#162262 = CARTESIAN_POINT ( 'NONE',  ( 4.270664716992385479, -1.744513905240049567, -0.6754176267826096369 ) ) ;
#162263 = CARTESIAN_POINT ( 'NONE',  ( -0.02319159430947541692, 2.051704324979522820, -2.228571760951563618 ) ) ;
#162264 = CARTESIAN_POINT ( 'NONE',  ( 5.885121196783658526, 9.023669275293071834, 1.199719254218452047 ) ) ;
#162265 = CARTESIAN_POINT ( 'NONE',  ( -1.499999999999997558, 7.388542872122518368, -4.154462424328208670 ) ) ;
#162266 = CARTESIAN_POINT ( 'NONE',  ( -5.998939594393441155, 7.096481464931535754, 1.069142741232721461 ) ) ;
#162267 = CARTESIAN_POINT ( 'NONE',  ( -5.829642864196175722, 7.824335979694092558, 1.443375672974064550 ) ) ;
#162268 = CARTESIAN_POINT ( 'NONE',  ( 2.998324526916512411, 6.649795714711241423, 0.000000000000000000 ) ) ;
#162269 = CARTESIAN_POINT ( 'NONE',  ( 0.8132587859420150611, -1.660809389245621492, -1.058212622827129357 ) ) ;
#162270 = CARTESIAN_POINT ( 'NONE',  ( 2.495720449669075247, -1.994069261235394741, 0.2986488809556055446 ) ) ;
#162271 = CARTESIAN_POINT ( 'NONE',  ( -7.374745490829552885, 10.69128794168811680, -1.199719254218446718 ) ) ;
#162272 = CARTESIAN_POINT ( 'NONE',  ( 6.378184920586140727, 6.405913593630768510, 0.000000000000000000 ) ) ;
#162273 = CARTESIAN_POINT ( 'NONE',  ( -11.86145016429273014, 10.19999999999999929, -1.100000000000000311 ) ) ;
#162274 = CARTESIAN_POINT ( 'NONE',  ( 2.466951935624495551, 0.1062163371072753354, -2.188993582743845590 ) ) ;
#162275 = PRESENTATION_STYLE_ASSIGNMENT (( #196892 ) ) ;
#162276 = CARTESIAN_POINT ( 'NONE',  ( -8.299562589859897699, 12.83457345481192036, -0.7998128361456281477 ) ) ;
#162277 = CARTESIAN_POINT ( 'NONE',  ( -0.9486429539267164923, 3.042910930033675854, 1.028101543437260013 ) ) ;
#162278 = CARTESIAN_POINT ( 'NONE',  ( 3.469446951953614189E-15, 6.400000000000023448, 1.214306433183764966E-14 ) ) ;
#162279 = CARTESIAN_POINT ( 'NONE',  ( -10.41986968326957808, 5.020773655391575829, -5.279272669861445166 ) ) ;
#162280 = CARTESIAN_POINT ( 'NONE',  ( 6.923409998072794558, 11.22906209772695618, 1.040834085586084257E-14 ) ) ;
#162281 = CARTESIAN_POINT ( 'NONE',  ( 8.103009739377979415, -6.893137084989842123, -7.439168848974011539 ) ) ;
#162282 = CARTESIAN_POINT ( 'NONE',  ( 6.427974226654860956, 7.632296364919712417, -1.082531754730548412 ) ) ;
#162283 = EDGE_LOOP ( 'NONE', ( #121466, #96917, #73998, #134568, #153751 ) ) ;
#162285 = CARTESIAN_POINT ( 'NONE',  ( 2.086589530005359183, -1.236640506920426263, 1.588416314350507674 ) ) ;
#162284 = CARTESIAN_POINT ( 'NONE',  ( 5.284640796330934087, 1.621094592300664328, -0.8731043043393662550 ) ) ;
#162286 = CARTESIAN_POINT ( 'NONE',  ( 3.726148964702048705, -2.024938297411133625, -1.087335920097615594 ) ) ;
#162288 = CARTESIAN_POINT ( 'NONE',  ( 2.254548712976621516, -0.4907705908011159579, -1.795021142807408543 ) ) ;
#162287 = CARTESIAN_POINT ( 'NONE',  ( -0.02919842301645457147, -0.002306431287177941429, -2.073770398395402115 ) ) ;
#162289 = CARTESIAN_POINT ( 'NONE',  ( 3.285556943749998737, -2.005208332855377140, -1.896917185911906500 ) ) ;
#162290 = CARTESIAN_POINT ( 'NONE',  ( -9.386220697865741869, 15.51845925627288203, -7.476614105868906179 ) ) ;
#162291 = CARTESIAN_POINT ( 'NONE',  ( 5.888906298306328502, -1.818048641159516476, -0.5935555146628914702 ) ) ;
#162292 = CARTESIAN_POINT ( 'NONE',  ( -7.147119532698295252, 11.49005655479003174, 0.000000000000000000 ) ) ;
#162293 = CARTESIAN_POINT ( 'NONE',  ( -4.502716413514296079, 8.267269892493059658, -0.7216878364870338292 ) ) ;
#162295 = CARTESIAN_POINT ( 'NONE',  ( 3.678450976403758066, -1.802590750232490491, -0.4997190347926713794 ) ) ;
#162294 = CARTESIAN_POINT ( 'NONE',  ( 5.390208805286830440, -0.5092157624977285968, -2.027641083400610000 ) ) ;
#162296 = CARTESIAN_POINT ( 'NONE',  ( 5.639828713604826405, 9.523624565940227882, -0.7216878364870267237 ) ) ;
#162297 = EDGE_CURVE ( 'NONE', #83982, #8134, #97143, .T. ) ;
#162298 = CARTESIAN_POINT ( 'NONE',  ( 5.372543328820884589, -0.05112055865702340440, -1.840719716649619198 ) ) ;
#162299 = STYLED_ITEM ( 'NONE', ( #37465 ), #22947 ) ;
#162300 = FACE_OUTER_BOUND ( 'NONE', #99631, .T. ) ;
#162301 = CARTESIAN_POINT ( 'NONE',  ( 0.08202876420372311184, -7.861065518611666469, -10.99977341864973468 ) ) ;
#162302 = CARTESIAN_POINT ( 'NONE',  ( 5.355954780876127863, 1.722648150766812103, -0.09025627888907016005 ) ) ;
#162303 = CARTESIAN_POINT ( 'NONE',  ( -6.847031270101295419, 7.946956888995021728, -1.199719254218446718 ) ) ;
#162304 = CARTESIAN_POINT ( 'NONE',  ( 0.7208516900601771304, 1.708106959156988847, 0.2981761063507569198 ) ) ;
#162305 = FILL_AREA_STYLE ('',( #48559 ) ) ;
#162306 = CARTESIAN_POINT ( 'NONE',  ( 0.000000000000000000, 7.999999999999992895, 0.000000000000000000 ) ) ;
#162307 = CARTESIAN_POINT ( 'NONE',  ( 4.645498245716852992, 1.942073188235559522, -0.9706016350095565404 ) ) ;
#162308 = CARTESIAN_POINT ( 'NONE',  ( 3.351995281737112364, 1.825872481133209879, -0.0009662468829912954560 ) ) ;
#162309 = CARTESIAN_POINT ( 'NONE',  ( 1.041763817972749750, 1.313373124611896703, 1.457441342770829262 ) ) ;
#162310 = CARTESIAN_POINT ( 'NONE',  ( 0.5623061109219238407, -1.172325791230070857, 1.762859051686527012 ) ) ;
#162312 = CARTESIAN_POINT ( 'NONE',  ( -1.201851678989727383E-14, 4.509375000341417916, -1.575800808251660134 ) ) ;
#162311 = CARTESIAN_POINT ( 'NONE',  ( 0.1294186239076781653, -2.093018298938463140, 0.9351526010841960668 ) ) ;
#162313 = CARTESIAN_POINT ( 'NONE',  ( 2.065088895208962327, 8.523968132013681753, 2.459875961809493639 ) ) ;
#162314 = CARTESIAN_POINT ( 'NONE',  ( 9.738834413317897898, 10.25639499182604730, 0.000000000000000000 ) ) ;
#162315 = CARTESIAN_POINT ( 'NONE',  ( 3.088655771522513582, -1.261447869382603004, 1.704333039148818507 ) ) ;
#162316 = CARTESIAN_POINT ( 'NONE',  ( -4.934804725694236893, 4.859619722839116918, -0.7216878364870207285 ) ) ;
#162317 = COLOUR_RGB ( '', 0.08235294, 0.09019608, 0.10196078) ;
#162318 = CARTESIAN_POINT ( 'NONE',  ( 2.373851744317274193, 1.000000000000000888, -11.76285798163019969 ) ) ;
#162319 = CARTESIAN_POINT ( 'NONE',  ( -4.406036734316898240, 6.163462161501577441, -1.443375672974051449 ) ) ;
#162320 = CARTESIAN_POINT ( 'NONE',  ( 0.3915760470782835845, -1.894197279051227811, 0.8358220917567968922 ) ) ;
#162322 = CARTESIAN_POINT ( 'NONE',  ( 0.7500000000000006661, 13.61458333401613352, 1.299038105676657340 ) ) ;
#162321 = CARTESIAN_POINT ( 'NONE',  ( 6.983263157960365675, -0.006178392973848687020, 2.053544886540019210 ) ) ;
#162324 = VERTEX_POINT ( 'NONE', #75173 ) ;
#162323 = CARTESIAN_POINT ( 'NONE',  ( 2.174768466102798836, 0.9529365794415098900, 2.006655600372597714 ) ) ;
#162325 = CARTESIAN_POINT ( 'NONE',  ( 0.3000039258060793745, 1.578900123410318823, -1.670874907869798864 ) ) ;
#162327 = CARTESIAN_POINT ( 'NONE',  ( 5.858276910504900847, -2.062741130177087268, -0.005609060510954055022 ) ) ;
#162326 = CARTESIAN_POINT ( 'NONE',  ( 4.033714395265605823, 4.664753868353354704, -1.199719254218446718 ) ) ;
#162329 = CARTESIAN_POINT ( 'NONE',  ( 1.001543065824772753E-15, -2.012499999999999289, 4.012584370867899430 ) ) ;
#162328 = CARTESIAN_POINT ( 'NONE',  ( 6.690022453700429139, 6.769724048930809701, 0.7998128361456331437 ) ) ;
#162330 = CARTESIAN_POINT ( 'NONE',  ( 6.398522151006641678, 6.429640362454684954, 0.000000000000000000 ) ) ;
#162331 = CARTESIAN_POINT ( 'NONE',  ( 0.2331563151865486683, 2.034376611827843906, -2.362208330281903024 ) ) ;
#162332 = CARTESIAN_POINT ( 'NONE',  ( 5.847170753249844033, 0.5281823367668266878, -1.763884204139199330 ) ) ;
#162333 = EDGE_CURVE ( 'NONE', #211245, #178928, #24094, .T. ) ;
#162335 = ORIENTED_EDGE ( 'NONE', *, *, #32928, .F. ) ;
#162334 = CARTESIAN_POINT ( 'NONE',  ( 4.008406971134620633, 7.828225232965717595, 0.7998128361456321445 ) ) ;
#162336 = CARTESIAN_POINT ( 'NONE',  ( -0.2104748580754426390, 2.865278511227668634, -2.591885361450113834 ) ) ;
#162337 = CARTESIAN_POINT ( 'NONE',  ( 1.922448523189672853, 1.607815062812420370, 0.6247884732281087095 ) ) ;
#162338 = CARTESIAN_POINT ( 'NONE',  ( 1.639861632979456418, 2.010800986640928656, -0.1531718788195315928 ) ) ;
#162339 = CARTESIAN_POINT ( 'NONE',  ( 1.846706770127172881, 0.3881029198684777803, -2.265567138619323018 ) ) ;
#162340 = CARTESIAN_POINT ( 'NONE',  ( -1.201851678989727383E-14, 3.759375000341422801, -1.575800808251660134 ) ) ;
#162341 = CARTESIAN_POINT ( 'NONE',  ( 2.073834635255236147, 2.165437736866062224, -0.6553434645707820749 ) ) ;
#162342 = CARTESIAN_POINT ( 'NONE',  ( 4.442079272866404693, 0.9008978453017953969, -1.903793715863113523 ) ) ;
#162343 = CARTESIAN_POINT ( 'NONE',  ( -3.135678666510573365, 6.880318554229450712, 0.000000000000000000 ) ) ;
#162344 = CARTESIAN_POINT ( 'NONE',  ( 3.057584390254026729, 1.761565543986362670, -0.1695560061622681525 ) ) ;
#162345 = CARTESIAN_POINT ( 'NONE',  ( 6.173040012923759257, 6.096301524699504704, -0.7998128361456281477 ) ) ;
#162347 = CARTESIAN_POINT ( 'NONE',  ( 4.845436733290686249, 0.7204735554154987343, -2.176297985750157427 ) ) ;
#162346 = CARTESIAN_POINT ( 'NONE',  ( 6.183927461164522299, 6.387205924212962849, 0.000000000000000000 ) ) ;
#162348 = CARTESIAN_POINT ( 'NONE',  ( -3.249150368769345043, 6.942425863539538611, 0.7998128361456341429 ) ) ;
#162349 =( GEOMETRIC_REPRESENTATION_CONTEXT ( 3 ) GLOBAL_UNCERTAINTY_ASSIGNED_CONTEXT ( ( #49407 ) ) GLOBAL_UNIT_ASSIGNED_CONTEXT ( ( #31107, #49471, #63588 ) ) REPRESENTATION_CONTEXT ( 'NONE', 'WORKASPACE' ) );
#162350 = UNCERTAINTY_MEASURE_WITH_UNIT (LENGTH_MEASURE( 1.000000000000000082E-05 ), #46512, 'distance_accuracy_value', 'NONE');
#162351 = CARTESIAN_POINT ( 'NONE',  ( 6.331294547457450683, 7.449227062530913379, -1.082531754730543083 ) ) ;
#162352 = CARTESIAN_POINT ( 'NONE',  ( 1.499999999999987121, 2.045833333333356929, -0.8660254037844262731 ) ) ;
#162353 = CARTESIAN_POINT ( 'NONE',  ( 4.488337453930180132, -0.4787454259813396229, -2.138356021698713416 ) ) ;
#162354 = CARTESIAN_POINT ( 'NONE',  ( -4.355193658487827690, 6.104145239700998538, -1.599625672291256295 ) ) ;
#162355 = CARTESIAN_POINT ( 'NONE',  ( 0.2184521437216075668, 7.205153265248421590, -1.990034439536078725 ) ) ;
#162356 = EDGE_CURVE ( 'NONE', #81693, #95637, #194271, .T. ) ;
#162357 = CARTESIAN_POINT ( 'NONE',  ( 4.929342268689171469, 7.989555622611471897, -1.003472558803005565 ) ) ;
#162358 = CARTESIAN_POINT ( 'NONE',  ( -1.364683531249997417, 3.259375000341423245, 1.214306433183764966E-14 ) ) ;
#162359 = CARTESIAN_POINT ( 'NONE',  ( 3.527879399192564325, -1.148099800794393444, -1.546878348965428973 ) ) ;
#162360 = CARTESIAN_POINT ( 'NONE',  ( 1.364683531249997417, 9.234375000341396245, 2.602085213965210642E-15 ) ) ;
#162361 = CARTESIAN_POINT ( 'NONE',  ( -3.294268138440636928, 6.787137228248626641, 1.040834085586084257E-14 ) ) ;
#162362 = CARTESIAN_POINT ( 'NONE',  ( 6.135037582782754129, 1.979230198018981701, 0.7618025574447004900 ) ) ;
#162363 = CARTESIAN_POINT ( 'NONE',  ( -5.966997003790228682, 8.054858819212300958, -1.443375672974066548 ) ) ;
#162364 = VERTEX_POINT ( 'NONE', #80503 ) ;
#162365 = CARTESIAN_POINT ( 'NONE',  ( -4.611181642423629157, 7.433443445252599702, 1.082531754730549967 ) ) ;
#162366 = CARTESIAN_POINT ( 'NONE',  ( 3.506755287428983792, 7.242964935309132990, 1.040834085586084257E-14 ) ) ;
#162367 = CARTESIAN_POINT ( 'NONE',  ( 6.356982874815331641, 0.3076174260261410054, -1.815216213958574132 ) ) ;
#162368 = STYLED_ITEM ( 'NONE', ( #43218 ), #37246 ) ;
#162369 = CARTESIAN_POINT ( 'NONE',  ( 11.41381675112453564, 13.53005666089991443, 3.704697986577181190 ) ) ;
#162370 = CARTESIAN_POINT ( 'NONE',  ( 0.6823417656249899377, 3.488541667008085323, -1.181850606188754593 ) ) ;
#162371 = CARTESIAN_POINT ( 'NONE',  ( 2.366429680491717313, 0.08383053003592833008, -1.738530308508005273 ) ) ;
#162372 = CARTESIAN_POINT ( 'NONE',  ( -15.75000000000000000, 13.40000000000000036, 1.099999999999996758 ) ) ;
#162373 = CARTESIAN_POINT ( 'NONE',  ( 0.000000000000000000, 6.161115872820241535, 1.249999999999999778 ) ) ;
#162374 = CARTESIAN_POINT ( 'NONE',  ( -1.402160292154681736E-14, 0.2593750003414224681, -1.575800808251665908 ) ) ;
#162375 = CARTESIAN_POINT ( 'NONE',  ( -4.286372615631644400, 7.381325999705229179, -1.030941853605553016 ) ) ;
#162376 = VECTOR ( 'NONE', #147834, 1000.000000000000000 ) ;
#162377 = CARTESIAN_POINT ( 'NONE',  ( 6.719591497160966931, -2.098179372288328182, 0.5198544864785522579 ) ) ;
#162378 = CARTESIAN_POINT ( 'NONE',  ( -10.62011439820619429, 11.28455497419572318, -0.7998128361456221525 ) ) ;
#162379 = CARTESIAN_POINT ( 'NONE',  ( -5.029711800545518585, 8.811821500704338561, 0.7216878364870458196 ) ) ;
#162380 = CARTESIAN_POINT ( 'NONE',  ( 6.051685545382852638, 0.6321331830463626789, -2.067208725892249799 ) ) ;
#162382 = ORIENTED_EDGE ( 'NONE', *, *, #140437, .T. ) ;
#162381 = DIRECTION ( 'NONE',  ( -1.276756478318932585E-15, 1.000000000000000000, -1.665334536937738262E-16 ) ) ;
#162383 = CARTESIAN_POINT ( 'NONE',  ( 0.6823417656249917140, 4.842708333674755394, 1.181850606188765695 ) ) ;
#162384 = CARTESIAN_POINT ( 'NONE',  ( 6.081318999601531772, 1.822420489394786625, -0.7521447986948930353 ) ) ;
#162385 = CARTESIAN_POINT ( 'NONE',  ( 4.868316058674494684, -0.4618845756635507893, 1.671066720262862182 ) ) ;
#162386 = ADVANCED_FACE ( 'NONE', ( #31768 ), #15479, .T. ) ;
#162388 = CARTESIAN_POINT ( 'NONE',  ( 1.488088480104592826, -2.181432686776756391, -0.2102995727721947705 ) ) ;
#162387 = CARTESIAN_POINT ( 'NONE',  ( -0.6801582343750074422, 0.5989583336747372755, -1.178068619123841643 ) ) ;
#162389 = CARTESIAN_POINT ( 'NONE',  ( 3.505163243484223479, 1.820685690116738531, -1.417681053453226703 ) ) ;
#162390 = CARTESIAN_POINT ( 'NONE',  ( 5.606733736089553055, 1.563247385715782700, -1.342922781998987736 ) ) ;
#162391 = CARTESIAN_POINT ( 'NONE',  ( 1.376788300709189450, 1.794419955772775355, -0.7429034522522351969 ) ) ;
#162392 = CARTESIAN_POINT ( 'NONE',  ( -5.355107487273497391, 9.191449801886996340, 0.7216878364870458196 ) ) ;
#162394 = EDGE_CURVE ( 'NONE', #123589, #23747, #58250, .T. ) ;
#162393 = CARTESIAN_POINT ( 'NONE',  ( -3.481411583659053566, 7.283673624236017830, 0.000000000000000000 ) ) ;
#162395 =( NAMED_UNIT ( * ) SI_UNIT ( $, .STERADIAN. ) SOLID_ANGLE_UNIT ( ) );
#162396 = CARTESIAN_POINT ( 'NONE',  ( 4.078469121099765005, 1.002472831208834680, 1.868716877859360137 ) ) ;
#162397 = CARTESIAN_POINT ( 'NONE',  ( 2.865861461037176205, -0.1511401116795624278, -2.010826411938296143 ) ) ;
#162398 = CARTESIAN_POINT ( 'NONE',  ( -5.707619481228822345, 7.681975366232176583, -1.443375672974051449 ) ) ;
#162399 = CARTESIAN_POINT ( 'NONE',  ( 4.383934217864794647, 1.438874268414831015, 1.673263306058408340 ) ) ;
#162400 = CARTESIAN_POINT ( 'NONE',  ( -3.285556943750000070, -0.1968749995220411830, 0.000000000000000000 ) ) ;
#162401 = CARTESIAN_POINT ( 'NONE',  ( -1.325546123766559337, -3.124052913013680488, -3.130165297716357209 ) ) ;
#162402 = CARTESIAN_POINT ( 'NONE',  ( 0.001355176523862845501, 14.56276549857873093, 11.93721147252166048 ) ) ;
#162403 = CARTESIAN_POINT ( 'NONE',  ( -6.994027139803241866, 9.253060644560830994, -1.599625672291271394 ) ) ;
#162405 = LINE ( 'NONE', #29197, #196337 ) ;
#162404 = CARTESIAN_POINT ( 'NONE',  ( -4.631600894319110040, 8.440630447364583233, 0.4419995416731822280 ) ) ;
#162406 = CARTESIAN_POINT ( 'NONE',  ( 0.3282377607281116716, 2.073664549684627545, 1.224999999999953015 ) ) ;
#162407 = VERTEX_POINT ( 'NONE', #152968 ) ;
#162408 = CARTESIAN_POINT ( 'NONE',  ( 3.995036845513312951, 1.742007986889832161, -1.100897373992800299 ) ) ;
#162409 = CARTESIAN_POINT ( 'NONE',  ( -9.569358774130435563, 3.553060279300347180, -7.167287524826059020 ) ) ;
#162410 = CARTESIAN_POINT ( 'NONE',  ( 0.3773006915670404915, -8.233136995002887204, 9.492905263954449779 ) ) ;
#162411 = CARTESIAN_POINT ( 'NONE',  ( -4.069418662396130593, 7.899405539437467816, -0.7998128361456281477 ) ) ;
#162412 = CARTESIAN_POINT ( 'NONE',  ( -4.522526758610270647, 7.433975764090723359, -1.199719254218453823 ) ) ;
#162413 = CARTESIAN_POINT ( 'NONE',  ( 3.457679895445249674, -1.530724978927421986, -1.317682070945853656 ) ) ;
#162414 = CARTESIAN_POINT ( 'NONE',  ( 1.499999999999987121, 0.2541666666666844154, 0.8660254037844524744 ) ) ;
#162416 = CARTESIAN_POINT ( 'NONE',  ( 10.24960094225127172, 11.06021530882240356, -0.7216878364870257245 ) ) ;
#162415 = CARTESIAN_POINT ( 'NONE',  ( -5.978219388983010418, 5.939287140093762574, -0.7998128361456362523 ) ) ;
#162417 = CARTESIAN_POINT ( 'NONE',  ( 7.644099680006512187, 7.812537802962739697, 1.040834085586084257E-14 ) ) ;
#162418 = CARTESIAN_POINT ( 'NONE',  ( 3.432544477427549534, 2.010279954523132240, 0.4531449079418439774 ) ) ;
#162419 = CARTESIAN_POINT ( 'NONE',  ( 2.461564753630896440, -1.930417925741171103, -0.5826551686555283549 ) ) ;
#162420 = DIRECTION ( 'NONE',  ( -0.000000000000000000, -1.000000000000000000, -0.000000000000000000 ) ) ;
#162421 = CARTESIAN_POINT ( 'NONE',  ( 5.843727902690005749, 6.776436293681846301, -1.199719254218445830 ) ) ;
#162422 = FACE_OUTER_BOUND ( 'NONE', #84599, .T. ) ;
#162423 = CARTESIAN_POINT ( 'NONE',  ( 0.9547317490294878750, 0.3612830171869831353, -1.805165878648997690 ) ) ;
#162424 = CARTESIAN_POINT ( 'NONE',  ( 6.322910218073367616, 2.057572540570989261, 0.7984293639632376038 ) ) ;
#162425 = CARTESIAN_POINT ( 'NONE',  ( 5.899733120602060232, 6.912052057904395141, -1.199719254218452047 ) ) ;
#162426 = CARTESIAN_POINT ( 'NONE',  ( 2.618638089201937635, 1.414096770131420877, -1.634928933042498755 ) ) ;
#162427 = CARTESIAN_POINT ( 'NONE',  ( -5.097502569058225852, 5.049433873430440478, -0.7216878364870207285 ) ) ;
#162428 = CARTESIAN_POINT ( 'NONE',  ( 4.100857973768299303, 1.937344669444723166, 0.8546590867991187279 ) ) ;
#162429 = CARTESIAN_POINT ( 'NONE',  ( 2.812212034788389214, -1.912053501320301718, 1.275153900055803646 ) ) ;
#162430 = CARTESIAN_POINT ( 'NONE',  ( 0.01777464290183803503, 3.404255796403599987, -2.081138097628782990 ) ) ;
#162431 = CARTESIAN_POINT ( 'NONE',  ( 1.129532124359374334, -1.183843481993757774, -1.448407549327054955 ) ) ;
#162432 = CARTESIAN_POINT ( 'NONE',  ( 4.996930482532231821, 1.639556309048403770, -1.094490209086243171 ) ) ;
#162433 = CARTESIAN_POINT ( 'NONE',  ( 4.698454014923811428, 1.387101836239763131, -1.463925544105355803 ) ) ;
#162435 = CARTESIAN_POINT ( 'NONE',  ( 9.856414487010587422, 11.56186699200962487, 1.082531754730548412 ) ) ;
#162434 = CARTESIAN_POINT ( 'NONE',  ( -1.364683531250012516, 2.738541667008090208, -0.7879004041258289570 ) ) ;
#162437 = CARTESIAN_POINT ( 'NONE',  ( 5.936178820057578243, 1.039279821879979693, -1.831694563109196316 ) ) ;
#162436 = CARTESIAN_POINT ( 'NONE',  ( -6.226218857173722476, 8.287007971501239467, 1.599625672291283607 ) ) ;
#162438 = CARTESIAN_POINT ( 'NONE',  ( 6.619590326553026038, 0.3579758704960536719, -2.039031579972025554 ) ) ;
#162439 = CARTESIAN_POINT ( 'NONE',  ( 5.575427483717746213, 7.527751369135936343, 1.599625672291267398 ) ) ;
#162440 = CARTESIAN_POINT ( 'NONE',  ( -5.280010757518168063, 8.247430752824802980, -1.199719254218446718 ) ) ;
#162441 = DIRECTION ( 'NONE',  ( 0.2684563758389304500, 5.821219718043054220E-15, 0.9632918427306581544 ) ) ;
#162442 = CARTESIAN_POINT ( 'NONE',  ( 4.680523324745738734, -1.912062325676016306, -0.4798145647967356764 ) ) ;
#162443 = CARTESIAN_POINT ( 'NONE',  ( 5.941667304196568189, -1.900381328601069342, 0.6844855596733252501 ) ) ;
#162444 = CARTESIAN_POINT ( 'NONE',  ( -0.7500000000000215383, 0.4729166673494850093, 1.299038105676659116 ) ) ;
#162445 = CARTESIAN_POINT ( 'NONE',  ( 4.565214137342485934, -2.059927483508086965, -1.040394749072820701 ) ) ;
#162446 = CARTESIAN_POINT ( 'NONE',  ( 2.149356475496758456, 1.796580072245733462, -1.012980232677022974 ) ) ;
#162447 = CARTESIAN_POINT ( 'NONE',  ( 7.510853912290742507, 8.825379654836435606, -1.082531754730537976 ) ) ;
#162448 = CARTESIAN_POINT ( 'NONE',  ( 5.123001941117305336, 7.070197912760590064, 1.599625672291268286 ) ) ;
#162449 = CARTESIAN_POINT ( 'NONE',  ( 5.246079093845007257, 5.085123462432798114, 0.7998128361456352531 ) ) ;
#162450 = CARTESIAN_POINT ( 'NONE',  ( -1.201851678989727383E-14, 2.134375000341423689, 1.575800808251672791 ) ) ;
#162451 = CARTESIAN_POINT ( 'NONE',  ( 3.040771591214902259, 6.769593633051179005, -0.7998128361456362523 ) ) ;
#162452 = CARTESIAN_POINT ( 'NONE',  ( 5.463572716182812705, 9.317992568947877530, 0.7216878364870438212 ) ) ;
#162453 = CARTESIAN_POINT ( 'NONE',  ( 4.510331875626576448, 2.170777084992558059, -0.04906379945510477847 ) ) ;
#162454 = DIRECTION ( 'NONE',  ( 0.6507913734559641616, -0.7592566023653004592, 0.000000000000000000 ) ) ;
#162456 = CARTESIAN_POINT ( 'NONE',  ( 2.753256032281672372, 1.832158412346639453, -0.1828795585285883096 ) ) ;
#162455 = CARTESIAN_POINT ( 'NONE',  ( -2.806174608348664723, 6.217694776474651519, 1.040834085586084257E-14 ) ) ;
#162458 = CARTESIAN_POINT ( 'NONE',  ( 6.620655732516647518, 0.01042156863438310939, 1.726407961933309920 ) ) ;
#162457 = CARTESIAN_POINT ( 'NONE',  ( 0.6823417656249899377, 4.676041667008086655, -1.181850606188754593 ) ) ;
#162459 = CARTESIAN_POINT ( 'NONE',  ( 5.108995794240286159, -0.3219066699026683631, 2.167653318578148358 ) ) ;
#162460 = CARTESIAN_POINT ( 'NONE',  ( 8.753616243065934555, 13.39305056715447861, 8.208245953058789013 ) ) ;
#162461 = CARTESIAN_POINT ( 'NONE',  ( 5.506774338047922157, 1.717276559928378132, -1.473185486808053835 ) ) ;
#162462 = CARTESIAN_POINT ( 'NONE',  ( -4.712932107567791462, 7.040231785572885315, -1.411385885297003373 ) ) ;
#162463 = CARTESIAN_POINT ( 'NONE',  ( 4.595652554671352696, 8.489339133230261680, -0.03962354257190832396 ) ) ;
#162464 = VECTOR ( 'NONE', #47393, 1000.000000000000114 ) ;
#162465 = CARTESIAN_POINT ( 'NONE',  ( -5.221298554594238084, 8.145246509451649075, 1.082531754730549967 ) ) ;
#162466 = CARTESIAN_POINT ( 'NONE',  ( -9.828980619278564011E-14, 7.054063922337708625, 3.955400951015630273 ) ) ;
#162467 =( BOUNDED_CURVE ( )  B_SPLINE_CURVE ( 2, ( #48423, #67803, #114536, #32152, #98230 ),
 .UNSPECIFIED., .F., .T. ) 
 B_SPLINE_CURVE_WITH_KNOTS ( ( 3, 2, 3 ),
 ( 0.01067668659529987657, 0.01250000000000000069, 0.01407841936770215865 ),
 .UNSPECIFIED. ) 
 CURVE ( )  GEOMETRIC_REPRESENTATION_ITEM ( )  RATIONAL_B_SPLINE_CURVE ( ( 0.9340561916853915569, 0.9413733574794114212, 1.000000000000000000, 0.9492476566127876492, 0.9369473844697255860 ) ) 
 REPRESENTATION_ITEM ( '' )  );
#162468 = CARTESIAN_POINT ( 'NONE',  ( 0.9886869571070689977, 1.563518247070281086, -0.8293041508813036033 ) ) ;
#162469 = CARTESIAN_POINT ( 'NONE',  ( 4.529943747908701468, -1.973814829549960237, 0.3949202218342766080 ) ) ;
#162470 = B_SPLINE_CURVE_WITH_KNOTS ( 'NONE', 3,
 ( #33275, #149162, #66805, #35401, #184847, #132947 ),
 .UNSPECIFIED., .F., .F.,
 ( 4, 2, 4 ),
 ( 0.000000000000000000, 0.002037565947615825948, 0.004075131895231652764 ),
 .UNSPECIFIED. ) ;
#162471 = CARTESIAN_POINT ( 'NONE',  ( 5.459129407796876166, 9.520734742405036144, 1.040834085586084257E-14 ) ) ;
#162472 = CARTESIAN_POINT ( 'NONE',  ( 3.575310672209235374, 0.05349853608750848588, -2.105455972502618955 ) ) ;
#162473 = CARTESIAN_POINT ( 'NONE',  ( 2.548326723280808892, -1.319200400300493570, 1.389225609306585119 ) ) ;
#162474 = CARTESIAN_POINT ( 'NONE',  ( 3.846762897975340767, 5.510976019103107859, -1.599625672291256295 ) ) ;
#162475 = CARTESIAN_POINT ( 'NONE',  ( 3.226963424687212090, -1.818787540941589009, -0.7562359814760648558 ) ) ;
#162476 = CARTESIAN_POINT ( 'NONE',  ( 5.818619510638624703, -0.7308962487734929070, -1.883076464014792117 ) ) ;
#162477 = CARTESIAN_POINT ( 'NONE',  ( 1.709613803025863188, -1.856884215550944850, 0.2259493607114013147 ) ) ;
#162478 = CARTESIAN_POINT ( 'NONE',  ( 1.697631272820496307, -1.418720726069604865, -1.355276769646639901 ) ) ;
#162481 = ORIENTED_EDGE ( 'NONE', *, *, #180453, .F. ) ;
#162480 = CARTESIAN_POINT ( 'NONE',  ( 1.336036003918249948, -1.064896177285217016, -1.588262137521757822 ) ) ;
#162479 = CARTESIAN_POINT ( 'NONE',  ( 3.826516835200497457, 1.638561065401537897, 0.5390252620694930830 ) ) ;
#162483 = CARTESIAN_POINT ( 'NONE',  ( 6.046573322014824114, 7.117052299514516456, -1.082531754730543083 ) ) ;
#162482 = CARTESIAN_POINT ( 'NONE',  ( 0.8564375766340023288, 2.204168734417511821, -0.1118928034387969561 ) ) ;
#162484 = CARTESIAN_POINT ( 'NONE',  ( 1.364683531249988757, 1.446875000341421469, 0.000000000000000000 ) ) ;
#162486 = AXIS2_PLACEMENT_3D ( 'NONE', #103890, #120205, #73504 ) ;
#162485 = CARTESIAN_POINT ( 'NONE',  ( 7.242026607993941489, 11.60078147596829901, 0.7998128361456462443 ) ) ;
#162487 = DIRECTION ( 'NONE',  ( 0.000000000000000000, 0.7999999999999973799, 0.6000000000000034195 ) ) ;
#162488 = FACE_OUTER_BOUND ( 'NONE', #97260, .T. ) ;
#162489 = FACE_OUTER_BOUND ( 'NONE', #94510, .T. ) ;
#162490 = ORIENTED_EDGE ( 'NONE', *, *, #118098, .T. ) ;
#162491 = CYLINDRICAL_SURFACE ( 'NONE', #82216, 0.08000000000000004330 ) ;
#162492 = CARTESIAN_POINT ( 'NONE',  ( 1.434126425884488354, 1.231690216755284562, 1.664001042209894088 ) ) ;
#162493 = CARTESIAN_POINT ( 'NONE',  ( -1.500000000000013101, 1.420833333333354043, 0.8660254037844403729 ) ) ;
#162494 = CARTESIAN_POINT ( 'NONE',  ( 6.425674737872927089, 9.584038729905381970, -1.199719254218440723 ) ) ;
#162495 = CARTESIAN_POINT ( 'NONE',  ( -7.557780564614042795, 10.90482886110335414, -1.199719254218446718 ) ) ;
#162496 = CARTESIAN_POINT ( 'NONE',  ( 3.705121118284530279, 7.544668081299086282, -1.734723475976807094E-15 ) ) ;
#162497 = CARTESIAN_POINT ( 'NONE',  ( 5.672555391165950311, 0.8593836824349295744, 1.938725756316476589 ) ) ;
#162498 = CARTESIAN_POINT ( 'NONE',  ( 3.410758162289653672, 6.136912401716668519, -1.199719254218453823 ) ) ;
#162499 = CARTESIAN_POINT ( 'NONE',  ( -1.364683531249997417, 2.759375000341422801, 1.214306433183764966E-14 ) ) ;
#162500 = ORIENTED_EDGE ( 'NONE', *, *, #170541, .F. ) ;
#162501 = CARTESIAN_POINT ( 'NONE',  ( 0.7499999999999920064, 4.483333333333352932, 1.299038105676669330 ) ) ;
#162503 = CARTESIAN_POINT ( 'NONE',  ( 3.225950485047770933, 5.851027101609320269, 1.199719254218450271 ) ) ;
#162502 = CARTESIAN_POINT ( 'NONE',  ( 6.514115657861259123, 1.956686900881845714, -0.1430618042221123987 ) ) ;
#162504 = CARTESIAN_POINT ( 'NONE',  ( 4.218124927476913477, -1.674631575811252215, -1.122325875776951420 ) ) ;
#162505 = CARTESIAN_POINT ( 'NONE',  ( 3.696418550083080401, 1.350829783741511969, -1.358666786172907592 ) ) ;
#162506 = DIRECTION ( 'NONE',  ( 0.000000000000000000, 1.000000000000000000, 0.000000000000000000 ) ) ;
#162507 = CARTESIAN_POINT ( 'NONE',  ( 1.699035084177059174, 1.824418957995146195, 1.213967346723361596 ) ) ;
#162508 = CARTESIAN_POINT ( 'NONE',  ( -1.500000000000013101, 0.9520833340161557468, 0.8660254037844403729 ) ) ;
#162509 = CARTESIAN_POINT ( 'NONE',  ( 4.781498422495529255, 0.1932255103699429266, -2.003883580701450562 ) ) ;
#162510 = CARTESIAN_POINT ( 'NONE',  ( -5.371001409308059138, 9.417918744168066070, -0.7998128361456231517 ) ) ;
#162512 = CARTESIAN_POINT ( 'NONE',  ( 6.064083512088704886, -1.132370213454384045, 1.788784107109566701 ) ) ;
#162511 = CARTESIAN_POINT ( 'NONE',  ( -2.968872451712654126, 6.407508927065978632, 1.040834085586084257E-14 ) ) ;
#162514 = CARTESIAN_POINT ( 'NONE',  ( -7.553827861469316396, 8.841829255582865699, -1.199719254218452047 ) ) ;
#162513 = CARTESIAN_POINT ( 'NONE',  ( 2.771125873548622831, 1.984386128312282116, -0.6585125772022564217 ) ) ;
#162516 = ORIENTED_EDGE ( 'NONE', *, *, #75988, .F. ) ;
#162515 = CARTESIAN_POINT ( 'NONE',  ( 0.4633286609967076086, 1.707074611214503435, -0.2455724507211871910 ) ) ;
#162517 = CARTESIAN_POINT ( 'NONE',  ( 7.298366762858032430, 7.409182732956175244, 1.040834085586084257E-14 ) ) ;
#162518 = EDGE_CURVE ( 'NONE', #8341, #112905, #166819, .T. ) ;
#162519 = DIRECTION ( 'NONE',  ( 0.000000000000000000, 0.000000000000000000, 1.000000000000000000 ) ) ;
#162520 = CARTESIAN_POINT ( 'NONE',  ( 0.000000000000000000, -0.2000000000000057288, 6.200000000000000178 ) ) ;
#162522 = CARTESIAN_POINT ( 'NONE',  ( 9.042925270190632858, 10.61279623905300085, 1.082531754730549967 ) ) ;
#162521 = CARTESIAN_POINT ( 'NONE',  ( 6.632963465583686435, 8.761543347979550589, -1.599625672291262513 ) ) ;
#162523 = VERTEX_POINT ( 'NONE', #86386 ) ;
#162524 = DIRECTION ( 'NONE',  ( -0.05872483221476459958, -0.000000000000000000, -0.9982742078614211811 ) ) ;
#162526 = CARTESIAN_POINT ( 'NONE',  ( 1.295247000857565167, 1.673883212702592660, -0.6929762496888560719 ) ) ;
#162525 = CARTESIAN_POINT ( 'NONE',  ( 5.397027666691686321, 8.454226823519094935, 1.199719254218451159 ) ) ;
#162527 = CARTESIAN_POINT ( 'NONE',  ( -7.043624497499477499, 8.176315654292865887, 1.199719254218450271 ) ) ;
#162528 = CARTESIAN_POINT ( 'NONE',  ( 3.623053363349855172, 5.249981562040033189, 1.599625672291267398 ) ) ;
#162529 = ORIENTED_EDGE ( 'NONE', *, *, #147605, .F. ) ;
#162530 = CARTESIAN_POINT ( 'NONE',  ( 6.387826650694035990, 7.481494509678370264, -1.199719254218452047 ) ) ;
#162531 = CARTESIAN_POINT ( 'NONE',  ( 2.156637704053586901, 0.3978940469637832766, 1.767043172555267772 ) ) ;
#162532 = CARTESIAN_POINT ( 'NONE',  ( 6.639320575229251453, 0.008029245381881154262, 1.796863947021019481 ) ) ;
#162533 = SURFACE_SIDE_STYLE ('',( #100705 ) ) ;
#162534 = CARTESIAN_POINT ( 'NONE',  ( 4.027228449831594226, 7.557535101434955216, 0.3677212997342318990 ) ) ;
#162535 = ORIENTED_EDGE ( 'NONE', *, *, #90176, .F. ) ;
#162536 = EDGE_CURVE ( 'NONE', #96352, #14053, #193894, .T. ) ;
#162537 = COLOUR_RGB ( '', 0.40784314, 0.44705882, 0.49803922) ;
#162538 = CARTESIAN_POINT ( 'NONE',  ( 2.506119797010537997, 1.860588423725167306, 0.04906839929019050223 ) ) ;
#162539 = EDGE_CURVE ( 'NONE', #322, #50087, #138557, .T. ) ;
#162540 = CARTESIAN_POINT ( 'NONE',  ( 0.1049102937123137097, -0.09321989032292328503, 1.913444960606479395 ) ) ;
#162541 = CARTESIAN_POINT ( 'NONE',  ( 0.1471128783409255958, -1.407412912164500263, -1.162481699956314785 ) ) ;
#162542 = CARTESIAN_POINT ( 'NONE',  ( 1.493107181547908668, 4.435412813646488317, 0.1630395111544306885 ) ) ;
#162543 = CARTESIAN_POINT ( 'NONE',  ( 4.635702676548680401, 8.322458603728597026, -0.3981331281527732968 ) ) ;
#162544 = DIRECTION ( 'NONE',  ( 0.000000000000000000, 0.000000000000000000, 1.000000000000000000 ) ) ;
#162545 = CARTESIAN_POINT ( 'NONE',  ( -4.175548123328963079, 4.934189567714277302, 1.082531754730560403 ) ) ;
#162546 = CARTESIAN_POINT ( 'NONE',  ( 8.459924665247367415, 8.972259652317825740, -0.7216878364870267237 ) ) ;
#162547 = CARTESIAN_POINT ( 'NONE',  ( 4.258625426654465862, -0.6138343748593175775, -1.871441549783653180 ) ) ;
#162548 = CARTESIAN_POINT ( 'NONE',  ( -3.567766978690493307, 7.314145241780881435, 1.040834085586084257E-14 ) ) ;
#162549 = DIRECTION ( 'NONE',  ( -0.05872483221476467591, 7.952201780260630618E-17, -0.9982742078614211811 ) ) ;
#162550 = CARTESIAN_POINT ( 'NONE',  ( 6.580031370938625557, -2.148343778048496411, -0.4316624935760752790 ) ) ;
#162551 = CARTESIAN_POINT ( 'NONE',  ( 4.552304845665864796, 6.880248622055519903, 1.357528830636938189 ) ) ;
#162552 = CARTESIAN_POINT ( 'NONE',  ( 5.508790920392054424, 1.458765576344657866, -1.258282468310659707 ) ) ;
#162553 = CARTESIAN_POINT ( 'NONE',  ( -5.682838942422375084, 9.781729199468104596, 0.000000000000000000 ) ) ;
#162554 = CARTESIAN_POINT ( 'NONE',  ( -1.225000000000036282, 2.291666667349470554, -0.7072540797573277915 ) ) ;
#162555 = CARTESIAN_POINT ( 'NONE',  ( 2.649284799151204073, -1.834272514977531632, 1.226802785254533346 ) ) ;
#162556 = CARTESIAN_POINT ( 'NONE',  ( -6.243047111023654949, 6.927230885129543658, 0.8200755559147846485 ) ) ;
#162557 = CARTESIAN_POINT ( 'NONE',  ( 0.07037084582631887575, 0.7337836260858082715, 1.766209603411242668 ) ) ;
#162558 = ORIENTED_EDGE ( 'NONE', *, *, #202320, .T. ) ;
#162559 = ORIENTED_EDGE ( 'NONE', *, *, #157961, .F. ) ;
#162560 = CARTESIAN_POINT ( 'NONE',  ( 0.1331715793776600265, 0.003733371859311259821, -1.953671397793784070 ) ) ;
#162561 = CARTESIAN_POINT ( 'NONE',  ( 1.804143404396211681, 1.437808690349717589, -1.305647666910898730 ) ) ;
#162562 = CARTESIAN_POINT ( 'NONE',  ( 0.7376574009502723239, -1.897405874265755354, -0.6818954202830117550 ) ) ;
#162564 = CARTESIAN_POINT ( 'NONE',  ( 4.944130858096120740, -0.8794851946119870423, 1.640036094180880477 ) ) ;
#162563 = CARTESIAN_POINT ( 'NONE',  ( -5.981082042284069367, 7.006959133200059142, 1.199719254218452935 ) ) ;
#162565 = CARTESIAN_POINT ( 'NONE',  ( 6.225128807330042591, 7.291680359087043151, -1.199719254218452047 ) ) ;
#162566 = CARTESIAN_POINT ( 'NONE',  ( 6.509000000000037645, 7.629137130509070275, 2.600000000000001421 ) ) ;
#162567 = CARTESIAN_POINT ( 'NONE',  ( -5.603597561149804562, 5.431951997629870910, 0.7998128361456341429 ) ) ;
#162568 = CARTESIAN_POINT ( 'NONE',  ( -5.915100157312088491, 10.12297696016459092, -0.7998128361456362523 ) ) ;
#162569 = CARTESIAN_POINT ( 'NONE',  ( 1.312353134292881141, 1.468346937154514364, -1.627112938194043235 ) ) ;
#162570 = CARTESIAN_POINT ( 'NONE',  ( 3.063779527008311021, 5.557864633942907417, 1.082531754730546636 ) ) ;
#162571 = CARTESIAN_POINT ( 'NONE',  ( 0.3817069231124535778, 3.999999999999974243, -1.007084182327222965 ) ) ;
#162572 = SURFACE_SIDE_STYLE ('',( #212352 ) ) ;
#162573 = CARTESIAN_POINT ( 'NONE',  ( 2.033574986395149775, -1.191784744093337123, -1.383114941912518159 ) ) ;
#162574 = CARTESIAN_POINT ( 'NONE',  ( -3.110706179331648169, 5.716575411607132118, 1.199719254218462483 ) ) ;
#162575 = PRESENTATION_LAYER_ASSIGNMENT (  '', '', ( #69140 ) ) ;
#162576 = CARTESIAN_POINT ( 'NONE',  ( -0.4603033281871871663, 3.129930857433576907, -1.947265364836649137 ) ) ;
#162577 = CARTESIAN_POINT ( 'NONE',  ( 6.509000000000011887, 3.696273625755361447, 2.514342382328867753 ) ) ;
#162578 = CARTESIAN_POINT ( 'NONE',  ( 7.716561984472250835, 12.15440608185967086, 1.040834085586084257E-14 ) ) ;
#162579 = CARTESIAN_POINT ( 'NONE',  ( 6.305291373979138747, 1.520805759102667132, 1.009792402853857407 ) ) ;
#162580 = CARTESIAN_POINT ( 'NONE',  ( 4.645332984504850771, 1.754159843842403976, -0.8783796436172899291 ) ) ;
#162581 = CARTESIAN_POINT ( 'NONE',  ( -7.167456763118792651, 11.51378332361394818, 0.000000000000000000 ) ) ;
#162582 = CARTESIAN_POINT ( 'NONE',  ( 5.636439174979242850, 7.598931675607687453, -1.599625672291262513 ) ) ;
#162583 = CARTESIAN_POINT ( 'NONE',  ( 4.528971853086540378, -2.003544689622422936, 0.8885388601788182239 ) ) ;
#162584 = CARTESIAN_POINT ( 'NONE',  ( 5.671388329218120639, 5.511041227042920099, 1.040834085586084257E-14 ) ) ;
#162585 = CARTESIAN_POINT ( 'NONE',  ( 3.766520095694513959, -0.8345382577515870759, -1.894767260282135712 ) ) ;
#162587 = CARTESIAN_POINT ( 'NONE',  ( -0.6823417656250212460, 1.363541667008083547, 1.181850606188755259 ) ) ;
#162586 =( NAMED_UNIT ( * ) PLANE_ANGLE_UNIT ( ) SI_UNIT ( $, .RADIAN. ) );
#162588 = EDGE_LOOP ( 'NONE', ( #99669, #201664, #30105, #42464 ) ) ;
#162589 = CARTESIAN_POINT ( 'NONE',  ( 3.797728626882245884, 1.624942816722572125, -1.626123495085467496 ) ) ;
#162590 = CARTESIAN_POINT ( 'NONE',  ( 7.619319141200063150, 9.912291636198670375, 1.443375672974076540 ) ) ;
#162592 = CARTESIAN_POINT ( 'NONE',  ( 3.285556943750000070, -0.2843749995220419269, 0.000000000000000000 ) ) ;
#162591 = CARTESIAN_POINT ( 'NONE',  ( 6.048345925472183637, 8.149765894507963182, 1.443375672974065660 ) ) ;
#162593 = CARTESIAN_POINT ( 'NONE',  ( 6.620655732516631531, 2.063554893983750027, 2.233578047529918287 ) ) ;
#162594 = CARTESIAN_POINT ( 'NONE',  ( -10.50059885609814536, 5.377696206510357513, -5.808392519734771220 ) ) ;
#162595 = CARTESIAN_POINT ( 'NONE',  ( 3.749888610702892144, 0.6998405808875374223, 1.811630882863373149 ) ) ;
#162596 = ORIENTED_EDGE ( 'NONE', *, *, #107493, .F. ) ;
#162597 = CARTESIAN_POINT ( 'NONE',  ( 0.04277205541326366267, -9.414847940711716490, 9.500256024741366545 ) ) ;
#162598 = EDGE_CURVE ( 'NONE', #100096, #96449, #120023, .T. ) ;
#162599 = CARTESIAN_POINT ( 'NONE',  ( 5.484596585704371918, -1.208295678440996390, 1.482354609825987435 ) ) ;
#162600 = CARTESIAN_POINT ( 'NONE',  ( 5.016472913109910614, 1.187476848380929928, -1.251119849200056366 ) ) ;
#162601 = CARTESIAN_POINT ( 'NONE',  ( 5.102750050473856547, 1.865045247124358818, 0.7672954931761332142 ) ) ;
#162602 = CARTESIAN_POINT ( 'NONE',  ( 4.992985585870878928, -2.287786813913486039, 0.2239274308311194894 ) ) ;
#162603 = CARTESIAN_POINT ( 'NONE',  ( 11.43204722947019825, 12.44407245973824239, 3.649275849833181429 ) ) ;
#162604 = CARTESIAN_POINT ( 'NONE',  ( 0.7157882511714327434, -0.3199875008889854766, 2.183444778895065941 ) ) ;
#162606 = CARTESIAN_POINT ( 'NONE',  ( -5.316205630334276400, 5.374863788244313767, -0.7216878364870338292 ) ) ;
#162605 = CARTESIAN_POINT ( 'NONE',  ( 0.000000000000000000, 11.37999999999999901, 0.000000000000000000 ) ) ;
#162607 = CARTESIAN_POINT ( 'NONE',  ( 6.169200886764430791, 0.1279487620423936933, -1.765195888111121159 ) ) ;
#162608 = CARTESIAN_POINT ( 'NONE',  ( 4.553361389630797618, -1.314998166741452090, 1.528740011303417745 ) ) ;
#162610 = CARTESIAN_POINT ( 'NONE',  ( 2.256202855815407915, 0.9821592622454662358, 2.071323110799852873 ) ) ;
#162609 = CARTESIAN_POINT ( 'NONE',  ( 3.562760505341037831, 7.378580699531681830, -1.734723475976807094E-15 ) ) ;
#162611 = CARTESIAN_POINT ( 'NONE',  ( 1.464397578914914400, 0.1305661322733233098, -1.735479185401978208 ) ) ;
#162612 = CARTESIAN_POINT ( 'NONE',  ( 11.89942855770814312, 13.79999999999999893, 0.6999999999999992895 ) ) ;
#162613 = CARTESIAN_POINT ( 'NONE',  ( 1.141452232654313059, -0.03515412242651934360, -1.733669386235114906 ) ) ;
#162614 = CARTESIAN_POINT ( 'NONE',  ( -2.353626204688216217E-14, 0.7343750003414536431, 1.570758158831780271 ) ) ;
#162615 = LINE ( 'NONE', #66125, #108265 ) ;
#162616 = EDGE_CURVE ( 'NONE', #7772, #72818, #56024, .T. ) ;
#162617 = CARTESIAN_POINT ( 'NONE',  ( 1.574930973106080545, 1.458645925580204006, -1.608354241196547685 ) ) ;
#162618 = CARTESIAN_POINT ( 'NONE',  ( 2.764861550476094276, -0.1531697945360478985, -2.010801143277194392 ) ) ;
#162619 = CARTESIAN_POINT ( 'NONE',  ( -1.500000000000001332, 0.9312500006828163812, 0.000000000000000000 ) ) ;
#162620 = CARTESIAN_POINT ( 'NONE',  ( 6.041620323887018529, -1.397190737843529540, -1.326607404314980254 ) ) ;
#162621 = CARTESIAN_POINT ( 'NONE',  ( 0.6823417656249969321, 13.27604166700806232, -1.181850606188757036 ) ) ;
#162622 = CARTESIAN_POINT ( 'NONE',  ( 2.232967058637932656, 1.447036570497368446, -1.685575845266892747 ) ) ;
#162623 = VERTEX_POINT ( 'NONE', #4033 ) ;
#162624 = CARTESIAN_POINT ( 'NONE',  ( 6.773376336902542150, -7.645781813054120413, 6.661184053806703531 ) ) ;
#162625 = CARTESIAN_POINT ( 'NONE',  ( 0.7499999999999885647, -0.5166666666666444030, 1.299038105676657340 ) ) ;
#162626 = CARTESIAN_POINT ( 'NONE',  ( 7.944187942603509356, 11.35563746875774882, 1.199719254218460707 ) ) ;
#162627 =( LENGTH_UNIT ( ) NAMED_UNIT ( * ) SI_UNIT ( .MILLI., .METRE. ) );
#162628 = CARTESIAN_POINT ( 'NONE',  ( -1.402160292154681736E-14, -1.178124999658576311, 1.575800808251672791 ) ) ;
#162629 = CARTESIAN_POINT ( 'NONE',  ( 5.688919983501732780, 1.323409507385058914, 1.130498143038612513 ) ) ;
#162630 = CARTESIAN_POINT ( 'NONE',  ( 3.314850587115983238, -1.487306837207631016, 1.279512770686676904 ) ) ;
#162632 = CARTESIAN_POINT ( 'NONE',  ( -7.429504990608782222, 8.730472579540773381, 1.082531754730549967 ) ) ;
#162631 = CARTESIAN_POINT ( 'NONE',  ( 2.198393463710220264, 5.716542807637226886, 0.7998128361456462443 ) ) ;
#162633 = VECTOR ( 'NONE', #188982, 1000.000000000000000 ) ;
#162634 = DIRECTION ( 'NONE',  ( 0.7592566023652995710, 0.6507913734559650498, -0.000000000000000000 ) ) ;
#162635 = CARTESIAN_POINT ( 'NONE',  ( 4.341306091576823789, -1.971171287362062818, 1.110239852968941232 ) ) ;
#162636 = CARTESIAN_POINT ( 'NONE',  ( 0.9946673667629982729, 2.031838985545178389, 0.3545390999590279368 ) ) ;
#162637 = CARTESIAN_POINT ( 'NONE',  ( -5.506582945444718824, 9.576097202994168001, 0.7998128361456481317 ) ) ;
#162638 = CARTESIAN_POINT ( 'NONE',  ( 2.096875702627752691, -0.6037365238656807742, -2.180425337281781673 ) ) ;
#162639 = EDGE_LOOP ( 'NONE', ( #91133, #79110, #24243, #154493 ) ) ;
#162640 = CARTESIAN_POINT ( 'NONE',  ( -1.500000000000013101, 1.660416667349487119, -0.8660254037844313801 ) ) ;
#162641 = CARTESIAN_POINT ( 'NONE',  ( 3.479631686803522417, 1.184185218286455621, 1.448006030947253331 ) ) ;
#162642 = CARTESIAN_POINT ( 'NONE',  ( 2.918323747256291956, -1.167012588333454781, -1.282868673017246941 ) ) ;
#162643 = EDGE_CURVE ( 'NONE', #82462, #109831, #153527, .T. ) ;
#162644 = CARTESIAN_POINT ( 'NONE',  ( 5.987848539424092564, -2.180829346447300310, -0.2163489798085171945 ) ) ;
#162645 = CARTESIAN_POINT ( 'NONE',  ( 6.616287922300326585, -1.079552588663035051, -2.039509185488725951 ) ) ;
#162646 = CARTESIAN_POINT ( 'NONE',  ( 3.784175263432405956, -1.067420458145739826, 1.879713924940962677 ) ) ;
#162647 = CARTESIAN_POINT ( 'NONE',  ( 4.628815217244971691, -1.774851831708891714, 0.7884768782448601243 ) ) ;
#162648 = CARTESIAN_POINT ( 'NONE',  ( -9.130526383799315582, 12.73969898348616070, 1.199719254218462483 ) ) ;
#162649 = CARTESIAN_POINT ( 'NONE',  ( 6.766881895623299670, -1.710433013466134744, -0.7576501205904457859 ) ) ;
#162650 =( NAMED_UNIT ( * ) SI_UNIT ( $, .STERADIAN. ) SOLID_ANGLE_UNIT ( ) );
#162651 = EDGE_CURVE ( 'NONE', #143111, #187426, #45003, .T. ) ;
#162652 = CARTESIAN_POINT ( 'NONE',  ( 4.324073113486339714, 7.195437805949965515, 1.011975886212188813 ) ) ;
#162653 = LINE ( 'NONE', #80319, #31197 ) ;
#162654 = CARTESIAN_POINT ( 'NONE',  ( 2.687227643083427534E-13, -3.232243495192088201, 3.285556943749999625 ) ) ;
#162655 = CARTESIAN_POINT ( 'NONE',  ( -1.360316468750034646, 2.619791667008062319, -0.7853790794159261068 ) ) ;
#162656 = CARTESIAN_POINT ( 'NONE',  ( 5.678361341766085424, 1.528739221709461082, 1.314999087022615587 ) ) ;
#162657 = CARTESIAN_POINT ( 'NONE',  ( -4.256897044566581911, 4.068727428190179296, 1.214306433183764966E-14 ) ) ;
#162658 =( BOUNDED_SURFACE ( )  B_SPLINE_SURFACE ( 1, 2, ( 
 ( #63226, #180186, #76274, #109917, #210535, #44872, #28601, #126176, #45936, #47000, #94690, #11263, #142382, #129389, #92560, #192140, #175928, #128328, #12325, #78405, #112055, #27521, #29673, #95757, #10199, #161810, #114187, #13400, #145594, #211590, #179122, #80545, #195368, #113116, #96825, #64299, #162874, #14454, #146642, #196432, #48076, #99993, #166059, #17646, #116301, #184427, #201730, #199604, #83730, #51247, #149822, #19792, #181233, #197482, #84804, #1392, #67453, #81606, #132536, #151952, #182291, #115243, #134658, #119506, #164991, #36044, #16582, #3522, #32861, #133599, #117372, #98937, #183369, #34974, #82664, #53371, #163945, #33918, #101045, #49125, #102124, #15520, #85875, #150893, #167135, #147690, #18720, #2454, #68530, #200661, #148748, #52310, #168193, #118440, #318, #69596, #66388, #135704, #31808, #213708, #50180, #198534, #65331, #97884, #131478, #71731, #55510, #157294, #5651, #105353, #20844, #139993, #171390, #56586, #37117, #203866, #90164, #173560, #106450, #121665, #88012, #107529, #8884, #138916, #22981, #170314, #7807, #156230, #89100, #21902, #187632, #153010, #154083, #73900, #103196, #137845, #72814, #57650, #25132, #169258, #6735, #104269, #91234, #86943, #123809, #41421, #39259, #74963, #155154, #204935, #122746, #188708, #189770, #141073, #40344, #172474, #24061, #206014, #207081, #120591, #136770, #58712, #185492, #4586, #70660, #202799, #54448, #186568, #38196, #13147, #212400, #43552, #129136, #109673, #30488, #125932, #192961, #110729, #59773, #12084, #144282, #175675, #146386, #42486, #127003, #78151, #76027, #195112, #108595, #178876, #29420, #128075, #26199, #44614, #210275, #60841, #28343, #142130, #61915, #46749, #194031, #191890, #94438, #27264, #160477, #45682, #174623, #143211, #93371, #92317, #211342, #124861, #11007, #209201, #96572, #159407, #176729, #158358, #79224, #111798, #177804, #190827, #95511, #161559, #112861, #145341, #62967, #77084, #162619, #14195, #80288, #9951, #208144, #100790, #34719, #116042, #114981, #148496, #31553, #48865, #183111, #130187, #97628, #17389, #18466, #16324, #197225, #47822, #166874, #151698, #113933, #81354, #182030, #180981, #164733, #32602, #179929, #65082, #66128, #64042, #98677, #85610, #83472, #163685, #82407, #33659, #15267, #35789, #131237, #149553, #64, #117109, #118181, #132272, #99733, #134404, #198280, #49921, #50988, #147434, #84544, #213458, #165805, #150634, #67200, #1138, #133337, #200408, #101865, #199341, #2195, #68272, #52054, #184169, #167933, #19533, #196180, #7543, #73628, #186299, #3267, #155957, #153822, #205750, #5393, #71471, #36850, #6473, #4328, #139727, #70397, #57381, #123545, #136515, #121401, #22720, #172211, #41155, #107264, #21639, #189510, #56319, #173284, #204670, #24866, #90970, #203601, #86679, #37935, #87746, #54183, #187373, #119243, #69334, #122479, #105088, #23800 ),
 ( #135445, #137584, #188440, #201467, #138648, #55254, #120323, #53110, #185227, #171126, #39004, #202534, #40074, #106186, #88834, #104009, #154892, #102934, #170054, #89905, #168994, #20593, #72550, #152746, #109409, #75766, #140805, #127814, #30218, #9689, #46473, #206817, #8619, #190564, #178608, #95238, #157032, #126732, #94175, #11815, #110468, #141874, #174357, #25935, #12873, #207883, #62697, #10747, #76818, #142938, #26998, #161287, #112596, #176469, #208938, #28079, #60573, #145071, #92043, #108337, #210005, #192692, #44346, #58451, #43288, #128858, #93104, #158100, #45415, #74701, #59506, #78949, #125663, #194840, #191625, #160214, #77891, #175414, #144012, #61647, #159146, #124606, #42220, #193769, #111531, #177538, #211074, #29149, #150377, #876, #99485, #212137, #98414, #115785, #32349, #214243, #47556, #181773, #166616, #165543, #163424, #65874, #147180, #132022, #17136, #80020, #114726, #97366, #63773, #182853, #117930, #196972, #180724, #68009, #130981, #16065, #146123, #50726, #82149, #33407, #162358, #164478, #66942, #84292, #83212, #148241, #213206, #18208, #134149, #49662, #198032, #81092, #133082, #199080, #149295, #64835, #116851, #129931, #48611, #34471, #13937, #195920, #100543, #1947, #200158, #15001, #113667, #51812, #183924, #96302, #179671, #31291, #20349, #136265, #152499, #151444, #36600, #37684, #123303, #86434, #57135, #55006, #202285, #137336, #122230, #23546, #101613, #71219, #168745, #155709, #167680, #188190, #103761, #35536, #4082, #19280, #121156, #53937, #203353, #39825, #89656, #85362, #187123, #70153, #7291, #3017, #105933, #171958, #120073, #73369, #169812, #21400, #87510, #186049, #139474, #205503, #38754, #153574, #104835, #5144, #69085, #184975, #201222, #88583, #170880, #22472, #135206, #154641, #52863, #6222, #118997, #138400, #102688, #72292, #204419, #56074, #97924, #190319, #43049, #175173, #124362, #76578, #208700, #25690, #213746, #107011, #191383, #142690, #140561, #196473, #173035, #31847, #93932, #192451, #90725, #109162, #60327, #125417, #92862, #206574, #126488, #48115, #44105, #41978, #158909, #91798, #10505, #110226, #24617, #207641, #108088, #156788, #61405, #65369, #75520, #59259, #163982, #9449, #26761, #8374, #143770, #176234, #27836, #40905, #159973, #11577, #180225, #77648, #209764, #157855, #114227, #15557, #130485, #81644, #174117, #147731, #189266, #74457, #141633, #58202, #98976, #116338, #36081, #197519, #165029, #84843, #85914, #83769, #50219, #115280, #102164, #117411, #182329, #68568, #33957, #100033, #17683, #166095, #32898, #132569, #353, #149862, #1430, #67495, #101082, #16622, #37157, #118478, #18758, #151988, #133639, #183407, #181272, #103234, #66426, #19830, #82704, #199640, #86978, #131516, #51286, #168232, #20879, #35011, #167171, #184463, #150932, #3562, #148783, #49163, #2494, #169294, #134695, #198570, #200699, #52351, #69635 ) ),
 .UNSPECIFIED., .F., .F., .T. ) 
 B_SPLINE_SURFACE_WITH_KNOTS ( ( 2, 2 ),
 ( 3, 2, 2, 2, 2, 2, 2, 2, 2, 2, 2, 2, 2, 2, 2, 2, 2, 2, 2, 2, 2, 2, 2, 2, 2, 2, 2, 2, 2, 2, 2, 2, 2, 2, 2, 2, 2, 2, 2, 2, 2, 2, 2, 2, 2, 2, 2, 2, 2, 2, 2, 2, 2, 2, 2, 2, 2, 2, 2, 2, 2, 2, 2, 2, 2, 2, 2, 2, 2, 2, 2, 2, 2, 2, 2, 2, 2, 2, 2, 2, 2, 2, 2, 2, 2, 2, 2, 2, 2, 2, 2, 2, 2, 2, 2, 2, 2, 2, 2, 2, 2, 2, 2, 2, 2, 2, 2, 2, 2, 2, 2, 2, 2, 2, 2, 2, 2, 2, 2, 2, 2, 2, 2, 2, 2, 2, 2, 2, 2, 2, 2, 2, 2, 2, 2, 2, 2, 2, 2, 2, 2, 2, 2, 2, 2, 2, 2, 2, 2, 2, 2, 2, 2, 2, 2, 2, 2, 2, 2, 2, 2, 2, 2, 2, 2, 2, 2, 2, 3 ),
 ( 0.000000000000000000, 1.000000000000000000 ),
 ( 0.000000000000000000, 0.005952380952380952051, 0.01190476190476190410, 0.01785714285714285615, 0.02380952380952380820, 0.02976190476190476025, 0.03571428571428571230, 0.04166666666666666435, 0.04761904761904761640, 0.05357142857142856845, 0.05952380952380952051, 0.06547619047619047949, 0.07142857142857142461, 0.07738095238095238360, 0.08333333333333332871, 0.08928571428571428770, 0.09523809523809523281, 0.1011904761904761918, 0.1071428571428571369, 0.1130952380952380959, 0.1190476190476190410, 0.1250000000000000000, 0.1309523809523809590, 0.1369047619047619180, 0.1428571428571428492, 0.1488095238095238082, 0.1547619047619047672, 0.1607142857142857262, 0.1666666666666666574, 0.1726190476190476164, 0.1785714285714285754, 0.1845238095238095344, 0.1904761904761904656, 0.1964285714285714246, 0.2023809523809523836, 0.2083333333333333426, 0.2142857142857142738, 0.2202380952380952328, 0.2261904761904761918, 0.2321428571428571508, 0.2380952380952380820, 0.2440476190476190410, 0.2500000000000000000, 0.2559523809523809312, 0.2619047619047619180, 0.2678571428571428492, 0.2738095238095238360, 0.2797619047619047672, 0.2857142857142856984, 0.2916666666666666852, 0.2976190476190476164, 0.3035714285714285476, 0.3095238095238095344, 0.3154761904761904656, 0.3214285714285714524, 0.3273809523809523836, 0.3333333333333333148, 0.3392857142857143016, 0.3452380952380952328, 0.3511904761904761640, 0.3571428571428571508, 0.3630952380952380820, 0.3690476190476190688, 0.3750000000000000000, 0.3809523809523809312, 0.3869047619047619180, 0.3928571428571428492, 0.3988095238095238360, 0.4047619047619047672, 0.4107142857142856984, 0.4166666666666666852, 0.4226190476190476164, 0.4285714285714285476, 0.4345238095238095344, 0.4404761904761904656, 0.4464285714285714524, 0.4523809523809523836, 0.4583333333333333148, 0.4642857142857143016, 0.4702380952380952328, 0.4761904761904761640, 0.4821428571428571508, 0.4880952380952380820, 0.4940476190476190688, 0.5000000000000000000, 0.5059523809523809312, 0.5119047619047618625, 0.5178571428571429047, 0.5238095238095238360, 0.5297619047619047672, 0.5357142857142856984, 0.5416666666666666297, 0.5476190476190476719, 0.5535714285714286031, 0.5595238095238095344, 0.5654761904761904656, 0.5714285714285713969, 0.5773809523809523281, 0.5833333333333333703, 0.5892857142857143016, 0.5952380952380952328, 0.6011904761904761640, 0.6071428571428570953, 0.6130952380952381375, 0.6190476190476190688, 0.6250000000000000000, 0.6309523809523809312, 0.6369047619047618625, 0.6428571428571429047, 0.6488095238095238360, 0.6547619047619047672, 0.6607142857142856984, 0.6666666666666666297, 0.6726190476190476719, 0.6785714285714286031, 0.6845238095238095344, 0.6904761904761904656, 0.6964285714285713969, 0.7023809523809523281, 0.7083333333333333703, 0.7142857142857143016, 0.7202380952380952328, 0.7261904761904761640, 0.7321428571428570953, 0.7380952380952381375, 0.7440476190476190688, 0.7500000000000000000, 0.7559523809523809312, 0.7619047619047618625, 0.7678571428571429047, 0.7738095238095238360, 0.7797619047619047672, 0.7857142857142856984, 0.7916666666666666297, 0.7976190476190476719, 0.8035714285714286031, 0.8095238095238095344, 0.8154761904761904656, 0.8214285714285713969, 0.8273809523809523281, 0.8333333333333333703, 0.8392857142857143016, 0.8452380952380952328, 0.8511904761904761640, 0.8571428571428570953, 0.8630952380952381375, 0.8690476190476190688, 0.8750000000000000000, 0.8809523809523809312, 0.8869047619047618625, 0.8928571428571429047, 0.8988095238095238360, 0.9047619047619047672, 0.9107142857142856984, 0.9166666666666666297, 0.9226190476190476719, 0.9285714285714286031, 0.9345238095238095344, 0.9404761904761904656, 0.9464285714285713969, 0.9523809523809523281, 0.9583333333333333703, 0.9642857142857143016, 0.9702380952380952328, 0.9761904761904761640, 0.9821428571428570953, 0.9880952380952381375, 0.9940476190476190688, 1.000000000000000000 ),
 .UNSPECIFIED. ) 
 GEOMETRIC_REPRESENTATION_ITEM ( )  RATIONAL_B_SPLINE_SURFACE ( (
 ( 1.000000000000000000, 0.8660254037844387076, 1.000000000000000000, 0.8660254037844387076, 1.000000000000000000, 0.8660254037844387076, 1.000000000000000000, 0.8660254037844387076, 1.000000000000000000, 0.8660254037844387076, 1.000000000000000000, 0.8660254037844387076, 1.000000000000000000, 0.8660254037844387076, 1.000000000000000000, 0.8660254037844387076, 1.000000000000000000, 0.8660254037844387076, 1.000000000000000000, 0.8660254037844387076, 1.000000000000000000, 0.8660254037844387076, 1.000000000000000000, 0.8660254037844387076, 1.000000000000000000, 0.8660254037844387076, 1.000000000000000000, 0.8660254037844387076, 1.000000000000000000, 0.8660254037844387076, 1.000000000000000000, 0.8660254037844387076, 1.000000000000000000, 0.8660254037844387076, 1.000000000000000000, 0.8660254037844387076, 1.000000000000000000, 0.8660254037844387076, 1.000000000000000000, 0.8660254037844387076, 1.000000000000000000, 0.8660254037844387076, 1.000000000000000000, 0.8660254037844387076, 1.000000000000000000, 0.8660254037844387076, 1.000000000000000000, 0.8660254037844387076, 1.000000000000000000, 0.8660254037844387076, 1.000000000000000000, 0.8660254037844387076, 1.000000000000000000, 0.8660254037844387076, 1.000000000000000000, 0.8660254037844387076, 1.000000000000000000, 0.8660254037844387076, 1.000000000000000000, 0.8660254037844387076, 1.000000000000000000, 0.8660254037844387076, 1.000000000000000000, 0.8660254037844387076, 1.000000000000000000, 0.8660254037844387076, 1.000000000000000000, 0.8660254037844387076, 1.000000000000000000, 0.8660254037844387076, 1.000000000000000000, 0.8660254037844387076, 1.000000000000000000, 0.8660254037844387076, 1.000000000000000000, 0.8660254037844387076, 1.000000000000000000, 0.8660254037844387076, 1.000000000000000000, 0.8660254037844387076, 1.000000000000000000, 0.8660254037844387076, 1.000000000000000000, 0.8660254037844387076, 1.000000000000000000, 0.8660254037844387076, 1.000000000000000000, 0.8660254037844387076, 1.000000000000000000, 0.8660254037844387076, 1.000000000000000000, 0.8660254037844387076, 1.000000000000000000, 0.8660254037844387076, 1.000000000000000000, 0.8660254037844387076, 1.000000000000000000, 0.8660254037844387076, 1.000000000000000000, 0.8660254037844387076, 1.000000000000000000, 0.8660254037844387076, 1.000000000000000000, 0.8660254037844387076, 1.000000000000000000, 0.8660254037844387076, 1.000000000000000000, 0.8660254037844387076, 1.000000000000000000, 0.8660254037844387076, 1.000000000000000000, 0.8660254037844387076, 1.000000000000000000, 0.8660254037844387076, 1.000000000000000000, 0.8660254037844387076, 1.000000000000000000, 0.8660254037844387076, 1.000000000000000000, 0.8660254037844387076, 1.000000000000000000, 0.8660254037844387076, 1.000000000000000000, 0.8660254037844387076, 1.000000000000000000, 0.8660254037844387076, 1.000000000000000000, 0.8660254037844387076, 1.000000000000000000, 0.8660254037844387076, 1.000000000000000000, 0.8660254037844387076, 1.000000000000000000, 0.8660254037844387076, 1.000000000000000000, 0.8660254037844387076, 1.000000000000000000, 0.8660254037844387076, 1.000000000000000000, 0.8660254037844387076, 1.000000000000000000, 0.8660254037844387076, 1.000000000000000000, 0.8660254037844387076, 1.000000000000000000, 0.8660254037844387076, 1.000000000000000000, 0.8660254037844387076, 1.000000000000000000, 0.8660254037844387076, 1.000000000000000000, 0.8660254037844387076, 1.000000000000000000, 0.8660254037844387076, 1.000000000000000000, 0.8660254037844387076, 1.000000000000000000, 0.8660254037844387076, 1.000000000000000000, 0.8660254037844387076, 1.000000000000000000, 0.8660254037844387076, 1.000000000000000000, 0.8660254037844387076, 1.000000000000000000, 0.8660254037844387076, 1.000000000000000000, 0.8660254037844387076, 1.000000000000000000, 0.8660254037844387076, 1.000000000000000000, 0.8660254037844387076, 1.000000000000000000, 0.8660254037844387076, 1.000000000000000000, 0.8660254037844387076, 1.000000000000000000, 0.8660254037844387076, 1.000000000000000000, 0.8660254037844387076, 1.000000000000000000, 0.8660254037844387076, 1.000000000000000000, 0.8660254037844387076, 1.000000000000000000, 0.8660254037844387076, 1.000000000000000000, 0.8660254037844387076, 1.000000000000000000, 0.8660254037844387076, 1.000000000000000000, 0.8660254037844387076, 1.000000000000000000, 0.8660254037844387076, 1.000000000000000000, 0.8660254037844387076, 1.000000000000000000, 0.8660254037844387076, 1.000000000000000000, 0.8660254037844387076, 1.000000000000000000, 0.8660254037844387076, 1.000000000000000000, 0.8660254037844387076, 1.000000000000000000, 0.8660254037844387076, 1.000000000000000000, 0.8660254037844387076, 1.000000000000000000, 0.8660254037844387076, 1.000000000000000000, 0.8660254037844387076, 1.000000000000000000, 0.8660254037844387076, 1.000000000000000000, 0.8660254037844387076, 1.000000000000000000, 0.8660254037844387076, 1.000000000000000000, 0.8660254037844387076, 1.000000000000000000, 0.8660254037844387076, 1.000000000000000000, 0.8660254037844387076, 1.000000000000000000, 0.8660254037844387076, 1.000000000000000000, 0.8660254037844387076, 1.000000000000000000, 0.8660254037844387076, 1.000000000000000000, 0.8660254037844387076, 1.000000000000000000, 0.8660254037844387076, 1.000000000000000000, 0.8660254037844387076, 1.000000000000000000, 0.8660254037844387076, 1.000000000000000000, 0.8660254037844387076, 1.000000000000000000, 0.8660254037844387076, 1.000000000000000000, 0.8660254037844387076, 1.000000000000000000, 0.8660254037844387076, 1.000000000000000000, 0.8660254037844387076, 1.000000000000000000, 0.8660254037844387076, 1.000000000000000000, 0.8660254037844387076, 1.000000000000000000, 0.8660254037844387076, 1.000000000000000000, 0.8660254037844387076, 1.000000000000000000, 0.8660254037844387076, 1.000000000000000000, 0.8660254037844387076, 1.000000000000000000, 0.8660254037844387076, 1.000000000000000000, 0.8660254037844387076, 1.000000000000000000, 0.8660254037844387076, 1.000000000000000000, 0.8660254037844387076, 1.000000000000000000, 0.8660254037844387076, 1.000000000000000000, 0.8660254037844387076, 1.000000000000000000, 0.8660254037844387076, 1.000000000000000000, 0.8660254037844387076, 1.000000000000000000, 0.8660254037844387076, 1.000000000000000000, 0.8660254037844387076, 1.000000000000000000, 0.8660254037844387076, 1.000000000000000000, 0.8660254037844387076, 1.000000000000000000, 0.8660254037844387076, 1.000000000000000000, 0.8660254037844387076, 1.000000000000000000, 0.8660254037844387076, 1.000000000000000000, 0.8660254037844387076, 1.000000000000000000, 0.8660254037844387076, 1.000000000000000000, 0.8660254037844387076, 1.000000000000000000, 0.8660254037844387076, 1.000000000000000000, 0.8660254037844387076, 1.000000000000000000, 0.8660254037844387076, 1.000000000000000000, 0.8660254037844387076, 1.000000000000000000, 0.8660254037844387076, 1.000000000000000000, 0.8660254037844387076, 1.000000000000000000, 0.8660254037844387076, 1.000000000000000000, 0.8660254037844387076, 1.000000000000000000, 0.8660254037844387076, 1.000000000000000000, 0.8660254037844387076, 1.000000000000000000, 0.8660254037844387076, 1.000000000000000000, 0.8660254037844387076, 1.000000000000000000, 0.8660254037844387076, 1.000000000000000000, 0.8660254037844387076, 1.000000000000000000, 0.8660254037844387076, 1.000000000000000000, 0.8660254037844387076, 1.000000000000000000, 0.8660254037844387076, 1.000000000000000000, 0.8660254037844387076, 1.000000000000000000, 0.8660254037844387076, 1.000000000000000000, 0.8660254037844387076, 1.000000000000000000),
 ( 1.000000000000000000, 0.8660254037844387076, 1.000000000000000000, 0.8660254037844387076, 1.000000000000000000, 0.8660254037844387076, 1.000000000000000000, 0.8660254037844387076, 1.000000000000000000, 0.8660254037844387076, 1.000000000000000000, 0.8660254037844387076, 1.000000000000000000, 0.8660254037844387076, 1.000000000000000000, 0.8660254037844387076, 1.000000000000000000, 0.8660254037844387076, 1.000000000000000000, 0.8660254037844387076, 1.000000000000000000, 0.8660254037844387076, 1.000000000000000000, 0.8660254037844387076, 1.000000000000000000, 0.8660254037844387076, 1.000000000000000000, 0.8660254037844387076, 1.000000000000000000, 0.8660254037844387076, 1.000000000000000000, 0.8660254037844387076, 1.000000000000000000, 0.8660254037844387076, 1.000000000000000000, 0.8660254037844387076, 1.000000000000000000, 0.8660254037844387076, 1.000000000000000000, 0.8660254037844387076, 1.000000000000000000, 0.8660254037844387076, 1.000000000000000000, 0.8660254037844387076, 1.000000000000000000, 0.8660254037844387076, 1.000000000000000000, 0.8660254037844387076, 1.000000000000000000, 0.8660254037844387076, 1.000000000000000000, 0.8660254037844387076, 1.000000000000000000, 0.8660254037844387076, 1.000000000000000000, 0.8660254037844387076, 1.000000000000000000, 0.8660254037844387076, 1.000000000000000000, 0.8660254037844387076, 1.000000000000000000, 0.8660254037844387076, 1.000000000000000000, 0.8660254037844387076, 1.000000000000000000, 0.8660254037844387076, 1.000000000000000000, 0.8660254037844387076, 1.000000000000000000, 0.8660254037844387076, 1.000000000000000000, 0.8660254037844387076, 1.000000000000000000, 0.8660254037844387076, 1.000000000000000000, 0.8660254037844387076, 1.000000000000000000, 0.8660254037844387076, 1.000000000000000000, 0.8660254037844387076, 1.000000000000000000, 0.8660254037844387076, 1.000000000000000000, 0.8660254037844387076, 1.000000000000000000, 0.8660254037844387076, 1.000000000000000000, 0.8660254037844387076, 1.000000000000000000, 0.8660254037844387076, 1.000000000000000000, 0.8660254037844387076, 1.000000000000000000, 0.8660254037844387076, 1.000000000000000000, 0.8660254037844387076, 1.000000000000000000, 0.8660254037844387076, 1.000000000000000000, 0.8660254037844387076, 1.000000000000000000, 0.8660254037844387076, 1.000000000000000000, 0.8660254037844387076, 1.000000000000000000, 0.8660254037844387076, 1.000000000000000000, 0.8660254037844387076, 1.000000000000000000, 0.8660254037844387076, 1.000000000000000000, 0.8660254037844387076, 1.000000000000000000, 0.8660254037844387076, 1.000000000000000000, 0.8660254037844387076, 1.000000000000000000, 0.8660254037844387076, 1.000000000000000000, 0.8660254037844387076, 1.000000000000000000, 0.8660254037844387076, 1.000000000000000000, 0.8660254037844387076, 1.000000000000000000, 0.8660254037844387076, 1.000000000000000000, 0.8660254037844387076, 1.000000000000000000, 0.8660254037844387076, 1.000000000000000000, 0.8660254037844387076, 1.000000000000000000, 0.8660254037844387076, 1.000000000000000000, 0.8660254037844387076, 1.000000000000000000, 0.8660254037844387076, 1.000000000000000000, 0.8660254037844387076, 1.000000000000000000, 0.8660254037844387076, 1.000000000000000000, 0.8660254037844387076, 1.000000000000000000, 0.8660254037844387076, 1.000000000000000000, 0.8660254037844387076, 1.000000000000000000, 0.8660254037844387076, 1.000000000000000000, 0.8660254037844387076, 1.000000000000000000, 0.8660254037844387076, 1.000000000000000000, 0.8660254037844387076, 1.000000000000000000, 0.8660254037844387076, 1.000000000000000000, 0.8660254037844387076, 1.000000000000000000, 0.8660254037844387076, 1.000000000000000000, 0.8660254037844387076, 1.000000000000000000, 0.8660254037844387076, 1.000000000000000000, 0.8660254037844387076, 1.000000000000000000, 0.8660254037844387076, 1.000000000000000000, 0.8660254037844387076, 1.000000000000000000, 0.8660254037844387076, 1.000000000000000000, 0.8660254037844387076, 1.000000000000000000, 0.8660254037844387076, 1.000000000000000000, 0.8660254037844387076, 1.000000000000000000, 0.8660254037844387076, 1.000000000000000000, 0.8660254037844387076, 1.000000000000000000, 0.8660254037844387076, 1.000000000000000000, 0.8660254037844387076, 1.000000000000000000, 0.8660254037844387076, 1.000000000000000000, 0.8660254037844387076, 1.000000000000000000, 0.8660254037844387076, 1.000000000000000000, 0.8660254037844387076, 1.000000000000000000, 0.8660254037844387076, 1.000000000000000000, 0.8660254037844387076, 1.000000000000000000, 0.8660254037844387076, 1.000000000000000000, 0.8660254037844387076, 1.000000000000000000, 0.8660254037844387076, 1.000000000000000000, 0.8660254037844387076, 1.000000000000000000, 0.8660254037844387076, 1.000000000000000000, 0.8660254037844387076, 1.000000000000000000, 0.8660254037844387076, 1.000000000000000000, 0.8660254037844387076, 1.000000000000000000, 0.8660254037844387076, 1.000000000000000000, 0.8660254037844387076, 1.000000000000000000, 0.8660254037844387076, 1.000000000000000000, 0.8660254037844387076, 1.000000000000000000, 0.8660254037844387076, 1.000000000000000000, 0.8660254037844387076, 1.000000000000000000, 0.8660254037844387076, 1.000000000000000000, 0.8660254037844387076, 1.000000000000000000, 0.8660254037844387076, 1.000000000000000000, 0.8660254037844387076, 1.000000000000000000, 0.8660254037844387076, 1.000000000000000000, 0.8660254037844387076, 1.000000000000000000, 0.8660254037844387076, 1.000000000000000000, 0.8660254037844387076, 1.000000000000000000, 0.8660254037844387076, 1.000000000000000000, 0.8660254037844387076, 1.000000000000000000, 0.8660254037844387076, 1.000000000000000000, 0.8660254037844387076, 1.000000000000000000, 0.8660254037844387076, 1.000000000000000000, 0.8660254037844387076, 1.000000000000000000, 0.8660254037844387076, 1.000000000000000000, 0.8660254037844387076, 1.000000000000000000, 0.8660254037844387076, 1.000000000000000000, 0.8660254037844387076, 1.000000000000000000, 0.8660254037844387076, 1.000000000000000000, 0.8660254037844387076, 1.000000000000000000, 0.8660254037844387076, 1.000000000000000000, 0.8660254037844387076, 1.000000000000000000, 0.8660254037844387076, 1.000000000000000000, 0.8660254037844387076, 1.000000000000000000, 0.8660254037844387076, 1.000000000000000000, 0.8660254037844387076, 1.000000000000000000, 0.8660254037844387076, 1.000000000000000000, 0.8660254037844387076, 1.000000000000000000, 0.8660254037844387076, 1.000000000000000000, 0.8660254037844387076, 1.000000000000000000, 0.8660254037844387076, 1.000000000000000000, 0.8660254037844387076, 1.000000000000000000, 0.8660254037844387076, 1.000000000000000000, 0.8660254037844387076, 1.000000000000000000, 0.8660254037844387076, 1.000000000000000000, 0.8660254037844387076, 1.000000000000000000, 0.8660254037844387076, 1.000000000000000000, 0.8660254037844387076, 1.000000000000000000, 0.8660254037844387076, 1.000000000000000000, 0.8660254037844387076, 1.000000000000000000, 0.8660254037844387076, 1.000000000000000000, 0.8660254037844387076, 1.000000000000000000, 0.8660254037844387076, 1.000000000000000000, 0.8660254037844387076, 1.000000000000000000, 0.8660254037844387076, 1.000000000000000000, 0.8660254037844387076, 1.000000000000000000, 0.8660254037844387076, 1.000000000000000000, 0.8660254037844387076, 1.000000000000000000, 0.8660254037844387076, 1.000000000000000000, 0.8660254037844387076, 1.000000000000000000, 0.8660254037844387076, 1.000000000000000000, 0.8660254037844387076, 1.000000000000000000, 0.8660254037844387076, 1.000000000000000000, 0.8660254037844387076, 1.000000000000000000) ) ) 
 REPRESENTATION_ITEM ( '' )  SURFACE ( )  );
#162659 = CARTESIAN_POINT ( 'NONE',  ( 6.909851844459134362, 11.21324425184434936, -0.7998128361456291469 ) ) ;
#162660 = APPLICATION_CONTEXT ( 'automotive_design' ) ;
#162661 = DIRECTION ( 'NONE',  ( 0.000000000000000000, 0.000000000000000000, 1.000000000000000000 ) ) ;
#162663 = CARTESIAN_POINT ( 'NONE',  ( -6.781144757626061725, -7.161464053357567749, 6.776370306708065172 ) ) ;
#162662 = CARTESIAN_POINT ( 'NONE',  ( 2.965264444195826243, 0.2674972279559268973, -1.805858685475017378 ) ) ;
#162664 = CARTESIAN_POINT ( 'NONE',  ( -9.000007961041697868, 1.000000000000000888, -7.937244906211844864 ) ) ;
#162665 = EDGE_LOOP ( 'NONE', ( #173602, #205459, #34352, #117167 ) ) ;
#162666 = CARTESIAN_POINT ( 'NONE',  ( -3.648552735408985725, 7.270745601370182776, -0.7216878364870458196 ) ) ;
#162667 = CARTESIAN_POINT ( 'NONE',  ( -1.642778471874998480, -3.988541666188710089, 2.845375778867863303 ) ) ;
#162668 = CARTESIAN_POINT ( 'NONE',  ( -7.811469059767924605, 12.26513100303794168, -0.7998128361456281477 ) ) ;
#162669 = CARTESIAN_POINT ( 'NONE',  ( 6.498695841808301843, -1.981098178724240322, -0.3918999010058578092 ) ) ;
#162670 = CARTESIAN_POINT ( 'NONE',  ( 1.383610671357866639, 0.1525377206293351273, -2.115047022047947589 ) ) ;
#162671 = ORIENTED_EDGE ( 'NONE', *, *, #64463, .T. ) ;
#162672 = CARTESIAN_POINT ( 'NONE',  ( -5.261446130555064826, 8.296048364692991228, 1.199719254218452935 ) ) ;
#162673 = CARTESIAN_POINT ( 'NONE',  ( 2.201794467188260995, 0.7177229581568910222, -1.717183780122087056 ) ) ;
#162674 = CARTESIAN_POINT ( 'NONE',  ( 4.650610384687404952, 5.384465856012134566, 1.199719254218462483 ) ) ;
#162675 = CARTESIAN_POINT ( 'NONE',  ( 6.684453628662900826, -2.020573120193806638, -0.4047117086388977714 ) ) ;
#162676 = CARTESIAN_POINT ( 'NONE',  ( 6.205703963786828758, 1.882472927010571118, 0.7231429968634556227 ) ) ;
#162677 = ORIENTED_EDGE ( 'NONE', *, *, #118655, .F. ) ;
#162678 = ORIENTED_EDGE ( 'NONE', *, *, #117402, .F. ) ;
#162679 = CARTESIAN_POINT ( 'NONE',  ( 0.07419657009811017612, 6.490528840037850244, -3.104513093580470340 ) ) ;
#162680 = CARTESIAN_POINT ( 'NONE',  ( 8.154303043976348420, 8.478051404252736845, 0.7998128361456281477 ) ) ;
#162682 = CARTESIAN_POINT ( 'NONE',  ( 0.07680821025394034274, 2.052785608010514018, -2.228496998325917744 ) ) ;
#162681 = CARTESIAN_POINT ( 'NONE',  ( -4.145761110728687804, 8.058748072483927771, -0.7998128361456481317 ) ) ;
#162683 = CARTESIAN_POINT ( 'NONE',  ( 6.410638904775656677, 6.895589754593423493, 0.7569561588358000304 ) ) ;
#162684 = CARTESIAN_POINT ( 'NONE',  ( 6.257185446134499784, -2.006139278912861368, -0.2004013049526700285 ) ) ;
#162685 = CARTESIAN_POINT ( 'NONE',  ( 4.558453444723221892, -1.645810703501834560, -0.8254300276653583346 ) ) ;
#162686 = DIRECTION ( 'NONE',  ( -0.7592566023652990159, -0.6507913734559659380, 0.000000000000000000 ) ) ;
#162687 = CARTESIAN_POINT ( 'NONE',  ( 3.844573663522454332, 2.296428955072826295, 0.2277027427845106922 ) ) ;
#162688 = CARTESIAN_POINT ( 'NONE',  ( 5.234329823327693809, 8.264412672927770487, 1.199719254218451159 ) ) ;
#162689 = CARTESIAN_POINT ( 'NONE',  ( 5.431013727915853906, 0.1530101862373678123, 2.156222312673663488 ) ) ;
#162690 = CARTESIAN_POINT ( 'NONE',  ( 8.471147050440139381, 8.777426401801974976, -0.7998128361456281477 ) ) ;
#162691 = CARTESIAN_POINT ( 'NONE',  ( 1.347104335016526599, 0.5619601930287048130, -1.858996895088180556 ) ) ;
#162692 = CARTESIAN_POINT ( 'NONE',  ( -3.249150368769345043, 6.942425863539538611, 0.7998128361456341429 ) ) ;
#162693 = ORIENTED_EDGE ( 'NONE', *, *, #199649, .T. ) ;
#162694 = ADVANCED_FACE ( 'NONE', ( #117883 ), #14056, .T. ) ;
#162695 = COLOUR_RGB ( '', 0.08235294, 0.09019608, 0.10196078) ;
#162696 = CARTESIAN_POINT ( 'NONE',  ( 5.114793989753786185, 0.7273159113986256141, -2.180329384352611033 ) ) ;
#162697 = DIRECTION ( 'NONE',  ( 0.000000000000000000, -1.000000000000000000, 0.000000000000000000 ) ) ;
#162698 = CARTESIAN_POINT ( 'NONE',  ( -4.630991987519598396, 7.560518531151607213, 1.199719254218452935 ) ) ;
#162699 = CARTESIAN_POINT ( 'NONE',  ( 4.768341783539651324, -1.221614081569386334, 1.416756073533788518 ) ) ;
#162702 = CARTESIAN_POINT ( 'NONE',  ( -6.608673532018475960, 6.674816973635147477, -0.7998128361456362523 ) ) ;
#162701 = CARTESIAN_POINT ( 'NONE',  ( -1.402160292154681736E-14, -0.2562499993171780122, 1.732050807568877637 ) ) ;
#162700 = CARTESIAN_POINT ( 'NONE',  ( 1.300873410958070409, -0.2835801433653042380, -1.891145142470892715 ) ) ;
#162703 = CARTESIAN_POINT ( 'NONE',  ( 2.895379187063460424, 1.892502543702856865, -1.135010264495312837 ) ) ;
#162704 = CARTESIAN_POINT ( 'NONE',  ( 6.883263157960373135, 2.058310207169287143, 2.252834201749584153 ) ) ;
#162705 = CARTESIAN_POINT ( 'NONE',  ( -11.33772463945036968, 10.90000000000000036, -3.600000000000002309 ) ) ;
#162706 = CARTESIAN_POINT ( 'NONE',  ( 6.170369307550815030, 8.292126506933040986, 1.443375672974064550 ) ) ;
#162707 = CARTESIAN_POINT ( 'NONE',  ( -2.462777459176719308, 6.024990802348131780, -0.7998128361456281477 ) ) ;
#162708 = CARTESIAN_POINT ( 'NONE',  ( -4.923019175093582334, 8.757623114335565617, 0.7216878364870267237 ) ) ;
#162709 = CARTESIAN_POINT ( 'NONE',  ( 1.335163258876404857, -1.783904897583366012, 0.8392522581757311251 ) ) ;
#162710 = CARTESIAN_POINT ( 'NONE',  ( 0.7457024085506950284, -1.977219658456253359, 1.189539768987533330 ) ) ;
#162711 = CARTESIAN_POINT ( 'NONE',  ( 2.734756269166933151, -1.876540383875524576, -0.5722209215143353456 ) ) ;
#162712 = CARTESIAN_POINT ( 'NONE',  ( 5.120015017920454881, 2.040880116263335431, -0.2974388374509198685 ) ) ;
#162713 = CARTESIAN_POINT ( 'NONE',  ( 5.016153647376212277, 5.914896012436124728, 1.082531754730558626 ) ) ;
#162714 = CARTESIAN_POINT ( 'NONE',  ( 6.527324610336440180, 6.579909898339485252, 0.7998128361456331437 ) ) ;
#162715 = VERTEX_POINT ( 'NONE', #54956 ) ;
#162716 = CARTESIAN_POINT ( 'NONE',  ( -1.201851678989727383E-14, 5.509375000341415252, -1.575800808251660134 ) ) ;
#162717 = CARTESIAN_POINT ( 'NONE',  ( 0.000000000000000000, -1.600000000000000755, 0.000000000000000000 ) ) ;
#162718 = CARTESIAN_POINT ( 'NONE',  ( 2.968872451268290913, 5.447139712246216625, -1.082531754730543971 ) ) ;
#162719 = CARTESIAN_POINT ( 'NONE',  ( 1.446384731406271218, -0.9785283779201507937, 1.938150590114567473 ) ) ;
#162721 = DIRECTION ( 'NONE',  ( 0.000000000000000000, 1.000000000000000000, 0.000000000000000000 ) ) ;
#162720 = CARTESIAN_POINT ( 'NONE',  ( -1.938011383317839176E-15, -9.900000000000005684, -10.91970695577503214 ) ) ;
#162722 = CARTESIAN_POINT ( 'NONE',  ( 11.44779964734654598, 10.99810470129597917, -3.599999963171534478 ) ) ;
#162724 = CARTESIAN_POINT ( 'NONE',  ( 0.3999999999999758193, 3.000000000029069636, -2.023857702507768419 ) ) ;
#162723 = B_SPLINE_CURVE_WITH_KNOTS ( 'NONE', 3,
 ( #22784, #6540, #137650, #121470 ),
 .UNSPECIFIED., .F., .F.,
 ( 4, 4 ),
 ( 0.000000000000000000, 6.033646489354581229E-05 ),
 .UNSPECIFIED. ) ;
#162725 = CARTESIAN_POINT ( 'NONE',  ( 2.213927045526514537, -0.8776910013945339317, -1.651823421649289081 ) ) ;
#162726 = CARTESIAN_POINT ( 'NONE',  ( 6.292270065666691892, -2.150519007954437622, -0.2187886337903441336 ) ) ;
#162727 = CARTESIAN_POINT ( 'NONE',  ( -6.133411998150831046, 5.998805638374869353, -0.1291943307598683033 ) ) ;
#162729 = CARTESIAN_POINT ( 'NONE',  ( 6.727182134110193168, 4.701113012587437190, 2.373661997258198486 ) ) ;
#162728 = FACE_OUTER_BOUND ( 'NONE', #80142, .T. ) ;
#162730 = CARTESIAN_POINT ( 'NONE',  ( -1.364683531250014514, -0.2614583329919080157, -0.7879004041258359514 ) ) ;
#162731 = CARTESIAN_POINT ( 'NONE',  ( 2.174333686202088334, 0.8191313854410250395, 1.728107290330855639 ) ) ;
#162732 = CARTESIAN_POINT ( 'NONE',  ( 3.713518252986651724, -1.743675808792734205, 0.3021571867034832382 ) ) ;
#162733 = CARTESIAN_POINT ( 'NONE',  ( 2.121601645288184290, -0.4173985973947492711, 1.866012167355892704 ) ) ;
#162734 = CARTESIAN_POINT ( 'NONE',  ( -6.389970470742427189, 6.349387058821269747, -0.7998128361456291469 ) ) ;
#162736 = CARTESIAN_POINT ( 'NONE',  ( 5.607027416250175200, -0.04201266709560196738, 1.915314589656505362 ) ) ;
#162735 = CARTESIAN_POINT ( 'NONE',  ( 7.564733433744389224, -6.863455982311506887, 7.986233326679982092 ) ) ;
#162737 = CARTESIAN_POINT ( 'NONE',  ( 6.707475516188797116, -1.580950341439198992, -1.174378316608926331 ) ) ;
#162738 = CARTESIAN_POINT ( 'NONE',  ( 1.499999999999989120, 4.504166666666688634, 0.8660254037844524744 ) ) ;
#162739 = CARTESIAN_POINT ( 'NONE',  ( 2.601940685209406467, 1.502730264585940168, 1.496503045097858919 ) ) ;
#162740 = DIRECTION ( 'NONE',  ( -0.6507913734559640506, -0.7592566023653003482, 0.000000000000000000 ) ) ;
#162741 = CARTESIAN_POINT ( 'NONE',  ( 4.803500792215161574, -0.4985019455652460740, 1.802925825644098534 ) ) ;
#162743 = EDGE_LOOP ( 'NONE', ( #10406, #22985, #194981, #59779, #3935, #14794, #190994, #169427, #176521 ) ) ;
#162742 = CARTESIAN_POINT ( 'NONE',  ( 0.7854531640391904102, 1.224056292049885419, 1.354719642434290439 ) ) ;
#162745 = DIRECTION ( 'NONE',  ( 0.000000000000000000, 0.000000000000000000, -1.000000000000000000 ) ) ;
#162744 = CARTESIAN_POINT ( 'NONE',  ( 4.160898416275903067, -1.636102012888400292, 1.481223685352812680 ) ) ;
#162746 = CARTESIAN_POINT ( 'NONE',  ( -1.364683531250014514, -0.7614583329919104582, -0.7879004041258359514 ) ) ;
#162747 = CARTESIAN_POINT ( 'NONE',  ( 2.172402883950707686, -0.9704110660942105726, -1.820128386451558500 ) ) ;
#162748 = CARTESIAN_POINT ( 'NONE',  ( 4.801558957534076022, 8.753569217098425170, 0.7998128361456462443 ) ) ;
#162749 = B_SPLINE_CURVE_WITH_KNOTS ( 'NONE', 3,
 ( #197770, #178358, #66672, #198824, #78695, #46229 ),
 .UNSPECIFIED., .F., .F.,
 ( 4, 2, 4 ),
 ( 0.000000000000000000, 0.002109688543090480761, 0.004219377086180961522 ),
 .UNSPECIFIED. ) ;
#162750 = CARTESIAN_POINT ( 'NONE',  ( -7.720478407978036195, 11.09464301169468037, -1.199719254218446718 ) ) ;
#162751 = CARTESIAN_POINT ( 'NONE',  ( 11.97929049433705373, 13.88000000000000078, 0.7046979865771783036 ) ) ;
#162752 = CARTESIAN_POINT ( 'NONE',  ( 9.673906298550626559, 11.24497775551929557, 1.199719254218452047 ) ) ;
#162753 = CARTESIAN_POINT ( 'NONE',  ( 11.89942855770814312, 11.29999999999999893, -0.7000000000000009548 ) ) ;
#162754 = CARTESIAN_POINT ( 'NONE',  ( 1.000000000000001554, 5.868705557303652398, -4.125226524755055024 ) ) ;
#162755 = CARTESIAN_POINT ( 'NONE',  ( 7.452141709366786770, 8.723195411463290583, 1.199719254218452047 ) ) ;
#162756 = VERTEX_POINT ( 'NONE', #118950 ) ;
#162757 = CARTESIAN_POINT ( 'NONE',  ( 4.545415791725802457, 1.850806902094417783, -0.9279678557222792445 ) ) ;
#162758 = CARTESIAN_POINT ( 'NONE',  ( -1.500000000000011324, 5.420833333333356485, 0.8660254037844403729 ) ) ;
#162759 = CARTESIAN_POINT ( 'NONE',  ( 2.899875653925917174, -0.6810940995312758650, 2.051530325002319799 ) ) ;
#162760 = CARTESIAN_POINT ( 'NONE',  ( -5.764421489320544545, 7.269302474779911982, -1.197982331091128616 ) ) ;
#162761 = CARTESIAN_POINT ( 'NONE',  ( 1.805337931753002501, 1.756199045189226204, -0.9973023101699033388 ) ) ;
#162762 = VERTEX_POINT ( 'NONE', #85314 ) ;
#162764 = CARTESIAN_POINT ( 'NONE',  ( 6.155038550924133212, 10.12470270947942730, 0.7216878364870438212 ) ) ;
#162763 = CARTESIAN_POINT ( 'NONE',  ( 0.07479286986305369589, 0.2526433113205875935, -1.890777245541554574 ) ) ;
#162765 = CARTESIAN_POINT ( 'NONE',  ( -3.648552735408985725, 7.270745601370182776, -0.7216878364870458196 ) ) ;
#162766 = CARTESIAN_POINT ( 'NONE',  ( -0.1531117392989979065, -1.803405091603600185, -0.9023890051431044945 ) ) ;
#162767 = CARTESIAN_POINT ( 'NONE',  ( 5.144143540903125533, 0.6357783856077160456, 2.097287126430439130 ) ) ;
#162768 = CARTESIAN_POINT ( 'NONE',  ( -0.7500000000000215383, 5.222916667349482012, 1.299038105676671107 ) ) ;
#162769 = CARTESIAN_POINT ( 'NONE',  ( 4.148624843374196125, 1.876505540506741010, 0.3678670841067503416 ) ) ;
#162770 = CARTESIAN_POINT ( 'NONE',  ( -5.115504031057831469, 4.862509545855891346, 0.7998128361456341429 ) ) ;
#162771 = CARTESIAN_POINT ( 'NONE',  ( 6.792271770322100721, 7.026664608238323950, -0.7216878364870257245 ) ) ;
#162773 = CARTESIAN_POINT ( 'NONE',  ( 2.442982655898734645, -1.755780842375562312, -0.9913809985205720432 ) ) ;
#162772 = CARTESIAN_POINT ( 'NONE',  ( -9.788623718942277563, 10.52240854829523187, 1.040834085586084257E-14 ) ) ;
#162774 = CARTESIAN_POINT ( 'NONE',  ( 0.6823417656249969321, 12.83854166700806942, -1.181850606188757036 ) ) ;
#162775 = CARTESIAN_POINT ( 'NONE',  ( -3.494969737272722643, 7.299491470118629088, -0.7998128361456481317 ) ) ;
#162776 = CARTESIAN_POINT ( 'NONE',  ( 5.104412161113025093, -0.5839786719442441321, -1.623048794067801781 ) ) ;
#162777 = CARTESIAN_POINT ( 'NONE',  ( 0.1405533004714799583, 1.991423289015941345, -2.694406653617386294 ) ) ;
#162778 = CARTESIAN_POINT ( 'NONE',  ( 9.164948653157988900, 11.71552606681625619, -1.443375672974057666 ) ) ;
#162779 = CARTESIAN_POINT ( 'NONE',  ( -6.716119544743476943, -7.217450603038121137, -6.719405205105408285 ) ) ;
#162780 = CARTESIAN_POINT ( 'NONE',  ( 4.487912541323413329, 5.194651705420806564, 1.199719254218462483 ) ) ;
#162781 = DIRECTION ( 'NONE',  ( 1.000000000000000000, 1.725633230170963762E-31, 8.638326563840814399E-31 ) ) ;
#162782 = VERTEX_POINT ( 'NONE', #121108 ) ;
#162783 = CARTESIAN_POINT ( 'NONE',  ( 0.2861044793709514589, -1.271156181823060560, -1.634742764404631066 ) ) ;
#162784 = ORIENTED_EDGE ( 'NONE', *, *, #62145, .F. ) ;
#162785 = CARTESIAN_POINT ( 'NONE',  ( 4.986864056229866726, -1.707513420791425540, -0.6052512474536574372 ) ) ;
#162786 = CARTESIAN_POINT ( 'NONE',  ( 3.881377115262159894, 7.750300077773022878, 0.7998128361456271485 ) ) ;
#162787 = DIRECTION ( 'NONE',  ( 0.000000000000000000, 0.000000000000000000, 1.000000000000000000 ) ) ;
#162788 = CARTESIAN_POINT ( 'NONE',  ( 5.725234622465176670, 1.600757532941178063, 0.8479277756611166561 ) ) ;
#162789 = CARTESIAN_POINT ( 'NONE',  ( 4.950135482320912494, 6.868520377498098739, -1.443375672974068769 ) ) ;
#162790 = CARTESIAN_POINT ( 'NONE',  ( 7.777446446097294519, -5.502990254781792601, -7.779015489124648575 ) ) ;
#162791 = CARTESIAN_POINT ( 'NONE',  ( 2.800927341068761844, 1.851789894747071008, 1.171597702228709181 ) ) ;
#162792 = ORIENTED_EDGE ( 'NONE', *, *, #89086, .T. ) ;
#162793 = EDGE_CURVE ( 'NONE', #28009, #173308, #8919, .T. ) ;
#162795 = CARTESIAN_POINT ( 'NONE',  ( 9.562578416340237197, 10.05076299535211781, 0.7998128361456462443 ) ) ;
#162794 = CARTESIAN_POINT ( 'NONE',  ( 6.865680895677650497, -0.4029405758906497437, 1.823372528724865438 ) ) ;
#162796 = CARTESIAN_POINT ( 'NONE',  ( 4.622610566699385082, 0.3315282304991398754, 1.886534565956134335 ) ) ;
#162797 = CARTESIAN_POINT ( 'NONE',  ( 0.000000000000000000, 8.920000000000001705, 0.000000000000000000 ) ) ;
#162798 = SURFACE_SIDE_STYLE ('',( #46922 ) ) ;
#162799 = CARTESIAN_POINT ( 'NONE',  ( -1.364683531250014514, -0.4697916663252449943, 0.7879004041258379498 ) ) ;
#162800 = CARTESIAN_POINT ( 'NONE',  ( 5.341549334104194635, 6.294524313618772737, 1.082531754730558626 ) ) ;
#162801 = CARTESIAN_POINT ( 'NONE',  ( -9.341204650135658483, 10.00041963468749984, 1.040834085586084257E-14 ) ) ;
#162802 = CARTESIAN_POINT ( 'NONE',  ( 1.938557520917514987, 2.138169252768943984, 0.3173444169591658204 ) ) ;
#162803 = CARTESIAN_POINT ( 'NONE',  ( -6.608673532018475960, 6.674816973635147477, -0.7998128361456362523 ) ) ;
#162804 = CARTESIAN_POINT ( 'NONE',  ( 4.960304097753311936, 6.880383762169266504, 1.599625672291268286 ) ) ;
#162805 = CARTESIAN_POINT ( 'NONE',  ( 2.467563089314188662, 1.790814366166630034, -0.3536809140580049471 ) ) ;
#162806 = CARTESIAN_POINT ( 'NONE',  ( -3.090368948911150770, 5.692848642783215674, 1.199719254218462483 ) ) ;
#162807 = CARTESIAN_POINT ( 'NONE',  ( 4.752862199841776381, -1.465721779273346570, 1.088108411805274622 ) ) ;
#162808 = EDGE_CURVE ( 'NONE', #129260, #76748, #176973, .T. ) ;
#162809 = CARTESIAN_POINT ( 'NONE',  ( 13.13868652300558715, 6.588164048981460574, -1.077943021382721245 ) ) ;
#162810 = CARTESIAN_POINT ( 'NONE',  ( 2.531394148431935776, -0.1834752923718513118, 1.903540536635806912 ) ) ;
#162811 = VERTEX_POINT ( 'NONE', #24569 ) ;
#162812 = CARTESIAN_POINT ( 'NONE',  ( 3.367590298639517421, -0.3867537717311599343, 1.931019599036578160 ) ) ;
#162813 = EDGE_LOOP ( 'NONE', ( #181970, #202290, #138289, #13244 ) ) ;
#162814 = CARTESIAN_POINT ( 'NONE',  ( 4.985854738014197984, -1.927824157794202353, -0.2341192097771953584 ) ) ;
#162815 = EDGE_LOOP ( 'NONE', ( #32769, #20881, #187568, #160826 ) ) ;
#162816 = CARTESIAN_POINT ( 'NONE',  ( -5.237192476628793614, 9.332084666034067055, 0.7998128361456291469 ) ) ;
#162818 = CARTESIAN_POINT ( 'NONE',  ( 4.799148092389167175, -0.2621723519393297508, -2.104289960152181393 ) ) ;
#162817 = CARTESIAN_POINT ( 'NONE',  ( 6.343235766347262938, 8.493804042195527870, -1.599625672291281386 ) ) ;
#162819 = MANIFOLD_SOLID_BREP ( 'Sweep1[10]', #191758 ) ;
#162820 = CARTESIAN_POINT ( 'NONE',  ( 10.97030176249251099, 9.799999999999982947, 1.695215491223429183 ) ) ;
#162821 = CARTESIAN_POINT ( 'NONE',  ( 2.613799471529183460, -0.5979904443059110841, 1.816458080996792068 ) ) ;
#162822 = CARTESIAN_POINT ( 'NONE',  ( 5.456969279648811622, 6.453098228331718644, -1.278498092073777626 ) ) ;
#162823 = CARTESIAN_POINT ( 'NONE',  ( 6.983263157960366563, 2.446371134953594151, 2.328889586965996905 ) ) ;
#162824 = ORIENTED_EDGE ( 'NONE', *, *, #12707, .F. ) ;
#162825 = CARTESIAN_POINT ( 'NONE',  ( 3.203469434578891661, 6.959407783642502565, -0.7998128361456362523 ) ) ;
#162826 = CARTESIAN_POINT ( 'NONE',  ( 4.793612393603923216, 1.877549684267119101, -0.7266104139797191497 ) ) ;
#162827 = CARTESIAN_POINT ( 'NONE',  ( 0.08118383494905327680, -9.908729948657658326, 9.499653137018322369 ) ) ;
#162828 = CARTESIAN_POINT ( 'NONE',  ( 4.705575438601840688, -0.4840451379145363497, 1.760283039881085809 ) ) ;
#162829 = CARTESIAN_POINT ( 'NONE',  ( 1.082579992370054311, 1.234693400583252609, -1.661741702728709802 ) ) ;
#162830 = CARTESIAN_POINT ( 'NONE',  ( -8.026063749610056419, 10.38682701267698150, -1.443375672974059665 ) ) ;
#162831 = CARTESIAN_POINT ( 'NONE',  ( -6.169688749744446810, 7.059909438329341036, 1.079748085779270950 ) ) ;
#162832 = CARTESIAN_POINT ( 'NONE',  ( 3.475000000000000533, -2.902083332377417779, -2.006292185433951047 ) ) ;
#162833 = CARTESIAN_POINT ( 'NONE',  ( 5.524238439434661530, 1.113281918156138639, -1.503147240406087271 ) ) ;
#162834 = CARTESIAN_POINT ( 'NONE',  ( 5.099838337034727331, 9.101561826515851550, -0.7998128361456281477 ) ) ;
#162835 = CARTESIAN_POINT ( 'NONE',  ( -3.574546055497324293, 7.322054164722185732, 0.7998128361456341429 ) ) ;
#162836 = AXIS2_PLACEMENT_3D ( 'NONE', #39248, #120580, #188696 ) ;
#162837 = CARTESIAN_POINT ( 'NONE',  ( 1.364683531249996529, 10.77604166700806765, 0.7879004041258405033 ) ) ;
#162838 = CARTESIAN_POINT ( 'NONE',  ( -4.791917227426195858, 7.677988301050826969, -1.199719254218452047 ) ) ;
#162840 = CARTESIAN_POINT ( 'NONE',  ( -4.462041952228957165, 5.338708711422782471, -1.082531754730549967 ) ) ;
#162839 = CARTESIAN_POINT ( 'NONE',  ( -11.97929049433705373, 11.37999999999999901, -0.7046979865771821894 ) ) ;
#162841 = CARTESIAN_POINT ( 'NONE',  ( -4.608882153641705059, 7.464447381635583412, -1.199719254218452047 ) ) ;
#162842 = CARTESIAN_POINT ( 'NONE',  ( 1.780221101387355009, -1.146701191353172611, -1.723467693327894068 ) ) ;
#162843 = CARTESIAN_POINT ( 'NONE',  ( 2.161849840330143824, 1.305120488479810659, 1.667033946717882742 ) ) ;
#162844 = CARTESIAN_POINT ( 'NONE',  ( 7.130698725783555680, 10.40656671580112658, 1.199719254218460707 ) ) ;
#162845 = CARTESIAN_POINT ( 'NONE',  ( 0.000000000000000000, 2.800000000000024691, 1.214306433183764966E-14 ) ) ;
#162846 = CARTESIAN_POINT ( 'NONE',  ( 1.041781249306489965, 1.318715992218882693, 1.462978117936466926 ) ) ;
#162847 = CARTESIAN_POINT ( 'NONE',  ( 5.168313817042160530, 6.667327647676385638, 1.400930397336812572 ) ) ;
#162848 = CARTESIAN_POINT ( 'NONE',  ( 3.985733972737593778, 6.633478153960411738, -1.082531754730548412 ) ) ;
#162850 = CARTESIAN_POINT ( 'NONE',  ( 0.000000000000000000, 2.800000000000024691, 1.214306433183764966E-14 ) ) ;
#162849 = CARTESIAN_POINT ( 'NONE',  ( -3.475000000000000533, -3.849999999999999201, 0.000000000000000000 ) ) ;
#162851 = CARTESIAN_POINT ( 'NONE',  ( 3.099882009726143917, -2.289598904869084350, 0.1129434519280565069 ) ) ;
#162852 = CARTESIAN_POINT ( 'NONE',  ( 1.207329354700342305, -0.4456725867950651621, 1.770335049871730071 ) ) ;
#162853 = CARTESIAN_POINT ( 'NONE',  ( 1.951281838316549777, -1.706683157587106425, 0.8630329916254894096 ) ) ;
#162854 = ORIENTED_EDGE ( 'NONE', *, *, #155093, .F. ) ;
#162855 = CARTESIAN_POINT ( 'NONE',  ( 6.087247782411444597, 10.04561347954795281, -0.7216878364870267237 ) ) ;
#162856 = EDGE_CURVE ( 'NONE', #41100, #130351, #86755, .T. ) ;
#162857 = CARTESIAN_POINT ( 'NONE',  ( 1.424089148264463089, -1.997494042244374768, 0.2507359931839692191 ) ) ;
#162858 = CARTESIAN_POINT ( 'NONE',  ( 1.428482823135175606, -1.248714028858177283, 1.512975372890807524 ) ) ;
#162859 = CARTESIAN_POINT ( 'NONE',  ( -10.32183501870554387, 10.93656236477829502, 0.7998128361456462443 ) ) ;
#162860 = CARTESIAN_POINT ( 'NONE',  ( -5.703176172842872482, 9.805455968292021041, 0.000000000000000000 ) ) ;
#162861 = CARTESIAN_POINT ( 'NONE',  ( -7.725699985795428049, -5.832912386296868590, -7.725699985795385416 ) ) ;
#162863 = CARTESIAN_POINT ( 'NONE',  ( 3.379546851323252721, 1.122120933264129539, 1.368648242959294992 ) ) ;
#162862 = CARTESIAN_POINT ( 'NONE',  ( 4.242189115703227209, 0.5575990197337198362, 2.014825664747122769 ) ) ;
#162864 = CARTESIAN_POINT ( 'NONE',  ( -1.225000000000046052, 0.04166666734950023182, -0.7072540797573217963 ) ) ;
#162865 = CARTESIAN_POINT ( 'NONE',  ( 6.509759575370489770, -1.074588918421373940, -2.024802758542126213 ) ) ;
#162866 = CARTESIAN_POINT ( 'NONE',  ( 4.435344831996881787, 0.7407458870649418214, -1.574957418989342939 ) ) ;
#162867 = CARTESIAN_POINT ( 'NONE',  ( 7.879259827836241570, 12.34422023245099176, 1.040834085586084257E-14 ) ) ;
#162868 = CARTESIAN_POINT ( 'NONE',  ( 7.221001870987139526, -6.414086731524418994, -6.604641253243922705 ) ) ;
#162869 = CARTESIAN_POINT ( 'NONE',  ( 4.850818353276647343, -0.8162368348260983231, 1.529697846671844941 ) ) ;
#162870 = CARTESIAN_POINT ( 'NONE',  ( 5.090355501040885855, 1.120491699331874536, -1.859593947532897973 ) ) ;
#162871 = CARTESIAN_POINT ( 'NONE',  ( 2.822068529938852155, 6.444163718237301275, -0.7998128361456291469 ) ) ;
#162872 = CARTESIAN_POINT ( 'NONE',  ( 5.348842313791752900, -1.825074749614737701, -0.8578464102408298597 ) ) ;
#162873 = CARTESIAN_POINT ( 'NONE',  ( 6.500000003069670740, 7.552736074387352678E-08, -2.052068128417939175 ) ) ;
#162874 = CARTESIAN_POINT ( 'NONE',  ( -1.499999999999997780, 4.931250000682820378, 1.214306433183764966E-14 ) ) ;
#162875 = CARTESIAN_POINT ( 'NONE',  ( 3.293886989636186868, -0.7820812614263569218, 1.760672275598859748 ) ) ;
#162876 = CARTESIAN_POINT ( 'NONE',  ( -1.402160292154681736E-14, 9.593750000682801371, 1.732050807568881190 ) ) ;
#162877 = CARTESIAN_POINT ( 'NONE',  ( 0.2061412868327249515, 1.650399489264813502, 1.486927644236696766 ) ) ;
#162878 = VERTEX_POINT ( 'NONE', #63214 ) ;
#162880 = TOROIDAL_SURFACE ( 'NONE', #69453, 6.330000000000000959, 0.08000000000000000167 ) ;
#162879 = CARTESIAN_POINT ( 'NONE',  ( 6.983263157960365675, 7.629137130509066722, 2.646189081643287810 ) ) ;
#162881 = CARTESIAN_POINT ( 'NONE',  ( -1.201851678989727383E-14, 3.587500000000020339, -1.732050807568863648 ) ) ;
#162882 = CARTESIAN_POINT ( 'NONE',  ( 4.774442650306744085, 8.721933525333202653, -0.7998128361456281477 ) ) ;
#162883 = CARTESIAN_POINT ( 'NONE',  ( 1.489269531296941507, -2.110695925841240772, -0.6924467157797905559 ) ) ;
#162884 = CARTESIAN_POINT ( 'NONE',  ( 7.782016984564060103, 9.141736572488651902, 1.082531754730558626 ) ) ;
#162885 = CARTESIAN_POINT ( 'NONE',  ( 0.4396008313321266292, 7.377972292137268795, 2.042906170116781439 ) ) ;
#162886 = CARTESIAN_POINT ( 'NONE',  ( 6.861835142292135536, 9.098836647464588978, 1.443375672974065660 ) ) ;
#162887 = CARTESIAN_POINT ( 'NONE',  ( -3.851925040058337579, 6.547644075826416277, -1.082531754730546636 ) ) ;
#162889 = CARTESIAN_POINT ( 'NONE',  ( 5.810998785189021909, -1.628375694745004321, 1.266036720739783128 ) ) ;
#162888 = LINE ( 'NONE', #86683, #199269 ) ;
#162890 = CARTESIAN_POINT ( 'NONE',  ( -3.253066792275140173, 5.882662793374543675, 1.199719254218462483 ) ) ;
#162891 = CARTESIAN_POINT ( 'NONE',  ( 1.499999999999989120, 5.577083334016153415, -0.8660254037844323793 ) ) ;
#162892 = CARTESIAN_POINT ( 'NONE',  ( 1.364683531249986537, 0.1552083336747499542, -0.7879004041258309554 ) ) ;
#162893 = CARTESIAN_POINT ( 'NONE',  ( 6.573518820989787237, 1.789947451694915204, -0.5432430119688207437 ) ) ;
#162894 = CARTESIAN_POINT ( 'NONE',  ( 5.414640894582111841, -1.106827951885097638, -1.334981224695269475 ) ) ;
#162895 = CARTESIAN_POINT ( 'NONE',  ( 4.300191697305631777, 1.341742100086223743, -1.108517911846224502 ) ) ;
#162896 = CARTESIAN_POINT ( 'NONE',  ( 4.844340958784499662, 4.546152628203684820, 0.7998128361456341429 ) ) ;
#162897 = ADVANCED_FACE ( 'NONE', ( #113106 ), #134830, .T. ) ;
#162898 = CARTESIAN_POINT ( 'NONE',  ( 3.386539700769741312, -0.4487184517108309123, -2.247870937536749381 ) ) ;
#162899 = CARTESIAN_POINT ( 'NONE',  ( 1.364683531249992088, 5.696875000341418804, 1.214306433183764966E-14 ) ) ;
#162900 = CARTESIAN_POINT ( 'NONE',  ( 1.394213304513430174, 1.506067903837378097, -1.058747118707924262 ) ) ;
#162901 = CARTESIAN_POINT ( 'NONE',  ( -0.3645075752536136582, 3.999999999999973799, 0.9782388703846811584 ) ) ;
#162902 = CARTESIAN_POINT ( 'NONE',  ( -11.30177626766236365, 6.974151656887320527, -4.150880038395990290 ) ) ;
#162903 = CARTESIAN_POINT ( 'NONE',  ( 1.834698128333624112, 0.1755570873784827179, 1.817110820650599923 ) ) ;
#162904 = CARTESIAN_POINT ( 'NONE',  ( 2.725232599228684993, 2.001511357256777313, 0.2440295182731533341 ) ) ;
#162905 = CARTESIAN_POINT ( 'NONE',  ( 1.201424296212102893, -0.5295503721958020327, 2.126384922054704862 ) ) ;
#162906 = CARTESIAN_POINT ( 'NONE',  ( 9.673880494682652653, 13.47554395514287684, -8.174421919205036247 ) ) ;
#162907 = CARTESIAN_POINT ( 'NONE',  ( 4.454198790814194453, 2.105553956100237656, -0.04914431425445846269 ) ) ;
#162908 = CARTESIAN_POINT ( 'NONE',  ( -6.418895661066105873, 9.576129806964074120, -1.199719254218440723 ) ) ;
#162909 = CARTESIAN_POINT ( 'NONE',  ( 9.143844951682952527, 13.34121998047297808, 9.071981315083665010 ) ) ;
#162910 = CARTESIAN_POINT ( 'NONE',  ( 1.434126425884488354, 1.231690216755284562, 1.664001042209894088 ) ) ;
#162911 = CARTESIAN_POINT ( 'NONE',  ( 5.691725559638619814, 5.534767995866836543, 1.040834085586084257E-14 ) ) ;
#162912 = CARTESIAN_POINT ( 'NONE',  ( 1.360316468749997565, 2.744791667008062763, 0.7853790794158921340 ) ) ;
#162913 = CARTESIAN_POINT ( 'NONE',  ( 4.072980787186268437, -1.570383936966279981, 1.425070900414181052 ) ) ;
#162914 = ITEM_DEFINED_TRANSFORMATION ( 'NONE', 'NONE', #207992,  #200407 ) ;
#162916 = ADVANCED_FACE ( 'NONE', ( #143443 ), #110965, .T. ) ;
#162915 = CARTESIAN_POINT ( 'NONE',  ( -0.02299388927988389730, 0.001624902753813092359, -1.910968047046639251 ) ) ;
#162917 = ORIENTED_EDGE ( 'NONE', *, *, #119057, .F. ) ;
#162918 = CARTESIAN_POINT ( 'NONE',  ( -4.522526758610270647, 7.433975764090723359, -1.199719254218453823 ) ) ;
#162919 = CARTESIAN_POINT ( 'NONE',  ( 9.748476143425788720, 11.33197590787365172, -1.199719254218440723 ) ) ;
#162920 = CARTESIAN_POINT ( 'NONE',  ( 5.465345319640213972, 8.429967735338637524, -1.082531754730548412 ) ) ;
#162921 = CARTESIAN_POINT ( 'NONE',  ( 3.475000000000000533, -3.310416665710749218, 2.006292185433948827 ) ) ;
#162922 = CARTESIAN_POINT ( 'NONE',  ( -3.716906668440817185, 7.488141546489591072, 0.7998128361456341429 ) ) ;
#162923 = CARTESIAN_POINT ( 'NONE',  ( 3.199477664157297063, 1.824241505505564964, -0.8673461216518009165 ) ) ;
#162924 = CARTESIAN_POINT ( 'NONE',  ( 0.7277292075377658209, -1.999665741513008799, 0.6608504825312794262 ) ) ;
#162925 = CARTESIAN_POINT ( 'NONE',  ( -6.466312919074983512, 6.508729591867735031, -0.7998128361456362523 ) ) ;
#162926 = CARTESIAN_POINT ( 'NONE',  ( 9.511208455186636712, 11.05516360492796935, 1.199719254218453823 ) ) ;
#162927 = CARTESIAN_POINT ( 'NONE',  ( 4.979284885303652430, -0.09383206328643842187, 1.858730327737258436 ) ) ;
#162928 = CARTESIAN_POINT ( 'NONE',  ( 7.401861798056875053, 10.72292363345333399, -1.199719254218441611 ) ) ;
#162929 = FACE_OUTER_BOUND ( 'NONE', #175842, .T. ) ;
#162930 = CARTESIAN_POINT ( 'NONE',  ( -4.878955176071358757, 6.785476686873604280, -1.599625672291271394 ) ) ;
#162931 = CARTESIAN_POINT ( 'NONE',  ( -9.246297574839990929, 11.81043314211192019, 1.443375672974076540 ) ) ;
#162933 = CARTESIAN_POINT ( 'NONE',  ( 1.855835942623608181, -0.6640040153468586004, 1.846199708051485811 ) ) ;
#162932 = CARTESIAN_POINT ( 'NONE',  ( -6.856673000209188906, 9.022537805042615489, 1.599625672291283607 ) ) ;
#162934 = CARTESIAN_POINT ( 'NONE',  ( 0.5675189469334164238, 0.2105291993744831114, -2.151437729447757796 ) ) ;
#162936 = CARTESIAN_POINT ( 'NONE',  ( -5.391143034427437364, 6.494952464278877180, 1.342996321926675396 ) ) ;
#162935 = CARTESIAN_POINT ( 'NONE',  ( -5.367048706163331850, 7.354919138647580290, -1.599625672291271394 ) ) ;
#162937 = CARTESIAN_POINT ( 'NONE',  ( -1.402160292154681736E-14, 0.9468750003414176941, -1.575800808251659024 ) ) ;
#162938 = CARTESIAN_POINT ( 'NONE',  ( 3.180671111220879865, -0.8518272437034493105, -1.510038686645834183 ) ) ;
#162939 = CARTESIAN_POINT ( 'NONE',  ( 2.325747778006927557, 1.687818050649522617, 0.4237310505307323449 ) ) ;
#162941 = CARTESIAN_POINT ( 'NONE',  ( 7.944714827928056167, 8.371181508778631652, 0.7216878364870458196 ) ) ;
#162940 = CARTESIAN_POINT ( 'NONE',  ( 6.164718480307596060, -1.636601974411681981, 1.627217620858178337 ) ) ;
#162942 = CARTESIAN_POINT ( 'NONE',  ( -10.96041802301306944, 4.843384909922287207, -4.379099270644332798 ) ) ;
#162943 = CARTESIAN_POINT ( 'NONE',  ( 2.548181945144313953, 2.060261615984103400, 0.05380422017278729124 ) ) ;
#162944 = CARTESIAN_POINT ( 'NONE',  ( 6.342516933094585418, 6.294024598232139667, 1.040834085586084257E-14 ) ) ;
#162945 = CARTESIAN_POINT ( 'NONE',  ( 1.704453651327157537, -1.458331393932917885, -1.392334588655015803 ) ) ;
#162946 = CARTESIAN_POINT ( 'NONE',  ( 6.925078400183531713, -0.004750840071900476122, 2.044148492825672569 ) ) ;
#162947 = CARTESIAN_POINT ( 'NONE',  ( -3.797165540279144214, 6.587721009371067638, 1.199719254218452935 ) ) ;
#162949 = EDGE_CURVE ( 'NONE', #57555, #87955, #52128, .T. ) ;
#162948 = CIRCLE ( 'NONE', #62568, 0.08000000000000020983 ) ;
#162950 = CARTESIAN_POINT ( 'NONE',  ( 0.9890677962714401472, 1.739647146885098694, -0.9275093368027197416 ) ) ;
#162952 = CARTESIAN_POINT ( 'NONE',  ( -6.509323148336870091, 7.727203440215372865, 1.082531754730549078 ) ) ;
#162951 = CARTESIAN_POINT ( 'NONE',  ( 4.377155534175989793, -1.710687068321177007, -0.8549628122409487219 ) ) ;
#162953 = CARTESIAN_POINT ( 'NONE',  ( -6.414416072596845986, 8.576847732820027659, -1.443375672974066548 ) ) ;
#162954 = CARTESIAN_POINT ( 'NONE',  ( 7.095713291905693332, 9.371694488680407886, 1.599625672291268286 ) ) ;
#162955 = CARTESIAN_POINT ( 'NONE',  ( -6.526270840131767059, 8.707344961610770540, -1.599625672291271394 ) ) ;
#162956 = CARTESIAN_POINT ( 'NONE',  ( 1.119792439799172978, -0.4886160933238526405, 1.959555815251372568 ) ) ;
#162957 = DIRECTION ( 'NONE',  ( 0.000000000000000000, 1.000000000000000000, 0.000000000000000000 ) ) ;
#162958 = CARTESIAN_POINT ( 'NONE',  ( 4.208297055918253093, -2.301676378859803584, 0.1658454734064350733 ) ) ;
#162959 = CARTESIAN_POINT ( 'NONE',  ( 5.863715402168388380, -0.4781514528688200483, 1.902565108626976809 ) ) ;
#162960 = CARTESIAN_POINT ( 'NONE',  ( 2.149198318390078910, 1.709348667602617722, -0.9624241554767107854 ) ) ;
#162961 = CARTESIAN_POINT ( 'NONE',  ( -4.956281507356261606, 4.676749934870729319, -0.1948928627674308134 ) ) ;
#162962 = CARTESIAN_POINT ( 'NONE',  ( -0.01695367945527340853, -2.016028864686558730, -0.04667425414178057869 ) ) ;
#162963 = ORIENTED_EDGE ( 'NONE', *, *, #105361, .T. ) ;
#162964 = CARTESIAN_POINT ( 'NONE',  ( 1.059931528796464129, 1.266109226500349960, 1.696929307225014449 ) ) ;
#162966 = CARTESIAN_POINT ( 'NONE',  ( -7.694415870955439551, 8.935572256658169010, 1.199719254218462483 ) ) ;
#162965 = CARTESIAN_POINT ( 'NONE',  ( -5.935772324684618795, 5.819489221753827657, 0.000000000000000000 ) ) ;
#162967 = CARTESIAN_POINT ( 'NONE',  ( 1.130510352786683326, -1.665311210022573540, 0.7854980884962546872 ) ) ;
#162968 = ORIENTED_EDGE ( 'NONE', *, *, #46280, .T. ) ;
#162969 = CARTESIAN_POINT ( 'NONE',  ( 4.416952212917071741, -1.612892420192946652, 1.453532087098859504 ) ) ;
#162970 = CARTESIAN_POINT ( 'NONE',  ( 11.80845508765946050, 7.960079180001382149, 2.175004853915265546 ) ) ;
#162971 = CARTESIAN_POINT ( 'NONE',  ( 1.916421503514931679, -2.120014230100770725, 0.05699577502370903326 ) ) ;
#162972 = CARTESIAN_POINT ( 'NONE',  ( -1.201851678989727383E-14, 2.493750000682819046, 1.732050807568877637 ) ) ;
#162973 = CARTESIAN_POINT ( 'NONE',  ( 7.242026607993941489, 11.60078147596829901, 0.7998128361456462443 ) ) ;
#162974 = CARTESIAN_POINT ( 'NONE',  ( -0.3282377607281317111, 0.4486645496846296544, -1.225000000000047828 ) ) ;
#162975 = CARTESIAN_POINT ( 'NONE',  ( 2.882161881593125585, -1.062215874558822826, 1.765801728998709352 ) ) ;
#162976 = VECTOR ( 'NONE', #116468, 1000.000000000000000 ) ;
#162978 = CARTESIAN_POINT ( 'NONE',  ( 0.3976880421775743635, -0.6195963491163231085, -1.733980255833282191 ) ) ;
#162977 = CARTESIAN_POINT ( 'NONE',  ( -8.585337585951595685, 11.03931315507545108, -1.599625672291263179 ) ) ;
#162979 = CARTESIAN_POINT ( 'NONE',  ( 1.364683531249990311, 3.884375000341417028, 1.214306433183764966E-14 ) ) ;
#162980 = CARTESIAN_POINT ( 'NONE',  ( 1.342212891865499298E-15, -1.000000000000000888, 10.92000000000000171 ) ) ;
#162981 = CARTESIAN_POINT ( 'NONE',  ( 1.466385641617009128, 4.235413722433956529, -0.3259940066991331431 ) ) ;
#162982 = CARTESIAN_POINT ( 'NONE',  ( 1.318052817733056825, -2.207296558944459974, 0.4957021660386366491 ) ) ;
#162983 = CARTESIAN_POINT ( 'NONE',  ( -10.15469386695561482, 10.94949038764413096, 1.040834085586084257E-14 ) ) ;
#162984 = CARTESIAN_POINT ( 'NONE',  ( 2.917991513842286277, -1.809334129394428947, 0.09316547460730231767 ) ) ;
#162985 = CARTESIAN_POINT ( 'NONE',  ( 1.727608309356289729, 0.7294743340424666433, -1.771600730223451547 ) ) ;
#162986 = CARTESIAN_POINT ( 'NONE',  ( 3.666520218671379450, -0.8364210039109070127, -1.894060025281426807 ) ) ;
#162987 = CARTESIAN_POINT ( 'NONE',  ( -1.402160292154681736E-14, 1.009375000341417916, -1.575800808251659024 ) ) ;
#162988 = AXIS2_PLACEMENT_3D ( 'NONE', #34201, #99228, #129678 ) ;
#162989 = CARTESIAN_POINT ( 'NONE',  ( 1.270321628189803542, -1.252206795699914332, 1.522702518494284396 ) ) ;
#162990 = CARTESIAN_POINT ( 'NONE',  ( 0.3406813593837527687, 0.3259726575214479394, 1.898462188649749249 ) ) ;
#162991 = CARTESIAN_POINT ( 'NONE',  ( 3.238977024203249400, -1.650389259550872456, 0.8806316622528218563 ) ) ;
#162993 = CARTESIAN_POINT ( 'NONE',  ( 4.597876849858236525, 8.486543085689454813, -0.1053875944492469602 ) ) ;
#162992 = CARTESIAN_POINT ( 'NONE',  ( 1.137850649969934347, -2.084210194689451789, 0.9910022104400189047 ) ) ;
#162994 = CARTESIAN_POINT ( 'NONE',  ( 2.259996020855909116, -1.860750554326926487, 0.04185779618384557338 ) ) ;
#162995 = CARTESIAN_POINT ( 'NONE',  ( -1.364683531250012516, 3.030208333674755394, 0.7879004041258379498 ) ) ;
#162996 = CARTESIAN_POINT ( 'NONE',  ( 5.740703853076708718, -2.011634581743710903, -0.4553567745326501104 ) ) ;
#162997 = CARTESIAN_POINT ( 'NONE',  ( -4.252453736180621391, 8.112946458852704268, -0.7998128361456281477 ) ) ;
#162998 = CARTESIAN_POINT ( 'NONE',  ( -1.300073763039018004, 3.592844841581338322, -0.4337670944211725055 ) ) ;
#162999 = CARTESIAN_POINT ( 'NONE',  ( 6.458053290436937210, 2.100604981398071835, -0.1509308302805877633 ) ) ;
#163000 = CARTESIAN_POINT ( 'NONE',  ( -1.201851678989727383E-14, 3.259375000341420581, -1.575800808251660134 ) ) ;
#163001 = CARTESIAN_POINT ( 'NONE',  ( 5.606754022945427351, 1.640879930231559758, -1.407263238018638507 ) ) ;
#163002 = CARTESIAN_POINT ( 'NONE',  ( 1.048114208743459619, -1.451426956872736262, 1.132798186660122441 ) ) ;
#163003 = CARTESIAN_POINT ( 'NONE',  ( 5.936196224836090884, -1.123750473735840361, -1.677956830082157236 ) ) ;
#163004 = CARTESIAN_POINT ( 'NONE',  ( -4.772106882330234612, 6.590544000850480089, -1.443375672974053892 ) ) ;
#163005 = CARTESIAN_POINT ( 'NONE',  ( -4.853455804012230423, 6.685451076146141425, 1.443375672974064550 ) ) ;
#163008 = CARTESIAN_POINT ( 'NONE',  ( 5.070386261830877928, 5.978167395966564435, -1.082531754730548412 ) ) ;
#163007 = CARTESIAN_POINT ( 'NONE',  ( 3.285556943750000514, -0.6635416661887083567, 1.896917185911906500 ) ) ;
#163006 = CARTESIAN_POINT ( 'NONE',  ( 5.840530312436913007, 10.03597880781023299, 0.000000000000000000 ) ) ;
#163009 = CARTESIAN_POINT ( 'NONE',  ( -4.793689830883590020, 7.750332681742931662, 1.199719254218452935 ) ) ;
#163010 = CARTESIAN_POINT ( 'NONE',  ( 4.100796195634116792, 1.845626398921360822, 0.8128187495666516771 ) ) ;
#163011 = CARTESIAN_POINT ( 'NONE',  ( -8.877891658850122880, 9.251961778280284321, 0.7998128361456462443 ) ) ;
#163013 = CARTESIAN_POINT ( 'NONE',  ( -6.075462232255183892, 10.10214001435745246, 0.000000000000000000 ) ) ;
#163012 = CARTESIAN_POINT ( 'NONE',  ( -3.684065054611367351, 5.321161868511784299, -1.599625672291256295 ) ) ;
#163014 = CARTESIAN_POINT ( 'NONE',  ( 1.364683531249990311, 4.884375000341417916, 1.214306433183764966E-14 ) ) ;
#163016 = CARTESIAN_POINT ( 'NONE',  ( 1.364683531249996529, 9.713541667008064096, 0.7879004041258403923 ) ) ;
#163015 = CARTESIAN_POINT ( 'NONE',  ( 6.086834708314957432, -0.3123483334277510348, -2.138898144987111838 ) ) ;
#163017 = CARTESIAN_POINT ( 'NONE',  ( 10.28586320583508495, 2.972657967447012162, -5.491880110201817544 ) ) ;
#163018 = CARTESIAN_POINT ( 'NONE',  ( -11.50347174040005527, 6.904995786113715006, 3.422550450347928486 ) ) ;
#163020 = CARTESIAN_POINT ( 'NONE',  ( 5.677361293727043901, 1.528752376640944100, 1.314985542479940817 ) ) ;
#163019 = CARTESIAN_POINT ( 'NONE',  ( -7.659993601596726265, 8.039006744725394782, -0.7216878364870267237 ) ) ;
#163021 = CARTESIAN_POINT ( 'NONE',  ( -1.402160292154681736E-14, -0.9906249996585834161, -1.575800808251665908 ) ) ;
#163022 = CARTESIAN_POINT ( 'NONE',  ( 2.156509779666794024, -1.334175267976490664, 1.093223185313265899 ) ) ;
#163023 = CARTESIAN_POINT ( 'NONE',  ( 5.734172623936983904, 5.654565914206774124, 0.7998128361456352531 ) ) ;
#163025 = CARTESIAN_POINT ( 'NONE',  ( 5.494797395288433250, 9.632623737803665875, 0.000000000000000000 ) ) ;
#163024 = CARTESIAN_POINT ( 'NONE',  ( 6.887178846062110615, 9.058127958537705027, -1.443375672974057666 ) ) ;
#163026 = CARTESIAN_POINT ( 'NONE',  ( 0.4717386086568179926, 2.948512804476515647, -1.943622686712360714 ) ) ;
#163027 = CARTESIAN_POINT ( 'NONE',  ( 0.3679306741783492929, -1.162814898748459225, 1.334192561405376676 ) ) ;
#163029 = CARTESIAN_POINT ( 'NONE',  ( 0.3287710483851979393, 1.386612999538240576, -1.459627859818838802 ) ) ;
#163028 = PRODUCT_DEFINITION_FORMATION_WITH_SPECIFIED_SOURCE ( 'ANY', '', #107661, .NOT_KNOWN. ) ;
#163030 = CARTESIAN_POINT ( 'NONE',  ( -4.848970937371709589, 4.819285127202144636, 0.1070505994550537271 ) ) ;
#163031 = CARTESIAN_POINT ( 'NONE',  ( 3.505080564089088746, 1.740947047783932611, -1.355986173033681075 ) ) ;
#163032 = VECTOR ( 'NONE', #135260, 1000.000000000000000 ) ;
#163033 = CARTESIAN_POINT ( 'NONE',  ( 5.014598762909163732, 0.8246402433861481640, 2.008555861535677778 ) ) ;
#163034 = EDGE_LOOP ( 'NONE', ( #3858, #163064 ) ) ;
#163035 = CARTESIAN_POINT ( 'NONE',  ( 3.573456005653643519, 6.326726552307992080, -1.199719254218453823 ) ) ;
#163037 = CARTESIAN_POINT ( 'NONE',  ( 9.286972035236624734, 11.85788667924133399, -1.443375672974058777 ) ) ;
#163036 = CIRCLE ( 'NONE', #48931, 0.07999999999999993228 ) ;
#163039 = CARTESIAN_POINT ( 'NONE',  ( 1.476185646619165404, -2.006963189339417308, -0.1948195631672477446 ) ) ;
#163038 = CARTESIAN_POINT ( 'NONE',  ( 2.649219347560148208, 0.2619616101627724736, 2.104190563435456518 ) ) ;
#163041 = ORIENTED_EDGE ( 'NONE', *, *, #126913, .T. ) ;
#163040 = CARTESIAN_POINT ( 'NONE',  ( 2.812559491778331200, -0.5300286150072616165, -1.732275345909091380 ) ) ;
#163042 = CARTESIAN_POINT ( 'NONE',  ( 6.737475991348287785, 6.825086509519945999, -0.7998128361456481317 ) ) ;
#163043 = ORIENTED_EDGE ( 'NONE', *, *, #6657, .T. ) ;
#163044 = EDGE_CURVE ( 'NONE', #93441, #60282, #149056, .T. ) ;
#163045 = CARTESIAN_POINT ( 'NONE',  ( 5.961834861707224320, 7.978559976790334574, -1.599625672291262513 ) ) ;
#163047 = CARTESIAN_POINT ( 'NONE',  ( 1.674859764755828095, 1.664904793830531027, -0.9475745862929999541 ) ) ;
#163046 = CARTESIAN_POINT ( 'NONE',  ( -5.278201874421821316, 5.052323696447222900, 0.7998128361456341429 ) ) ;
#163048 = CARTESIAN_POINT ( 'NONE',  ( -1.500000000000051514, 3.420833333333354265, 0.8660254037844170583 ) ) ;
#163049 = CARTESIAN_POINT ( 'NONE',  ( -4.877338746226314470, 4.951936442570412211, -0.6255423638818237153 ) ) ;
#163050 =( BOUNDED_SURFACE ( )  B_SPLINE_SURFACE ( 3, 3, ( 
 ( #113748, #97445, #11897, #209016, #114802, #77971, #127896, #110547, #95325, #30301, #10823, #176549, #180801, #163501, #32427, #194921, #162438, #80100, #28159, #212220, #63855, #130011, #126815, #193847, #46558, #94255, #197049, #210089, #160294, #47636, #144094, #196002, #178688, #161374, #76897, #12957, #31369, #112678, #61728, #15085, #143021, #213286, #179752, #81175, #45497, #111613, #147254, #64912, #131061, #177625, #48687, #29233, #79035, #145150, #211156, #62780, #100617, #122027, #182930, #116931, #2018, #65949, #187994, #123113, #199158, #34546, #73166, #133157, #18283, #104636, #68087, #203164, #22270, #164557, #166692, #6027, #89459, #88379, #84369, #955, #23349, #139272, #54809, #150457, #83287, #137136, #120957, #205302, #16142, #186928, #49737, #155512, #198107, #82227, #132098, #38560, #55871, #50803, #17211, #148318, #72096, #56941, #149372, #170683, #154447, #67021, #138206, #204218, #214317, #99558, #39619, #189071, #105723, #171753, #98493, #7093, #165623, #115864, #181849, #33486, #76383, #190129, #142492, #143569, #158712, #177095, #78516, #111088, #157655, #93732, #193334, #40706, #108959, #210648, #208499, #174979, #60134, #126291, #191185, #25497, #62274, #107898, #173924, #206376, #10309, #141441, #160845, #125227, #124167, #209561, #128435, #91605, #44980, #192250, #159772, #28710, #41784, #26561, #9253, #43912, #61206, #127364, #94796, #75324, #90525, #106810, #207447, #59066, #58003, #42852, #110026, #172840, #74265, #24411, #12437, #156587, #176040, #27632, #11371, #140358, #77451, #144633, #8181, #92668, #162986, #164055, #161924, #17752, #30859, #195480, #82781, #211704, #165104, #113230, #131591, #99049, #15634, #16696, #13514, #145705, #181346, #129499, #63340, #47113, #179235, #114298, #148854, #116411, #213822, #64408, #81721, #96936, #180296, #427, #50292, #79586, #65440, #198644, #182401, #112165, #14567, #80663, #66499, #34031, #196544, #130552, #146754, #32973, #178168, #83842, #149931, #100104, #166164, #212772, #97997, #197592, #132638, #1500, #67566, #48187, #194402, #95868, #31919, #46044, #29784, #147803, #49236, #115355, #117485, #23092, #89207, #119619, #152061, #105467, #186675, #20952, #88124, #69709, #185603, #183476, #39370, #68641, #22014, #121773, #38302, #35083, #120700, #102233, #170427, #155261, #3631, #135813, #104380, #103306, #154194, #101155, #133709, #85986, #171500, #5762, #71842, #201836, #202909, #55618, #137951, #53481, #203971, #168304, #19901, #6842, #37234, #2569, #187742, #199715, #52423, #51362, #87049, #167241, #18829, #134764, #169367, #200772, #153122, #4693, #70768, #84913, #136882, #151001, #54553, #118549, #184531, #36154, #127111, #191997, #76136, #188820, #24164, #109778, #208251, #59885, #90267, #92420, #143314, #142239, #74006, #139025, #44728, #75073, #93480, #157406, #91345, #190935, #40454, #159519, #94548, #173670, #8998, #110836, #107638, #207196, #126034, #42599, #174734, #43662, #205049, #141186, #175787, #60954, #27379, #58821, #189884, #209307, #176841, #26306, #124974, #57756, #108705, #158459, #28454, #56692, #10060, #156335, #193076, #172585, #122859, #106556, #11118, #77194, #25245, #206126, #7921, #160586, #72920, #123916, #140099, #41526, #211451, #112975, #129255, #128185, #13264, #14309, #99855, #63085, #195225, #182146, #46862 ),
 ( #82520, #178987, #65191, #164849, #12193, #80404, #33776, #180043, #146501, #31665, #47936, #162737, #30601, #78264, #79337, #145454, #177915, #130302, #62030, #144388, #96690, #212518, #29529, #64160, #97742, #210388, #45794, #194146, #16441, #111915, #196290, #163801, #81471, #95620, #213570, #15377, #131345, #161671, #114050, #147548, #197340, #50035, #48982, #115100, #181097, #32713, #98795, #148607, #176, #66244, #132392, #198394, #116160, #117226, #152864, #100904, #183224, #34830, #18584, #85726, #54303, #87866, #185349, #35906, #201584, #166993, #151812, #186415, #21758, #51101, #36971, #170170, #153938, #83590, #199459, #84662, #202654, #5507, #168050, #101981, #150751, #4442, #149672, #55364, #121517, #71587, #137696, #2312, #69455, #103054, #120441, #203716, #187488, #19652, #104124, #67311, #3385, #70512, #39118, #165917, #135560, #53231, #1253, #17502, #133454, #119361, #184280, #68389, #136627, #169107, #38052, #20704, #86798, #134518, #200522, #52168, #118294, #93224, #9803, #88948, #92161, #73743, #141985, #209051, #123661, #41272, #158214, #74822, #207999, #6587, #105201, #57502, #143056, #75878, #59625, #189624, #174473, #27118, #125782, #107381, #191744, #139839, #43399, #109521, #175528, #172322, #171238, #138764, #126851, #159256, #192808, #140922, #42338, #26048, #204781, #10857, #190679, #76930, #155002, #205868, #206936, #72666, #60687, #156073, #106300, #22834, #122594, #56435, #23912, #108453, #188557, #58565, #40188, #90016, #7659, #173404, #24985, #91088, #157148, #8741, #124719, #147288, #180834, #63890, #128979, #80136, #210124, #178724, #64943, #114836, #144131, #130045, #48721, #32459, #176585, #78007, #177660, #81209, #98530, #46594, #194958, #61765, #31405, #28197, #148353, #214352, #164590, #16176, #111648, #162475, #196038, #213320, #82260, #65982, #112712, #197084, #160331, #96424, #97479, #132133, #44467, #30339, #14048, #94291, #110583, #11935, #146240, #62819, #127933, #163535, #212256, #131095, #47672, #113783, #193886, #45534, #29268, #95360, #161410, #15121, #12994, #79069, #145187, #211193, #179785, #2051, #134259, #36708, #167792, #86538, #99592, #198140, #150492, #21502, #102794, #168851, #68123, #52964, #120181, #4189, #200265, #152603, #18321, #70259, #136373, #202392, #50841, #33520, #153681, #116967, #166730, #149409, #51916, #69191, #20454, #118039, #119102, #186157, #54044, #184026, #37791, #84404, #103865, #169915, #87610, #182965, #165658, #5250, #34580, #35642, #991, #101721, #135312, #49772, #17245, #71326, #115898, #181884, #19387, #201326, #185084, #83321, #67055, #133191, #199192, #100652, #85466, #151552, #3122, #91905, #204527, #154748, #74565, #22582, #8478, #138504, #41011, #140664, #205608, #206679, #104943, #88688, #24725, #6331, #170983, #72404, #56176, #155816, #58310, #108197, #189369, #106043, #57245, #122338, #7400, #124466, #190425, #188295, #107121, #42082, #174221, #203457, #38860, #39935, #25796, #157962, #23659, #172066, #89770, #90828, #55112, #9554, #75629, #141739, #137441, #73481, #123405, #173144, #121258, #187230, #139581, #156890, #54730, #17937, #168479, #103486, #104563, #138132, #102411, #36333, #100280, #5949, #72019, #20077, #134941, #88308, #169547, #3808, #70951, #52596, #86166, #166346, #22195, #51543, #4872, #170608, #21128 ),
 ( #152236, #101341, #118724, #167422, #2749, #19014, #84023, #117667, #184709, #204141, #85094, #151179, #116590, #68819, #183660, #203086, #154372, #182584, #69881, #35264, #135992, #137061, #202006, #38486, #34207, #186855, #200947, #87232, #120881, #150113, #53666, #1686, #119797, #185777, #37410, #153296, #67740, #133890, #199896, #111719, #93295, #142052, #77003, #157215, #125855, #12003, #61834, #91159, #10927, #210198, #128000, #123731, #25057, #124789, #28267, #193954, #208067, #59692, #8811, #192880, #189693, #95432, #161485, #45602, #177727, #58636, #109594, #143129, #160401, #29339, #13063, #191812, #144202, #107453, #43476, #44535, #79142, #205941, #175599, #27189, #41344, #57573, #173480, #159331, #9874, #74889, #110653, #209125, #78077, #60762, #126922, #140997, #207005, #190749, #94359, #42413, #176654, #108518, #174547, #26122, #92233, #158284, #75950, #81281, #198205, #114905, #33584, #46665, #145259, #97551, #183031, #49840, #115967, #15190, #76424, #67124, #165726, #147357, #99657, #179853, #17314, #83392, #149476, #212323, #195031, #100717, #63961, #113858, #96497, #213384, #16244, #1059, #112786, #197151, #132198, #133257, #166794, #131160, #65008, #129057, #34647, #18388, #48788, #163608, #117036, #181956, #32525, #199263, #180902, #98601, #178797, #50908, #80208, #211264, #62888, #30413, #162547, #14117, #31476, #146309, #130116, #164662, #82330, #196106, #148422, #47742, #66054, #84465, #36771, #122397, #203518, #137501, #168913, #153740, #6392, #105003, #20516, #187292, #119161, #171042, #38919, #22641, #151617, #134324, #39995, #3184, #53028, #35709, #86601, #169974, #150557, #118105, #106103, #88749, #172125, #54107, #21562, #5308, #184090, #71389, #87668, #55172, #200330, #185147, #120242, #51980, #188355, #135372, #85528, #154806, #101786, #121317, #69255, #72465, #138565, #186220, #204586, #167854, #19452, #56237, #201390, #102857, #152667, #4251, #70320, #2117, #68191, #37851, #136437, #202453, #103929, #158019, #44261, #94091, #123467, #43209, #27994, #160130, #155874, #57304, #156947, #60486, #11729, #25850, #174275, #189430, #10661, #7463, #127725, #193684, #77805, #143926, #90888, #141794, #109325, #192609, #61559, #45328, #91959, #175332, #41072, #9607, #110384, #209921, #107179, #26915, #111447, #23719, #73542, #173205, #8538, #126644, #89826, #75684, #207798, #24785, #76733, #139644, #205666, #74620, #140725, #206738, #58369, #59426, #93024, #176389, #124523, #190480, #125584, #42139, #108254, #191544, #142851, #159065, #208855, #163334, #97280, #161201, #66847, #132991, #14914, #195829, #149205, #15978, #64750, #131932, #113582, #81008, #12787, #83125, #112507, #65782, #165451, #82063, #78861, #164395, #146038, #214156, #198991, #47467, #179584, #148155, #147096, #197942, #144982, #177452, #129846, #780, #49570, #115694, #31206, #32261, #99398, #181687, #213120, #33317, #212052, #17046, #50638, #29066, #30129, #210986, #95149, #96218, #63692, #128776, #130892, #48524, #62614, #194753, #46390, #178519, #162269, #196886, #114644, #98329, #13856, #79932, #180637, #169722, #166525, #85271, #86343, #84203, #154554, #167594, #117844, #5056, #134064, #87419, #35445, #53850, #21312, #152415, #153485, #150292, #67919, #103674, #51722, #200073, #183836, #101524, #36514, #71131, #22383, #3994, #52770 ),
 ( #204325, #19193, #151357, #72202, #2926, #68999, #203269, #104745, #182761, #70063, #135116, #136175, #137249, #20259, #38666, #6133, #187033, #201132, #54915, #121066, #116764, #184890, #138310, #202194, #102600, #119983, #185960, #118906, #168655, #34379, #37592, #18116, #170792, #88493, #100452, #1859, #140473, #139379, #158820, #143682, #189179, #60240, #157762, #175085, #44017, #205411, #41891, #57051, #9362, #75434, #206485, #77559, #58115, #142598, #141546, #7203, #126399, #39731, #110136, #26672, #59172, #171863, #73276, #92776, #191294, #42960, #123215, #207552, #192359, #125331, #40816, #122135, #27748, #124274, #76488, #190232, #74371, #174029, #23457, #208608, #55982, #156696, #108002, #93844, #90636, #25600, #109069, #91713, #10416, #176148, #188100, #159882, #11487, #105836, #89569, #155618, #172948, #106924, #24527, #8286, #47223, #194507, #211813, #13620, #33080, #127478, #179346, #160956, #131692, #94905, #61318, #177206, #163096, #164155, #162029, #128541, #193449, #14676, #65547, #212882, #210756, #45093, #181449, #63450, #15741, #79693, #145806, #113341, #28820, #81826, #16798, #95977, #129603, #99155, #29891, #195589, #64513, #30968, #97043, #130658, #111202, #80773, #114400, #197698, #196648, #146860, #112268, #49340, #165208, #48288, #180398, #46155, #32019, #98104, #82882, #12546, #147909, #78621, #115459, #144745, #62377, #178282, #213924, #209674, #101262, #67665, #132744, #119722, #38405, #199823, #20003, #134867, #133809, #35186, #51464, #50394, #150035, #151107, #22115, #117588, #183579, #104487, #167346, #1605, #21054, #136985, #531, #184637, #83944, #36254, #37335, #52519, #70870, #186778, #4792, #18932, #201931, #87151, #148959, #2673, #170530, #102334, #68745, #168406, #86087, #85018, #200874, #66598, #118651, #198746, #185701, #53587, #152163, #54654, #3732, #17861, #103408, #116514, #69807, #153222, #135913, #169469, #203012, #120802, #182504, #34134, #100203, #166269, #24265, #109883, #90370, #174837, #41634, #39469, #92527, #71943, #142349, #207301, #91449, #204066, #105567, #125083, #9105, #75181, #171600, #23192, #191041, #175896, #6941, #158567, #189982, #58924, #76240, #89309, #74113, #155356, #107748, #173774, #156439, #88226, #8022, #26415, #25349, #73022, #10166, #138053, #208359, #42706, #157510, #55718, #139120, #108814, #141293, #59989, #205147, #126143, #192104, #43770, #56790, #154295, #5870, #140208, #121872, #172687, #106661, #206228, #187843, #122958, #188918, #40556, #57855, #124017, #62133, #161775, #30710, #145559, #129356, #162842, #93587, #45901, #146606, #15486, #14420, #178020, #144490, #163910, #213673, #195334, #79442, #12289, #29638, #112019, #65298, #159631, #211557, #193188, #81573, #127219, #11227, #209414, #46965, #196398, #194255, #160696, #77307, #212625, #131444, #78370, #113082, #13368, #210498, #128293, #95723, #143419, #28565, #63192, #115208, #179087, #96793, #197447, #80510, #94652, #114156, #147657, #61060, #64266, #176948, #130410, #48042, #180149, #49088, #27487, #97847, #31775, #44836, #110942, #181198, #37890, #139684, #137540, #103968, #203557, #5346, #117336, #166024, #205706, #170010, #16547, #154846, #88788, #67419, #89863, #51212, #71428, #138603, #186255, #21598, #82629, #155913, #116266, #72504, #172166, #6430, #164955, #171080, #149783, #204626 ),
 ( #22676, #87703, #38960, #106142, #56277, #153776, #122436, #1357, #188394, #40030, #23758, #33882, #148714, #57341, #99960, #133561, #132501, #55210, #121356, #32826, #283, #98902, #7498, #66355, #187331, #105043, #73582, #198499, #50144, #182257, #17609, #83694, #199568, #93061, #90924, #161239, #174313, #124561, #11769, #140761, #94130, #42177, #60525, #28035, #159100, #160169, #156989, #74657, #110423, #58407, #206773, #190520, #108292, #43243, #77842, #29105, #10702, #59464, #208894, #25887, #109362, #143965, #193724, #8577, #142894, #127768, #45368, #41111, #91997, #158057, #209959, #111484, #125623, #191581, #9643, #176426, #107220, #12825, #78900, #177492, #95188, #75719, #26954, #126686, #61598, #145022, #211026, #175371, #123504, #24822, #76771, #189469, #173244, #141833, #192648, #44301, #207838, #166568, #18156, #48562, #81047, #34420, #115735, #194791, #84244, #150330, #199030, #66890, #129884, #180675, #82102, #17086, #100493, #62651, #130932, #820, #178556, #114682, #49610, #50678, #128810, #32300, #196925, #46428, #112546, #30166, #98367, #147132, #96254, #181725, #164430, #83164, #213158, #16016, #162307, #182803, #212089, #165492, #116803, #33356, #13892, #99437, #31242, #149247, #79973, #64788, #148195, #133030, #214195, #146077, #63725, #195868, #14950, #47507, #113619, #179622, #65824, #131972, #97319, #163375, #197982, #104785, #36551, #22422, #170831, #154594, #69036, #51761, #171904, #135154, #184927, #167631, #152452, #87457, #67957, #35486, #23500, #6172, #89607, #185996, #153525, #71169, #101564, #203305, #5094, #54954, #117881, #102638, #37631, #183874, #39774, #52810, #2967, #88532, #19232, #187072, #201171, #137287, #121106, #103710, #38705, #85312, #151396, #72241, #118948, #168694, #20299, #86384, #136214, #138348, #122176, #169761, #4031, #204365, #70100, #202234, #56022, #188141, #53886, #21350, #105879, #1897, #134101, #120021, #200110, #192398, #143718, #157802, #91749, #189217, #142638, #60278, #158856, #57087, #106963, #44054, #76526, #208647, #172987, #175123, #11525, #10453, #156735, #7239, #127514, #9400, #176184, #25637, #174065, #59209, #123252, #27784, #177242, #41928, #75470, #193486, #190271, #141583, #126435, #125366, #42995, #110173, #73316, #207590, #93882, #209710, #159921, #191330, #58153, #77595, #45128, #109108, #26710, #140510, #92812, #61355, #111238, #139419, #28855, #24567, #155657, #40856, #205454, #90673, #8326, #74410, #108040, #206522, #124312, #65576, #198776, #145842, #180431, #80804, #79726, #195626, #211848, #210790, #96012, #97076, #182536, #63485, #129640, #50425, #47261, #162064, #181479, #82913, #160990, #130692, #29928, #196682, #197728, #212914, #16830, #132773, #165237, #113375, #147942, #33109, #94942, #163129, #116544, #48321, #14712, #114432, #32048, #31002, #179381, #12582, #146894, #144782, #131723, #213955, #64548, #561, #98136, #178320, #49368, #78654, #13654, #99186, #164186, #115486, #148986, #15772, #81858, #66627, #62413, #128577, #194542, #46188, #112304, #120831, #201961, #199853, #38435, #17891, #88256, #71972, #102364, #186807, #150065, #86119, #21080, #22142, #55747, #20033, #168434, #83978, #138081, #204095, #152192, #52550, #5899, #87183, #135945, #203040, #184666, #3760, #1636, #154325, #183612, #137013, #121903, #153248, #67695 ),
 ( #18964, #36286, #118681, #34163, #166302, #69835, #51494, #170559, #133842, #100234, #117621, #53617, #54681, #200901, #167375, #35219, #4823, #101295, #85048, #119750, #185729, #151136, #134895, #2702, #68776, #37363, #103437, #169498, #70902, #104515, #143449, #8057, #188947, #60020, #175924, #39499, #9136, #122989, #75210, #76270, #91479, #109913, #11259, #43800, #90399, #26447, #126172, #187871, #41665, #209446, #141321, #107776, #207334, #58956, #124047, #172717, #61091, #173801, #23226, #158596, #92556, #74144, #93616, #57884, #56820, #142378, #105598, #106692, #192135, #125111, #10195, #27517, #40587, #25379, #24295, #191069, #42735, #190013, #171630, #157539, #159659, #108841, #139149, #77336, #89338, #155386, #208387, #174867, #156469, #140237, #206259, #6969, #73050, #205178, #313, #178051, #29669, #82660, #161805, #128324, #213703, #115239, #193221, #162870, #62165, #14450, #15516, #30740, #49121, #164987, #197477, #95753, #180181, #65327, #127250, #195364, #148744, #80541, #46995, #146638, #212653, #63222, #112051, #44867, #113112, #176979, #97880, #31804, #13396, #32857, #211586, #210531, #81601, #110973, #45932, #131474, #64294, #163941, #181229, #194287, #179117, #79472, #130440, #196427, #129385, #28597, #96821, #98932, #48072, #78401, #16577, #94685, #160727, #147686, #114183, #12320, #144521, #145590, #201726, #53367, #17641, #85870, #136766, #84800, #200657, #50176, #170310, #21898, #52306, #150888, #38192, #119502, #168189, #20840, #2450, #118436, #116296, #186564, #1388, #169254, #54444, #185487, #182287, #37113, #34969, #103191, #88008, #68525, #134654, #86939, #36040, #153005, #33913, #66384, #18716, #104264, #4582, #70656, #184423, #135700, #202794, #120586, #102120, #154079, #101041, #132532, #198529, #99989, #133594, #166055, #83726, #199599, #167131, #149817, #19788, #151947, #3518, #67449, #117368, #183365, #51242, #69590, #6731, #92312, #208140, #71727, #41417, #155149, #107524, #108592, #123805, #142127, #43549, #76024, #122741, #58709, #158355, #5646, #73896, #175672, #173555, #139989, #25128, #91231, #156226, #204931, #27260, #206010, #55506, #190822, #124858, #106446, #125929, #90160, #89096, #174620, #93368, #138911, #9948, #157291, #42483, #59770, #72810, #57645, #56582, #8881, #74960, #7803, #137839, #189765, #191887, #141070, #171386, #109670, #203861, #121660, #26196, #207077, #187628, #22977, #39255, #105349, #188704, #40340, #172469, #24057, #79220, #160474, #11003, #131234, #161555, #179927, #29417, #177800, #62963, #126999, #31550, #180978, #45678, #95508, #197223, #194028, #145338, #162617, #129133, #46745, #80285, #77080, #13144, #64040, #147432, #146384, #211339, #61910, #81352, #48863, #112858, #195109, #144278, #178874, #30485, #114978, #143208, #96569, #110726, #213456, #44610, #209198, #192958, #14193, #113931, #111795, #78148, #60838, #130185, #32600, #210272, #212398, #196178, #128072, #47820, #97625, #176726, #12081, #28339, #163683, #15265, #65080, #159404, #94435, #182028, #201464, #186297, #17387, #102931, #200404, #3264, #86677, #33656, #84542, #99731, #52052, #118179, #34717, #120321, #100788, #185224, #184166, #49919, #168992, #82405, #152744, #69332, #101863, #62, #116040, #135443, #19531, #85607, #20591, #36848, #4325, #18464, #165802, #164731, #70395, #166871 ),
 ( #150632, #167931, #2193, #35787, #151696, #16320, #117107, #53108, #136513, #119241, #68269, #1135, #202532, #54181, #98675, #134402, #83470, #148494, #183108, #66126, #132269, #198278, #149550, #67198, #133335, #199339, #50985, #205747, #206814, #204667, #171124, #21636, #8617, #141872, #88832, #123543, #23798, #22718, #138646, #154887, #153820, #39001, #40072, #125661, #6471, #72547, #207881, #56316, #105086, #124602, #25933, #104007, #73624, #187371, #139724, #140803, #155955, #174355, #75764, #108334, #122477, #90967, #190562, #37933, #106184, #59504, #57379, #172208, #189507, #41153, #188438, #89903, #170051, #7541, #107262, #173282, #5391, #87744, #24864, #157030, #58448, #55252, #74699, #42218, #92041, #158098, #9686, #71468, #137581, #203599, #121399, #126730, #142935, #60571, #44344, #114469, #82951, #100273, #81894, #130726, #65610, #208936, #180470, #600, #50463, #76816, #213990, #198817, #116582, #109406, #10745, #110466, #16870, #182577, #196717, #48358, #192690, #181517, #175412, #84015, #150106, #34199, #166339, #176466, #98173, #131760, #149025, #17930, #1678, #32085, #132813, #93102, #164221, #197765, #191623, #14749, #212948, #15808, #26995, #67732, #43286, #147980, #64585, #159143, #33146, #49403, #66666, #115522, #99226, #31038, #97112, #163164, #80841, #146931, #165276, #117660, #120872, #102403, #170599, #23265, #152229, #69874, #186846, #103476, #22186, #35257, #133882, #86158, #171668, #38478, #104555, #3800, #203078, #55787, #154362, #135983, #88301, #168471, #5941, #72012, #138125, #200940, #183652, #89377, #52589, #20069, #85087, #201997, #4864, #199889, #167415, #155426, #204134, #7012, #169538, #70942, #54723, #19006, #121944, #137053, #187910, #101333, #39540, #53656, #36325, #105641, #51535, #87224, #185769, #118716, #119788, #37402, #151171, #2742, #21118, #68812, #134934, #184703, #153288, #40629, #26486, #27559, #25417, #206301, #56860, #43838, #177020, #124090, #158638, #58995, #57925, #173840, #190053, #188985, #74189, #75249, #160769, #41705, #107815, #28637, #91523, #140281, #159698, #61129, #139188, #108885, #8099, #174908, #175965, #191110, #209488, #111015, #143492, #157581, #126216, #11297, #73087, #141362, #94724, #92596, #207375, #10235, #76310, #9174, #125151, #205218, #42777, #123034, #109954, #192177, #142417, #193260, #208426, #156510, #93655, #106732, #60060, #77376, #127289, #44907, #172759, #24334, #90442, #29711, #212696, #130479, #113154, #16618, #179159, #213742, #64337, #112092, #131512, #144561, #115276, #97920, #48111, #62205, #178094, #15553, #180221, #31843, #197515, #65365, #49159, #96862, #95792, #12362, #32894, #30783, #181268, #162910, #47038, #80582, #194329, #98972, #82700, #195409, #14492, #165024, #63263, #146680, #114223, #196469, #163978, #81640, #210571, #147725, #78441, #128362, #45971, #161849, #13437, #79514, #145632, #211628, #129425, #155640, #176169, #74393, #11510, #44038, #175108, #39756, #42982, #24549, #92796, #159903, #140495, #206505, #109092, #25622, #158841, #171887, #56006, #8309, #93865, #26694, #10438, #58136, #125351, #192384, #76510, #124295, #142621, #90656, #208630, #60263, #126420, #123236, #105861, #77581, #189201, #156718, #7224, #190254, #141567, #122157, #89591, #143704, #110156, #188125, #91734, #207575, #191314, #73300, #27769 ) ),
 .UNSPECIFIED., .T., .F., .T. ) 
 B_SPLINE_SURFACE_WITH_KNOTS ( ( 4, 3, 4 ),
 ( 4, 1, 1, 1, 1, 1, 1, 1, 1, 1, 1, 1, 1, 1, 1, 1, 1, 1, 1, 1, 1, 1, 1, 1, 1, 1, 1, 1, 1, 1, 1, 1, 1, 1, 1, 1, 1, 1, 1, 1, 1, 1, 1, 1, 1, 1, 1, 1, 1, 1, 1, 1, 1, 1, 1, 1, 1, 1, 1, 1, 1, 1, 1, 1, 1, 1, 1, 1, 1, 1, 1, 1, 1, 1, 1, 1, 1, 1, 1, 1, 1, 1, 1, 1, 1, 1, 1, 1, 1, 1, 1, 1, 1, 1, 1, 1, 1, 1, 1, 1, 1, 1, 1, 1, 1, 1, 1, 1, 1, 1, 1, 1, 1, 1, 1, 1, 1, 1, 1, 1, 1, 1, 1, 1, 1, 1, 1, 1, 1, 1, 1, 1, 1, 1, 1, 1, 1, 1, 1, 1, 1, 1, 1, 1, 1, 1, 1, 1, 1, 1, 1, 1, 1, 1, 1, 1, 1, 1, 1, 1, 1, 1, 1, 1, 1, 1, 1, 1, 1, 1, 1, 1, 1, 1, 1, 1, 1, 1, 1, 1, 1, 1, 1, 1, 1, 1, 1, 1, 1, 1, 1, 1, 1, 1, 1, 1, 1, 1, 1, 1, 1, 1, 1, 1, 1, 1, 1, 1, 1, 1, 1, 1, 1, 1, 1, 1, 1, 1, 1, 1, 1, 1, 1, 1, 1, 1, 1, 1, 1, 1, 1, 1, 1, 1, 1, 1, 1, 1, 1, 1, 1, 1, 1, 1, 1, 1, 1, 1, 1, 1, 1, 1, 1, 1, 1, 1, 1, 1, 1, 1, 1, 1, 1, 1, 1, 1, 1, 1, 1, 1, 1, 1, 1, 1, 1, 1, 1, 1, 1, 1, 1, 1, 1, 1, 1, 1, 1, 1, 1, 1, 1, 1, 1, 1, 1, 1, 1, 1, 1, 1, 1, 1, 1, 1, 1, 1, 1, 1, 1, 1, 1, 1, 1, 1, 1, 1, 1, 1, 1, 1, 1, 1, 1, 1, 1, 1, 1, 1, 1, 1, 1, 1, 1, 1, 1, 1, 1, 1, 1, 1, 1, 1, 1, 1, 1, 1, 1, 1, 1, 1, 1, 1, 1, 1, 1, 1, 1, 1, 1, 1, 1, 1, 1, 1, 1, 1, 1, 1, 1, 1, 1, 1, 1, 1, 1, 1, 1, 1, 1, 1, 1, 1, 1, 1, 4 ),
 ( 0.000000000000000000, 0.5000000000000000000, 1.000000000000000000 ),
 ( 0.000000000000000000, 0.002599974731368114196, 0.005208790931971673047, 0.007813145979665977320, 0.01041652777592116073, 0.01302061325022423749, 0.01562498222773845216, 0.01822909327250534645, 0.02083329118620782031, 0.02343750764584028035, 0.02604160881127103033, 0.02864587273906003470, 0.03124992668191499748, 0.03385418289307650513, 0.03645825757725845717, 0.03906249379052053466, 0.04166666320740203266, 0.04427081823557592333, 0.04687506849204003262, 0.04947913642841410276, 0.05208339700068515682, 0.05468745344639398126, 0.05729170333903113588, 0.05989581325979084075, 0.06250002080062810883, 0.06510424464624173235, 0.06770834408375023261, 0.07031260355790951155, 0.07291665769283758869, 0.07552091454841564078, 0.07812498837240108851, 0.08072922377910608793, 0.08333339284475561881, 0.08593754734057650058, 0.08854179710653446722, 0.09114586450482109470, 0.09375012458370637902, 0.09635418052565795921, 0.09895842987840544613, 0.1015625393267825388, 0.1041667463075427041, 0.1067709697059155277, 0.1093750686050062593, 0.1119793276133541904, 0.1145833812402851093, 0.1171876375884709082, 0.1197917109360151500, 0.1223959458003068407, 0.1250001144218755300, 0.1276042683764700425, 0.1302085177025434359, 0.1328125845892443313, 0.1354168441945610146, 0.1380208996559441903, 0.1406251484930516882, 0.1432292574929059925, 0.1458334639374244401, 0.1484376869122458475, 0.1510417852965526830, 0.1536460438630466996, 0.1562500970055218374, 0.1588543528702505148, 0.1614584257649260002, 0.1640626601106844606, 0.1666668283118819260, 0.1692709817489688462, 0.1718752306590244638, 0.1744792970577103974, 0.1770835562133957763, 0.1796876112177483997, 0.1822918595631332073, 0.1848959681380851483, 0.1875001740701665309, 0.1901043966452301559, 0.1927084945383780445, 0.1953127526869259389, 0.1979168053684795814, 0.2005210607736844508, 0.2031251332390507092, 0.2057293670901427229, 0.2083335348946688259, 0.2109376878379560227, 0.2135419363558502259, 0.2161460022900811573, 0.2187502610200618980, 0.2213543155909112325, 0.2239585634684796434, 0.2265626716421396125, 0.2291668770855771753, 0.2317710992846666596, 0.2343751967102698508, 0.2369794544647692847, 0.2395835067089256143, 0.2421877616785296505, 0.2447918337381362330, 0.2473960671184182170, 0.2500002345499632850, 0.2526043870231480248, 0.2552086351727278490, 0.2578127006660536624, 0.2604169589942467167, 0.2630210131551104502, 0.2656252605887587936, 0.2682293683847277177, 0.2708335733633049913, 0.2734377952101950116, 0.2760418921918580404, 0.2786461495761977103, 0.2812502014064713896, 0.2838544559643880194, 0.2864585276417753179, 0.2890627605750938911, 0.2916669276573394809, 0.2942710796841097043, 0.2968753274892133587, 0.2994793925651746958, 0.3020836505154881335, 0.3046877042898750165, 0.3072919513034905736, 0.3098960587453611915, 0.3125002632828523530, 0.3151044848013095923, 0.3177085813626279731, 0.3203128384006882490, 0.3229168898405855304, 0.3255211440107198539, 0.3281252153294201834, 0.3307294478396133885, 0.3333336145962333963, 0.3359377662002681064, 0.3385420136847264727, 0.3411460783668558427, 0.3437503359631899347, 0.3463543893746011126, 0.3489586359920627823, 0.3515627431034201722, 0.3541669472235909888, 0.3567711684373747749, 0.3593752646019360286, 0.3619795213175900916, 0.3645835723906095116, 0.3671878261968588575, 0.3697918971803975663, 0.3723961292912953969, 0.3750002957459567798, 0.3776044469509276524, 0.3802086941385645069, 0.3828127584503868142, 0.3854170157166348365, 0.3880210687885642384, 0.3906253150337437030, 0.3932294218381663375, 0.3958336255647753599, 0.3984378464976386924, 0.4010419422890235119, 0.4036461987061379930, 0.4062502494357712601, 0.4088545029020263510, 0.4114585735739221262, 0.4140628053093475813, 0.4166669714857112461, 0.4192711223152827404, 0.4218753692299160307, 0.4244794331949501842, 0.4270836901549991405, 0.4296877429109347002, 0.4322919888076972583, 0.4348960953287579478, 0.4375002986855570652, 0.4401045193612476147, 0.4427086148030301427, 0.4453128709454660106, 0.4479169213551993378, 0.4505211745053449013, 0.4531252448891109341, 0.4557294762728811288, 0.4583336421946030970, 0.4609377926724337327, 0.4635420393378766879, 0.4661461029796354349, 0.4687503596573671660, 0.4713544121207915438, 0.4739586576929967765, 0.4765627639542633909, 0.4791669669649988861, 0.4817711874072597711, 0.4843752825230089321, 0.4869795384146229367, 0.4895835885279371524, 0.4921878413858530310, 0.4947919115049980165, 0.4973961425609249032, 0.5000003082516567554, 0.5026044584014001115, 0.5052087048414615200, 0.5078127681834534446, 0.5104170246027455171, 0.5130210767971369323, 0.5156253220686399796, 0.5182294280936764475, 0.5208336307820899957, 0.5234378510146604491, 0.5260419458279406157, 0.5286462014925853437, 0.5312502513329574461, 0.5338545039225196520, 0.5364585738005485105, 0.5390628045524396006, 0.5416669700358295314, 0.5442711198811350792, 0.5468753661196208427, 0.5494794291853500878, 0.5520836853700766822, 0.5546877373189100791, 0.5572919823135623618, 0.5598960881259297251, 0.5625002905157588939, 0.5651045105623757614, 0.5677086050967478092, 0.5703128605582734600, 0.5729169101491768945, 0.5755211624942581095, 0.5781252321546730411, 0.5807294626263322934, 0.5833336279260263879, 0.5859377774905402125, 0.5885420235512536236, 0.5911460863642216124, 0.5937503423382545220, 0.5963543940650019026, 0.5989586388066517886, 0.6015627444299086468, 0.6041669465448881171, 0.6067711664292861906, 0.6093752607083083861, 0.6119795159905627724, 0.6145835653554690969, 0.6171878174799397820, 0.6197918869462408775, 0.6223961171614702526, 0.6250002823011129305, 0.6276044316084782304, 0.6302086775152213605, 0.6328127400989277396, 0.6354169958861367595, 0.6380210474142689048, 0.6406252919267632073, 0.6432293973844667168, 0.6458335992483292820, 0.6484378189942425763, 0.6510419130414711875, 0.6536461681683013447, 0.6562502173306804520, 0.6588544692584096252, 0.6614585385540960871, 0.6640627685366956579, 0.6666669335399304508, 0.6692710826137896474, 0.6718753283903641238, 0.6744793907683068745, 0.6770836463925611337, 0.6796876977455479363, 0.6822919420527318035, 0.6848960473684391204, 0.6875002490049163528, 0.6901044686360783276, 0.6927085624750688453, 0.6953128174703216979, 0.6979168664536427036, 0.7005211182084990496, 0.7031251873570698585, 0.7057294171308388098, 0.7083335820213095824, 0.7109377308853042088, 0.7135419765555117699, 0.7161460387511890957, 0.7187502942363581671, 0.7213543454376690756, 0.7239585895633880996, 0.7265626947606567132, 0.7291668961934797411, 0.7317711157336249661, 0.7343752093879328813, 0.7369794642754557978, 0.7395835131031885945, 0.7421877647090413532, 0.7447918337339959338, 0.7473960633227341166, 0.7500002281240860658, 0.7526043768018576552, 0.7552086223895014827, 0.7578126844264116979, 0.7604169397963658206, 0.7630209908694718379, 0.7656252348375721661, 0.7682293399399604539, 0.7708335411928610714, 0.7734377606657260040, 0.7760418541589074737, 0.7786461089625497101, 0.7812501576581653007, 0.7838544091388848223, 0.7864584780637244865, 0.7890627074912324179, 0.7916668722271122949, 0.7942710207423038238, 0.7968752662711893198, 0.7994793281728324041, 0.8020835834514440377, 0.8046876344198176101, 0.8072918782541467220, 0.8098959832852158369, 0.8125001843819276148, 0.8151044038112509327, 0.8177084971668638902, 0.8203127519104773668, 0.8229168004974481976, 0.8255210518769072747, 0.8281251207251358881, 0.8307293500152160837, 0.8333335147092740813, 0.8359376630855301915, 0.8385419085794658667, 0.8411459703693440204, 0.8437502255804886220, 0.8463542764676049712, 0.8489585201920134550, 0.8515626251753276588, 0.8541668261395859441, 0.8567710455491102106, 0.8593751387907155870, 0.8619793934981552219, 0.8645834419999574028, 0.8671876933020320477, 0.8697917620971562513, 0.8723959912736143352, 0.8750001559495040881, 0.8776043042104727521, 0.8802085496932706699, 0.8828126113948897569, 0.8854168665624462253, 0.8880209173917842369, 0.8906251610301256783, 0.8932292659892527853, 0.8958334668447968108, 0.8984376862582688084, 0.9010417794094305322, 0.9036460341045560174, 0.9062500825446693220, 0.9088543337932389887, 0.9114584025587700866, 0.9140626316454156797, 0.9166667963267953745, 0.9192709444961273402, 0.9218751899916067805, 0.9244792516284782158, 0.9270835067763207871, 0.9296875575713596795, 0.9322918011475309630, 0.9348959061060417852, 0.9375001068764983181, 0.9401043263176916964, 0.9427084194022110619, 0.9453126741091559815, 0.9479167225106870376, 0.9505209737258253355, 0.9531250424882484751, 0.9557292715345466760, 0.9583334362123939743, 0.9609375841976093291, 0.9635418299546441023, 0.9661458919105455623, 0.9687501459642621215, 0.9713541960184646218, 0.9739584433044384815, 0.9765625494917742344, 0.9791667425299969141, 0.9817709508269629737, 0.9843750450459556323, 0.9869794226472197174, 0.9895834977571079660, 0.9921868632736227100, 0.9947912224625704569, 0.9974000159472320437, 1.000000000000000000 ),
 .UNSPECIFIED. ) 
 GEOMETRIC_REPRESENTATION_ITEM ( )  RATIONAL_B_SPLINE_SURFACE ( (
 ( 1.000000000000000000, 1.000000000000000000, 1.000000000000000000, 1.000000000000000222, 0.9999999999999997780, 1.000000000000000444, 0.9999999999999997780, 1.000000000000000222, 0.9999999999999996669, 1.000000000000000000, 1.000000000000000000, 1.000000000000000222, 1.000000000000000000, 1.000000000000000000, 0.9999999999999997780, 1.000000000000000000, 1.000000000000000000, 1.000000000000000000, 0.9999999999999997780, 1.000000000000000444, 0.9999999999999997780, 1.000000000000000222, 1.000000000000000000, 0.9999999999999997780, 1.000000000000000000, 1.000000000000000222, 0.9999999999999997780, 1.000000000000000222, 0.9999999999999997780, 1.000000000000000222, 1.000000000000000000, 0.9999999999999997780, 1.000000000000000444, 0.9999999999999997780, 1.000000000000000222, 0.9999999999999997780, 1.000000000000000444, 1.000000000000000000, 1.000000000000000000, 1.000000000000000000, 1.000000000000000000, 1.000000000000000000, 1.000000000000000000, 0.9999999999999997780, 1.000000000000000222, 0.9999999999999996669, 1.000000000000000444, 0.9999999999999994449, 1.000000000000000222, 1.000000000000000000, 1.000000000000000000, 1.000000000000000000, 1.000000000000000000, 1.000000000000000000, 0.9999999999999996669, 1.000000000000000444, 0.9999999999999997780, 1.000000000000000222, 0.9999999999999996669, 1.000000000000000000, 1.000000000000000000, 1.000000000000000222, 0.9999999999999997780, 1.000000000000000000, 1.000000000000000222, 0.9999999999999997780, 1.000000000000000000, 0.9999999999999997780, 1.000000000000000222, 0.9999999999999997780, 1.000000000000000444, 0.9999999999999994449, 1.000000000000000444, 0.9999999999999997780, 0.9999999999999997780, 1.000000000000000444, 0.9999999999999996669, 1.000000000000000000, 1.000000000000000000, 1.000000000000000000, 1.000000000000000000, 1.000000000000000222, 1.000000000000000000, 1.000000000000000000, 0.9999999999999996669, 1.000000000000000222, 1.000000000000000000, 0.9999999999999997780, 0.9999999999999997780, 0.9999999999999997780, 1.000000000000000000, 1.000000000000000222, 0.9999999999999997780, 1.000000000000000222, 0.9999999999999996669, 1.000000000000000444, 0.9999999999999997780, 1.000000000000000222, 1.000000000000000222, 0.9999999999999997780, 1.000000000000000222, 1.000000000000000000, 0.9999999999999997780, 1.000000000000000444, 1.000000000000000000, 1.000000000000000000, 1.000000000000000222, 1.000000000000000000, 1.000000000000000000, 1.000000000000000222, 0.9999999999999993339, 1.000000000000000444, 1.000000000000000222, 0.9999999999999997780, 1.000000000000000000, 1.000000000000000222, 1.000000000000000444, 1.000000000000000000, 1.000000000000000222, 0.9999999999999997780, 1.000000000000000222, 0.9999999999999997780, 1.000000000000000222, 1.000000000000000000, 0.9999999999999997780, 0.9999999999999996669, 1.000000000000000444, 0.9999999999999997780, 1.000000000000000444, 0.9999999999999997780, 1.000000000000000222, 1.000000000000000222, 1.000000000000000000, 0.9999999999999997780, 1.000000000000000222, 0.9999999999999997780, 1.000000000000000000, 1.000000000000000000, 1.000000000000000000, 0.9999999999999997780, 1.000000000000000222, 1.000000000000000000, 1.000000000000000000, 1.000000000000000000, 1.000000000000000222, 1.000000000000000222, 0.9999999999999994449, 1.000000000000000222, 1.000000000000000000, 0.9999999999999994449, 1.000000000000000444, 0.9999999999999997780, 1.000000000000000222, 0.9999999999999996669, 1.000000000000000444, 1.000000000000000000, 0.9999999999999996669, 1.000000000000000444, 0.9999999999999997780, 1.000000000000000000, 1.000000000000000444, 1.000000000000000000, 1.000000000000000222, 0.9999999999999996669, 1.000000000000000000, 0.9999999999999997780, 0.9999999999999997780, 1.000000000000000222, 1.000000000000000000, 1.000000000000000444, 0.9999999999999996669, 1.000000000000000222, 0.9999999999999997780, 0.9999999999999997780, 1.000000000000000444, 0.9999999999999997780, 1.000000000000000444, 0.9999999999999996669, 1.000000000000000222, 0.9999999999999996669, 1.000000000000000222, 0.9999999999999997780, 1.000000000000000444, 1.000000000000000222, 0.9999999999999996669, 1.000000000000000444, 0.9999999999999996669, 1.000000000000000000, 0.9999999999999997780, 1.000000000000000000, 1.000000000000000000, 1.000000000000000222, 0.9999999999999994449, 1.000000000000000444, 0.9999999999999993339, 1.000000000000000666, 0.9999999999999994449, 1.000000000000000222, 1.000000000000000222, 1.000000000000000000, 1.000000000000000000, 0.9999999999999997780, 1.000000000000000222, 0.9999999999999996669, 1.000000000000000222, 0.9999999999999996669, 1.000000000000000222, 1.000000000000000000, 1.000000000000000222, 0.9999999999999997780, 1.000000000000000222, 1.000000000000000222, 1.000000000000000000, 0.9999999999999997780, 1.000000000000000222, 1.000000000000000222, 1.000000000000000000, 1.000000000000000000, 1.000000000000000222, 0.9999999999999997780, 1.000000000000000000, 1.000000000000000222, 0.9999999999999996669, 0.9999999999999997780, 1.000000000000000222, 0.9999999999999997780, 1.000000000000000000, 0.9999999999999997780, 0.9999999999999997780, 1.000000000000000222, 1.000000000000000000, 1.000000000000000000, 1.000000000000000222, 0.9999999999999996669, 1.000000000000000444, 1.000000000000000000, 1.000000000000000222, 0.9999999999999997780, 1.000000000000000222, 0.9999999999999997780, 1.000000000000000444, 0.9999999999999997780, 1.000000000000000222, 0.9999999999999997780, 1.000000000000000222, 0.9999999999999997780, 1.000000000000000222, 1.000000000000000000, 1.000000000000000222, 1.000000000000000000, 1.000000000000000000, 1.000000000000000222, 1.000000000000000000, 1.000000000000000000, 0.9999999999999997780, 1.000000000000000000, 1.000000000000000444, 0.9999999999999996669, 1.000000000000000222, 0.9999999999999997780, 1.000000000000000000, 0.9999999999999997780, 1.000000000000000222, 1.000000000000000222, 1.000000000000000000, 1.000000000000000000, 0.9999999999999996669, 1.000000000000000444, 0.9999999999999997780, 1.000000000000000000, 1.000000000000000222, 0.9999999999999996669, 1.000000000000000444, 1.000000000000000000, 0.9999999999999997780, 1.000000000000000222, 0.9999999999999997780, 1.000000000000000000, 1.000000000000000000, 1.000000000000000000, 1.000000000000000000, 1.000000000000000000, 1.000000000000000222, 1.000000000000000444, 0.9999999999999997780, 1.000000000000000222, 1.000000000000000000, 1.000000000000000444, 0.9999999999999997780, 1.000000000000000222, 0.9999999999999997780, 1.000000000000000222, 0.9999999999999997780, 1.000000000000000222, 1.000000000000000000, 1.000000000000000222, 1.000000000000000222, 1.000000000000000222, 0.9999999999999997780, 1.000000000000000222, 0.9999999999999997780, 1.000000000000000222, 0.9999999999999997780, 1.000000000000000444, 0.9999999999999996669, 1.000000000000000444, 1.000000000000000000, 1.000000000000000000, 0.9999999999999997780, 1.000000000000000222, 1.000000000000000000, 0.9999999999999997780, 1.000000000000000000, 0.9999999999999997780, 1.000000000000000222, 1.000000000000000000, 1.000000000000000000, 1.000000000000000222, 0.9999999999999997780, 1.000000000000000444, 0.9999999999999996669, 1.000000000000000222, 1.000000000000000222, 0.9999999999999997780, 1.000000000000000000, 0.9999999999999997780, 1.000000000000000000, 0.9999999999999996669, 1.000000000000000444, 0.9999999999999997780, 1.000000000000000222, 1.000000000000000000, 1.000000000000000000, 1.000000000000000000, 0.9999999999999997780, 0.9999999999999997780, 1.000000000000000000, 0.9999999999999997780, 1.000000000000000444, 0.9999999999999996669, 1.000000000000000222, 1.000000000000000000, 1.000000000000000444, 1.000000000000000222, 1.000000000000000000, 0.9999999999999997780, 1.000000000000000222, 1.000000000000000444, 0.9999999999999997780, 1.000000000000000222, 0.9999999999999997780, 1.000000000000000000, 1.000000000000000000, 1.000000000000000222, 0.9999999999999997780, 1.000000000000000222, 1.000000000000000000, 1.000000000000000222, 0.9999999999999997780, 1.000000000000000000, 1.000000000000000222, 1.000000000000000000, 1.000000000000000222, 1.000000000000000000, 1.000000000000000000, 0.9999999999999997780, 1.000000000000000444, 0.9999999999999997780, 1.000000000000000000, 1.000000000000000000, 1.000000000000000444, 0.9999999999999996669, 1.000000000000000222, 1.000000000000000000, 0.9999999999999996669, 1.000000000000000444, 0.9999999999999996669, 1.000000000000000444, 0.9999999999999997780, 1.000000000000000222, 0.9999999999999997780, 1.000000000000000222, 1.000000000000000222, 1.000000000000000222, 1.000000000000000000, 1.000000000000000000, 1.000000000000000000),
 ( 0.3333333333333333703, 0.3333333333333333703, 0.3333333333333334259, 0.3333333333333334259, 0.3333333333333333703, 0.3333333333333334259, 0.3333333333333333148, 0.3333333333333333703, 0.3333333333333333148, 0.3333333333333333703, 0.3333333333333333703, 0.3333333333333334259, 0.3333333333333333703, 0.3333333333333333703, 0.3333333333333333703, 0.3333333333333333703, 0.3333333333333333703, 0.3333333333333333148, 0.3333333333333333703, 0.3333333333333334814, 0.3333333333333333148, 0.3333333333333334259, 0.3333333333333333148, 0.3333333333333334259, 0.3333333333333332593, 0.3333333333333335369, 0.3333333333333333703, 0.3333333333333333703, 0.3333333333333333703, 0.3333333333333333703, 0.3333333333333333703, 0.3333333333333333703, 0.3333333333333334259, 0.3333333333333333703, 0.3333333333333333703, 0.3333333333333333703, 0.3333333333333334814, 0.3333333333333333703, 0.3333333333333333703, 0.3333333333333333703, 0.3333333333333334259, 0.3333333333333332593, 0.3333333333333334814, 0.3333333333333332593, 0.3333333333333334259, 0.3333333333333332038, 0.3333333333333335369, 0.3333333333333332593, 0.3333333333333334814, 0.3333333333333333703, 0.3333333333333333148, 0.3333333333333333703, 0.3333333333333333703, 0.3333333333333333148, 0.3333333333333333148, 0.3333333333333334814, 0.3333333333333332593, 0.3333333333333334259, 0.3333333333333332593, 0.3333333333333333703, 0.3333333333333333703, 0.3333333333333334259, 0.3333333333333333148, 0.3333333333333333148, 0.3333333333333334259, 0.3333333333333333703, 0.3333333333333333703, 0.3333333333333333703, 0.3333333333333334814, 0.3333333333333332038, 0.3333333333333335924, 0.3333333333333332593, 0.3333333333333335369, 0.3333333333333333148, 0.3333333333333332593, 0.3333333333333335924, 0.3333333333333332038, 0.3333333333333333703, 0.3333333333333333703, 0.3333333333333334259, 0.3333333333333333148, 0.3333333333333334259, 0.3333333333333333703, 0.3333333333333334259, 0.3333333333333332038, 0.3333333333333333703, 0.3333333333333333703, 0.3333333333333333703, 0.3333333333333332593, 0.3333333333333333703, 0.3333333333333333148, 0.3333333333333334259, 0.3333333333333333148, 0.3333333333333334259, 0.3333333333333333148, 0.3333333333333334814, 0.3333333333333333703, 0.3333333333333334259, 0.3333333333333333703, 0.3333333333333333148, 0.3333333333333333703, 0.3333333333333334259, 0.3333333333333333148, 0.3333333333333334814, 0.3333333333333334259, 0.3333333333333333703, 0.3333333333333334259, 0.3333333333333333703, 0.3333333333333334259, 0.3333333333333334814, 0.3333333333333332038, 0.3333333333333334259, 0.3333333333333334259, 0.3333333333333333703, 0.3333333333333333148, 0.3333333333333334259, 0.3333333333333334259, 0.3333333333333334259, 0.3333333333333333703, 0.3333333333333333148, 0.3333333333333334259, 0.3333333333333333703, 0.3333333333333334259, 0.3333333333333333703, 0.3333333333333333148, 0.3333333333333332593, 0.3333333333333334259, 0.3333333333333333148, 0.3333333333333335369, 0.3333333333333332593, 0.3333333333333334814, 0.3333333333333334259, 0.3333333333333334259, 0.3333333333333333148, 0.3333333333333334259, 0.3333333333333333148, 0.3333333333333333148, 0.3333333333333333703, 0.3333333333333333703, 0.3333333333333332593, 0.3333333333333334259, 0.3333333333333333148, 0.3333333333333333703, 0.3333333333333334259, 0.3333333333333333148, 0.3333333333333334814, 0.3333333333333332593, 0.3333333333333333703, 0.3333333333333334259, 0.3333333333333332038, 0.3333333333333335369, 0.3333333333333333703, 0.3333333333333333703, 0.3333333333333333148, 0.3333333333333334259, 0.3333333333333333703, 0.3333333333333332593, 0.3333333333333335369, 0.3333333333333332593, 0.3333333333333333703, 0.3333333333333334814, 0.3333333333333333703, 0.3333333333333334259, 0.3333333333333332593, 0.3333333333333334259, 0.3333333333333332593, 0.3333333333333333703, 0.3333333333333334259, 0.3333333333333333703, 0.3333333333333334814, 0.3333333333333332593, 0.3333333333333333703, 0.3333333333333333703, 0.3333333333333333703, 0.3333333333333334259, 0.3333333333333333148, 0.3333333333333334259, 0.3333333333333332593, 0.3333333333333333703, 0.3333333333333332593, 0.3333333333333334814, 0.3333333333333333703, 0.3333333333333334259, 0.3333333333333334259, 0.3333333333333332593, 0.3333333333333334814, 0.3333333333333333148, 0.3333333333333333148, 0.3333333333333333148, 0.3333333333333333703, 0.3333333333333333703, 0.3333333333333334259, 0.3333333333333332593, 0.3333333333333335369, 0.3333333333333332038, 0.3333333333333335924, 0.3333333333333332593, 0.3333333333333334814, 0.3333333333333333703, 0.3333333333333333703, 0.3333333333333333703, 0.3333333333333333148, 0.3333333333333334259, 0.3333333333333333703, 0.3333333333333333703, 0.3333333333333333148, 0.3333333333333333703, 0.3333333333333333148, 0.3333333333333333703, 0.3333333333333332593, 0.3333333333333334259, 0.3333333333333333703, 0.3333333333333334259, 0.3333333333333333148, 0.3333333333333334259, 0.3333333333333333703, 0.3333333333333334259, 0.3333333333333334259, 0.3333333333333334259, 0.3333333333333332593, 0.3333333333333334259, 0.3333333333333333703, 0.3333333333333333148, 0.3333333333333333148, 0.3333333333333335369, 0.3333333333333332593, 0.3333333333333333148, 0.3333333333333333703, 0.3333333333333333148, 0.3333333333333334814, 0.3333333333333333703, 0.3333333333333334814, 0.3333333333333333703, 0.3333333333333332593, 0.3333333333333334259, 0.3333333333333333703, 0.3333333333333335369, 0.3333333333333333148, 0.3333333333333334259, 0.3333333333333333148, 0.3333333333333335924, 0.3333333333333332593, 0.3333333333333334259, 0.3333333333333334259, 0.3333333333333333703, 0.3333333333333333703, 0.3333333333333334259, 0.3333333333333334259, 0.3333333333333334259, 0.3333333333333333703, 0.3333333333333333703, 0.3333333333333334259, 0.3333333333333333148, 0.3333333333333333703, 0.3333333333333332038, 0.3333333333333334259, 0.3333333333333334814, 0.3333333333333332593, 0.3333333333333333703, 0.3333333333333333148, 0.3333333333333334814, 0.3333333333333332593, 0.3333333333333334259, 0.3333333333333333703, 0.3333333333333333703, 0.3333333333333333703, 0.3333333333333333148, 0.3333333333333334259, 0.3333333333333333703, 0.3333333333333333148, 0.3333333333333334259, 0.3333333333333332038, 0.3333333333333334259, 0.3333333333333333703, 0.3333333333333333703, 0.3333333333333333703, 0.3333333333333334259, 0.3333333333333333148, 0.3333333333333333703, 0.3333333333333333703, 0.3333333333333333703, 0.3333333333333333703, 0.3333333333333334259, 0.3333333333333334814, 0.3333333333333332593, 0.3333333333333333703, 0.3333333333333334259, 0.3333333333333334814, 0.3333333333333333148, 0.3333333333333333703, 0.3333333333333333703, 0.3333333333333334259, 0.3333333333333333148, 0.3333333333333334814, 0.3333333333333333148, 0.3333333333333334814, 0.3333333333333333703, 0.3333333333333334814, 0.3333333333333333148, 0.3333333333333334259, 0.3333333333333332593, 0.3333333333333335369, 0.3333333333333333148, 0.3333333333333334814, 0.3333333333333333148, 0.3333333333333334259, 0.3333333333333333703, 0.3333333333333333148, 0.3333333333333333703, 0.3333333333333333703, 0.3333333333333334259, 0.3333333333333333148, 0.3333333333333334259, 0.3333333333333333148, 0.3333333333333334814, 0.3333333333333333148, 0.3333333333333334259, 0.3333333333333334259, 0.3333333333333333703, 0.3333333333333334259, 0.3333333333333333703, 0.3333333333333333703, 0.3333333333333335369, 0.3333333333333332593, 0.3333333333333334259, 0.3333333333333333703, 0.3333333333333333703, 0.3333333333333333148, 0.3333333333333335369, 0.3333333333333333148, 0.3333333333333334259, 0.3333333333333333703, 0.3333333333333333703, 0.3333333333333334259, 0.3333333333333333148, 0.3333333333333333703, 0.3333333333333333148, 0.3333333333333333148, 0.3333333333333334814, 0.3333333333333332593, 0.3333333333333334259, 0.3333333333333333703, 0.3333333333333334814, 0.3333333333333334259, 0.3333333333333333148, 0.3333333333333333703, 0.3333333333333333703, 0.3333333333333335369, 0.3333333333333333148, 0.3333333333333334259, 0.3333333333333333703, 0.3333333333333333148, 0.3333333333333334259, 0.3333333333333334259, 0.3333333333333333703, 0.3333333333333333703, 0.3333333333333334259, 0.3333333333333334259, 0.3333333333333333703, 0.3333333333333333148, 0.3333333333333334259, 0.3333333333333333703, 0.3333333333333334814, 0.3333333333333333703, 0.3333333333333333703, 0.3333333333333333703, 0.3333333333333334259, 0.3333333333333333148, 0.3333333333333333703, 0.3333333333333334259, 0.3333333333333334259, 0.3333333333333333148, 0.3333333333333333703, 0.3333333333333333148, 0.3333333333333333703, 0.3333333333333335369, 0.3333333333333333148, 0.3333333333333334259, 0.3333333333333333703, 0.3333333333333334259, 0.3333333333333333148, 0.3333333333333333148, 0.3333333333333335369, 0.3333333333333333703, 0.3333333333333333148, 0.3333333333333333703, 0.3333333333333333703),
 ( 0.3333333333333333703, 0.3333333333333333703, 0.3333333333333334259, 0.3333333333333334259, 0.3333333333333333703, 0.3333333333333334259, 0.3333333333333333148, 0.3333333333333333703, 0.3333333333333333148, 0.3333333333333333703, 0.3333333333333333703, 0.3333333333333334259, 0.3333333333333333703, 0.3333333333333333703, 0.3333333333333333703, 0.3333333333333333703, 0.3333333333333333703, 0.3333333333333333148, 0.3333333333333333703, 0.3333333333333334814, 0.3333333333333333148, 0.3333333333333334259, 0.3333333333333333148, 0.3333333333333334259, 0.3333333333333332593, 0.3333333333333335369, 0.3333333333333333703, 0.3333333333333333703, 0.3333333333333333703, 0.3333333333333333703, 0.3333333333333333703, 0.3333333333333333703, 0.3333333333333334259, 0.3333333333333333703, 0.3333333333333333703, 0.3333333333333333703, 0.3333333333333334814, 0.3333333333333333703, 0.3333333333333333703, 0.3333333333333333703, 0.3333333333333334259, 0.3333333333333332593, 0.3333333333333334814, 0.3333333333333332593, 0.3333333333333334259, 0.3333333333333332038, 0.3333333333333335369, 0.3333333333333332593, 0.3333333333333334814, 0.3333333333333333703, 0.3333333333333333148, 0.3333333333333333703, 0.3333333333333333703, 0.3333333333333333148, 0.3333333333333333148, 0.3333333333333334814, 0.3333333333333332593, 0.3333333333333334259, 0.3333333333333332593, 0.3333333333333333703, 0.3333333333333333703, 0.3333333333333334259, 0.3333333333333333148, 0.3333333333333333148, 0.3333333333333334259, 0.3333333333333333703, 0.3333333333333333703, 0.3333333333333333703, 0.3333333333333334814, 0.3333333333333332038, 0.3333333333333335924, 0.3333333333333332593, 0.3333333333333335369, 0.3333333333333333148, 0.3333333333333332593, 0.3333333333333335924, 0.3333333333333332038, 0.3333333333333333703, 0.3333333333333333703, 0.3333333333333334259, 0.3333333333333333148, 0.3333333333333334259, 0.3333333333333333703, 0.3333333333333334259, 0.3333333333333332038, 0.3333333333333333703, 0.3333333333333333703, 0.3333333333333333703, 0.3333333333333332593, 0.3333333333333333703, 0.3333333333333333148, 0.3333333333333334259, 0.3333333333333333148, 0.3333333333333334259, 0.3333333333333333148, 0.3333333333333334814, 0.3333333333333333703, 0.3333333333333334259, 0.3333333333333333703, 0.3333333333333333148, 0.3333333333333333703, 0.3333333333333334259, 0.3333333333333333148, 0.3333333333333334814, 0.3333333333333334259, 0.3333333333333333703, 0.3333333333333334259, 0.3333333333333333703, 0.3333333333333334259, 0.3333333333333334814, 0.3333333333333332038, 0.3333333333333334259, 0.3333333333333334259, 0.3333333333333333703, 0.3333333333333333148, 0.3333333333333334259, 0.3333333333333334259, 0.3333333333333334259, 0.3333333333333333703, 0.3333333333333333148, 0.3333333333333334259, 0.3333333333333333703, 0.3333333333333334259, 0.3333333333333333703, 0.3333333333333333148, 0.3333333333333332593, 0.3333333333333334259, 0.3333333333333333148, 0.3333333333333335369, 0.3333333333333332593, 0.3333333333333334814, 0.3333333333333334259, 0.3333333333333334259, 0.3333333333333333148, 0.3333333333333334259, 0.3333333333333333148, 0.3333333333333333148, 0.3333333333333333703, 0.3333333333333333703, 0.3333333333333332593, 0.3333333333333334259, 0.3333333333333333148, 0.3333333333333333703, 0.3333333333333334259, 0.3333333333333333148, 0.3333333333333334814, 0.3333333333333332593, 0.3333333333333333703, 0.3333333333333334259, 0.3333333333333332038, 0.3333333333333335369, 0.3333333333333333703, 0.3333333333333333703, 0.3333333333333333148, 0.3333333333333334259, 0.3333333333333333703, 0.3333333333333332593, 0.3333333333333335369, 0.3333333333333332593, 0.3333333333333333703, 0.3333333333333334814, 0.3333333333333333703, 0.3333333333333334259, 0.3333333333333332593, 0.3333333333333334259, 0.3333333333333332593, 0.3333333333333333703, 0.3333333333333334259, 0.3333333333333333703, 0.3333333333333334814, 0.3333333333333332593, 0.3333333333333333703, 0.3333333333333333703, 0.3333333333333333703, 0.3333333333333334259, 0.3333333333333333148, 0.3333333333333334259, 0.3333333333333332593, 0.3333333333333333703, 0.3333333333333332593, 0.3333333333333334814, 0.3333333333333333703, 0.3333333333333334259, 0.3333333333333334259, 0.3333333333333332593, 0.3333333333333334814, 0.3333333333333333148, 0.3333333333333333148, 0.3333333333333333148, 0.3333333333333333703, 0.3333333333333333703, 0.3333333333333334259, 0.3333333333333332593, 0.3333333333333335369, 0.3333333333333332038, 0.3333333333333335924, 0.3333333333333332593, 0.3333333333333334814, 0.3333333333333333703, 0.3333333333333333703, 0.3333333333333333703, 0.3333333333333333148, 0.3333333333333334259, 0.3333333333333333703, 0.3333333333333333703, 0.3333333333333333148, 0.3333333333333333703, 0.3333333333333333148, 0.3333333333333333703, 0.3333333333333332593, 0.3333333333333334259, 0.3333333333333333703, 0.3333333333333334259, 0.3333333333333333148, 0.3333333333333334259, 0.3333333333333333703, 0.3333333333333334259, 0.3333333333333334259, 0.3333333333333334259, 0.3333333333333332593, 0.3333333333333334259, 0.3333333333333333703, 0.3333333333333333148, 0.3333333333333333148, 0.3333333333333335369, 0.3333333333333332593, 0.3333333333333333148, 0.3333333333333333703, 0.3333333333333333148, 0.3333333333333334814, 0.3333333333333333703, 0.3333333333333334814, 0.3333333333333333703, 0.3333333333333332593, 0.3333333333333334259, 0.3333333333333333703, 0.3333333333333335369, 0.3333333333333333148, 0.3333333333333334259, 0.3333333333333333148, 0.3333333333333335924, 0.3333333333333332593, 0.3333333333333334259, 0.3333333333333334259, 0.3333333333333333703, 0.3333333333333333703, 0.3333333333333334259, 0.3333333333333334259, 0.3333333333333334259, 0.3333333333333333703, 0.3333333333333333703, 0.3333333333333334259, 0.3333333333333333148, 0.3333333333333333703, 0.3333333333333332038, 0.3333333333333334259, 0.3333333333333334814, 0.3333333333333332593, 0.3333333333333333703, 0.3333333333333333148, 0.3333333333333334814, 0.3333333333333332593, 0.3333333333333334259, 0.3333333333333333703, 0.3333333333333333703, 0.3333333333333333703, 0.3333333333333333148, 0.3333333333333334259, 0.3333333333333333703, 0.3333333333333333148, 0.3333333333333334259, 0.3333333333333332038, 0.3333333333333334259, 0.3333333333333333703, 0.3333333333333333703, 0.3333333333333333703, 0.3333333333333334259, 0.3333333333333333148, 0.3333333333333333703, 0.3333333333333333703, 0.3333333333333333703, 0.3333333333333333703, 0.3333333333333334259, 0.3333333333333334814, 0.3333333333333332593, 0.3333333333333333703, 0.3333333333333334259, 0.3333333333333334814, 0.3333333333333333148, 0.3333333333333333703, 0.3333333333333333703, 0.3333333333333334259, 0.3333333333333333148, 0.3333333333333334814, 0.3333333333333333148, 0.3333333333333334814, 0.3333333333333333703, 0.3333333333333334814, 0.3333333333333333148, 0.3333333333333334259, 0.3333333333333332593, 0.3333333333333335369, 0.3333333333333333148, 0.3333333333333334814, 0.3333333333333333148, 0.3333333333333334259, 0.3333333333333333703, 0.3333333333333333148, 0.3333333333333333703, 0.3333333333333333703, 0.3333333333333334259, 0.3333333333333333148, 0.3333333333333334259, 0.3333333333333333148, 0.3333333333333334814, 0.3333333333333333148, 0.3333333333333334259, 0.3333333333333334259, 0.3333333333333333703, 0.3333333333333334259, 0.3333333333333333703, 0.3333333333333333703, 0.3333333333333335369, 0.3333333333333332593, 0.3333333333333334259, 0.3333333333333333703, 0.3333333333333333703, 0.3333333333333333148, 0.3333333333333335369, 0.3333333333333333148, 0.3333333333333334259, 0.3333333333333333703, 0.3333333333333333703, 0.3333333333333334259, 0.3333333333333333148, 0.3333333333333333703, 0.3333333333333333148, 0.3333333333333333148, 0.3333333333333334814, 0.3333333333333332593, 0.3333333333333334259, 0.3333333333333333703, 0.3333333333333334814, 0.3333333333333334259, 0.3333333333333333148, 0.3333333333333333703, 0.3333333333333333703, 0.3333333333333335369, 0.3333333333333333148, 0.3333333333333334259, 0.3333333333333333703, 0.3333333333333333148, 0.3333333333333334259, 0.3333333333333334259, 0.3333333333333333703, 0.3333333333333333703, 0.3333333333333334259, 0.3333333333333334259, 0.3333333333333333703, 0.3333333333333333148, 0.3333333333333334259, 0.3333333333333333703, 0.3333333333333334814, 0.3333333333333333703, 0.3333333333333333703, 0.3333333333333333703, 0.3333333333333334259, 0.3333333333333333148, 0.3333333333333333703, 0.3333333333333334259, 0.3333333333333334259, 0.3333333333333333148, 0.3333333333333333703, 0.3333333333333333148, 0.3333333333333333703, 0.3333333333333335369, 0.3333333333333333148, 0.3333333333333334259, 0.3333333333333333703, 0.3333333333333334259, 0.3333333333333333148, 0.3333333333333333148, 0.3333333333333335369, 0.3333333333333333703, 0.3333333333333333148, 0.3333333333333333703, 0.3333333333333333703),
 ( 1.000000000000000000, 1.000000000000000000, 1.000000000000000000, 1.000000000000000222, 0.9999999999999997780, 1.000000000000000444, 0.9999999999999997780, 1.000000000000000222, 0.9999999999999996669, 1.000000000000000000, 1.000000000000000000, 1.000000000000000222, 1.000000000000000000, 1.000000000000000000, 0.9999999999999997780, 1.000000000000000000, 1.000000000000000000, 1.000000000000000000, 0.9999999999999997780, 1.000000000000000444, 0.9999999999999997780, 1.000000000000000222, 1.000000000000000000, 0.9999999999999997780, 1.000000000000000000, 1.000000000000000222, 0.9999999999999997780, 1.000000000000000222, 0.9999999999999997780, 1.000000000000000222, 1.000000000000000000, 0.9999999999999997780, 1.000000000000000444, 0.9999999999999997780, 1.000000000000000222, 0.9999999999999997780, 1.000000000000000444, 1.000000000000000000, 1.000000000000000000, 1.000000000000000000, 1.000000000000000000, 1.000000000000000000, 1.000000000000000000, 0.9999999999999997780, 1.000000000000000222, 0.9999999999999996669, 1.000000000000000444, 0.9999999999999994449, 1.000000000000000222, 1.000000000000000000, 1.000000000000000000, 1.000000000000000000, 1.000000000000000000, 1.000000000000000000, 0.9999999999999996669, 1.000000000000000444, 0.9999999999999997780, 1.000000000000000222, 0.9999999999999996669, 1.000000000000000000, 1.000000000000000000, 1.000000000000000222, 0.9999999999999997780, 1.000000000000000000, 1.000000000000000222, 0.9999999999999997780, 1.000000000000000000, 0.9999999999999997780, 1.000000000000000222, 0.9999999999999997780, 1.000000000000000444, 0.9999999999999994449, 1.000000000000000444, 0.9999999999999997780, 0.9999999999999997780, 1.000000000000000444, 0.9999999999999996669, 1.000000000000000000, 1.000000000000000000, 1.000000000000000000, 1.000000000000000000, 1.000000000000000222, 1.000000000000000000, 1.000000000000000000, 0.9999999999999996669, 1.000000000000000222, 1.000000000000000000, 0.9999999999999997780, 0.9999999999999997780, 0.9999999999999997780, 1.000000000000000000, 1.000000000000000222, 0.9999999999999997780, 1.000000000000000222, 0.9999999999999996669, 1.000000000000000444, 0.9999999999999997780, 1.000000000000000222, 1.000000000000000222, 0.9999999999999997780, 1.000000000000000222, 1.000000000000000000, 0.9999999999999997780, 1.000000000000000444, 1.000000000000000000, 1.000000000000000000, 1.000000000000000222, 1.000000000000000000, 1.000000000000000000, 1.000000000000000222, 0.9999999999999993339, 1.000000000000000444, 1.000000000000000222, 0.9999999999999997780, 1.000000000000000000, 1.000000000000000222, 1.000000000000000444, 1.000000000000000000, 1.000000000000000222, 0.9999999999999997780, 1.000000000000000222, 0.9999999999999997780, 1.000000000000000222, 1.000000000000000000, 0.9999999999999997780, 0.9999999999999996669, 1.000000000000000444, 0.9999999999999997780, 1.000000000000000444, 0.9999999999999997780, 1.000000000000000222, 1.000000000000000222, 1.000000000000000000, 0.9999999999999997780, 1.000000000000000222, 0.9999999999999997780, 1.000000000000000000, 1.000000000000000000, 1.000000000000000000, 0.9999999999999997780, 1.000000000000000222, 1.000000000000000000, 1.000000000000000000, 1.000000000000000000, 1.000000000000000222, 1.000000000000000222, 0.9999999999999994449, 1.000000000000000222, 1.000000000000000000, 0.9999999999999994449, 1.000000000000000444, 0.9999999999999997780, 1.000000000000000222, 0.9999999999999996669, 1.000000000000000444, 1.000000000000000000, 0.9999999999999996669, 1.000000000000000444, 0.9999999999999997780, 1.000000000000000000, 1.000000000000000444, 1.000000000000000000, 1.000000000000000222, 0.9999999999999996669, 1.000000000000000000, 0.9999999999999997780, 0.9999999999999997780, 1.000000000000000222, 1.000000000000000000, 1.000000000000000444, 0.9999999999999996669, 1.000000000000000222, 0.9999999999999997780, 0.9999999999999997780, 1.000000000000000444, 0.9999999999999997780, 1.000000000000000444, 0.9999999999999996669, 1.000000000000000222, 0.9999999999999996669, 1.000000000000000222, 0.9999999999999997780, 1.000000000000000444, 1.000000000000000222, 0.9999999999999996669, 1.000000000000000444, 0.9999999999999996669, 1.000000000000000000, 0.9999999999999997780, 1.000000000000000000, 1.000000000000000000, 1.000000000000000222, 0.9999999999999994449, 1.000000000000000444, 0.9999999999999993339, 1.000000000000000666, 0.9999999999999994449, 1.000000000000000222, 1.000000000000000222, 1.000000000000000000, 1.000000000000000000, 0.9999999999999997780, 1.000000000000000222, 0.9999999999999996669, 1.000000000000000222, 0.9999999999999996669, 1.000000000000000222, 1.000000000000000000, 1.000000000000000222, 0.9999999999999997780, 1.000000000000000222, 1.000000000000000222, 1.000000000000000000, 0.9999999999999997780, 1.000000000000000222, 1.000000000000000222, 1.000000000000000000, 1.000000000000000000, 1.000000000000000222, 0.9999999999999997780, 1.000000000000000000, 1.000000000000000222, 0.9999999999999996669, 0.9999999999999997780, 1.000000000000000222, 0.9999999999999997780, 1.000000000000000000, 0.9999999999999997780, 0.9999999999999997780, 1.000000000000000222, 1.000000000000000000, 1.000000000000000000, 1.000000000000000222, 0.9999999999999996669, 1.000000000000000444, 1.000000000000000000, 1.000000000000000222, 0.9999999999999997780, 1.000000000000000222, 0.9999999999999997780, 1.000000000000000444, 0.9999999999999997780, 1.000000000000000222, 0.9999999999999997780, 1.000000000000000222, 0.9999999999999997780, 1.000000000000000222, 1.000000000000000000, 1.000000000000000222, 1.000000000000000000, 1.000000000000000000, 1.000000000000000222, 1.000000000000000000, 1.000000000000000000, 0.9999999999999997780, 1.000000000000000000, 1.000000000000000444, 0.9999999999999996669, 1.000000000000000222, 0.9999999999999997780, 1.000000000000000000, 0.9999999999999997780, 1.000000000000000222, 1.000000000000000222, 1.000000000000000000, 1.000000000000000000, 0.9999999999999996669, 1.000000000000000444, 0.9999999999999997780, 1.000000000000000000, 1.000000000000000222, 0.9999999999999996669, 1.000000000000000444, 1.000000000000000000, 0.9999999999999997780, 1.000000000000000222, 0.9999999999999997780, 1.000000000000000000, 1.000000000000000000, 1.000000000000000000, 1.000000000000000000, 1.000000000000000000, 1.000000000000000222, 1.000000000000000444, 0.9999999999999997780, 1.000000000000000222, 1.000000000000000000, 1.000000000000000444, 0.9999999999999997780, 1.000000000000000222, 0.9999999999999997780, 1.000000000000000222, 0.9999999999999997780, 1.000000000000000222, 1.000000000000000000, 1.000000000000000222, 1.000000000000000222, 1.000000000000000222, 0.9999999999999997780, 1.000000000000000222, 0.9999999999999997780, 1.000000000000000222, 0.9999999999999997780, 1.000000000000000444, 0.9999999999999996669, 1.000000000000000444, 1.000000000000000000, 1.000000000000000000, 0.9999999999999997780, 1.000000000000000222, 1.000000000000000000, 0.9999999999999997780, 1.000000000000000000, 0.9999999999999997780, 1.000000000000000222, 1.000000000000000000, 1.000000000000000000, 1.000000000000000222, 0.9999999999999997780, 1.000000000000000444, 0.9999999999999996669, 1.000000000000000222, 1.000000000000000222, 0.9999999999999997780, 1.000000000000000000, 0.9999999999999997780, 1.000000000000000000, 0.9999999999999996669, 1.000000000000000444, 0.9999999999999997780, 1.000000000000000222, 1.000000000000000000, 1.000000000000000000, 1.000000000000000000, 0.9999999999999997780, 0.9999999999999997780, 1.000000000000000000, 0.9999999999999997780, 1.000000000000000444, 0.9999999999999996669, 1.000000000000000222, 1.000000000000000000, 1.000000000000000444, 1.000000000000000222, 1.000000000000000000, 0.9999999999999997780, 1.000000000000000222, 1.000000000000000444, 0.9999999999999997780, 1.000000000000000222, 0.9999999999999997780, 1.000000000000000000, 1.000000000000000000, 1.000000000000000222, 0.9999999999999997780, 1.000000000000000222, 1.000000000000000000, 1.000000000000000222, 0.9999999999999997780, 1.000000000000000000, 1.000000000000000222, 1.000000000000000000, 1.000000000000000222, 1.000000000000000000, 1.000000000000000000, 0.9999999999999997780, 1.000000000000000444, 0.9999999999999997780, 1.000000000000000000, 1.000000000000000000, 1.000000000000000444, 0.9999999999999996669, 1.000000000000000222, 1.000000000000000000, 0.9999999999999996669, 1.000000000000000444, 0.9999999999999996669, 1.000000000000000444, 0.9999999999999997780, 1.000000000000000222, 0.9999999999999997780, 1.000000000000000222, 1.000000000000000222, 1.000000000000000222, 1.000000000000000000, 1.000000000000000000, 1.000000000000000000),
 ( 0.3333333333333333703, 0.3333333333333333703, 0.3333333333333334259, 0.3333333333333334259, 0.3333333333333333703, 0.3333333333333334259, 0.3333333333333333148, 0.3333333333333333703, 0.3333333333333333148, 0.3333333333333333703, 0.3333333333333333703, 0.3333333333333334259, 0.3333333333333333703, 0.3333333333333333703, 0.3333333333333333703, 0.3333333333333333703, 0.3333333333333333703, 0.3333333333333333148, 0.3333333333333333703, 0.3333333333333334814, 0.3333333333333333148, 0.3333333333333334259, 0.3333333333333333148, 0.3333333333333334259, 0.3333333333333332593, 0.3333333333333335369, 0.3333333333333333703, 0.3333333333333333703, 0.3333333333333333703, 0.3333333333333333703, 0.3333333333333333703, 0.3333333333333333703, 0.3333333333333334259, 0.3333333333333333703, 0.3333333333333333703, 0.3333333333333333703, 0.3333333333333334814, 0.3333333333333333703, 0.3333333333333333703, 0.3333333333333333703, 0.3333333333333334259, 0.3333333333333332593, 0.3333333333333334814, 0.3333333333333332593, 0.3333333333333334259, 0.3333333333333332038, 0.3333333333333335369, 0.3333333333333332593, 0.3333333333333334814, 0.3333333333333333703, 0.3333333333333333148, 0.3333333333333333703, 0.3333333333333333703, 0.3333333333333333148, 0.3333333333333333148, 0.3333333333333334814, 0.3333333333333332593, 0.3333333333333334259, 0.3333333333333332593, 0.3333333333333333703, 0.3333333333333333703, 0.3333333333333334259, 0.3333333333333333148, 0.3333333333333333148, 0.3333333333333334259, 0.3333333333333333703, 0.3333333333333333703, 0.3333333333333333703, 0.3333333333333334814, 0.3333333333333332038, 0.3333333333333335924, 0.3333333333333332593, 0.3333333333333335369, 0.3333333333333333148, 0.3333333333333332593, 0.3333333333333335924, 0.3333333333333332038, 0.3333333333333333703, 0.3333333333333333703, 0.3333333333333334259, 0.3333333333333333148, 0.3333333333333334259, 0.3333333333333333703, 0.3333333333333334259, 0.3333333333333332038, 0.3333333333333333703, 0.3333333333333333703, 0.3333333333333333703, 0.3333333333333332593, 0.3333333333333333703, 0.3333333333333333148, 0.3333333333333334259, 0.3333333333333333148, 0.3333333333333334259, 0.3333333333333333148, 0.3333333333333334814, 0.3333333333333333703, 0.3333333333333334259, 0.3333333333333333703, 0.3333333333333333148, 0.3333333333333333703, 0.3333333333333334259, 0.3333333333333333148, 0.3333333333333334814, 0.3333333333333334259, 0.3333333333333333703, 0.3333333333333334259, 0.3333333333333333703, 0.3333333333333334259, 0.3333333333333334814, 0.3333333333333332038, 0.3333333333333334259, 0.3333333333333334259, 0.3333333333333333703, 0.3333333333333333148, 0.3333333333333334259, 0.3333333333333334259, 0.3333333333333334259, 0.3333333333333333703, 0.3333333333333333148, 0.3333333333333334259, 0.3333333333333333703, 0.3333333333333334259, 0.3333333333333333703, 0.3333333333333333148, 0.3333333333333332593, 0.3333333333333334259, 0.3333333333333333148, 0.3333333333333335369, 0.3333333333333332593, 0.3333333333333334814, 0.3333333333333334259, 0.3333333333333334259, 0.3333333333333333148, 0.3333333333333334259, 0.3333333333333333148, 0.3333333333333333148, 0.3333333333333333703, 0.3333333333333333703, 0.3333333333333332593, 0.3333333333333334259, 0.3333333333333333148, 0.3333333333333333703, 0.3333333333333334259, 0.3333333333333333148, 0.3333333333333334814, 0.3333333333333332593, 0.3333333333333333703, 0.3333333333333334259, 0.3333333333333332038, 0.3333333333333335369, 0.3333333333333333703, 0.3333333333333333703, 0.3333333333333333148, 0.3333333333333334259, 0.3333333333333333703, 0.3333333333333332593, 0.3333333333333335369, 0.3333333333333332593, 0.3333333333333333703, 0.3333333333333334814, 0.3333333333333333703, 0.3333333333333334259, 0.3333333333333332593, 0.3333333333333334259, 0.3333333333333332593, 0.3333333333333333703, 0.3333333333333334259, 0.3333333333333333703, 0.3333333333333334814, 0.3333333333333332593, 0.3333333333333333703, 0.3333333333333333703, 0.3333333333333333703, 0.3333333333333334259, 0.3333333333333333148, 0.3333333333333334259, 0.3333333333333332593, 0.3333333333333333703, 0.3333333333333332593, 0.3333333333333334814, 0.3333333333333333703, 0.3333333333333334259, 0.3333333333333334259, 0.3333333333333332593, 0.3333333333333334814, 0.3333333333333333148, 0.3333333333333333148, 0.3333333333333333148, 0.3333333333333333703, 0.3333333333333333703, 0.3333333333333334259, 0.3333333333333332593, 0.3333333333333335369, 0.3333333333333332038, 0.3333333333333335924, 0.3333333333333332593, 0.3333333333333334814, 0.3333333333333333703, 0.3333333333333333703, 0.3333333333333333703, 0.3333333333333333148, 0.3333333333333334259, 0.3333333333333333703, 0.3333333333333333703, 0.3333333333333333148, 0.3333333333333333703, 0.3333333333333333148, 0.3333333333333333703, 0.3333333333333332593, 0.3333333333333334259, 0.3333333333333333703, 0.3333333333333334259, 0.3333333333333333148, 0.3333333333333334259, 0.3333333333333333703, 0.3333333333333334259, 0.3333333333333334259, 0.3333333333333334259, 0.3333333333333332593, 0.3333333333333334259, 0.3333333333333333703, 0.3333333333333333148, 0.3333333333333333148, 0.3333333333333335369, 0.3333333333333332593, 0.3333333333333333148, 0.3333333333333333703, 0.3333333333333333148, 0.3333333333333334814, 0.3333333333333333703, 0.3333333333333334814, 0.3333333333333333703, 0.3333333333333332593, 0.3333333333333334259, 0.3333333333333333703, 0.3333333333333335369, 0.3333333333333333148, 0.3333333333333334259, 0.3333333333333333148, 0.3333333333333335924, 0.3333333333333332593, 0.3333333333333334259, 0.3333333333333334259, 0.3333333333333333703, 0.3333333333333333703, 0.3333333333333334259, 0.3333333333333334259, 0.3333333333333334259, 0.3333333333333333703, 0.3333333333333333703, 0.3333333333333334259, 0.3333333333333333148, 0.3333333333333333703, 0.3333333333333332038, 0.3333333333333334259, 0.3333333333333334814, 0.3333333333333332593, 0.3333333333333333703, 0.3333333333333333148, 0.3333333333333334814, 0.3333333333333332593, 0.3333333333333334259, 0.3333333333333333703, 0.3333333333333333703, 0.3333333333333333703, 0.3333333333333333148, 0.3333333333333334259, 0.3333333333333333703, 0.3333333333333333148, 0.3333333333333334259, 0.3333333333333332038, 0.3333333333333334259, 0.3333333333333333703, 0.3333333333333333703, 0.3333333333333333703, 0.3333333333333334259, 0.3333333333333333148, 0.3333333333333333703, 0.3333333333333333703, 0.3333333333333333703, 0.3333333333333333703, 0.3333333333333334259, 0.3333333333333334814, 0.3333333333333332593, 0.3333333333333333703, 0.3333333333333334259, 0.3333333333333334814, 0.3333333333333333148, 0.3333333333333333703, 0.3333333333333333703, 0.3333333333333334259, 0.3333333333333333148, 0.3333333333333334814, 0.3333333333333333148, 0.3333333333333334814, 0.3333333333333333703, 0.3333333333333334814, 0.3333333333333333148, 0.3333333333333334259, 0.3333333333333332593, 0.3333333333333335369, 0.3333333333333333148, 0.3333333333333334814, 0.3333333333333333148, 0.3333333333333334259, 0.3333333333333333703, 0.3333333333333333148, 0.3333333333333333703, 0.3333333333333333703, 0.3333333333333334259, 0.3333333333333333148, 0.3333333333333334259, 0.3333333333333333148, 0.3333333333333334814, 0.3333333333333333148, 0.3333333333333334259, 0.3333333333333334259, 0.3333333333333333703, 0.3333333333333334259, 0.3333333333333333703, 0.3333333333333333703, 0.3333333333333335369, 0.3333333333333332593, 0.3333333333333334259, 0.3333333333333333703, 0.3333333333333333703, 0.3333333333333333148, 0.3333333333333335369, 0.3333333333333333148, 0.3333333333333334259, 0.3333333333333333703, 0.3333333333333333703, 0.3333333333333334259, 0.3333333333333333148, 0.3333333333333333703, 0.3333333333333333148, 0.3333333333333333148, 0.3333333333333334814, 0.3333333333333332593, 0.3333333333333334259, 0.3333333333333333703, 0.3333333333333334814, 0.3333333333333334259, 0.3333333333333333148, 0.3333333333333333703, 0.3333333333333333703, 0.3333333333333335369, 0.3333333333333333148, 0.3333333333333334259, 0.3333333333333333703, 0.3333333333333333148, 0.3333333333333334259, 0.3333333333333334259, 0.3333333333333333703, 0.3333333333333333703, 0.3333333333333334259, 0.3333333333333334259, 0.3333333333333333703, 0.3333333333333333148, 0.3333333333333334259, 0.3333333333333333703, 0.3333333333333334814, 0.3333333333333333703, 0.3333333333333333703, 0.3333333333333333703, 0.3333333333333334259, 0.3333333333333333148, 0.3333333333333333703, 0.3333333333333334259, 0.3333333333333334259, 0.3333333333333333148, 0.3333333333333333703, 0.3333333333333333148, 0.3333333333333333703, 0.3333333333333335369, 0.3333333333333333148, 0.3333333333333334259, 0.3333333333333333703, 0.3333333333333334259, 0.3333333333333333148, 0.3333333333333333148, 0.3333333333333335369, 0.3333333333333333703, 0.3333333333333333148, 0.3333333333333333703, 0.3333333333333333703),
 ( 0.3333333333333333703, 0.3333333333333333703, 0.3333333333333334259, 0.3333333333333334259, 0.3333333333333333703, 0.3333333333333334259, 0.3333333333333333148, 0.3333333333333333703, 0.3333333333333333148, 0.3333333333333333703, 0.3333333333333333703, 0.3333333333333334259, 0.3333333333333333703, 0.3333333333333333703, 0.3333333333333333703, 0.3333333333333333703, 0.3333333333333333703, 0.3333333333333333148, 0.3333333333333333703, 0.3333333333333334814, 0.3333333333333333148, 0.3333333333333334259, 0.3333333333333333148, 0.3333333333333334259, 0.3333333333333332593, 0.3333333333333335369, 0.3333333333333333703, 0.3333333333333333703, 0.3333333333333333703, 0.3333333333333333703, 0.3333333333333333703, 0.3333333333333333703, 0.3333333333333334259, 0.3333333333333333703, 0.3333333333333333703, 0.3333333333333333703, 0.3333333333333334814, 0.3333333333333333703, 0.3333333333333333703, 0.3333333333333333703, 0.3333333333333334259, 0.3333333333333332593, 0.3333333333333334814, 0.3333333333333332593, 0.3333333333333334259, 0.3333333333333332038, 0.3333333333333335369, 0.3333333333333332593, 0.3333333333333334814, 0.3333333333333333703, 0.3333333333333333148, 0.3333333333333333703, 0.3333333333333333703, 0.3333333333333333148, 0.3333333333333333148, 0.3333333333333334814, 0.3333333333333332593, 0.3333333333333334259, 0.3333333333333332593, 0.3333333333333333703, 0.3333333333333333703, 0.3333333333333334259, 0.3333333333333333148, 0.3333333333333333148, 0.3333333333333334259, 0.3333333333333333703, 0.3333333333333333703, 0.3333333333333333703, 0.3333333333333334814, 0.3333333333333332038, 0.3333333333333335924, 0.3333333333333332593, 0.3333333333333335369, 0.3333333333333333148, 0.3333333333333332593, 0.3333333333333335924, 0.3333333333333332038, 0.3333333333333333703, 0.3333333333333333703, 0.3333333333333334259, 0.3333333333333333148, 0.3333333333333334259, 0.3333333333333333703, 0.3333333333333334259, 0.3333333333333332038, 0.3333333333333333703, 0.3333333333333333703, 0.3333333333333333703, 0.3333333333333332593, 0.3333333333333333703, 0.3333333333333333148, 0.3333333333333334259, 0.3333333333333333148, 0.3333333333333334259, 0.3333333333333333148, 0.3333333333333334814, 0.3333333333333333703, 0.3333333333333334259, 0.3333333333333333703, 0.3333333333333333148, 0.3333333333333333703, 0.3333333333333334259, 0.3333333333333333148, 0.3333333333333334814, 0.3333333333333334259, 0.3333333333333333703, 0.3333333333333334259, 0.3333333333333333703, 0.3333333333333334259, 0.3333333333333334814, 0.3333333333333332038, 0.3333333333333334259, 0.3333333333333334259, 0.3333333333333333703, 0.3333333333333333148, 0.3333333333333334259, 0.3333333333333334259, 0.3333333333333334259, 0.3333333333333333703, 0.3333333333333333148, 0.3333333333333334259, 0.3333333333333333703, 0.3333333333333334259, 0.3333333333333333703, 0.3333333333333333148, 0.3333333333333332593, 0.3333333333333334259, 0.3333333333333333148, 0.3333333333333335369, 0.3333333333333332593, 0.3333333333333334814, 0.3333333333333334259, 0.3333333333333334259, 0.3333333333333333148, 0.3333333333333334259, 0.3333333333333333148, 0.3333333333333333148, 0.3333333333333333703, 0.3333333333333333703, 0.3333333333333332593, 0.3333333333333334259, 0.3333333333333333148, 0.3333333333333333703, 0.3333333333333334259, 0.3333333333333333148, 0.3333333333333334814, 0.3333333333333332593, 0.3333333333333333703, 0.3333333333333334259, 0.3333333333333332038, 0.3333333333333335369, 0.3333333333333333703, 0.3333333333333333703, 0.3333333333333333148, 0.3333333333333334259, 0.3333333333333333703, 0.3333333333333332593, 0.3333333333333335369, 0.3333333333333332593, 0.3333333333333333703, 0.3333333333333334814, 0.3333333333333333703, 0.3333333333333334259, 0.3333333333333332593, 0.3333333333333334259, 0.3333333333333332593, 0.3333333333333333703, 0.3333333333333334259, 0.3333333333333333703, 0.3333333333333334814, 0.3333333333333332593, 0.3333333333333333703, 0.3333333333333333703, 0.3333333333333333703, 0.3333333333333334259, 0.3333333333333333148, 0.3333333333333334259, 0.3333333333333332593, 0.3333333333333333703, 0.3333333333333332593, 0.3333333333333334814, 0.3333333333333333703, 0.3333333333333334259, 0.3333333333333334259, 0.3333333333333332593, 0.3333333333333334814, 0.3333333333333333148, 0.3333333333333333148, 0.3333333333333333148, 0.3333333333333333703, 0.3333333333333333703, 0.3333333333333334259, 0.3333333333333332593, 0.3333333333333335369, 0.3333333333333332038, 0.3333333333333335924, 0.3333333333333332593, 0.3333333333333334814, 0.3333333333333333703, 0.3333333333333333703, 0.3333333333333333703, 0.3333333333333333148, 0.3333333333333334259, 0.3333333333333333703, 0.3333333333333333703, 0.3333333333333333148, 0.3333333333333333703, 0.3333333333333333148, 0.3333333333333333703, 0.3333333333333332593, 0.3333333333333334259, 0.3333333333333333703, 0.3333333333333334259, 0.3333333333333333148, 0.3333333333333334259, 0.3333333333333333703, 0.3333333333333334259, 0.3333333333333334259, 0.3333333333333334259, 0.3333333333333332593, 0.3333333333333334259, 0.3333333333333333703, 0.3333333333333333148, 0.3333333333333333148, 0.3333333333333335369, 0.3333333333333332593, 0.3333333333333333148, 0.3333333333333333703, 0.3333333333333333148, 0.3333333333333334814, 0.3333333333333333703, 0.3333333333333334814, 0.3333333333333333703, 0.3333333333333332593, 0.3333333333333334259, 0.3333333333333333703, 0.3333333333333335369, 0.3333333333333333148, 0.3333333333333334259, 0.3333333333333333148, 0.3333333333333335924, 0.3333333333333332593, 0.3333333333333334259, 0.3333333333333334259, 0.3333333333333333703, 0.3333333333333333703, 0.3333333333333334259, 0.3333333333333334259, 0.3333333333333334259, 0.3333333333333333703, 0.3333333333333333703, 0.3333333333333334259, 0.3333333333333333148, 0.3333333333333333703, 0.3333333333333332038, 0.3333333333333334259, 0.3333333333333334814, 0.3333333333333332593, 0.3333333333333333703, 0.3333333333333333148, 0.3333333333333334814, 0.3333333333333332593, 0.3333333333333334259, 0.3333333333333333703, 0.3333333333333333703, 0.3333333333333333703, 0.3333333333333333148, 0.3333333333333334259, 0.3333333333333333703, 0.3333333333333333148, 0.3333333333333334259, 0.3333333333333332038, 0.3333333333333334259, 0.3333333333333333703, 0.3333333333333333703, 0.3333333333333333703, 0.3333333333333334259, 0.3333333333333333148, 0.3333333333333333703, 0.3333333333333333703, 0.3333333333333333703, 0.3333333333333333703, 0.3333333333333334259, 0.3333333333333334814, 0.3333333333333332593, 0.3333333333333333703, 0.3333333333333334259, 0.3333333333333334814, 0.3333333333333333148, 0.3333333333333333703, 0.3333333333333333703, 0.3333333333333334259, 0.3333333333333333148, 0.3333333333333334814, 0.3333333333333333148, 0.3333333333333334814, 0.3333333333333333703, 0.3333333333333334814, 0.3333333333333333148, 0.3333333333333334259, 0.3333333333333332593, 0.3333333333333335369, 0.3333333333333333148, 0.3333333333333334814, 0.3333333333333333148, 0.3333333333333334259, 0.3333333333333333703, 0.3333333333333333148, 0.3333333333333333703, 0.3333333333333333703, 0.3333333333333334259, 0.3333333333333333148, 0.3333333333333334259, 0.3333333333333333148, 0.3333333333333334814, 0.3333333333333333148, 0.3333333333333334259, 0.3333333333333334259, 0.3333333333333333703, 0.3333333333333334259, 0.3333333333333333703, 0.3333333333333333703, 0.3333333333333335369, 0.3333333333333332593, 0.3333333333333334259, 0.3333333333333333703, 0.3333333333333333703, 0.3333333333333333148, 0.3333333333333335369, 0.3333333333333333148, 0.3333333333333334259, 0.3333333333333333703, 0.3333333333333333703, 0.3333333333333334259, 0.3333333333333333148, 0.3333333333333333703, 0.3333333333333333148, 0.3333333333333333148, 0.3333333333333334814, 0.3333333333333332593, 0.3333333333333334259, 0.3333333333333333703, 0.3333333333333334814, 0.3333333333333334259, 0.3333333333333333148, 0.3333333333333333703, 0.3333333333333333703, 0.3333333333333335369, 0.3333333333333333148, 0.3333333333333334259, 0.3333333333333333703, 0.3333333333333333148, 0.3333333333333334259, 0.3333333333333334259, 0.3333333333333333703, 0.3333333333333333703, 0.3333333333333334259, 0.3333333333333334259, 0.3333333333333333703, 0.3333333333333333148, 0.3333333333333334259, 0.3333333333333333703, 0.3333333333333334814, 0.3333333333333333703, 0.3333333333333333703, 0.3333333333333333703, 0.3333333333333334259, 0.3333333333333333148, 0.3333333333333333703, 0.3333333333333334259, 0.3333333333333334259, 0.3333333333333333148, 0.3333333333333333703, 0.3333333333333333148, 0.3333333333333333703, 0.3333333333333335369, 0.3333333333333333148, 0.3333333333333334259, 0.3333333333333333703, 0.3333333333333334259, 0.3333333333333333148, 0.3333333333333333148, 0.3333333333333335369, 0.3333333333333333703, 0.3333333333333333148, 0.3333333333333333703, 0.3333333333333333703),
 ( 1.000000000000000000, 1.000000000000000000, 1.000000000000000000, 1.000000000000000222, 0.9999999999999997780, 1.000000000000000444, 0.9999999999999997780, 1.000000000000000222, 0.9999999999999996669, 1.000000000000000000, 1.000000000000000000, 1.000000000000000222, 1.000000000000000000, 1.000000000000000000, 0.9999999999999997780, 1.000000000000000000, 1.000000000000000000, 1.000000000000000000, 0.9999999999999997780, 1.000000000000000444, 0.9999999999999997780, 1.000000000000000222, 1.000000000000000000, 0.9999999999999997780, 1.000000000000000000, 1.000000000000000222, 0.9999999999999997780, 1.000000000000000222, 0.9999999999999997780, 1.000000000000000222, 1.000000000000000000, 0.9999999999999997780, 1.000000000000000444, 0.9999999999999997780, 1.000000000000000222, 0.9999999999999997780, 1.000000000000000444, 1.000000000000000000, 1.000000000000000000, 1.000000000000000000, 1.000000000000000000, 1.000000000000000000, 1.000000000000000000, 0.9999999999999997780, 1.000000000000000222, 0.9999999999999996669, 1.000000000000000444, 0.9999999999999994449, 1.000000000000000222, 1.000000000000000000, 1.000000000000000000, 1.000000000000000000, 1.000000000000000000, 1.000000000000000000, 0.9999999999999996669, 1.000000000000000444, 0.9999999999999997780, 1.000000000000000222, 0.9999999999999996669, 1.000000000000000000, 1.000000000000000000, 1.000000000000000222, 0.9999999999999997780, 1.000000000000000000, 1.000000000000000222, 0.9999999999999997780, 1.000000000000000000, 0.9999999999999997780, 1.000000000000000222, 0.9999999999999997780, 1.000000000000000444, 0.9999999999999994449, 1.000000000000000444, 0.9999999999999997780, 0.9999999999999997780, 1.000000000000000444, 0.9999999999999996669, 1.000000000000000000, 1.000000000000000000, 1.000000000000000000, 1.000000000000000000, 1.000000000000000222, 1.000000000000000000, 1.000000000000000000, 0.9999999999999996669, 1.000000000000000222, 1.000000000000000000, 0.9999999999999997780, 0.9999999999999997780, 0.9999999999999997780, 1.000000000000000000, 1.000000000000000222, 0.9999999999999997780, 1.000000000000000222, 0.9999999999999996669, 1.000000000000000444, 0.9999999999999997780, 1.000000000000000222, 1.000000000000000222, 0.9999999999999997780, 1.000000000000000222, 1.000000000000000000, 0.9999999999999997780, 1.000000000000000444, 1.000000000000000000, 1.000000000000000000, 1.000000000000000222, 1.000000000000000000, 1.000000000000000000, 1.000000000000000222, 0.9999999999999993339, 1.000000000000000444, 1.000000000000000222, 0.9999999999999997780, 1.000000000000000000, 1.000000000000000222, 1.000000000000000444, 1.000000000000000000, 1.000000000000000222, 0.9999999999999997780, 1.000000000000000222, 0.9999999999999997780, 1.000000000000000222, 1.000000000000000000, 0.9999999999999997780, 0.9999999999999996669, 1.000000000000000444, 0.9999999999999997780, 1.000000000000000444, 0.9999999999999997780, 1.000000000000000222, 1.000000000000000222, 1.000000000000000000, 0.9999999999999997780, 1.000000000000000222, 0.9999999999999997780, 1.000000000000000000, 1.000000000000000000, 1.000000000000000000, 0.9999999999999997780, 1.000000000000000222, 1.000000000000000000, 1.000000000000000000, 1.000000000000000000, 1.000000000000000222, 1.000000000000000222, 0.9999999999999994449, 1.000000000000000222, 1.000000000000000000, 0.9999999999999994449, 1.000000000000000444, 0.9999999999999997780, 1.000000000000000222, 0.9999999999999996669, 1.000000000000000444, 1.000000000000000000, 0.9999999999999996669, 1.000000000000000444, 0.9999999999999997780, 1.000000000000000000, 1.000000000000000444, 1.000000000000000000, 1.000000000000000222, 0.9999999999999996669, 1.000000000000000000, 0.9999999999999997780, 0.9999999999999997780, 1.000000000000000222, 1.000000000000000000, 1.000000000000000444, 0.9999999999999996669, 1.000000000000000222, 0.9999999999999997780, 0.9999999999999997780, 1.000000000000000444, 0.9999999999999997780, 1.000000000000000444, 0.9999999999999996669, 1.000000000000000222, 0.9999999999999996669, 1.000000000000000222, 0.9999999999999997780, 1.000000000000000444, 1.000000000000000222, 0.9999999999999996669, 1.000000000000000444, 0.9999999999999996669, 1.000000000000000000, 0.9999999999999997780, 1.000000000000000000, 1.000000000000000000, 1.000000000000000222, 0.9999999999999994449, 1.000000000000000444, 0.9999999999999993339, 1.000000000000000666, 0.9999999999999994449, 1.000000000000000222, 1.000000000000000222, 1.000000000000000000, 1.000000000000000000, 0.9999999999999997780, 1.000000000000000222, 0.9999999999999996669, 1.000000000000000222, 0.9999999999999996669, 1.000000000000000222, 1.000000000000000000, 1.000000000000000222, 0.9999999999999997780, 1.000000000000000222, 1.000000000000000222, 1.000000000000000000, 0.9999999999999997780, 1.000000000000000222, 1.000000000000000222, 1.000000000000000000, 1.000000000000000000, 1.000000000000000222, 0.9999999999999997780, 1.000000000000000000, 1.000000000000000222, 0.9999999999999996669, 0.9999999999999997780, 1.000000000000000222, 0.9999999999999997780, 1.000000000000000000, 0.9999999999999997780, 0.9999999999999997780, 1.000000000000000222, 1.000000000000000000, 1.000000000000000000, 1.000000000000000222, 0.9999999999999996669, 1.000000000000000444, 1.000000000000000000, 1.000000000000000222, 0.9999999999999997780, 1.000000000000000222, 0.9999999999999997780, 1.000000000000000444, 0.9999999999999997780, 1.000000000000000222, 0.9999999999999997780, 1.000000000000000222, 0.9999999999999997780, 1.000000000000000222, 1.000000000000000000, 1.000000000000000222, 1.000000000000000000, 1.000000000000000000, 1.000000000000000222, 1.000000000000000000, 1.000000000000000000, 0.9999999999999997780, 1.000000000000000000, 1.000000000000000444, 0.9999999999999996669, 1.000000000000000222, 0.9999999999999997780, 1.000000000000000000, 0.9999999999999997780, 1.000000000000000222, 1.000000000000000222, 1.000000000000000000, 1.000000000000000000, 0.9999999999999996669, 1.000000000000000444, 0.9999999999999997780, 1.000000000000000000, 1.000000000000000222, 0.9999999999999996669, 1.000000000000000444, 1.000000000000000000, 0.9999999999999997780, 1.000000000000000222, 0.9999999999999997780, 1.000000000000000000, 1.000000000000000000, 1.000000000000000000, 1.000000000000000000, 1.000000000000000000, 1.000000000000000222, 1.000000000000000444, 0.9999999999999997780, 1.000000000000000222, 1.000000000000000000, 1.000000000000000444, 0.9999999999999997780, 1.000000000000000222, 0.9999999999999997780, 1.000000000000000222, 0.9999999999999997780, 1.000000000000000222, 1.000000000000000000, 1.000000000000000222, 1.000000000000000222, 1.000000000000000222, 0.9999999999999997780, 1.000000000000000222, 0.9999999999999997780, 1.000000000000000222, 0.9999999999999997780, 1.000000000000000444, 0.9999999999999996669, 1.000000000000000444, 1.000000000000000000, 1.000000000000000000, 0.9999999999999997780, 1.000000000000000222, 1.000000000000000000, 0.9999999999999997780, 1.000000000000000000, 0.9999999999999997780, 1.000000000000000222, 1.000000000000000000, 1.000000000000000000, 1.000000000000000222, 0.9999999999999997780, 1.000000000000000444, 0.9999999999999996669, 1.000000000000000222, 1.000000000000000222, 0.9999999999999997780, 1.000000000000000000, 0.9999999999999997780, 1.000000000000000000, 0.9999999999999996669, 1.000000000000000444, 0.9999999999999997780, 1.000000000000000222, 1.000000000000000000, 1.000000000000000000, 1.000000000000000000, 0.9999999999999997780, 0.9999999999999997780, 1.000000000000000000, 0.9999999999999997780, 1.000000000000000444, 0.9999999999999996669, 1.000000000000000222, 1.000000000000000000, 1.000000000000000444, 1.000000000000000222, 1.000000000000000000, 0.9999999999999997780, 1.000000000000000222, 1.000000000000000444, 0.9999999999999997780, 1.000000000000000222, 0.9999999999999997780, 1.000000000000000000, 1.000000000000000000, 1.000000000000000222, 0.9999999999999997780, 1.000000000000000222, 1.000000000000000000, 1.000000000000000222, 0.9999999999999997780, 1.000000000000000000, 1.000000000000000222, 1.000000000000000000, 1.000000000000000222, 1.000000000000000000, 1.000000000000000000, 0.9999999999999997780, 1.000000000000000444, 0.9999999999999997780, 1.000000000000000000, 1.000000000000000000, 1.000000000000000444, 0.9999999999999996669, 1.000000000000000222, 1.000000000000000000, 0.9999999999999996669, 1.000000000000000444, 0.9999999999999996669, 1.000000000000000444, 0.9999999999999997780, 1.000000000000000222, 0.9999999999999997780, 1.000000000000000222, 1.000000000000000222, 1.000000000000000222, 1.000000000000000000, 1.000000000000000000, 1.000000000000000000) ) ) 
 REPRESENTATION_ITEM ( '' )  SURFACE ( )  );
#163051 = CARTESIAN_POINT ( 'NONE',  ( 4.297571505407542958, 7.957657823043374989, -0.7216878364870197293 ) ) ;
#163052 = CARTESIAN_POINT ( 'NONE',  ( -1.364683531250014514, -0.1572916663252435232, 0.7879004041258379498 ) ) ;
#163053 = CARTESIAN_POINT ( 'NONE',  ( 5.939505971022265740, 6.126191976022287378, 0.7574911370455077453 ) ) ;
#163054 = CARTESIAN_POINT ( 'NONE',  ( -9.833741488613570780, 10.36711991300432345, 0.7998128361456462443 ) ) ;
#163055 = CARTESIAN_POINT ( 'NONE',  ( 5.559502693676295237, 0.4258712887980077300, -2.119171757835013548 ) ) ;
#163056 = CARTESIAN_POINT ( 'NONE',  ( -5.234856708652269042, 7.200695141551334721, 1.443375672974058777 ) ) ;
#163057 = CARTESIAN_POINT ( 'NONE',  ( 4.095971805104276164, 7.792734516014745871, 0.7216878364870257245 ) ) ;
#163058 = CARTESIAN_POINT ( 'NONE',  ( 1.810938747355747447, -0.5704394276861005642, -2.042344090522000055 ) ) ;
#163060 = CARTESIAN_POINT ( 'NONE',  ( -11.82196040793749425, 4.889518425415825931, 4.884593937341564107 ) ) ;
#163059 = LINE ( 'NONE', #76453, #210900 ) ;
#163061 = CARTESIAN_POINT ( 'NONE',  ( 3.673081450605990117, 0.05180205286909286139, -1.970847691630872811 ) ) ;
#163062 =( BOUNDED_SURFACE ( )  B_SPLINE_SURFACE ( 3, 2, ( 
 ( #162720, #124160, #130287 ),
 ( #195209, #147533, #14292 ),
 ( #47922, #146483, #107889 ),
 ( #31649, #25491, #191178 ) ),
 .UNSPECIFIED., .F., .F., .F. ) 
 B_SPLINE_SURFACE_WITH_KNOTS ( ( 4, 4 ),
 ( 3, 3 ),
 ( 0.000000000000000000, 3.124373657233978183E-05 ),
 ( 0.000000000000000000, 1.000000000000000000 ),
 .UNSPECIFIED. ) 
 GEOMETRIC_REPRESENTATION_ITEM ( )  RATIONAL_B_SPLINE_SURFACE ( (
 ( 1.000000000000000000, 0.7045118851641303248, 1.000000000000000000),
 ( 1.000000000000000000, 0.7044892147945189809, 1.000000000000000000),
 ( 1.000000000000000000, 0.7053501046726613488, 1.000000000000000000),
 ( 1.000000000000000000, 0.7071067811869121700, 1.000000000000000000) ) ) 
 REPRESENTATION_ITEM ( '' )  SURFACE ( )  );
#163063 = CARTESIAN_POINT ( 'NONE',  ( 5.625241921295836889, 1.689600096388569561, 0.8957793909229803120 ) ) ;
#163064 = ORIENTED_EDGE ( 'NONE', *, *, #186745, .F. ) ;
#163065 = CARTESIAN_POINT ( 'NONE',  ( 0.1509401653462701109, -0.4529219869476922011, -2.027634260368789576 ) ) ;
#163066 = CARTESIAN_POINT ( 'NONE',  ( 1.675622358955121571, -1.039060084690484942, 1.640409814757173734 ) ) ;
#163067 = VERTEX_POINT ( 'NONE', #161799 ) ;
#163068 = CARTESIAN_POINT ( 'NONE',  ( -4.496464221587651799, 5.274905009054215554, 1.199719254218452935 ) ) ;
#163070 = CARTESIAN_POINT ( 'NONE',  ( 5.826972158823246595, 10.02016096192762085, -0.7998128361456481317 ) ) ;
#163069 = CARTESIAN_POINT ( 'NONE',  ( -6.129694847154220305, 8.244672969803623630, -1.443375672974066548 ) ) ;
#163072 = CARTESIAN_POINT ( 'NONE',  ( 5.445571254183207088, 9.504916896522420444, -0.7998128361456281477 ) ) ;
#163071 = CARTESIAN_POINT ( 'NONE',  ( 2.361375956566538648, 2.050102581710811389, -0.4087646360023765024 ) ) ;
#163073 = CARTESIAN_POINT ( 'NONE',  ( 4.380693030546913391, 7.164540064729805202, 1.082531754730549078 ) ) ;
#163075 = ORIENTED_EDGE ( 'NONE', *, *, #181317, .F. ) ;
#163074 = CARTESIAN_POINT ( 'NONE',  ( 6.533860241792342372, -1.853627334332415888, 0.4695604596292660138 ) ) ;
#163076 = CARTESIAN_POINT ( 'NONE',  ( 4.670673364294657404, -1.443042178620690841, 1.669811033208345341 ) ) ;
#163077 = CARTESIAN_POINT ( 'NONE',  ( 3.399657359236216703, 1.738403758043248759, 1.359216269546263511 ) ) ;
#163078 = CARTESIAN_POINT ( 'NONE',  ( 7.476431642932036326, 10.80992178580769014, 1.199719254218460707 ) ) ;
#163080 =( BOUNDED_CURVE ( )  B_SPLINE_CURVE ( 2, ( #112376, #113446, #50503, #46258, #166380, #13726, #164258, #63557, #66706 ),
 .UNSPECIFIED., .F., .T. ) 
 B_SPLINE_CURVE_WITH_KNOTS ( ( 3, 2, 2, 2, 3 ),
 ( 0.5625000000000000000, 0.5694444444444444198, 0.5833333333333333703, 0.5972222222222222099, 0.6041666666666667407 ),
 .UNSPECIFIED. ) 
 CURVE ( )  GEOMETRIC_REPRESENTATION_ITEM ( )  RATIONAL_B_SPLINE_CURVE ( ( 0.9330127018922194093, 0.9330127018922194093, 1.000000000000000000, 0.8660254037844387076, 1.000000000000000000, 0.8660254037844387076, 1.000000000000000000, 0.9330127018922187432, 0.9330127018922192983 ) ) 
 REPRESENTATION_ITEM ( '' )  );
#163079 = CARTESIAN_POINT ( 'NONE',  ( -11.91826849282518630, 12.69999999999997975, 1.399999999999996581 ) ) ;
#163081 = CARTESIAN_POINT ( 'NONE',  ( 1.734869227892420707, 1.784761669998648381, 0.6870963898520031643 ) ) ;
#163082 = CARTESIAN_POINT ( 'NONE',  ( 0.3459972005394982286, -9.006862989983986267, -9.494064636159277981 ) ) ;
#163083 = CARTESIAN_POINT ( 'NONE',  ( 9.243799147819517614, 13.41009114453062345, -7.924839666318222342 ) ) ;
#163084 = CARTESIAN_POINT ( 'NONE',  ( 4.334477209444559165, -1.194628513295314720, 1.690740121169509225 ) ) ;
#163086 = CARTESIAN_POINT ( 'NONE',  ( 1.323354039402934390, -0.05256100377049736927, 2.161234000603563299 ) ) ;
#163085 = CARTESIAN_POINT ( 'NONE',  ( -1.201851678989727383E-14, 3.837500000000022116, -1.732050807568863648 ) ) ;
#163087 = CARTESIAN_POINT ( 'NONE',  ( 3.808297599986898430, 1.548825491099754315, -1.550762550882843094 ) ) ;
#163088 = CARTESIAN_POINT ( 'NONE',  ( -0.02968770228140016343, 0.003472272166151618711, -1.826291111852257343 ) ) ;
#163089 = CARTESIAN_POINT ( 'NONE',  ( -3.535343422797964763, 15.44796817926509291, 11.42948407163687286 ) ) ;
#163090 = CARTESIAN_POINT ( 'NONE',  ( 6.059568310664962709, 6.034194215389424798, 0.7998128361456352531 ) ) ;
#163091 = CARTESIAN_POINT ( 'NONE',  ( 0.6823417656249934904, 13.75520833367473195, 1.181850606188764807 ) ) ;
#163092 = CARTESIAN_POINT ( 'NONE',  ( -5.191846479390389568, 5.021852078902356631, 0.7998128361456281477 ) ) ;
#163093 = CARTESIAN_POINT ( 'NONE',  ( 0.1412502902482688505, 0.7743183493036235321, 1.862015731718666078 ) ) ;
#163094 = VECTOR ( 'NONE', #201566, 1000.000000000000000 ) ;
#163095 = CARTESIAN_POINT ( 'NONE',  ( -8.175203439360366531, 12.48156174598837787, 1.040834085586084257E-14 ) ) ;
#163096 = CARTESIAN_POINT ( 'NONE',  ( 5.032118066406459533, 1.187563481491529460, 1.695602288408842417 ) ) ;
#163097 = CARTESIAN_POINT ( 'NONE',  ( 2.859893552614915180, 1.917175687707149967, -0.1893568897016733310 ) ) ;
#163098 = CARTESIAN_POINT ( 'NONE',  ( 6.239883422132978197, 2.111550094393780608, -0.1561052605421053563 ) ) ;
#163099 = CARTESIAN_POINT ( 'NONE',  ( 4.137209430464448445, 7.978494768850520558, 1.040834085586084257E-14 ) ) ;
#163100 = CARTESIAN_POINT ( 'NONE',  ( 9.651540038386141163, 3.878167290971874959, 7.130941910101068260 ) ) ;
#163101 = CARTESIAN_POINT ( 'NONE',  ( 3.959776185634265921, -0.5760637367184845425, 1.883274482577349973 ) ) ;
#163102 = CARTESIAN_POINT ( 'NONE',  ( 5.507889418014947580, -1.026508118683837401, -2.049657838918368391 ) ) ;
#163103 = CARTESIAN_POINT ( 'NONE',  ( 4.389149243953620605, 1.629682310347341456, -0.8231139397327084106 ) ) ;
#163104 = PRODUCT_DEFINITION_SHAPE ( 'NONE', 'NONE',  #214414 ) ;
#163105 = CARTESIAN_POINT ( 'NONE',  ( 5.885648082108188461, 8.920320958217979879, 1.082531754730549967 ) ) ;
#163106 = CARTESIAN_POINT ( 'NONE',  ( 4.161989969270892153, 6.839110149915929249, 1.082531754730558626 ) ) ;
#163107 = CARTESIAN_POINT ( 'NONE',  ( -4.932134020321308654, 8.976183133675331050, 0.7998128361456291469 ) ) ;
#163108 = CARTESIAN_POINT ( 'NONE',  ( 5.234329823327693809, 8.264412672927770487, 1.199719254218451159 ) ) ;
#163109 = EDGE_LOOP ( 'NONE', ( #40844, #187682, #46798, #165172 ) ) ;
#163110 = CARTESIAN_POINT ( 'NONE',  ( 4.816656863388896426, -0.6821788116995251006, -1.894207565886153910 ) ) ;
#163111 = CARTESIAN_POINT ( 'NONE',  ( 0.2108991129620274019, -1.778944881630979413, -1.454728436597878316 ) ) ;
#163112 = CARTESIAN_POINT ( 'NONE',  ( 5.506681978947471912, 0.5658967987182733639, 1.878394690154854496 ) ) ;
#163113 = CARTESIAN_POINT ( 'NONE',  ( -7.691553217654356622, 7.867900263551875994, -0.7998128361456291469 ) ) ;
#163114 = CARTESIAN_POINT ( 'NONE',  ( -5.935772324684618795, 5.819489221753827657, 0.000000000000000000 ) ) ;
#163115 = CARTESIAN_POINT ( 'NONE',  ( -15.75000000000000000, 12.30000000000000071, -3.200000000000001510 ) ) ;
#163116 = CARTESIAN_POINT ( 'NONE',  ( -6.947627372360122955, 7.070263120700404968, 0.000000000000000000 ) ) ;
#163118 = CARTESIAN_POINT ( 'NONE',  ( 0.2329894512427649333, -1.712236961970284632, 0.7538099095961707796 ) ) ;
#163117 = CARTESIAN_POINT ( 'NONE',  ( 1.558266987246118562, -1.476132899515494534, 1.480894285863892934 ) ) ;
#163119 = DIRECTION ( 'NONE',  ( 0.000000000000000000, 0.000000000000000000, -1.000000000000000000 ) ) ;
#163120 = CARTESIAN_POINT ( 'NONE',  ( 5.701106494887172360, -0.4696333794993942101, 1.884192904834626869 ) ) ;
#163121 = LINE ( 'NONE', #92801, #18689 ) ;
#163122 = CARTESIAN_POINT ( 'NONE',  ( 1.364397727108757730, 0.1285707514647760064, -1.735724436397204196 ) ) ;
#163123 = CARTESIAN_POINT ( 'NONE',  ( 6.986529229743720926, 7.045372277656132276, -0.7998128361456281477 ) ) ;
#163124 = CARTESIAN_POINT ( 'NONE',  ( 6.875078400183575411, 7.629137130509070275, 2.455651831298297338 ) ) ;
#163125 = CARTESIAN_POINT ( 'NONE',  ( 1.752176261082264208, 0.5389683859425442591, 1.638572262730133566 ) ) ;
#163126 = CARTESIAN_POINT ( 'NONE',  ( 2.120887600855193345, 0.003649250790785373531, 2.191739723551556551 ) ) ;
#163127 = CARTESIAN_POINT ( 'NONE',  ( 3.862124860921032354, 2.190326239153097543, -0.2693113811002012525 ) ) ;
#163128 =( BOUNDED_SURFACE ( )  B_SPLINE_SURFACE ( 3, 2, ( 
 ( #50147, #52279, #2422 ),
 ( #167104, #17612, #34940 ),
 ( #3491, #135671, #133565 ),
 ( #68499, #199571, #18691 ),
 ( #83698, #116271, #103160 ),
 ( #69561, #134627, #16550 ),
 ( #149786, #82632, #53339 ),
 ( #70625, #117339, #148717 ) ),
 .UNSPECIFIED., .F., .F., .T. ) 
 B_SPLINE_SURFACE_WITH_KNOTS ( ( 4, 2, 2, 4 ),
 ( 3, 3 ),
 ( 0.000000000000000000, 0.003135730046001663184, 0.004703595069002494342, 0.006271460092003326367 ),
 ( 0.000000000000000000, 1.000000000000000000 ),
 .UNSPECIFIED. ) 
 GEOMETRIC_REPRESENTATION_ITEM ( )  RATIONAL_B_SPLINE_SURFACE ( (
 ( 1.000000000000000000, 0.7762074382822432561, 1.000000000000000000),
 ( 1.000000000000000000, 0.7833603871961897225, 1.000000000000000000),
 ( 1.000000000000000000, 0.7921476697827543045, 1.000000000000000000),
 ( 1.000000000000000000, 0.8128220030704583765, 1.000000000000000000),
 ( 1.000000000000000000, 0.8210052159719404274, 1.000000000000000000),
 ( 1.000000000000000000, 0.8412342355964647078, 1.000000000000000000),
 ( 1.000000000000000000, 0.8534349975674863087, 1.000000000000000000),
 ( 1.000000000000000000, 0.8671614222306937014, 1.000000000000000000) ) ) 
 REPRESENTATION_ITEM ( '' )  SURFACE ( )  );
#163129 = CARTESIAN_POINT ( 'NONE',  ( 1.358521007292138538, -2.171239805896512554, -0.002410242577662382712 ) ) ;
#163130 = CARTESIAN_POINT ( 'NONE',  ( 0.4865809202317071813, -0.2202831055867389420, -1.812292406919484344 ) ) ;
#163131 = CARTESIAN_POINT ( 'NONE',  ( 2.009133639091817525, 0.005444305534021975056, 2.117513411327852868 ) ) ;
#163132 = CARTESIAN_POINT ( 'NONE',  ( 6.639320575229276322, 3.701785489019034259, 2.411212692025939131 ) ) ;
#163133 = EDGE_LOOP ( 'NONE', ( #25218, #64218, #95956, #200765, #182331, #204832, #165084 ) ) ;
#163135 = CARTESIAN_POINT ( 'NONE',  ( -1.364683531250000748, 0.07187500034142035865, 0.000000000000000000 ) ) ;
#163134 = CARTESIAN_POINT ( 'NONE',  ( 2.331904285594294191, 1.077338530963572127, -2.023425408739158105 ) ) ;
#163136 = DIRECTION ( 'NONE',  ( 1.000000000000000000, 0.000000000000000000, -0.000000000000000000 ) ) ;
#163137 = CARTESIAN_POINT ( 'NONE',  ( 4.976006071415387311, 5.764094157194782575, 1.199719254218462483 ) ) ;
#163138 = CIRCLE ( 'NONE', #170066, 0.5000000000000005551 ) ;
#163139 = CARTESIAN_POINT ( 'NONE',  ( 5.180443790456886077, 1.093758630767979412, 1.933306047416243567 ) ) ;
#163140 = CARTESIAN_POINT ( 'NONE',  ( -7.863365906246074566, 8.276274433482971205, -0.7216878364870278340 ) ) ;
#163141 = CARTESIAN_POINT ( 'NONE',  ( 4.175548123328908900, 7.815297210618305179, -0.7216878364870197293 ) ) ;
#163142 = CARTESIAN_POINT ( 'NONE',  ( -5.843201017365469596, 9.760892253660966134, 0.7216878364870458196 ) ) ;
#163143 = CARTESIAN_POINT ( 'NONE',  ( 5.560252395380222090, 5.659585014131299552, 0.7216878364870328300 ) ) ;
#163144 = EDGE_LOOP ( 'NONE', ( #166734, #122342, #169045, #87109 ) ) ;
#163145 = CARTESIAN_POINT ( 'NONE',  ( 2.443982611291168450, -1.755769474653746665, -0.9913988478210812305 ) ) ;
#163147 = CARTESIAN_POINT ( 'NONE',  ( 1.868110439076278384, -2.047461887716729656, 0.2484499435305431159 ) ) ;
#163146 = CARTESIAN_POINT ( 'NONE',  ( 6.262976894508937242, 9.394224579314053969, -1.199719254218440723 ) ) ;
#163148 = DIRECTION ( 'NONE',  ( 0.7408284471490506062, -1.804614770759932615E-12, -0.6716942845482062330 ) ) ;
#163149 = CARTESIAN_POINT ( 'NONE',  ( 5.411112705185558092, 6.445957923205511086, -1.082531754730548412 ) ) ;
#163150 = ORIENTED_EDGE ( 'NONE', *, *, #149244, .T. ) ;
#163151 = CARTESIAN_POINT ( 'NONE',  ( -3.633221978782310124, 7.182583375313863705, -0.7216878364870463747 ) ) ;
#163152 = CARTESIAN_POINT ( 'NONE',  ( -0.6823417656250212460, 5.051041667008086655, 1.181850606188767472 ) ) ;
#163153 = CARTESIAN_POINT ( 'NONE',  ( 4.593798273609356997, -2.190911875110569174, -0.05534364095756416635 ) ) ;
#163154 = CARTESIAN_POINT ( 'NONE',  ( 2.690077459517980163, 1.704938782060089864, 1.076316768488336351 ) ) ;
#163155 = CARTESIAN_POINT ( 'NONE',  ( 0.6613494997313728030, 0.9071737413179328247, 1.602200521169500957 ) ) ;
#163156 = CARTESIAN_POINT ( 'NONE',  ( 7.796102023057898123, 9.054206100777749455, -1.199719254218441611 ) ) ;
#163157 = CARTESIAN_POINT ( 'NONE',  ( 5.122008332510333162, -0.9777984688263160473, -1.541441239866998103 ) ) ;
#163158 = CARTESIAN_POINT ( 'NONE',  ( 6.363907750917786821, -0.1017471579566435469, -2.013986097687201049 ) ) ;
#163159 = CARTESIAN_POINT ( 'NONE',  ( -8.199983978166823562, 8.461069484149769337, -0.7998128361456291469 ) ) ;
#163161 = CARTESIAN_POINT ( 'NONE',  ( -6.469175572376043348, 7.576401584974034265, 1.199719254218452047 ) ) ;
#163160 = CARTESIAN_POINT ( 'NONE',  ( 6.192268726830573833, -2.250890937568471362, -0.2291988078206678991 ) ) ;
#163162 = CARTESIAN_POINT ( 'NONE',  ( 0.9265589629697315033, 1.253077620556674932, -1.692570004448453957 ) ) ;
#163163 = CARTESIAN_POINT ( 'NONE',  ( -7.370792787684826486, 8.628288336167626582, -1.199719254218452047 ) ) ;
#163164 = CARTESIAN_POINT ( 'NONE',  ( 4.246580143467587831, -2.047389768388275577, -0.3068500204662719666 ) ) ;
#163165 = CARTESIAN_POINT ( 'NONE',  ( 8.204655514564224816, 12.72384853363364066, 1.040834085586084257E-14 ) ) ;
#163166 = SURFACE_STYLE_FILL_AREA ( #113412 ) ;
#163167 = DIRECTION ( 'NONE',  ( 4.643935581739670507E-17, -1.000000000000000000, 5.596873555263448697E-16 ) ) ;
#163169 = ADVANCED_FACE ( 'NONE', ( #179111 ), #65989, .T. ) ;
#163168 = CARTESIAN_POINT ( 'NONE',  ( -7.506410603460441422, 11.90922947067921278, -0.7998128361456291469 ) ) ;
#163170 = CARTESIAN_POINT ( 'NONE',  ( -0.1263102688159843667, 6.363441598446241798, 3.117922131261609664 ) ) ;
#163171 = CARTESIAN_POINT ( 'NONE',  ( 3.567203813726958828, 6.215469311773181182, 1.082531754730549078 ) ) ;
#163172 = CARTESIAN_POINT ( 'NONE',  ( 4.762865522572231392, 6.775349848016087861, -1.243673390893657471 ) ) ;
#163173 = CARTESIAN_POINT ( 'NONE',  ( -10.14113571334194930, 10.93367254176152059, -0.7216878364870267237 ) ) ;
#163175 = CARTESIAN_POINT ( 'NONE',  ( 2.619623270456972630, 1.879045213996872965, 1.184562869268386054 ) ) ;
#163174 = CARTESIAN_POINT ( 'NONE',  ( 1.529697670087664108, -0.2543295609688834835, 2.105205558366497698 ) ) ;
#163176 = CARTESIAN_POINT ( 'NONE',  ( 3.224997775515605181, 6.424863269013458833, -0.8838344238559818766 ) ) ;
#163177 = CARTESIAN_POINT ( 'NONE',  ( -7.110325215724114578, 7.260077271291732082, 0.000000000000000000 ) ) ;
#163178 = CARTESIAN_POINT ( 'NONE',  ( 6.205881626753210867, 8.263281202677319470, 1.599625672291281386 ) ) ;
#163179 = CARTESIAN_POINT ( 'NONE',  ( 3.314850587115983238, -1.487306837207631238, 1.279512770686676681 ) ) ;
#163180 = CARTESIAN_POINT ( 'NONE',  ( 6.173040012923759257, 6.096301524699504704, -0.7998128361456281477 ) ) ;
#163181 = CARTESIAN_POINT ( 'NONE',  ( -4.191772670604852813, 7.388608026231708870, 0.8008250379338277547 ) ) ;
#163182 = CARTESIAN_POINT ( 'NONE',  ( 4.196412238629597447, 4.854568018944682706, -1.199719254218452047 ) ) ;
#163183 = CARTESIAN_POINT ( 'NONE',  ( -4.150204419558982671, 7.856005899545188242, 0.7216878364870338292 ) ) ;
#163184 = CARTESIAN_POINT ( 'NONE',  ( -6.561783159334130922, 9.638868871656395498, -1.082531754730538864 ) ) ;
#163185 =( GEOMETRIC_REPRESENTATION_CONTEXT ( 3 ) GLOBAL_UNCERTAINTY_ASSIGNED_CONTEXT ( ( #78181 ) ) GLOBAL_UNIT_ASSIGNED_CONTEXT ( ( #23589, #53975, #171997 ) ) REPRESENTATION_CONTEXT ( 'NONE', 'WORKASPACE' ) );
#163186 = CARTESIAN_POINT ( 'NONE',  ( 1.863691559860299884, -1.706161385809309650, -1.259181899442491037 ) ) ;
#163187 = CARTESIAN_POINT ( 'NONE',  ( -6.448838341955544173, 7.552674816150118708, 1.199719254218452047 ) ) ;
#163188 = CARTESIAN_POINT ( 'NONE',  ( 4.944278945467968533, 2.155654431248493985, 0.1625706239713892443 ) ) ;
#163189 = CARTESIAN_POINT ( 'NONE',  ( 3.245484093776138668, 1.841430844176932480, -0.003062914905635482320 ) ) ;
#163190 = AXIS2_PLACEMENT_3D ( 'NONE', #24009, #74915, #190776 ) ;
#163191 = CARTESIAN_POINT ( 'NONE',  ( -4.167566996647928512, 7.418725663478599408, 0.7529690952402002813 ) ) ;
#163192 = CARTESIAN_POINT ( 'NONE',  ( 1.364683531249988757, -0.3031249996585799744, 0.000000000000000000 ) ) ;
#163193 = CARTESIAN_POINT ( 'NONE',  ( 5.490116972639333071, -0.4286210177542044697, -1.686591927243533240 ) ) ;
#163194 = CARTESIAN_POINT ( 'NONE',  ( 6.727182134110196721, 2.084960209934753284, 2.120171393779949565 ) ) ;
#163195 = CARTESIAN_POINT ( 'NONE',  ( 4.609409038966229666, 6.400729850259146758, -1.443375672974051449 ) ) ;
#163196 = CARTESIAN_POINT ( 'NONE',  ( -1.499999999999972689, 3.660416667349487341, -0.8660254037844548058 ) ) ;
#163197 = CARTESIAN_POINT ( 'NONE',  ( 3.555696680978126079, 0.5271953485486252644, -2.096301903996622862 ) ) ;
#163198 = CARTESIAN_POINT ( 'NONE',  ( 4.024767406304472495, 2.001204788683898617, -0.2439926020210633206 ) ) ;
#163199 = CARTESIAN_POINT ( 'NONE',  ( -7.483737604619046913, 11.67485160545682987, 0.000000000000000000 ) ) ;
#163200 = CARTESIAN_POINT ( 'NONE',  ( 1.973706723050288936, 2.068691090354588091, -0.6273066937243013674 ) ) ;
#163201 = ADVANCED_FACE ( 'NONE', ( #29663 ), #204220, .T. ) ;
#163202 = CARTESIAN_POINT ( 'NONE',  ( 2.741432468550320412, -1.458365196291089072, -1.326584384502631719 ) ) ;
#163203 = CARTESIAN_POINT ( 'NONE',  ( -6.615342224808818727, 6.750480251133849308, 0.3470571717737805373 ) ) ;
#163204 = CARTESIAN_POINT ( 'NONE',  ( 4.124509801231989847, 0.09871269697571230517, 1.939684287242355420 ) ) ;
#163207 = ORIENTED_EDGE ( 'NONE', *, *, #97858, .T. ) ;
#163206 = CARTESIAN_POINT ( 'NONE',  ( 0.000000000000000000, 11.37999999999999901, 0.000000000000000000 ) ) ;
#163205 = CARTESIAN_POINT ( 'NONE',  ( -8.310784975052671442, 11.67937098999472667, -1.082531754730543083 ) ) ;
#163208 = B_SPLINE_CURVE_WITH_KNOTS ( 'NONE', 3,
 ( #168991, #35786, #117106, #135442, #186295, #153819, #201463, #136511, #86676, #21635 ),
 .UNSPECIFIED., .F., .F.,
 ( 4, 2, 2, 2, 4 ),
 ( 0.000000000000000000, 0.0002554020510936944391, 0.0005108041021873888782, 0.0007662061532810833173, 0.001021608204374777756 ),
 .UNSPECIFIED. ) ;
#163209 = CARTESIAN_POINT ( 'NONE',  ( -7.957709816578236506, 8.248692638954882028, 0.7998128361456341429 ) ) ;
#163210 = CARTESIAN_POINT ( 'NONE',  ( 4.706615602599436343, 5.520081620234675412, 1.199719254218452935 ) ) ;
#163212 = ORIENTED_EDGE ( 'NONE', *, *, #114761, .F. ) ;
#163211 = CARTESIAN_POINT ( 'NONE',  ( -5.818384198920079520, 6.817144982608731141, 1.199719254218452935 ) ) ;
#163213 = CARTESIAN_POINT ( 'NONE',  ( -6.995644074527074707, 11.10540915368285475, 0.000000000000000000 ) ) ;
#163214 = CARTESIAN_POINT ( 'NONE',  ( 1.536444635327537833, 1.086998388645914027, -1.920427013416255768 ) ) ;
#163215 = CARTESIAN_POINT ( 'NONE',  ( 0.000000000000000000, -2.296874999522042327, -3.793834371823813001 ) ) ;
#163216 = CARTESIAN_POINT ( 'NONE',  ( 5.401206054008879320, -1.684469800357458302, 1.005230755432365175 ) ) ;
#163217 = CARTESIAN_POINT ( 'NONE',  ( -1.364683531249997417, 4.821875000341417916, 1.214306433183764966E-14 ) ) ;
#163218 = CARTESIAN_POINT ( 'NONE',  ( 1.499999999999987121, 2.827083334016148530, -0.8660254037844262731 ) ) ;
#163219 = CARTESIAN_POINT ( 'NONE',  ( 5.980536202102920917, 6.100347882654393317, -0.6550157475838751520 ) ) ;
#163220 = DIRECTION ( 'NONE',  ( 0.7592566023653005702, 0.6507913734559639396, 0.000000000000000000 ) ) ;
#163221 = CARTESIAN_POINT ( 'NONE',  ( 4.611176429654996412, -1.805050139478355353, 0.3618648703537508671 ) ) ;
#163222 = ORIENTED_EDGE ( 'NONE', *, *, #193237, .T. ) ;
#163223 = CARTESIAN_POINT ( 'NONE',  ( 1.360316468749977581, -0.2135416663252950598, -0.7853790794159261068 ) ) ;
#163224 = CARTESIAN_POINT ( 'NONE',  ( -6.645467848992654858, 10.90479625713344625, 0.7998128361456481317 ) ) ;
#163225 = CARTESIAN_POINT ( 'NONE',  ( -4.613268803136618246, 8.378775596900176481, 0.2107346534404584415 ) ) ;
#163226 = CARTESIAN_POINT ( 'NONE',  ( 5.344028447597857223, -1.346983732444573256, -1.637812552581649594 ) ) ;
#163227 = CARTESIAN_POINT ( 'NONE',  ( -1.499999999999997780, 4.431250000682819490, 1.214306433183765124E-14 ) ) ;
#163228 = CARTESIAN_POINT ( 'NONE',  ( 4.852928918687680948, 7.749168607522574526, 1.199719254218462483 ) ) ;
#163229 = CARTESIAN_POINT ( 'NONE',  ( 6.872340646960426902, -1.271554428311357565, 1.622191329735128029 ) ) ;
#163232 = CARTESIAN_POINT ( 'NONE',  ( 4.142028884782995135, 0.4951553702221401232, 1.773339192993342639 ) ) ;
#163231 = CARTESIAN_POINT ( 'NONE',  ( 0.6603357414211168397, -0.6217855776655777378, -1.754263843975149006 ) ) ;
#163230 = CARTESIAN_POINT ( 'NONE',  ( 10.51582573219069694, 12.48709141521726984, 3.554376768052132540 ) ) ;
#163233 = CARTESIAN_POINT ( 'NONE',  ( 6.760712154708803823, 11.03924794713562818, 1.040834085586084257E-14 ) ) ;
#163234 = CARTESIAN_POINT ( 'NONE',  ( -0.08053691275167716712, 15.51846456562902965, 11.99972973886013961 ) ) ;
#163235 = CARTESIAN_POINT ( 'NONE',  ( -7.293360289508603600, 7.473618190706972086, 0.000000000000000000 ) ) ;
#163236 = CARTESIAN_POINT ( 'NONE',  ( 9.333041836208478159, 3.553060279300227275, -7.472413793088525935 ) ) ;
#163237 = CARTESIAN_POINT ( 'NONE',  ( 3.229339687698820072, 0.05429069646168545316, 2.206380697113208722 ) ) ;
#163238 = CARTESIAN_POINT ( 'NONE',  ( 6.503223684228603751, 1.875565888388399660, 1.264963274899598256 ) ) ;
#163239 = CARTESIAN_POINT ( 'NONE',  ( -5.910991785878165317, 8.879612269291090598, -1.082531754730538864 ) ) ;
#163240 = CARTESIAN_POINT ( 'NONE',  ( 6.134996530155978789, 1.693739186514784167, 0.6432786700914516764 ) ) ;
#163241 = CARTESIAN_POINT ( 'NONE',  ( 5.893738820153655134, -1.900388249151972353, 0.2415585323580979049 ) ) ;
#163242 = CARTESIAN_POINT ( 'NONE',  ( 0.6823417656249917140, 5.405208333674749177, 1.181850606188765695 ) ) ;
#163243 = CARTESIAN_POINT ( 'NONE',  ( 5.840666405660361882, 0.3664468388623157158, 1.834233659845653897 ) ) ;
#163244 = CARTESIAN_POINT ( 'NONE',  ( 6.496546432963370421, 1.840999872533972903, 0.2716635292502044829 ) ) ;
#163245 = LINE ( 'NONE', #14828, #133598 ) ;
#163246 = MECHANICAL_DESIGN_GEOMETRIC_PRESENTATION_REPRESENTATION (  '', ( #114901 ), #529 ) ;
#163247 = CARTESIAN_POINT ( 'NONE',  ( 0.1450994221751950586, -1.442925249786636943, -1.190247126510869613 ) ) ;
#163248 = CARTESIAN_POINT ( 'NONE',  ( 1.376185782568883020, -2.007256511855738612, -0.1928315418098166534 ) ) ;
#163250 = CARTESIAN_POINT ( 'NONE',  ( 2.420660912963272349, 1.375124471020009231, -1.595256772795665023 ) ) ;
#163249 = CARTESIAN_POINT ( 'NONE',  ( -7.818248136574758256, 12.27303992597924420, 0.000000000000000000 ) ) ;
#163251 = CARTESIAN_POINT ( 'NONE',  ( 7.964525173024008531, 11.37936423758166526, 1.199719254218460707 ) ) ;
#163253 = CARTESIAN_POINT ( 'NONE',  ( -8.130085669689073313, 12.63685038127928806, 0.7998128361456481317 ) ) ;
#163252 = CARTESIAN_POINT ( 'NONE',  ( -1.500000000000001332, -1.099999999999976108, 0.000000000000000000 ) ) ;
#163254 = DIRECTION ( 'NONE',  ( -0.000000000000000000, -1.000000000000000000, -0.000000000000000000 ) ) ;
#163255 = CARTESIAN_POINT ( 'NONE',  ( 2.636978264590104537, 1.903244974434484371, 0.6766128908266034747 ) ) ;
#163256 = CARTESIAN_POINT ( 'NONE',  ( 1.364683531249988535, 3.863541667008087543, 0.7879004041258500513 ) ) ;
#163257 = CARTESIAN_POINT ( 'NONE',  ( 9.897088948295943212, 11.60932053017587506, 1.082531754730548412 ) ) ;
#163258 = CARTESIAN_POINT ( 'NONE',  ( 2.970174626046932609, 1.153603175066318931, 1.827835936144058371 ) ) ;
#163259 = CARTESIAN_POINT ( 'NONE',  ( 6.890000000000047642, 2.940278081043229186, 2.731889818495436995 ) ) ;
#163261 = CARTESIAN_POINT ( 'NONE',  ( 4.963960565410041603, 8.060099936542098220, -1.154953748940761971 ) ) ;
#163260 = CARTESIAN_POINT ( 'NONE',  ( 6.210516883511641772, 9.403297576475722508, 1.199719254218452047 ) ) ;
#163262 = CARTESIAN_POINT ( 'NONE',  ( 8.663296969007976855, 12.09063498294259809, -1.082531754730543083 ) ) ;
#163263 = CARTESIAN_POINT ( 'NONE',  ( 8.929730105901844794, 14.71341541692550514, -8.017539274085800471 ) ) ;
#163264 = CARTESIAN_POINT ( 'NONE',  ( -7.917598520700757980, 9.299915031314755609, 1.082531754730558626 ) ) ;
#163265 = CARTESIAN_POINT ( 'NONE',  ( 1.364683531249988757, 1.134375000341421247, 0.000000000000000000 ) ) ;
#163266 = CARTESIAN_POINT ( 'NONE',  ( 2.261505105119133052, 2.148611799745976381, -0.4309092228176118478 ) ) ;
#163267 = CARTESIAN_POINT ( 'NONE',  ( 0.2914054381963314677, 8.170846587878843437, 1.980990740193002919 ) ) ;
#163268 = CARTESIAN_POINT ( 'NONE',  ( 2.237552233957947667, -2.020869686619676919, 1.017492276205993695 ) ) ;
#163269 = CARTESIAN_POINT ( 'NONE',  ( -7.914208982075130905, 10.25632978388623684, -1.599625672291263179 ) ) ;
#163270 = CARTESIAN_POINT ( 'NONE',  ( -2.779058300676974014, 6.186059084191009916, -0.7216878364870257245 ) ) ;
#163271 = CARTESIAN_POINT ( 'NONE',  ( 1.364683531249988535, 3.467708333674749621, -0.7879004041258239610 ) ) ;
#163272 = CARTESIAN_POINT ( 'NONE',  ( 6.162627863271451290, 6.966383021533493647, 0.9102919922300183320 ) ) ;
#163273 =( GEOMETRIC_REPRESENTATION_CONTEXT ( 3 ) GLOBAL_UNCERTAINTY_ASSIGNED_CONTEXT ( ( #67796 ) ) GLOBAL_UNIT_ASSIGNED_CONTEXT ( ( #49934, #100805, #98692 ) ) REPRESENTATION_CONTEXT ( 'NONE', 'WORKASPACE' ) );
#163274 = CARTESIAN_POINT ( 'NONE',  ( -1.500000000000008216, 10.49999999999999467, 3.469446951953614189E-15 ) ) ;
#163275 = CARTESIAN_POINT ( 'NONE',  ( 2.891631901464575272, 6.595597328342462262, 0.000000000000000000 ) ) ;
#163276 = CARTESIAN_POINT ( 'NONE',  ( 2.688433849602299031, -0.2980574676569973658, -1.744271549386553932 ) ) ;
#163277 = CARTESIAN_POINT ( 'NONE',  ( 6.317417574511640765, -0.2763070477263400715, 2.189352377801502936 ) ) ;
#163278 = CARTESIAN_POINT ( 'NONE',  ( 1.364683531249997417, 9.734375000341396245, 2.602085213965210642E-15 ) ) ;
#163279 = CARTESIAN_POINT ( 'NONE',  ( -6.784929528996132220, 6.880448970109080520, 0.000000000000000000 ) ) ;
#163280 = CARTESIAN_POINT ( 'NONE',  ( 4.657827466662149973, 1.163286545301238206, 1.646828140416577879 ) ) ;
#163281 = ORIENTED_EDGE ( 'NONE', *, *, #5825, .T. ) ;
#163282 = EDGE_CURVE ( 'NONE', #138322, #48473, #72823, .T. ) ;
#163283 = CARTESIAN_POINT ( 'NONE',  ( 4.117926171558832671, -0.9613396577640184182, -1.604580606731422776 ) ) ;
#163284 = CARTESIAN_POINT ( 'NONE',  ( 3.801679563076823420, -1.564429233171928058, -1.355977067927462976 ) ) ;
#163285 = CARTESIAN_POINT ( 'NONE',  ( -7.743115126736118015, 8.206258200713163475, 0.7216878364870317197 ) ) ;
#163286 = CARTESIAN_POINT ( 'NONE',  ( -0.4839601414735590357, 3.595939936792758918, -0.4353502767700617171 ) ) ;
#163287 = DIRECTION ( 'NONE',  ( 0.000000000000000000, 0.000000000000000000, -1.000000000000000000 ) ) ;
#163288 = CARTESIAN_POINT ( 'NONE',  ( -5.153105136966797062, 6.602250206728904836, 1.217409160849269423 ) ) ;
#163289 = CARTESIAN_POINT ( 'NONE',  ( -1.001543065824772872E-14, 4.634375000341418804, 1.575800808251672791 ) ) ;
#163290 = CARTESIAN_POINT ( 'NONE',  ( 1.599720133015330337, 1.321132142916726204, 1.382909031182079307 ) ) ;
#163291 = EDGE_CURVE ( 'NONE', #12920, #116778, #201203, .T. ) ;
#163292 = CARTESIAN_POINT ( 'NONE',  ( 3.209375601822930690, -1.602329130913646926, -1.131729396966949963 ) ) ;
#163293 = CARTESIAN_POINT ( 'NONE',  ( 0.6849224457974397717, -1.076149790962807495, -1.704679027301945649 ) ) ;
#163294 = CARTESIAN_POINT ( 'NONE',  ( -3.935609729716867289, 7.813571461303467913, 0.7998128361456352531 ) ) ;
#163295 = CARTESIAN_POINT ( 'NONE',  ( 6.774270308322468459, 11.05506579301824743, 0.7998128361456462443 ) ) ;
#163296 =( BOUNDED_CURVE ( )  B_SPLINE_CURVE ( 2, ( #200424, #183128, #52070, #5410, #34734 ),
 .UNSPECIFIED., .F., .T. ) 
 B_SPLINE_CURVE_WITH_KNOTS ( ( 3, 2, 3 ),
 ( 0.02431251797087543784, 0.02500000000000000139, 0.02553812390681036229 ),
 .UNSPECIFIED. ) 
 CURVE ( )  GEOMETRIC_REPRESENTATION_ITEM ( )  RATIONAL_B_SPLINE_CURVE ( ( 0.9630840743150614891, 0.9778947694582196259, 1.000000000000000000, 0.9826972160490738961, 0.9698637321133645184 ) ) 
 REPRESENTATION_ITEM ( '' )  );
#163297 = CARTESIAN_POINT ( 'NONE',  ( 6.239525796224010712, -1.426203020326064275, -1.361167568813693718 ) ) ;
#163298 = CARTESIAN_POINT ( 'NONE',  ( 0.6823417656249882723, 2.926041667008084879, -1.181850606188754593 ) ) ;
#163299 = CARTESIAN_POINT ( 'NONE',  ( 1.722903956744771481, 1.489010464042400450, -1.355078301658399820 ) ) ;
#163301 = CARTESIAN_POINT ( 'NONE',  ( 2.179462045401040715, 1.638881033884627803, 1.340452329455198210 ) ) ;
#163300 = CARTESIAN_POINT ( 'NONE',  ( -5.558479791922849245, 9.428717490644563881, 0.7216878364870458196 ) ) ;
#163302 = CARTESIAN_POINT ( 'NONE',  ( 8.790438134619867228, 13.29428800202396133, -8.101059483297383679 ) ) ;
#163303 = CARTESIAN_POINT ( 'NONE',  ( 4.316890830952234914, -1.536253448065309613, 1.388129241271539138 ) ) ;
#163304 = CARTESIAN_POINT ( 'NONE',  ( 5.910428620914669473, 5.860197910680708944, 0.000000000000000000 ) ) ;
#163306 = CARTESIAN_POINT ( 'NONE',  ( 3.246287715468270108, 5.874753870433235825, 1.199719254218450271 ) ) ;
#163305 = CARTESIAN_POINT ( 'NONE',  ( 5.665992906516797767, -1.327130266483244059, 1.615391119202228332 ) ) ;
#163308 = ORIENTED_EDGE ( 'NONE', *, *, #193079, .F. ) ;
#163307 = CARTESIAN_POINT ( 'NONE',  ( 3.838725952263983388, 0.2674066485093031242, 1.805754746396167176 ) ) ;
#163309 = CARTESIAN_POINT ( 'NONE',  ( 8.191097360950562845, 12.70803068775103739, -0.7998128361456352531 ) ) ;
#163310 = SURFACE_STYLE_FILL_AREA ( #97256 ) ;
#163311 = CARTESIAN_POINT ( 'NONE',  ( 12.43511541931632891, 7.569548269842172772, -1.878403980710225518 ) ) ;
#163312 = CARTESIAN_POINT ( 'NONE',  ( 0.000000000000000000, -9.900000000000005684, 9.579665964948883783 ) ) ;
#163313 = CARTESIAN_POINT ( 'NONE',  ( 0.6823417656249934904, 10.50520833367472839, 1.181850606188764807 ) ) ;
#163314 = VERTEX_POINT ( 'NONE', #132525 ) ;
#163315 = CARTESIAN_POINT ( 'NONE',  ( 4.951771945676144426, -1.355037094400749487, -1.349591858340569717 ) ) ;
#163316 = CARTESIAN_POINT ( 'NONE',  ( -2.676845263694313637, 5.210404343363602919, -1.199719254218446718 ) ) ;
#163317 = CARTESIAN_POINT ( 'NONE',  ( 7.633404179693907388, 8.864391950186421454, -1.199719254218441611 ) ) ;
#163318 = AXIS2_PLACEMENT_3D ( 'NONE', #159516, #174731, #110833 ) ;
#163319 = CARTESIAN_POINT ( 'NONE',  ( -1.360316468750038865, 1.651041667008089853, -0.7853790794159041244 ) ) ;
#163320 = CARTESIAN_POINT ( 'NONE',  ( 4.975479186090857375, 5.867442474269873642, 1.082531754730560403 ) ) ;
#163321 = EDGE_CURVE ( 'NONE', #157333, #166808, #100501, .T. ) ;
#163322 = CARTESIAN_POINT ( 'NONE',  ( 9.495705940876563389, -8.203192640252447987, -0.2943368945747614762 ) ) ;
#163323 = CARTESIAN_POINT ( 'NONE',  ( -1.040834085586084257E-14, -9.900000000000005684, -9.579665964948867796 ) ) ;
#163324 = CARTESIAN_POINT ( 'NONE',  ( 0.5207438388301621757, -1.748553680932497745, 0.5769860859521497298 ) ) ;
#163325 = EDGE_LOOP ( 'NONE', ( #196316, #44069, #207086, #197486 ) ) ;
#163326 = CARTESIAN_POINT ( 'NONE',  ( -5.901542003698421190, 10.10715911428198055, 0.000000000000000000 ) ) ;
#163327 = CARTESIAN_POINT ( 'NONE',  ( 4.534354090784907143, 1.834037221929617711, 0.3668691113338993781 ) ) ;
#163328 = CARTESIAN_POINT ( 'NONE',  ( -0.02319159430947542386, 5.725354828811364705, -2.405035539666657840 ) ) ;
#163329 = FACE_OUTER_BOUND ( 'NONE', #91487, .T. ) ;
#163330 = DIRECTION ( 'NONE',  ( 0.000000000000000000, -1.000000000000000000, 0.000000000000000000 ) ) ;
#163331 = CARTESIAN_POINT ( 'NONE',  ( -6.316227922719336974, 6.878322274790401814, 0.7073135764556655047 ) ) ;
#163332 = CARTESIAN_POINT ( 'NONE',  ( -7.063434843039784639, 7.343021526408956667, 1.040834085586084257E-14 ) ) ;
#163333 = CARTESIAN_POINT ( 'NONE',  ( 4.578903193113299963, 6.365139696764064325, 1.599625672291267398 ) ) ;
#163334 = CARTESIAN_POINT ( 'NONE',  ( 1.815228950277411712, -1.686530385472130744, -1.016810816036699316 ) ) ;
#163335 = EDGE_CURVE ( 'NONE', #104450, #127597, #186029, .T. ) ;
#163336 = CARTESIAN_POINT ( 'NONE',  ( 2.812125237574263803, 1.117814398428567557, -1.678018709429726307 ) ) ;
#163337 = CARTESIAN_POINT ( 'NONE',  ( -7.320512876374914768, 10.62801655815766999, 1.199719254218453823 ) ) ;
#163338 = CARTESIAN_POINT ( 'NONE',  ( 6.391743074199808916, 6.421731439513382433, -0.7998128361456481317 ) ) ;
#163339 = DIRECTION ( 'NONE',  ( 0.000000000000000000, -1.000000000000000000, 0.000000000000000000 ) ) ;
#163340 = CARTESIAN_POINT ( 'NONE',  ( 2.888834398507355239, 1.879202789969806497, -1.127179367409691935 ) ) ;
#163341 = CARTESIAN_POINT ( 'NONE',  ( -5.572146871515974986, 5.861678842484318253, -0.6761443037284958768 ) ) ;
#163342 = CARTESIAN_POINT ( 'NONE',  ( -8.947491310014823895, 12.52615806407091803, 1.199719254218462483 ) ) ;
#163343 = EDGE_CURVE ( 'NONE', #171443, #5554, #50170, .T. ) ;
#163344 = DIRECTION ( 'NONE',  ( -3.330669073875478989E-16, 3.330669073875478989E-16, 1.000000000000000000 ) ) ;
#163345 = CARTESIAN_POINT ( 'NONE',  ( -1.499999999999997780, 8.627523663848661428, -2.579999999999990301 ) ) ;
#163346 = CARTESIAN_POINT ( 'NONE',  ( 4.936577329151614180, 4.931964103531220722, -0.7216878364870458196 ) ) ;
#163347 = CARTESIAN_POINT ( 'NONE',  ( 9.433775957010412938, 9.900493459467314850, 0.000000000000000000 ) ) ;
#163348 = CARTESIAN_POINT ( 'NONE',  ( 5.124091990960999432, 8.065525525174782828, -1.199719254218452047 ) ) ;
#163349 = DIRECTION ( 'NONE',  ( -0.6507913734559640506, -0.7592566023653004592, 0.000000000000000000 ) ) ;
#163350 = CARTESIAN_POINT ( 'NONE',  ( 5.966997003790217136, 8.054858819212300958, -1.443375672974078761 ) ) ;
#163351 = ORIENTED_EDGE ( 'NONE', *, *, #169868, .T. ) ;
#163352 = VERTEX_POINT ( 'NONE', #19782 ) ;
#163354 = CARTESIAN_POINT ( 'NONE',  ( 1.295565486743395889, 1.859180707359459284, -0.7724582428273608636 ) ) ;
#163353 = CARTESIAN_POINT ( 'NONE',  ( 4.528748383445759806, -1.681502307688139908, 0.7506017836093890061 ) ) ;
#163355 = CARTESIAN_POINT ( 'NONE',  ( 3.374663776259867909, -0.4515557078652779333, 2.253457335377069271 ) ) ;
#163357 = CARTESIAN_POINT ( 'NONE',  ( 2.342426049922683884, -1.823874001192757666, -0.3686824239186973218 ) ) ;
#163356 = PLANE ( 'NONE',  #119892 ) ;
#163358 = CARTESIAN_POINT ( 'NONE',  ( 3.285556943749998737, -2.355208332855375453, -1.896917185911906500 ) ) ;
#163359 = CARTESIAN_POINT ( 'NONE',  ( 6.883263157960362477, -0.004191378316371896506, 2.053658919477070910 ) ) ;
#163360 = CARTESIAN_POINT ( 'NONE',  ( 5.871340715825057011, -1.643613990083541143, -0.9773822251149253404 ) ) ;
#163361 = CARTESIAN_POINT ( 'NONE',  ( -8.779068160048691283, 10.20099992726700933, -1.199719254218446718 ) ) ;
#163362 = CARTESIAN_POINT ( 'NONE',  ( -5.777182853198894463, 9.754147405458438058, 0.7216878364870267237 ) ) ;
#163364 = CARTESIAN_POINT ( 'NONE',  ( 3.942156681999692491, 1.861596489644477437, 0.1839347620080991341 ) ) ;
#163363 = CARTESIAN_POINT ( 'NONE',  ( 5.425362623596053702, -1.327343567673059166, -1.615326566546205767 ) ) ;
#163365 = CARTESIAN_POINT ( 'NONE',  ( 8.297226821883377568, 8.782445501726501291, -0.7216878364870267237 ) ) ;
#163366 = CARTESIAN_POINT ( 'NONE',  ( 5.812015183962491172, 1.231757822100377320, -1.368757117762291253 ) ) ;
#163367 = AXIS2_PLACEMENT_3D ( 'NONE', #37822, #92992, #59398 ) ;
#163368 = CARTESIAN_POINT ( 'NONE',  ( 4.369805582306193870, 3.992528022312320957, 1.214306433183764966E-14 ) ) ;
#163369 = CARTESIAN_POINT ( 'NONE',  ( -9.604686356149279902, 3.481548657788669843, -7.193747284969073341 ) ) ;
#163370 = CARTESIAN_POINT ( 'NONE',  ( 5.479022876622000382, -0.04827441000932602283, -1.724383337574379116 ) ) ;
#163371 = CARTESIAN_POINT ( 'NONE',  ( -4.876128802409253282, 8.840567369452784874, 0.7998128361456481317 ) ) ;
#163372 = DIRECTION ( 'NONE',  ( -1.000000000000000000, 1.224646799147343593E-16, 0.000000000000000000 ) ) ;
#163373 = CARTESIAN_POINT ( 'NONE',  ( 0.3999999999999906408, 3.949999999999988187, -0.8338124244295798126 ) ) ;
#163374 = SURFACE_STYLE_USAGE ( .BOTH. , #31241 ) ;
#163375 = CARTESIAN_POINT ( 'NONE',  ( 4.206061555090504278, 0.7368182104705008895, -2.042320221205825792 ) ) ;
#163376 = CARTESIAN_POINT ( 'NONE',  ( 3.686012862905340803, -0.8985999850123352894, 1.589152278004740237 ) ) ;
#163377 = CARTESIAN_POINT ( 'NONE',  ( 0.8308171121041010299, -1.845250773774274267, -0.6662997747023180484 ) ) ;
#163379 = CARTESIAN_POINT ( 'NONE',  ( 5.858642105998121963, -2.011370865819528397, -0.6617598028889163375 ) ) ;
#163378 = B_SPLINE_CURVE_WITH_KNOTS ( 'NONE', 3,
 ( #103342, #20991, #186712, #175559 ),
 .UNSPECIFIED., .F., .F.,
 ( 4, 4 ),
 ( 8.194944171865289060E-14, 0.0009695358052320346897 ),
 .UNSPECIFIED. ) ;
#163381 = CARTESIAN_POINT ( 'NONE',  ( -1.364683531250012516, 3.551041667008086211, -0.7879004041258300672 ) ) ;
#163380 = CARTESIAN_POINT ( 'NONE',  ( 6.286719507307084065, 1.996765193862446885, -1.125943789698529818 ) ) ;
#163382 = CARTESIAN_POINT ( 'NONE',  ( 2.493739017040840888, 8.265916556960780426, 2.456386464945089276 ) ) ;
#163383 = CARTESIAN_POINT ( 'NONE',  ( 9.576136569953906275, 10.06658084123472641, 0.000000000000000000 ) ) ;
#163384 = CARTESIAN_POINT ( 'NONE',  ( 2.033984416766075665, -2.056095976692096094, 0.5180656111221926263 ) ) ;
#163385 = CARTESIAN_POINT ( 'NONE',  ( -4.609409038966248318, 5.440360635957812718, -1.082531754730544860 ) ) ;
#163386 = PRESENTATION_STYLE_ASSIGNMENT (( #31255 ) ) ;
#163387 = TOROIDAL_SURFACE ( 'NONE', #76781, 10.75000000000000000, 0.5000000000000007772 ) ;
#163388 = CARTESIAN_POINT ( 'NONE',  ( -4.487385655998893164, 6.258369236797239665, 1.443375672974064550 ) ) ;
#163389 = CARTESIAN_POINT ( 'NONE',  ( 6.385609454247954453, -2.047150228866960298, 0.7234482234039444348 ) ) ;
#163391 = CARTESIAN_POINT ( 'NONE',  ( 1.500000000000001332, 13.40625000068279604, 0.000000000000000000 ) ) ;
#163390 = CARTESIAN_POINT ( 'NONE',  ( 6.983263157960330147, 7.051826758666251749, 2.751962080009969114 ) ) ;
#163393 = ORIENTED_EDGE ( 'NONE', *, *, #83796, .F. ) ;
#163392 = CARTESIAN_POINT ( 'NONE',  ( 2.807538669062619174, 1.903917518177394630, -1.144040067606937550 ) ) ;
#163394 = CARTESIAN_POINT ( 'NONE',  ( 0.01878015289935238558, -2.097885004189947278, 0.9400277066241318202 ) ) ;
#163396 = CARTESIAN_POINT ( 'NONE',  ( 5.313357764218651802, -1.739529159241906875, -1.108013508251452395 ) ) ;
#163395 = CARTESIAN_POINT ( 'NONE',  ( 3.310162060030825248, 7.013606170011280838, -0.7998128361456291469 ) ) ;
#163398 = CARTESIAN_POINT ( 'NONE',  ( 1.737499999999999378, -1.866666666666665808, -3.009438278150925683 ) ) ;
#163397 = CARTESIAN_POINT ( 'NONE',  ( 4.193214648376505593, 8.114110533073061404, 0.000000000000000000 ) ) ;
#163399 = CARTESIAN_POINT ( 'NONE',  ( 6.710359684120930091, 6.793450817754725257, 0.7998128361456352531 ) ) ;
#163400 = CARTESIAN_POINT ( 'NONE',  ( -3.285556943750000070, -3.696874999522044458, 0.000000000000000000 ) ) ;
#163401 = CARTESIAN_POINT ( 'NONE',  ( 0.2333540202161610289, 4.089650199633740435, -2.600675808310505044 ) ) ;
#163402 = CARTESIAN_POINT ( 'NONE',  ( 5.460457653299121361, -1.667157065227730106, -0.7818181906407914994 ) ) ;
#163403 = CARTESIAN_POINT ( 'NONE',  ( 4.222474775652216294, 7.013638773981186958, 1.199719254218462483 ) ) ;
#163404 =( LENGTH_UNIT ( ) NAMED_UNIT ( * ) SI_UNIT ( .MILLI., .METRE. ) );
#163405 = CARTESIAN_POINT ( 'NONE',  ( 2.133451061308448526, -1.123891114067215424, -1.308414479858905022 ) ) ;
#163406 = CARTESIAN_POINT ( 'NONE',  ( -0.03006412033006514162, -0.9462945741195265548, 1.780671068589256834 ) ) ;
#163407 = CARTESIAN_POINT ( 'NONE',  ( 2.075183622135381434, -0.9789826713841279782, 2.079913408810558195 ) ) ;
#163408 = CARTESIAN_POINT ( 'NONE',  ( -0.6823417656249969321, 4.280208333674755394, -1.181850606188749264 ) ) ;
#163409 = CARTESIAN_POINT ( 'NONE',  ( 2.864839704461724867, -1.562160111903969417, 1.636705750015782224 ) ) ;
#163410 = CARTESIAN_POINT ( 'NONE',  ( 4.108114811375044084, -2.100464006233178083, 0.1544923775467464122 ) ) ;
#163411 = CARTESIAN_POINT ( 'NONE',  ( -5.008811405605897882, 4.808311159487113073, 0.7998128361456281477 ) ) ;
#163412 = CARTESIAN_POINT ( 'NONE',  ( 2.073191327021279839, 1.695144128639828551, -0.5084401619379045334 ) ) ;
#163413 = CARTESIAN_POINT ( 'NONE',  ( 6.799577732453452761, 7.891594428405881878, -1.199719254218446718 ) ) ;
#163414 = CARTESIAN_POINT ( 'NONE',  ( 4.217995187182915551, 7.935095128439824563, 0.7216878364870257245 ) ) ;
#163416 = EDGE_CURVE ( 'NONE', #148633, #166401, #155866, .T. ) ;
#163415 = CARTESIAN_POINT ( 'NONE',  ( -4.141125853970233806, 6.918731698685530063, -1.199719254218452047 ) ) ;
#163417 = CARTESIAN_POINT ( 'NONE',  ( -1.500000000000013101, 1.920833333333356263, 0.8660254037844403729 ) ) ;
#163418 = VECTOR ( 'NONE', #201478, 1000.000000000000000 ) ;
#163419 = CARTESIAN_POINT ( 'NONE',  ( 5.836230100724939085, -1.233609159639902142, -1.847210489216906781 ) ) ;
#163420 = CARTESIAN_POINT ( 'NONE',  ( 3.117305861062225958, -2.111875107304355570, 0.5849144002756587746 ) ) ;
#163421 = CARTESIAN_POINT ( 'NONE',  ( -5.623934791570306402, 5.455678766453782913, 0.7998128361456341429 ) ) ;
#163422 = CARTESIAN_POINT ( 'NONE',  ( 0.3520457843950711707, 7.165311474886529197, -1.969365997876474372 ) ) ;
#163423 = CARTESIAN_POINT ( 'NONE',  ( 6.445950376775947177, -1.384621037358444662, -1.606076714075025613 ) ) ;
#163424 = CARTESIAN_POINT ( 'NONE',  ( 0.6823417656249899377, 3.676041667008085767, -1.181850606188754593 ) ) ;
#163425 = CARTESIAN_POINT ( 'NONE',  ( -0.6823417656250003738, 9.401041667008065872, 1.181850606188754593 ) ) ;
#163426 = CARTESIAN_POINT ( 'NONE',  ( -3.633221978782290140, 6.222214161012547429, -1.082531754730549967 ) ) ;
#163427 = CARTESIAN_POINT ( 'NONE',  ( 6.082307721193076944, 1.091511717630256673, 1.817998432235830908 ) ) ;
#163428 = CARTESIAN_POINT ( 'NONE',  ( -4.990809943606273613, 7.876343129965691858, -1.082531754730549967 ) ) ;
#163429 = ORIENTED_EDGE ( 'NONE', *, *, #116484, .T. ) ;
#163430 = CARTESIAN_POINT ( 'NONE',  ( -5.153507786970275006, 7.105788066255672497, -1.443375672974066548 ) ) ;
#163431 = CARTESIAN_POINT ( 'NONE',  ( 6.356075086708249167, 6.309842444114747373, -0.7998128361456281477 ) ) ;
#163432 = CARTESIAN_POINT ( 'NONE',  ( 6.146043377905669125, 0.5841948715668408010, 1.746183665442810007 ) ) ;
#163433 = CYLINDRICAL_SURFACE ( 'NONE', #139208, 1.500000000000000222 ) ;
#163434 = CARTESIAN_POINT ( 'NONE',  ( -0.09252986283065423034, 7.021014873008922130, -3.994686497345164344 ) ) ;
#163435 = CARTESIAN_POINT ( 'NONE',  ( 0.6823417656249899377, 4.488541667008086655, -1.181850606188754593 ) ) ;
#163436 = CARTESIAN_POINT ( 'NONE',  ( 2.630072014739594177, 0.2149344560898290013, 1.727053582138169618 ) ) ;
#163437 = CARTESIAN_POINT ( 'NONE',  ( -5.916355281146389089, 6.815393236815656230, -0.9995835186326230692 ) ) ;
#163438 = CARTESIAN_POINT ( 'NONE',  ( -9.499766273075886502, -9.919999999999998153, 0.06663900456894958357 ) ) ;
#163439 = CARTESIAN_POINT ( 'NONE',  ( -1.402160292154681736E-14, -0.3656249996585805295, 1.575800808251672791 ) ) ;
#163440 = DIRECTION ( 'NONE',  ( 7.387867266669436732E-31, -1.000000000000000000, -8.546850786086424434E-32 ) ) ;
#163441 = CARTESIAN_POINT ( 'NONE',  ( -2.549999999999999378, 2.499999999999998668, 1.849324200890692271 ) ) ;
#163442 = CARTESIAN_POINT ( 'NONE',  ( -8.597841969360544567, 13.18256606422934674, 0.7998128361456341429 ) ) ;
#163443 = CARTESIAN_POINT ( 'NONE',  ( -5.870317324592812191, 7.871789516823500144, -1.443375672974051449 ) ) ;
#163444 = CARTESIAN_POINT ( 'NONE',  ( 5.928642344448160628, 2.082074431819755045, 0.5810635428650026135 ) ) ;
#163446 = ORIENTED_EDGE ( 'NONE', *, *, #122616, .T. ) ;
#163445 = LINE ( 'NONE', #165564, #174434 ) ;
#163447 = CARTESIAN_POINT ( 'NONE',  ( -0.6823417656250212460, 4.801041667008086655, 1.181850606188767472 ) ) ;
#163448 = CARTESIAN_POINT ( 'NONE',  ( 6.415303688471941435, -0.2438443212883933120, 1.956177878852760177 ) ) ;
#163449 = CARTESIAN_POINT ( 'NONE',  ( 5.624279254961046526, 0.3357223255188810374, -1.700804604882939053 ) ) ;
#163451 = CARTESIAN_POINT ( 'NONE',  ( 2.120887600855193345, 0.003649250790785373531, 2.191739723551556551 ) ) ;
#163450 = CARTESIAN_POINT ( 'NONE',  ( -1.360316468750030428, -0.6093749996585878792, -1.908195823574487804E-14 ) ) ;
#163452 = CARTESIAN_POINT ( 'NONE',  ( 3.329449612262088021, 0.05463889213834548231, 2.307092628889866326 ) ) ;
#163453 = CARTESIAN_POINT ( 'NONE',  ( 6.380161626619829107, -1.106262522808113324, 1.738493956250926287 ) ) ;
#163454 = CARTESIAN_POINT ( 'NONE',  ( 0.8845914429877841378, 1.712865214261191316, -0.9150308779080836841 ) ) ;
#163455 = CARTESIAN_POINT ( 'NONE',  ( -6.846504384776774366, 7.089935991768773427, -0.7216878364870267237 ) ) ;
#163457 = EDGE_CURVE ( 'NONE', #198860, #120109, #133074, .T. ) ;
#163456 = CARTESIAN_POINT ( 'NONE',  ( -4.248501033035892327, 6.049946853332221153, -1.599625672291271394 ) ) ;
#163458 = CARTESIAN_POINT ( 'NONE',  ( -9.439063866441687267, 15.48793654326890490, 7.409881740265291228 ) ) ;
#163459 = CARTESIAN_POINT ( 'NONE',  ( 4.219064148821600746, 1.637239594409030330, -1.347683705884415106 ) ) ;
#163460 = CARTESIAN_POINT ( 'NONE',  ( 1.811172873341511336, 1.158687402475454098, -1.650082692374904125 ) ) ;
#163461 = CARTESIAN_POINT ( 'NONE',  ( -4.867013957181525186, 8.622007350113015889, 0.7216878364870458196 ) ) ;
#163462 = CARTESIAN_POINT ( 'NONE',  ( 4.278500955059440614, -1.273273528111932063, 1.802203266693293671 ) ) ;
#163463 = CARTESIAN_POINT ( 'NONE',  ( -3.285556943750000070, -0.8968749995220438587, 0.000000000000000000 ) ) ;
#163464 = CARTESIAN_POINT ( 'NONE',  ( -10.16279779336428035, 3.829867255648772950, 5.736760595005079288 ) ) ;
#163465 = CARTESIAN_POINT ( 'NONE',  ( -8.103009739377986520, -6.893137084989842123, 7.439168848974023973 ) ) ;
#163466 = CARTESIAN_POINT ( 'NONE',  ( -6.424584688029276514, 8.588711117491191871, 1.599625672291269396 ) ) ;
#163468 = CARTESIAN_POINT ( 'NONE',  ( -10.71948157449083183, -8.605866298766125411, 0.1871092468795332309 ) ) ;
#163467 = CARTESIAN_POINT ( 'NONE',  ( -5.242543201390849283, 7.800132786123255002, 1.293859303942331840 ) ) ;
#163469 = DIRECTION ( 'NONE',  ( -1.000000000000000000, 0.000000000000000000, 0.000000000000000000 ) ) ;
#163470 = ORIENTED_EDGE ( 'NONE', *, *, #5768, .F. ) ;
#163471 = CARTESIAN_POINT ( 'NONE',  ( 4.909085936489448798, 1.792118714629163057, 1.017505292531006189 ) ) ;
#163472 = DIRECTION ( 'NONE',  ( -0.7592566023652995710, -0.6507913734559650498, 0.000000000000000000 ) ) ;
#163473 = CARTESIAN_POINT ( 'NONE',  ( -5.579343907223557331, 6.467988298970945849, 1.199719254218450271 ) ) ;
#163474 = CARTESIAN_POINT ( 'NONE',  ( 3.035811672558884400, -1.945802561663440455, 0.5409189654149139104 ) ) ;
#163475 = CARTESIAN_POINT ( 'NONE',  ( 1.499999999999987121, 0.5041666666666856367, 0.8660254037844524744 ) ) ;
#163476 = CARTESIAN_POINT ( 'NONE',  ( 10.05978679165993483, 11.79913468076720306, 1.082531754730548412 ) ) ;
#163477 = CARTESIAN_POINT ( 'NONE',  ( 5.445571254183207088, 9.504916896522420444, -0.7998128361456281477 ) ) ;
#163478 = CARTESIAN_POINT ( 'NONE',  ( 3.520434746236697610, 1.308796515248649817, -1.591936018771279659 ) ) ;
#163479 = CARTESIAN_POINT ( 'NONE',  ( 6.727182134110202938, 2.016807574165893513, 2.492494991173600738 ) ) ;
#163480 = CARTESIAN_POINT ( 'NONE',  ( 3.818592820543298405, 7.606775390609172405, -0.7998128361456221525 ) ) ;
#163481 = CIRCLE ( 'NONE', #177241, 10.99999999999999112 ) ;
#163482 = CARTESIAN_POINT ( 'NONE',  ( -0.1408020194050146334, 0.2351808081714431564, -2.134421755367508666 ) ) ;
#163483 = CARTESIAN_POINT ( 'NONE',  ( 1.077780131904103156, -1.795810734350095750, -0.4053039038426772267 ) ) ;
#163484 = MECHANICAL_DESIGN_GEOMETRIC_PRESENTATION_REPRESENTATION (  '', ( #87406 ), #170422 ) ;
#163485 = CARTESIAN_POINT ( 'NONE',  ( 0.1535068347273665368, -1.849414538273885578, 1.380102022147772667 ) ) ;
#163486 = CARTESIAN_POINT ( 'NONE',  ( 6.282224075085741433, 8.422623735723785643, 1.599625672291268286 ) ) ;
#163487 = CARTESIAN_POINT ( 'NONE',  ( 2.337400524717429207, -1.931973293601353392, 0.9696072025056484689 ) ) ;
#163488 = CARTESIAN_POINT ( 'NONE',  ( -4.202664430556263930, 5.926194473780837413, 1.443375672974064550 ) ) ;
#163489 = CARTESIAN_POINT ( 'NONE',  ( 1.393767942625488532, -2.000731169080074423, 0.2516357431460446992 ) ) ;
#163490 = ADVANCED_FACE ( 'NONE', ( #115233 ), #7794, .F. ) ;
#163491 = CARTESIAN_POINT ( 'NONE',  ( 2.478211020838327894, 2.052291828077044133, 1.034905392717075046 ) ) ;
#163492 = CARTESIAN_POINT ( 'NONE',  ( 4.183485216215308000, 3.563207579971337857, -2.499999999999995115 ) ) ;
#163493 = CARTESIAN_POINT ( 'NONE',  ( 1.355808955840422310E-16, 2.999999999999975131, 2.024999999999999911 ) ) ;
#163494 = ORIENTED_EDGE ( 'NONE', *, *, #57019, .F. ) ;
#163495 = CARTESIAN_POINT ( 'NONE',  ( 4.065273027966066266, 0.2426392691956253123, -1.956424757721614949 ) ) ;
#163496 = CARTESIAN_POINT ( 'NONE',  ( 4.962125165302472496, -1.116212726388360998, 1.679221540125563905 ) ) ;
#163498 = CARTESIAN_POINT ( 'NONE',  ( 9.042925270190622200, 12.53353466765568669, 1.082531754730546636 ) ) ;
#163497 = CARTESIAN_POINT ( 'NONE',  ( -0.6823417656250212460, 3.051041667008084879, 1.181850606188767472 ) ) ;
#163500 = CARTESIAN_POINT ( 'NONE',  ( 5.953767555512091469, 0.6130212357637642162, -2.014879775860946687 ) ) ;
#163499 = CARTESIAN_POINT ( 'NONE',  ( -7.237355071596549116, 7.338002426484427687, 1.040834085586084257E-14 ) ) ;
#163501 = CARTESIAN_POINT ( 'NONE',  ( 6.672334155782003506, -0.9722939650993901450, -1.827837255792996718 ) ) ;
#163502 = CARTESIAN_POINT ( 'NONE',  ( 5.469824908109481854, 8.468880595181346393, -1.199719254218446718 ) ) ;
#163503 = CARTESIAN_POINT ( 'NONE',  ( -6.551614543901706611, 8.666636272683888365, 1.599625672291283607 ) ) ;
#163504 = CARTESIAN_POINT ( 'NONE',  ( -1.474093356799783594, 8.744500914157981697, 2.533844564144187572 ) ) ;
#163505 = CARTESIAN_POINT ( 'NONE',  ( -0.1753031400193918732, -0.9122597987226389593, -1.912455998546586544 ) ) ;
#163506 = CARTESIAN_POINT ( 'NONE',  ( -1.500000000000001332, 0.4312500006828159926, 0.000000000000000000 ) ) ;
#163507 = CARTESIAN_POINT ( 'NONE',  ( 4.266487514486948740, 1.085833288323118095, 2.036285375418740884 ) ) ;
#163508 = CARTESIAN_POINT ( 'NONE',  ( 1.586864402838471522, 1.986712475098152408, 0.5538950855334312529 ) ) ;
#163509 = CARTESIAN_POINT ( 'NONE',  ( 7.958272981541723468, 8.386999354661243800, 1.040834085586084257E-14 ) ) ;
#163510 = CARTESIAN_POINT ( 'NONE',  ( 6.229045230835819069, 6.231917288922055320, -0.7998128361456481317 ) ) ;
#163511 = CARTESIAN_POINT ( 'NONE',  ( 5.357406976055401948, 6.279338222599979424, 1.199719254218452935 ) ) ;
#163512 = CARTESIAN_POINT ( 'NONE',  ( -1.364683531250014514, 1.051041667008090208, -0.7879004041258289570 ) ) ;
#163513 = CARTESIAN_POINT ( 'NONE',  ( 5.551137550152489553, 5.441024994791534120, 0.7998128361456352531 ) ) ;
#163514 = CARTESIAN_POINT ( 'NONE',  ( 6.195713011320782115, 8.251417818006149929, -1.443375672974057666 ) ) ;
#163515 = CARTESIAN_POINT ( 'NONE',  ( 3.684171759641508448, -1.290596846074614223, -1.745836057026050714 ) ) ;
#163516 = CARTESIAN_POINT ( 'NONE',  ( 0.3878679656440017220, 3.999999999999996891, 1.007084189318337542 ) ) ;
#163518 = CARTESIAN_POINT ( 'NONE',  ( 3.456447201099471123, -1.625387274077850996, -0.8650149607793489182 ) ) ;
#163517 = CARTESIAN_POINT ( 'NONE',  ( -3.877268743828284681, 5.546566172598190292, 1.443375672974064550 ) ) ;
#163519 = CARTESIAN_POINT ( 'NONE',  ( -1.201851678989727383E-14, 5.196875000341422357, -1.575800808251660134 ) ) ;
#163520 = CARTESIAN_POINT ( 'NONE',  ( 5.566036750361066154, -1.391122746885119499, 1.693456055751572986 ) ) ;
#163521 = CARTESIAN_POINT ( 'NONE',  ( 8.202753408314407579, 14.20975653142720319, 8.698399028645537712 ) ) ;
#163522 = CARTESIAN_POINT ( 'NONE',  ( 6.262609139476608355, -1.605266756365858027, 1.594658822776671592 ) ) ;
#163523 = CARTESIAN_POINT ( 'NONE',  ( -5.495703055830178485, 6.420018438214686540, -1.282350674470073448 ) ) ;
#163524 = CARTESIAN_POINT ( 'NONE',  ( 5.084740326411086642, 7.951855545768795608, 1.193092838546747414 ) ) ;
#163525 = AXIS2_PLACEMENT_3D ( 'NONE', #186749, #138021, #40525 ) ;
#163526 = CARTESIAN_POINT ( 'NONE',  ( -5.763624699140882157, 7.817591130454727200, -1.443375672974066548 ) ) ;
#163527 = CARTESIAN_POINT ( 'NONE',  ( -6.455298931196955969, -8.176227052203554280, -7.002681350352330192 ) ) ;
#163528 = CARTESIAN_POINT ( 'NONE',  ( 6.608682216863940084, 1.309337763449496705, -1.190854552318038051 ) ) ;
#163529 = CARTESIAN_POINT ( 'NONE',  ( 0.6823417656249969321, 12.52604166700806232, -1.181850606188757036 ) ) ;
#163530 = CARTESIAN_POINT ( 'NONE',  ( 4.512362120423671463, -2.012691318418479813, -0.04721358428917859368 ) ) ;
#163531 = CARTESIAN_POINT ( 'NONE',  ( 7.145310649601935182, 8.294949498412453437, -1.199719254218446718 ) ) ;
#163532 = CARTESIAN_POINT ( 'NONE',  ( 2.467921950875014314, 2.065534160692492627, -0.4097329821706324204 ) ) ;
#163533 = CARTESIAN_POINT ( 'NONE',  ( 2.126450742919711256, 0.4219061677965991741, 1.868383228629175719 ) ) ;
#163534 = CARTESIAN_POINT ( 'NONE',  ( 2.523789150438203510, 6.096171108819874007, 0.7998128361456462443 ) ) ;
#163536 = ADVANCED_FACE ( 'NONE', ( #187620 ), #75351, .T. ) ;
#163535 = CARTESIAN_POINT ( 'NONE',  ( 2.875404442980381781, -0.1956706474990059230, 1.959820717905029097 ) ) ;
#163537 = CARTESIAN_POINT ( 'NONE',  ( 2.096370420935515178, -0.4963513585865795275, -1.803540123670114736 ) ) ;
#163538 = CARTESIAN_POINT ( 'NONE',  ( 0.7308173252688826560, -1.846041318942293286, -0.6644482084196751126 ) ) ;
#163541 = ORIENTED_EDGE ( 'NONE', *, *, #45298, .T. ) ;
#163540 = CARTESIAN_POINT ( 'NONE',  ( 6.504213119055646253, -0.7662104867102972339, 1.640237621407932167 ) ) ;
#163539 = CARTESIAN_POINT ( 'NONE',  ( 3.510098308409233869, -0.7004517935718050925, -1.576443202522736842 ) ) ;
#163543 = CARTESIAN_POINT ( 'NONE',  ( 4.799223189557548785, 7.582548906917042864, -1.082531754730549078 ) ) ;
#163542 = CARTESIAN_POINT ( 'NONE',  ( 1.225528936851564721, -0.05108506852482053856, 2.206457870188942572 ) ) ;
#163544 = CARTESIAN_POINT ( 'NONE',  ( -0.6823417656250003738, 0.5302083336747518416, -1.181850606188749264 ) ) ;
#163545 = CARTESIAN_POINT ( 'NONE',  ( 11.44786932348528907, 12.30000000000000071, -3.303370173849653035 ) ) ;
#163546 = CARTESIAN_POINT ( 'NONE',  ( 0.000000000000000000, 7.980384757729337863, 0.000000000000000000 ) ) ;
#163547 = CARTESIAN_POINT ( 'NONE',  ( -0.5000000000000073275, 3.299999999999997158, 0.4999999999999917843 ) ) ;
#163548 = AXIS2_PLACEMENT_3D ( 'NONE', #184572, #59656, #142013 ) ;
#163549 = CARTESIAN_POINT ( 'NONE',  ( 6.614133338355735248, 2.065126723422955557, -0.1462301744803648496 ) ) ;
#163550 = AXIS2_PLACEMENT_3D ( 'NONE', #39613, #71016, #40700 ) ;
#163551 = CARTESIAN_POINT ( 'NONE',  ( 1.100149375694438714, 0.8407228983892693908, -1.892171374333020406 ) ) ;
#163552 = CARTESIAN_POINT ( 'NONE',  ( -1.500000000000013101, 1.629166666666691077, -0.8660254037844313801 ) ) ;
#163553 = CARTESIAN_POINT ( 'NONE',  ( 6.908042961362778733, 8.018137195466769285, 1.199719254218462483 ) ) ;
#163554 = CARTESIAN_POINT ( 'NONE',  ( -8.688077508258798431, 9.030511935923748013, -0.7998128361456291469 ) ) ;
#163555 = CARTESIAN_POINT ( 'NONE',  ( 6.364626766972446781, 6.390095747748157251, 0.7998128361456352531 ) ) ;
#163556 = CARTESIAN_POINT ( 'NONE',  ( 5.338584462458719315, 1.262900380722062454, -1.703257760751579530 ) ) ;
#163557 = CARTESIAN_POINT ( 'NONE',  ( 3.223806664999388172, 6.983134552466421674, -0.7998128361456362523 ) ) ;
#163558 = CARTESIAN_POINT ( 'NONE',  ( -1.364683531250014514, 1.738541667008085545, -0.7879004041258289570 ) ) ;
#163559 = VERTEX_POINT ( 'NONE', #94979 ) ;
#163561 = EDGE_CURVE ( 'NONE', #130319, #149611, #135162, .T. ) ;
#163560 = CARTESIAN_POINT ( 'NONE',  ( -1.499999999999997780, 2.900000000000020783, 1.214306433183764966E-14 ) ) ;
#163563 = CARTESIAN_POINT ( 'NONE',  ( 5.034155109375821446, 4.767602470560229122, -0.7998128361456221525 ) ) ;
#163562 = CARTESIAN_POINT ( 'NONE',  ( 6.549272904993657995, 1.707534169505098953, -0.9658701945045378157 ) ) ;
#163564 = CARTESIAN_POINT ( 'NONE',  ( 4.270861128529729989, -2.010896307770511537, 0.1455111863851859810 ) ) ;
#163565 = CARTESIAN_POINT ( 'NONE',  ( 3.555789339581526320, 1.068723753765013162, 1.589688962476828005 ) ) ;
#163566 = CARTESIAN_POINT ( 'NONE',  ( 2.679285714285720044, -0.4970443252110337551, 0.000000000000000000 ) ) ;
#163567 = CIRCLE ( 'NONE', #153186, 0.5000000000000004441 ) ;
#163568 = CARTESIAN_POINT ( 'NONE',  ( 1.312353134292881141, 1.468346937154514364, -1.627112938194043235 ) ) ;
#163569 = CARTESIAN_POINT ( 'NONE',  ( 0.1333692844072801587, 4.087911462428309051, -2.608372271572469092 ) ) ;
#163570 = CARTESIAN_POINT ( 'NONE',  ( 3.549935554046261821, 1.870726058081632504, 0.003126486288931861444 ) ) ;
#163571 = CARTESIAN_POINT ( 'NONE',  ( -1.402160292154681736E-14, 0.3687500006828169363, -1.732050807568870754 ) ) ;
#163572 = CARTESIAN_POINT ( 'NONE',  ( -6.205881626753225966, 8.263281202677319470, 1.599625672291283607 ) ) ;
#163574 = CARTESIAN_POINT ( 'NONE',  ( 5.870749427052773584, -0.3112397890362226249, -2.094129459642315005 ) ) ;
#163573 = CARTESIAN_POINT ( 'NONE',  ( -3.443407828190963915, 6.961133532957338943, 0.7216878364870317197 ) ) ;
#163575 = CARTESIAN_POINT ( 'NONE',  ( -1.380481604194455425, 13.35137502475254223, 0.2305342759981895417 ) ) ;
#163577 = DIRECTION ( 'NONE',  ( -0.000000000000000000, -0.000000000000000000, 1.000000000000000000 ) ) ;
#163576 = CARTESIAN_POINT ( 'NONE',  ( 2.683241491500857556, 1.480437668936212869, 1.476589516890645104 ) ) ;
#163579 = ORIENTED_EDGE ( 'NONE', *, *, #103623, .F. ) ;
#163578 = CARTESIAN_POINT ( 'NONE',  ( 1.219288043345586159, -1.683946549099228029, 0.3722564037182389818 ) ) ;
#163580 = CARTESIAN_POINT ( 'NONE',  ( 6.745345117998789775, 7.828323044875442172, 1.199719254218462483 ) ) ;
#163581 = AXIS2_PLACEMENT_3D ( 'NONE', #116011, #81321, #32567 ) ;
#163582 = DIRECTION ( 'NONE',  ( 1.000000000000000000, -0.000000000000000000, -0.000000000000000000 ) ) ;
#163583 = CARTESIAN_POINT ( 'NONE',  ( 0.01492019832702046536, -9.953727901176275594, 9.579640682430678567 ) ) ;
#163584 = CARTESIAN_POINT ( 'NONE',  ( -9.356550365033111660, 14.56579225990834736, 7.432331899221528815 ) ) ;
#163586 = CARTESIAN_POINT ( 'NONE',  ( 8.880227426826641235, 10.42298208846167284, 1.082531754730549967 ) ) ;
#163585 = CARTESIAN_POINT ( 'NONE',  ( 7.793239369756836510, 7.986534107671458216, 0.7998128361456341429 ) ) ;
#163587 = ORIENTED_EDGE ( 'NONE', *, *, #97862, .F. ) ;
#163588 = CARTESIAN_POINT ( 'NONE',  ( -0.4019237886466871523, 9.448664549684627545, -1.499999999999998668 ) ) ;
#163590 = CARTESIAN_POINT ( 'NONE',  ( 1.629273880293732768, -0.2214294203813528539, 1.797790724094426418 ) ) ;
#163589 = CARTESIAN_POINT ( 'NONE',  ( 5.855142236255289845, 7.924361590421551860, -1.599625672291281386 ) ) ;
#163591 = CARTESIAN_POINT ( 'NONE',  ( -6.531277313481209212, 8.642909503859968368, 1.599625672291283607 ) ) ;
#163592 = CARTESIAN_POINT ( 'NONE',  ( 4.761938266897790761, 6.578680616179308771, 1.599625672291267398 ) ) ;
#163593 = CARTESIAN_POINT ( 'NONE',  ( 6.398522151006641678, 6.429640362454684954, 0.000000000000000000 ) ) ;
#163594 = CARTESIAN_POINT ( 'NONE',  ( 6.639320575229255006, 1.299223727596211519, 1.914393416674460946 ) ) ;
#163595 = CARTESIAN_POINT ( 'NONE',  ( 1.500000000000001332, 9.125000000000001776, 0.000000000000000000 ) ) ;
#163596 = CARTESIAN_POINT ( 'NONE',  ( 4.097125688280337741, 7.463757567055806064, 0.6283840521477540575 ) ) ;
#163597 = CARTESIAN_POINT ( 'NONE',  ( 7.931156674314368438, 12.19684052010138586, 1.040834085586084257E-14 ) ) ;
#163598 = ORIENTED_EDGE ( 'NONE', *, *, #52269, .F. ) ;
#163599 = CARTESIAN_POINT ( 'NONE',  ( 3.086215985183130339, 1.036139677906501300, -1.545717422611452729 ) ) ;
#163600 = CARTESIAN_POINT ( 'NONE',  ( 0.5971114826688945776, -0.2799204757548044986, 1.894894164429518746 ) ) ;
#163601 = CARTESIAN_POINT ( 'NONE',  ( 6.756866522006341746, -1.488468187722398417, 1.222521302487014072 ) ) ;
#163602 = CARTESIAN_POINT ( 'NONE',  ( -10.38614328979761403, 3.507114751586604129, 5.996442624206741456 ) ) ;
#163603 = CARTESIAN_POINT ( 'NONE',  ( 5.040934186182656873, 4.775511393501539636, 1.040834085586084257E-14 ) ) ;
#163604 = CARTESIAN_POINT ( 'NONE',  ( 4.675188888464441028, 8.274035074156913083, -0.5495550137140058355 ) ) ;
#163605 = CARTESIAN_POINT ( 'NONE',  ( -1.806654366501805775, 2.518449987798942136, 2.500000000000000444 ) ) ;
#163606 = CARTESIAN_POINT ( 'NONE',  ( -2.928197990871687306, 5.399686175116803710, 1.082531754730560403 ) ) ;
#163607 = CARTESIAN_POINT ( 'NONE',  ( 8.920901888112002354, 9.510066412326583674, 0.7216878364870438212 ) ) ;
#163608 = CARTESIAN_POINT ( 'NONE',  ( 4.487129304207951641, 0.09229547738082846675, 1.967383831439367903 ) ) ;
#163609 = EDGE_CURVE ( 'NONE', #141559, #107270, #156053, .T. ) ;
#163610 = CARTESIAN_POINT ( 'NONE',  ( 1.190261156817543631, 1.266008754425467897, 1.700926646755014593 ) ) ;
#163611 = CARTESIAN_POINT ( 'NONE',  ( -5.042743069279040036, 7.970618449879118828, 1.199719254218464037 ) ) ;
#163612 = CARTESIAN_POINT ( 'NONE',  ( -11.52515587343483539, 8.148303942382858267, 3.187149427615555197 ) ) ;
#163613 = CARTESIAN_POINT ( 'NONE',  ( 10.39025099420818776, 3.467171072964057910, 5.998814208453757679 ) ) ;
#163614 = CARTESIAN_POINT ( 'NONE',  ( 5.402338782601354694, 1.661146971675907302, -1.429436781345946317 ) ) ;
#163615 = CARTESIAN_POINT ( 'NONE',  ( -0.4019237886467001974, 10.08258545099816850, 1.500000000000001998 ) ) ;
#163616 = CARTESIAN_POINT ( 'NONE',  ( 4.823225626762606133, -0.09501261394700975804, 1.924175346943966414 ) ) ;
#163617 = CARTESIAN_POINT ( 'NONE',  ( -5.747767057189642870, 8.793146435774861658, -1.199719254218440723 ) ) ;
#163618 = EDGE_CURVE ( 'NONE', #2249, #104090, #81244, .T. ) ;
#163619 = CARTESIAN_POINT ( 'NONE',  ( 0.7272432748211544729, -1.735090175422876246, 0.5678700757711930835 ) ) ;
#163620 = CARTESIAN_POINT ( 'NONE',  ( 0.7860941533469124609, 1.484900681275106216, 1.632775826992872492 ) ) ;
#163621 = DIRECTION ( 'NONE',  ( 0.000000000000000000, 1.000000000000000000, 0.000000000000000000 ) ) ;
#163622 = VERTEX_POINT ( 'NONE', #209749 ) ;
#163623 = CARTESIAN_POINT ( 'NONE',  ( 3.607878275012313285, 6.262922849939428716, 1.082531754730549078 ) ) ;
#163624 = ORIENTED_EDGE ( 'NONE', *, *, #209595, .T. ) ;
#163625 = CARTESIAN_POINT ( 'NONE',  ( 5.910992199152527604, -1.554775717584104378, 1.208803697826433599 ) ) ;
#163626 = CARTESIAN_POINT ( 'NONE',  ( 1.118581540066618141, -0.04615595083166770807, 1.941663063996822869 ) ) ;
#163627 = CARTESIAN_POINT ( 'NONE',  ( 6.884150280000160826, -0.1566355309425542519, 2.263600626914013869 ) ) ;
#163629 = CARTESIAN_POINT ( 'NONE',  ( 5.682414339916787682, 1.109973489246698808, -1.493480506080862469 ) ) ;
#163628 = CARTESIAN_POINT ( 'NONE',  ( -6.282224075085783177, 8.422623735723785643, 1.599625672291269396 ) ) ;
#163630 = CARTESIAN_POINT ( 'NONE',  ( 5.363132282657546490, 8.414682208812571673, -1.199719254218452047 ) ) ;
#163631 = CARTESIAN_POINT ( 'NONE',  ( 6.509000000000010999, 0.004788705324892603143, 2.000274819378269786 ) ) ;
#163632 = CARTESIAN_POINT ( 'NONE',  ( -7.203459687562382641, 7.298457811777897319, -0.7998128361456291469 ) ) ;
#163633 = CARTESIAN_POINT ( 'NONE',  ( -7.584860592202423035, 7.813701877183096833, -0.7998128361456362523 ) ) ;
#163634 = CARTESIAN_POINT ( 'NONE',  ( 1.470551405592795957, -2.082434148983134392, -0.6831980896230758216 ) ) ;
#163635 = CARTESIAN_POINT ( 'NONE',  ( 5.694061328059515148, 5.745419092265303007, -0.7216878364870207285 ) ) ;
#163636 = ORIENTED_EDGE ( 'NONE', *, *, #137720, .F. ) ;
#163637 = CARTESIAN_POINT ( 'NONE',  ( 0.4499999960734660243, 3.999999999999974243, -0.9281957781481884329 ) ) ;
#163638 = CARTESIAN_POINT ( 'NONE',  ( 7.334597915313080918, 9.580116872663850813, 1.040834085586084257E-14 ) ) ;
#163639 = CARTESIAN_POINT ( 'NONE',  ( 1.980809073483770000, -0.08854697198140694392, -1.823669195971427071 ) ) ;
#163640 = CARTESIAN_POINT ( 'NONE',  ( 6.966220764712121927, 6.002124920821316323, 2.420000000000000373 ) ) ;
#163641 = VECTOR ( 'NONE', #35769, 1000.000000000000000 ) ;
#163642 = CARTESIAN_POINT ( 'NONE',  ( -0.1240337052346596886, 2.520685617421167368, -1.998971434602998087 ) ) ;
#163643 = CARTESIAN_POINT ( 'NONE',  ( 6.509000000000045638, 3.691181720027385094, 2.614238911931165088 ) ) ;
#163644 = CARTESIAN_POINT ( 'NONE',  ( 9.402743226277308963, 10.92862083786708816, -1.199719254218446718 ) ) ;
#163645 = CIRCLE ( 'NONE', #191279, 6.264285714285709794 ) ;
#163646 = CARTESIAN_POINT ( 'NONE',  ( 0.08247339995742437868, -1.868340020190910833, -0.4694531300831055742 ) ) ;
#163647 = CARTESIAN_POINT ( 'NONE',  ( 4.346505277090593644, -1.939800950321630690, -0.2920161945778113055 ) ) ;
#163648 = CARTESIAN_POINT ( 'NONE',  ( -9.365985188942097750, 9.821404230054264772, 0.7998128361456462443 ) ) ;
#163649 = CARTESIAN_POINT ( 'NONE',  ( 6.474182045725470402, 7.511966127223233869, -1.199719254218446718 ) ) ;
#163650 = CARTESIAN_POINT ( 'NONE',  ( 3.773127072069931032, 2.063069237518061705, -0.7396954945804237180 ) ) ;
#163651 = CARTESIAN_POINT ( 'NONE',  ( 6.010342169559767633, 5.906487374108180255, -0.7998128361456282587 ) ) ;
#163652 = CARTESIAN_POINT ( 'NONE',  ( 2.606376076552410659, 2.069701014239883730, 0.05521581806712527740 ) ) ;
#163654 = CARTESIAN_POINT ( 'NONE',  ( -1.364683531250014514, 1.551041667008084435, -0.7879004041258289570 ) ) ;
#163653 = CARTESIAN_POINT ( 'NONE',  ( 1.608462485350599769, 8.735270501766756013, -2.463594439587629914 ) ) ;
#163655 = ORIENTED_EDGE ( 'NONE', *, *, #210859, .T. ) ;
#163656 = CARTESIAN_POINT ( 'NONE',  ( 3.604340556743702795, -0.1682163741436558391, 2.292568252494499692 ) ) ;
#163657 = CARTESIAN_POINT ( 'NONE',  ( 8.432808358020029260, 8.940623960552603222, 0.7216878364870438212 ) ) ;
#163659 = CARTESIAN_POINT ( 'NONE',  ( -3.285556943749998737, -0.7802083328553744979, 1.896917185911908499 ) ) ;
#163658 = CARTESIAN_POINT ( 'NONE',  ( 6.875393295905841917, 7.193916064744513506, 0.000000000000000000 ) ) ;
#163660 = CARTESIAN_POINT ( 'NONE',  ( 6.720655732516701342, 6.039000170257122768, 2.421169367564251385 ) ) ;
#163661 = CARTESIAN_POINT ( 'NONE',  ( -6.994027139803241866, 9.253060644560830994, -1.599625672291271394 ) ) ;
#163662 = CARTESIAN_POINT ( 'NONE',  ( 3.995986895217980894, -0.6101256969637807170, -1.843678354830182053 ) ) ;
#163663 = ORIENTED_EDGE ( 'NONE', *, *, #214161, .F. ) ;
#163664 = CARTESIAN_POINT ( 'NONE',  ( 8.703971429848968100, 13.09845773489176679, 0.000000000000000000 ) ) ;
#163665 = CARTESIAN_POINT ( 'NONE',  ( 3.726736447152957599, 1.348887845406310682, -1.355897031963343213 ) ) ;
#163666 = CARTESIAN_POINT ( 'NONE',  ( 7.898971854500432636E-16, 4.000000000000003553, -6.450000000000003730 ) ) ;
#163667 = CARTESIAN_POINT ( 'NONE',  ( 5.069259022003644866, 0.1660796517843898534, -1.716765078168249969 ) ) ;
#163668 = CARTESIAN_POINT ( 'NONE',  ( 4.680875185974167074, 1.673856063443099673, -1.124242729735332347 ) ) ;
#163669 = CARTESIAN_POINT ( 'NONE',  ( 4.869944851454918400, -0.2802274231045227548, -2.281517807288702127 ) ) ;
#163670 = CARTESIAN_POINT ( 'NONE',  ( 0.7500000000000006661, 11.08333333333333393, 1.299038105676657340 ) ) ;
#163671 = CARTESIAN_POINT ( 'NONE',  ( 0.9267433102794273569, 1.311770220233858586, -1.774563083084364834 ) ) ;
#163673 = CARTESIAN_POINT ( 'NONE',  ( -4.502716413514310290, 6.346531463890372926, -1.443375672974066548 ) ) ;
#163672 = CARTESIAN_POINT ( 'NONE',  ( -10.64045162862669081, 11.30828174301964140, -0.7998128361456221525 ) ) ;
#163674 = CARTESIAN_POINT ( 'NONE',  ( 6.046140008783082109, 1.767849252625730783, 0.08484812824352709615 ) ) ;
#163676 = CARTESIAN_POINT ( 'NONE',  ( 1.517954844142660464, -1.276539353255158105, -1.903739821206115623 ) ) ;
#163675 = CARTESIAN_POINT ( 'NONE',  ( 6.900173834712277632, 7.014900660111269559, -0.7998128361456341429 ) ) ;
#163677 = CARTESIAN_POINT ( 'NONE',  ( 0.8842106040080777163, 1.536738824236941747, -0.8168212061390681678 ) ) ;
#163678 = CIRCLE ( 'NONE', #66678, 0.08000000000000001554 ) ;
#163679 = CARTESIAN_POINT ( 'NONE',  ( 6.316381784907311392, 2.043361914081378128, 0.7923855730916643525 ) ) ;
#163680 = CARTESIAN_POINT ( 'NONE',  ( 0.6492036743409674848, -0.2036512653956819019, -1.721755200737408842 ) ) ;
#163681 = CARTESIAN_POINT ( 'NONE',  ( 0.6801582343749847936, 0.5052083336747614783, 1.178068619123803451 ) ) ;
#163682 = CARTESIAN_POINT ( 'NONE',  ( -11.86145016429273014, 13.40000000000000036, -1.100000000000000533 ) ) ;
#163683 = CARTESIAN_POINT ( 'NONE',  ( 0.8366658991775147713, -1.206067806592339142, 1.805196218089277549 ) ) ;
#163684 = CARTESIAN_POINT ( 'NONE',  ( 2.079314900164643820, 1.561883299538204151, 1.275554356156020308 ) ) ;
#163685 = CARTESIAN_POINT ( 'NONE',  ( -1.500000000000013101, 0.2020833340161521663, 0.8660254037844403729 ) ) ;
#163686 = CARTESIAN_POINT ( 'NONE',  ( 5.496683133134654398, -0.4700625557551000866, -1.868158488084943780 ) ) ;
#163687 = CARTESIAN_POINT ( 'NONE',  ( -1.364683531250014514, 12.58854166700806054, -0.7879004041258335089 ) ) ;
#163688 = CARTESIAN_POINT ( 'NONE',  ( 1.758359454726521998, 0.8447074013377148249, -2.054735579953733904 ) ) ;
#163689 = ORIENTED_EDGE ( 'NONE', *, *, #138377, .T. ) ;
#163690 = CARTESIAN_POINT ( 'NONE',  ( -9.578932859269652766, -9.985077769980607698, 0.1209251627559742304 ) ) ;
#163691 = CARTESIAN_POINT ( 'NONE',  ( 0.000000000000000000, 2.800000000000024691, 1.214306433183764966E-14 ) ) ;
#163692 = CARTESIAN_POINT ( 'NONE',  ( 9.402743226277308963, 10.92862083786708816, -1.199719254218446718 ) ) ;
#163693 = DIRECTION ( 'NONE',  ( 0.000000000000000000, 0.000000000000000000, 1.000000000000000000 ) ) ;
#163694 = CARTESIAN_POINT ( 'NONE',  ( -10.50000000000000000, 10.19999999999998153, 3.599999999999999201 ) ) ;
#163695 = CARTESIAN_POINT ( 'NONE',  ( 5.601031023413125531, -0.4148525734360584138, 1.690157204064596019 ) ) ;
#163696 = CARTESIAN_POINT ( 'NONE',  ( 3.174217076811707727, -0.9646401420641316227, -1.708233030250068785 ) ) ;
#163698 = CARTESIAN_POINT ( 'NONE',  ( -7.049876689426113785, 8.287572894827684777, -1.082531754730544860 ) ) ;
#163697 = CARTESIAN_POINT ( 'NONE',  ( 3.635557746758808495, 7.393234471193928847, -0.7998128361456291469 ) ) ;
#163699 = CARTESIAN_POINT ( 'NONE',  ( -1.367350270964193371, 4.283378765250654752, -0.2578043790911884736 ) ) ;
#163700 = CARTESIAN_POINT ( 'NONE',  ( 4.692800188189328203, -0.4894541170284586462, -2.208696565397149314 ) ) ;
#163701 = AXIS2_PLACEMENT_3D ( 'NONE', #137352, #35550, #151460 ) ;
#163702 = STYLED_ITEM ( 'NONE', ( #163386 ), #111806 ) ;
#163703 = CARTESIAN_POINT ( 'NONE',  ( 1.504421023514388889, 2.060217768730878696, 0.1034037034779722308 ) ) ;
#163704 = CARTESIAN_POINT ( 'NONE',  ( -7.369020184227459858, 8.555943955475521889, 1.199719254218450271 ) ) ;
#163705 = CARTESIAN_POINT ( 'NONE',  ( 2.747247497433321861, -1.881545503785379436, 1.256212651835092231 ) ) ;
#163706 = EDGE_LOOP ( 'NONE', ( #100250, #207499, #76437, #79730 ) ) ;
#163707 = CARTESIAN_POINT ( 'NONE',  ( -0.7500000000000215383, 1.222916667349485564, 1.299038105676659116 ) ) ;
#163708 = CARTESIAN_POINT ( 'NONE',  ( 2.741296213614560440, -1.383352855433259698, -1.259238407996167153 ) ) ;
#163709 = CARTESIAN_POINT ( 'NONE',  ( 1.775574910200255818, 1.508776774498999718, -0.8547552410581791271 ) ) ;
#163710 = CARTESIAN_POINT ( 'NONE',  ( 5.566036750361066154, -1.391122746885119499, 1.693456055751572986 ) ) ;
#163711 = CARTESIAN_POINT ( 'NONE',  ( 0.07755575628183573877, -0.002876890934064984650, -2.188974970840869005 ) ) ;
#163712 = CARTESIAN_POINT ( 'NONE',  ( 3.801785103514757846, -0.6297183656660889639, 2.067937956787009757 ) ) ;
#163713 = CARTESIAN_POINT ( 'NONE',  ( 4.189351911999553479, -0.7420460110593477543, 1.794775118790333135 ) ) ;
#163714 = CARTESIAN_POINT ( 'NONE',  ( -8.455481356417053007, 13.01647868246193518, 0.7998128361456341429 ) ) ;
#163715 = CARTESIAN_POINT ( 'NONE',  ( 6.626239551081194001, 1.076695052409048614, -1.529385127534782951 ) ) ;
#163716 = CARTESIAN_POINT ( 'NONE',  ( 2.125000000000001332, -2.052068128417950277, 1.216660472349556312E-13 ) ) ;
#163717 = CARTESIAN_POINT ( 'NONE',  ( 4.006694938150886287, 7.586369203660299654, 0.2279062292016853508 ) ) ;
#163718 = CARTESIAN_POINT ( 'NONE',  ( -1.214306433183764966E-14, 3.299999999999969624, -3.122502256758252770E-14 ) ) ;
#163719 = CARTESIAN_POINT ( 'NONE',  ( 1.360316468749965590, 2.494791667008093849, 0.7853790794158861388 ) ) ;
#163721 = CARTESIAN_POINT ( 'NONE',  ( 5.977185442992979603, -2.006959616289708315, -0.1948445219252663840 ) ) ;
#163720 = CIRCLE ( 'NONE', #59951, 11.09999999999999964 ) ;
#163722 = CARTESIAN_POINT ( 'NONE',  ( -2.887523529586332405, 5.352232636950553513, 1.082531754730560403 ) ) ;
#163723 = CARTESIAN_POINT ( 'NONE',  ( 9.108380270282433244, 9.520865158284665952, 1.040834085586084257E-14 ) ) ;
#163724 = CARTESIAN_POINT ( 'NONE',  ( 4.848976215542928792, 5.686169002002086970, 1.199719254218452047 ) ) ;
#163725 = CARTESIAN_POINT ( 'NONE',  ( 3.141029808440584326, -1.609794727316344209, 0.8612202190056221784 ) ) ;
#163726 = CARTESIAN_POINT ( 'NONE',  ( 11.48243876534946217, 13.79999999999999893, -3.200000000000001510 ) ) ;
#163727 = ORIENTED_EDGE ( 'NONE', *, *, #49388, .T. ) ;
#163728 = CARTESIAN_POINT ( 'NONE',  ( -4.733205024502264102, 7.575804057677677505, 1.082531754730549967 ) ) ;
#163729 = DIRECTION ( 'NONE',  ( 0.000000000000000000, 8.546850786086437571E-32, 1.000000000000000000 ) ) ;
#163730 = CARTESIAN_POINT ( 'NONE',  ( -8.833300774503376473, 10.26427131079744193, 1.199719254218462483 ) ) ;
#163731 = CARTESIAN_POINT ( 'NONE',  ( 0.07057728186875102117, 0.7769860399358395897, 1.864564603342239835 ) ) ;
#163732 = CARTESIAN_POINT ( 'NONE',  ( 1.489100733002651555, -2.014586327357254181, -0.6619970261998938676 ) ) ;
#163733 = CIRCLE ( 'NONE', #84089, 10.25000000000000000 ) ;
#163734 = VERTEX_POINT ( 'NONE', #33148 ) ;
#163735 = CARTESIAN_POINT ( 'NONE',  ( -5.798046968499580345, 6.793418213784815585, 1.199719254218452935 ) ) ;
#163736 = CARTESIAN_POINT ( 'NONE',  ( 3.194917754314666514, 6.879154480009089134, 0.7998128361456321445 ) ) ;
#163737 = CARTESIAN_POINT ( 'NONE',  ( 6.350472301779563900, 0.6441285046014081361, 1.957720813820832850 ) ) ;
#163738 = CARTESIAN_POINT ( 'NONE',  ( 6.188124994278806135, 1.678003296889327034, 1.117835524071027598 ) ) ;
#163739 = VERTEX_POINT ( 'NONE', #47297 ) ;
#163740 = ORIENTED_EDGE ( 'NONE', *, *, #100809, .F. ) ;
#163741 =( BOUNDED_CURVE ( )  B_SPLINE_CURVE ( 2, ( #20981, #166193, #36184, #168334, #86015, #185630, #37263, #103333, #87078 ),
 .UNSPECIFIED., .F., .T. ) 
 B_SPLINE_CURVE_WITH_KNOTS ( ( 3, 2, 2, 2, 3 ),
 ( 0.4017857142857143016, 0.4047619047619047672, 0.4107142857142856984, 0.4166666666666666852, 0.4196428571428570953 ),
 .UNSPECIFIED. ) 
 CURVE ( )  GEOMETRIC_REPRESENTATION_ITEM ( )  RATIONAL_B_SPLINE_CURVE ( ( 0.9330127018922194093, 0.9330127018922194093, 1.000000000000000000, 0.8660254037844387076, 1.000000000000000000, 0.8660254037844387076, 1.000000000000000000, 0.9330127018922206306, 0.9330127018922194093 ) ) 
 REPRESENTATION_ITEM ( '' )  );
#163742 = CARTESIAN_POINT ( 'NONE',  ( -10.48453286206953727, 11.12637651536962125, 0.7998128361456462443 ) ) ;
#163743 = CARTESIAN_POINT ( 'NONE',  ( 7.506374323821472849, 8.786466794993730289, -1.199719254218452047 ) ) ;
#163746 = VERTEX_POINT ( 'NONE', #178355 ) ;
#163745 = SPHERICAL_SURFACE ( 'NONE', #193218, 0.05000000000000000278 ) ;
#163744 = CARTESIAN_POINT ( 'NONE',  ( -5.550083779947821760, 7.568460058062819407, -1.599625672291271394 ) ) ;
#163747 = CARTESIAN_POINT ( 'NONE',  ( 6.333059215844621725, 6.948315255594014417, 0.8781869475623119703 ) ) ;
#163748 = CARTESIAN_POINT ( 'NONE',  ( 6.714220164357198151, -1.617572894677368422, -1.203167480739217643 ) ) ;
#163749 = CARTESIAN_POINT ( 'NONE',  ( 4.576008823784957436, -1.786506429242448624, -0.4446734633927542091 ) ) ;
#163750 = FACE_OUTER_BOUND ( 'NONE', #207255, .T. ) ;
#163751 = CARTESIAN_POINT ( 'NONE',  ( 3.088805445243738568, -2.273621702497233166, -0.3942619731671925254 ) ) ;
#163752 = CARTESIAN_POINT ( 'NONE',  ( 5.505492895601038938, 8.580769590579979678, -1.199719254218452047 ) ) ;
#163753 = CARTESIAN_POINT ( 'NONE',  ( 5.677088005223024147, -0.04676544374488527528, -2.161250967910962828 ) ) ;
#163754 = CARTESIAN_POINT ( 'NONE',  ( 7.365103760721646076, 9.615707025640515937, 1.599625672291281386 ) ) ;
#163755 = CARTESIAN_POINT ( 'NONE',  ( 0.9603743489425471402, -1.756279846738018291, -0.8291483874790173125 ) ) ;
#163756 = ADVANCED_FACE ( 'NONE', ( #13691 ), #50465, .F. ) ;
#163757 = CARTESIAN_POINT ( 'NONE',  ( -5.135841261478327979, 4.886236314679810455, 0.7998128361456341429 ) ) ;
#163758 = ORIENTED_EDGE ( 'NONE', *, *, #122192, .T. ) ;
#163759 = ADVANCED_FACE ( 'NONE', ( #97114 ), #14751, .F. ) ;
#163760 = CARTESIAN_POINT ( 'NONE',  ( 4.358954191739877082, -0.8846011062542002978, 2.121510506163324372 ) ) ;
#163761 = LINE ( 'NONE', #111871, #169146 ) ;
#163762 = CARTESIAN_POINT ( 'NONE',  ( -3.955946960137363799, 7.837298230127379917, 0.7998128361456352531 ) ) ;
#163763 = CARTESIAN_POINT ( 'NONE',  ( 3.467518583331068438, 1.825290416974333807, -0.4087457676540603990 ) ) ;
#163766 = CARTESIAN_POINT ( 'NONE',  ( -6.424584688029276514, 8.588711117491191871, 1.599625672291269396 ) ) ;
#163765 = CARTESIAN_POINT ( 'NONE',  ( -1.500000000000015099, -0.3395833326505143801, -0.8660254037844383745 ) ) ;
#163764 = CARTESIAN_POINT ( 'NONE',  ( 0.9141475326900462273, -1.912571728325639153, 0.002704284578637640348 ) ) ;
#163767 = CARTESIAN_POINT ( 'NONE',  ( 3.211752199052122503, -0.4303563718574507369, 2.164345902561148005 ) ) ;
#163768 = CARTESIAN_POINT ( 'NONE',  ( -1.569519686357809585, 8.730458328474719920, -2.495327313682848214 ) ) ;
#163769 = FACE_OUTER_BOUND ( 'NONE', #134408, .T. ) ;
#163770 = CARTESIAN_POINT ( 'NONE',  ( 5.519577934094840543, 9.453608333170423705, 0.7216878364870317197 ) ) ;
#163771 = CARTESIAN_POINT ( 'NONE',  ( -3.460355519985875983, 5.060167411448709629, 1.599625672291267398 ) ) ;
#163772 = CARTESIAN_POINT ( 'NONE',  ( -5.600926855776877211, 9.548515408466085930, -0.7216878364870338292 ) ) ;
#163773 = CARTESIAN_POINT ( 'NONE',  ( 0.7902269029948695289, -1.955937164205447054, -0.2457751801602201802 ) ) ;
#163774 = CARTESIAN_POINT ( 'NONE',  ( 1.642099192286674336, -1.672607260348612845, -1.589979871525433408 ) ) ;
#163775 = CARTESIAN_POINT ( 'NONE',  ( 1.363640982571033611, -0.4799814350611387725, 1.902108589862220311 ) ) ;
#163776 = CARTESIAN_POINT ( 'NONE',  ( 5.243062877513432696, -0.2472539590166565604, -2.047610945800168114 ) ) ;
#163777 = CARTESIAN_POINT ( 'NONE',  ( 3.714570900464269076, 7.277490450609545469, 0.7216878364870298324 ) ) ;
#163778 = CARTESIAN_POINT ( 'NONE',  ( 4.505052181490820651, 8.477920988373101707, -0.7998128361456381397 ) ) ;
#163779 = ORIENTED_EDGE ( 'NONE', *, *, #156034, .F. ) ;
#163780 = CARTESIAN_POINT ( 'NONE',  ( 0.6823417656249917140, 5.405208333674749177, 1.181850606188765695 ) ) ;
#163781 = CARTESIAN_POINT ( 'NONE',  ( 10.87247189006428272, -6.708723052947949128, -0.1888596022590607604 ) ) ;
#163782 = CARTESIAN_POINT ( 'NONE',  ( 3.917943204224906939, 5.594019709727598766, -1.443375672974051449 ) ) ;
#163783 = CARTESIAN_POINT ( 'NONE',  ( 1.340952317110634118, -2.117647682651255803, -0.4779334406839957916 ) ) ;
#163785 = CARTESIAN_POINT ( 'NONE',  ( 6.321814700078944860, 1.054209175812788502, -1.509406368332133930 ) ) ;
#163784 = CARTESIAN_POINT ( 'NONE',  ( -11.86145016429273191, 13.40000000000000036, 1.099999999999996758 ) ) ;
#163786 = CARTESIAN_POINT ( 'NONE',  ( 6.381095703207991576, -8.233137084989849086, 7.037870247915948063 ) ) ;
#163787 = CARTESIAN_POINT ( 'NONE',  ( -3.615586099537422271, 3.576626764850541651, -2.500000000000000444 ) ) ;
#163788 = CARTESIAN_POINT ( 'NONE',  ( 1.176777557245082262, -0.04011917365428705612, -1.870279424122413658 ) ) ;
#163789 = CARTESIAN_POINT ( 'NONE',  ( 5.677088005223024147, -0.04676544374488527528, -2.161250967910962828 ) ) ;
#163790 = CARTESIAN_POINT ( 'NONE',  ( -5.702738293170157569, 6.277038442308466415, 1.111922112425635989 ) ) ;
#163791 = CARTESIAN_POINT ( 'NONE',  ( 10.91804383151480096, -9.900000000000005684, -0.1905751639681742271 ) ) ;
#163792 = EDGE_CURVE ( 'NONE', #162623, #40788, #75860, .T. ) ;
#163793 = CARTESIAN_POINT ( 'NONE',  ( 0.6823417656249882723, -0.1572916663252488245, 1.181850606188755259 ) ) ;
#163794 = CARTESIAN_POINT ( 'NONE',  ( 2.754443878939544454, 1.898071056134968959, 0.2320119769325945103 ) ) ;
#163795 = AXIS2_PLACEMENT_3D ( 'NONE', #144535, #198544, #131488 ) ;
#163796 = CARTESIAN_POINT ( 'NONE',  ( 2.588433964080754546, -0.3000524435079615637, -1.744042203426913629 ) ) ;
#163797 = CARTESIAN_POINT ( 'NONE',  ( 0.5922591856823838929, -1.062013159134197693, 1.590055880637729402 ) ) ;
#163798 = AXIS2_PLACEMENT_3D ( 'NONE', #5753, #85977, #102226 ) ;
#163800 = CARTESIAN_POINT ( 'NONE',  ( 5.958580499074456860, -1.820587016788511647, -0.5960958187592230173 ) ) ;
#163799 = CARTESIAN_POINT ( 'NONE',  ( 7.439168848973994663, -6.893137084989842123, 8.103009739378013165 ) ) ;
#163801 = CARTESIAN_POINT ( 'NONE',  ( 6.355907380368630122, -0.6650989860433678125, 1.853973344504164622 ) ) ;
#163802 = CARTESIAN_POINT ( 'NONE',  ( 0.7499999999999902300, 4.816666666666684193, -1.299038105676658228 ) ) ;
#163803 = CARTESIAN_POINT ( 'NONE',  ( 1.353939357992512305, -1.539690173578952770, -1.458446627980537480 ) ) ;
#163804 = CARTESIAN_POINT ( 'NONE',  ( 5.051181283347249362, 7.973588670567067105, -1.225461877896296681 ) ) ;
#163805 = CARTESIAN_POINT ( 'NONE',  ( 4.838664814796108438, 0.3202261158844340594, 1.842872994462002367 ) ) ;
#163807 = ORIENTED_EDGE ( 'NONE', *, *, #162856, .F. ) ;
#163806 = CARTESIAN_POINT ( 'NONE',  ( 0.9788029507734037349, -0.04229004422508231970, -1.825371421953936757 ) ) ;
#163809 = DIRECTION ( 'NONE',  ( -0.5773502691896238437, 0.000000000000000000, 0.8164965809277274778 ) ) ;
#163808 = CARTESIAN_POINT ( 'NONE',  ( 4.073040751519330094, -2.058760688187323495, -0.7953439701907027981 ) ) ;
#163810 = CARTESIAN_POINT ( 'NONE',  ( -1.364683531250010295, 4.092708333674751842, 0.7879004041258379498 ) ) ;
#163811 = CARTESIAN_POINT ( 'NONE',  ( 2.119651477787509730, 0.3549358516394903740, -2.031769927719127455 ) ) ;
#163812 = CARTESIAN_POINT ( 'NONE',  ( 5.178324605415663306, 8.128796908705222535, 1.199719254218462483 ) ) ;
#163813 = CARTESIAN_POINT ( 'NONE',  ( -8.864333505236459132, 9.236143932397675727, 1.040834085586084257E-14 ) ) ;
#163814 = FACE_OUTER_BOUND ( 'NONE', #129297, .T. ) ;
#163815 = CARTESIAN_POINT ( 'NONE',  ( -3.423013188325464640, -0.02164107303108744884, -0.4185776113819570377 ) ) ;
#163816 = CARTESIAN_POINT ( 'NONE',  ( 6.481679955784983349, 9.719654494127929922, -1.199719254218452047 ) ) ;
#163817 = ORIENTED_EDGE ( 'NONE', *, *, #97172, .T. ) ;
#163818 = CARTESIAN_POINT ( 'NONE',  ( 4.070807014193541740, 1.466255041752505539, -1.461937513464212079 ) ) ;
#163819 = CARTESIAN_POINT ( 'NONE',  ( 0.7499999999999920064, 5.483333333333353821, 1.299038105676669330 ) ) ;
#163820 = CARTESIAN_POINT ( 'NONE',  ( 1.651884467337715989, 0.6291892518628816600, -2.067965918892029631 ) ) ;
#163821 = B_SPLINE_CURVE_WITH_KNOTS ( 'NONE', 3,
 ( #23509, #205462, #74418, #43003, #76533, #174073 ),
 .UNSPECIFIED., .F., .F.,
 ( 4, 2, 4 ),
 ( 0.000000000000000000, 0.0003239988925529258120, 0.0006479977851058516241 ),
 .UNSPECIFIED. ) ;
#163822 = CARTESIAN_POINT ( 'NONE',  ( -5.902949979233523159, 7.165898849449257924, -1.132310321155009847 ) ) ;
#163823 = CARTESIAN_POINT ( 'NONE',  ( 1.752609234595727816, 1.998021763388730720, 0.2939949305936078172 ) ) ;
#163824 = CARTESIAN_POINT ( 'NONE',  ( -6.773376349083143566, -7.473374494058229622, -6.661184041420940005 ) ) ;
#163825 = VERTEX_POINT ( 'NONE', #182579 ) ;
#163826 = ADVANCED_FACE ( 'NONE', ( #80843 ), #31089, .F. ) ;
#163828 = CARTESIAN_POINT ( 'NONE',  ( 7.782016984564060103, 9.141736572488651902, 1.082531754730558626 ) ) ;
#163827 = CARTESIAN_POINT ( 'NONE',  ( -3.474999999999998312, -2.770833333333333037, 2.006292185433951047 ) ) ;
#163829 = CARTESIAN_POINT ( 'NONE',  ( 0.2977236940312242286, -5.250949308401983373, 10.97067990664316284 ) ) ;
#163830 = CARTESIAN_POINT ( 'NONE',  ( 0.4972802279516430612, -0.2910764605805628014, 1.995268990643041640 ) ) ;
#163831 = CARTESIAN_POINT ( 'NONE',  ( 4.528971853086540378, -2.003544689622422936, 0.8885388601788182239 ) ) ;
#163832 = CARTESIAN_POINT ( 'NONE',  ( 1.499999999999990896, 4.806250000682819490, 1.214306433183764966E-14 ) ) ;
#163833 = CARTESIAN_POINT ( 'NONE',  ( 3.498220628606643956, -0.9384276995785534314, 1.666209768436441419 ) ) ;
#163834 = CARTESIAN_POINT ( 'NONE',  ( -5.278201874421821316, 5.052323696447222900, 0.7998128361456341429 ) ) ;
#163835 = CARTESIAN_POINT ( 'NONE',  ( 4.975479186090839612, 8.748550117173898855, 0.7216878364870438212 ) ) ;
#163837 = CARTESIAN_POINT ( 'NONE',  ( 2.073842424929934314, -0.8596134062341630466, 1.824128527830502833 ) ) ;
#163836 = CARTESIAN_POINT ( 'NONE',  ( -9.070041577417988776, 12.56517035942090388, 1.082531754730558626 ) ) ;
#163838 = CARTESIAN_POINT ( 'NONE',  ( 0.6823417656249969321, 11.83854166700806765, -1.181850606188757036 ) ) ;
#163840 = CARTESIAN_POINT ( 'NONE',  ( -6.050681693448748177, 10.28115541899069463, 0.7998128361456291469 ) ) ;
#163839 = CARTESIAN_POINT ( 'NONE',  ( 0.7324523162463879578, 2.259705603777485639, 0.3848113418177290801 ) ) ;
#163841 = CARTESIAN_POINT ( 'NONE',  ( 3.785938739704467260, -0.8500231715772713637, 1.500685565699668933 ) ) ;
#163842 = DIRECTION ( 'NONE',  ( 1.000000000000000000, -7.387867266669436732E-31, 0.000000000000000000 ) ) ;
#163843 = CARTESIAN_POINT ( 'NONE',  ( 4.792970997630896512, 5.550553237779539018, 1.199719254218464037 ) ) ;
#163844 = CARTESIAN_POINT ( 'NONE',  ( 0.000000000000000000, 0.5999999999999998668, 0.000000000000000000 ) ) ;
#163845 = EDGE_CURVE ( 'NONE', #213513, #175384, #50169, .T. ) ;
#163846 = CARTESIAN_POINT ( 'NONE',  ( 0.07536363704233049743, 0.2309889609098912111, -2.177957698420322163 ) ) ;
#163847 = ORIENTED_EDGE ( 'NONE', *, *, #120283, .T. ) ;
#163848 = CARTESIAN_POINT ( 'NONE',  ( 0.4442981077158770775, -0.9790059121952739973, 1.824179074426744762 ) ) ;
#163849 = EDGE_LOOP ( 'NONE', ( #31338, #17623, #170078, #14979 ) ) ;
#163850 = CARTESIAN_POINT ( 'NONE',  ( 4.916585655956178691, -0.6154711373431708266, -1.703840371469134807 ) ) ;
#163851 = ORIENTED_EDGE ( 'NONE', *, *, #119054, .T. ) ;
#163852 = CARTESIAN_POINT ( 'NONE',  ( 3.854260808034858155, 7.718664386007802136, -0.7998128361456362523 ) ) ;
#163853 = CYLINDRICAL_SURFACE ( 'NONE', #25000, 4.500000000000000000 ) ;
#163854 = CARTESIAN_POINT ( 'NONE',  ( 6.024035747493574178, -1.796918165027236780, 0.2286857708345239326 ) ) ;
#163855 = CARTESIAN_POINT ( 'NONE',  ( 6.983858524370782916, 7.320458831286981827, 0.7216878364870328300 ) ) ;
#163856 = DIRECTION ( 'NONE',  ( 0.000000000000000000, 1.000000000000000000, 0.000000000000000000 ) ) ;
#163857 = CARTESIAN_POINT ( 'NONE',  ( 3.504031732436951874, -0.8880451304637152488, -2.003635182500095535 ) ) ;
#163859 = CARTESIAN_POINT ( 'NONE',  ( 7.865701674222579598, 12.32840238656838139, -0.7998128361456352531 ) ) ;
#163858 = CARTESIAN_POINT ( 'NONE',  ( 6.250447302982959030, -1.852220608400175994, -0.1812639614414724432 ) ) ;
#163860 = VECTOR ( 'NONE', #51090, 1000.000000000000000 ) ;
#163861 = CARTESIAN_POINT ( 'NONE',  ( 3.497576124367638872, -1.886684243562693597, 0.3306681954469546936 ) ) ;
#163862 = MECHANICAL_DESIGN_GEOMETRIC_PRESENTATION_REPRESENTATION (  '', ( #46201 ), #115500 ) ;
#163863 = CARTESIAN_POINT ( 'NONE',  ( 5.602074566136501232, 5.729665287594564838, 0.6253354971682704155 ) ) ;
#163864 = CARTESIAN_POINT ( 'NONE',  ( -0.7500000000000006661, 11.95833333333333393, -1.299038105676657340 ) ) ;
#163865 = CARTESIAN_POINT ( 'NONE',  ( -1.364683531250000748, -0.2406249996585799189, 0.000000000000000000 ) ) ;
#163866 = CIRCLE ( 'NONE', #153487, 0.08000000000000020983 ) ;
#163867 = CARTESIAN_POINT ( 'NONE',  ( 4.500943810056890371, 8.194925511800951412, -0.7216878364870207285 ) ) ;
#163868 = EDGE_CURVE ( 'NONE', #52032, #47959, #174103, .T. ) ;
#163869 = CARTESIAN_POINT ( 'NONE',  ( -10.33094986393327197, 11.15512238411806578, 0.7216878364870438212 ) ) ;
#163870 = CARTESIAN_POINT ( 'NONE',  ( 0.3038912542124502236, -0.5749842496362895794, 2.083749421223294540 ) ) ;
#163871 = CARTESIAN_POINT ( 'NONE',  ( -4.261005416444848315, 8.193199762486115034, 0.7998128361456352531 ) ) ;
#163872 = CARTESIAN_POINT ( 'NONE',  ( 3.555981428534177091, 7.370671776590375757, 0.7998128361456271485 ) ) ;
#163873 = CARTESIAN_POINT ( 'NONE',  ( 2.326929888710258965, -0.002694909042751796133, 1.825762228105472840 ) ) ;
#163874 = CARTESIAN_POINT ( 'NONE',  ( -5.427341564172148303, 5.226320001155936090, 0.000000000000000000 ) ) ;
#163875 = EDGE_CURVE ( 'NONE', #69052, #120928, #97271, .T. ) ;
#163876 = CARTESIAN_POINT ( 'NONE',  ( 3.838725952263983388, 0.2674066485093031242, 1.805754746396167176 ) ) ;
#163877 = CIRCLE ( 'NONE', #142709, 0.07999999999999961309 ) ;
#163878 = CARTESIAN_POINT ( 'NONE',  ( 9.704905176613070950, 13.32621205788646002, -8.135614888031417635 ) ) ;
#163879 = CARTESIAN_POINT ( 'NONE',  ( 2.461071540317420592, -1.587761714688111780, 1.065645112462119570 ) ) ;
#163880 = EDGE_LOOP ( 'NONE', ( #96477, #85541, #128367, #13075 ) ) ;
#163881 = CARTESIAN_POINT ( 'NONE',  ( 2.348051406654600104, -0.8447338538565999366, 1.779358369178071886 ) ) ;
#163882 = ORIENTED_EDGE ( 'NONE', *, *, #59071, .F. ) ;
#163883 = CARTESIAN_POINT ( 'NONE',  ( 4.862805241732807815, 0.1868221656222105176, -1.933040885264789122 ) ) ;
#163884 = EDGE_LOOP ( 'NONE', ( #211863, #10797, #142547, #32538 ) ) ;
#163885 = CARTESIAN_POINT ( 'NONE',  ( -6.668631453075260396, 8.873432343378178544, -1.599625672291271394 ) ) ;
#163887 = CARTESIAN_POINT ( 'NONE',  ( 5.730757696090861941, 1.422813033107739988, -1.572628729999878905 ) ) ;
#163886 = CARTESIAN_POINT ( 'NONE',  ( 5.182959862174088883, 9.268813282503625572, 0.7998128361456331437 ) ) ;
#163888 = CARTESIAN_POINT ( 'NONE',  ( 0.000000000000000000, 6.062865449010541141, 0.000000000000000000 ) ) ;
#163889 = CARTESIAN_POINT ( 'NONE',  ( 2.543496672408153358, -1.783599581865771500, 0.6900697577220117340 ) ) ;
#163890 = CARTESIAN_POINT ( 'NONE',  ( 5.142929413680796813, 6.687119857356774055, -1.406168165883972421 ) ) ;
#163891 = LINE ( 'NONE', #145539, #139313 ) ;
#163892 = CARTESIAN_POINT ( 'NONE',  ( 5.388439706788500594, 5.251210844200210559, 0.7998128361456352531 ) ) ;
#163893 = CARTESIAN_POINT ( 'NONE',  ( 3.876741858503734761, 6.610283703974623393, 1.199719254218462483 ) ) ;
#163894 = CARTESIAN_POINT ( 'NONE',  ( 4.037747573665031453, -1.925786081212683465, 0.5863696817766034242 ) ) ;
#163895 = CARTESIAN_POINT ( 'NONE',  ( 0.07971467182324797063, -9.904506264776385294, 9.499665578938850885 ) ) ;
#163896 = CARTESIAN_POINT ( 'NONE',  ( 5.232948167349782409, 0.1380416123818763163, 1.820529236867339584 ) ) ;
#163897 = CARTESIAN_POINT ( 'NONE',  ( 0.8540665308606997241, -0.7467690478978536994, 1.931163149162813619 ) ) ;
#163898 = CARTESIAN_POINT ( 'NONE',  ( -7.456621297836087514, 9.722477485607340597, 1.443375672974090751 ) ) ;
#163899 = CARTESIAN_POINT ( 'NONE',  ( -6.329738897986983304, 6.948428204275519882, 0.9008771187248975076 ) ) ;
#163900 = DIRECTION ( 'NONE',  ( -3.330669073875479482E-16, 3.330669073875479482E-16, 1.000000000000000000 ) ) ;
#163901 = CARTESIAN_POINT ( 'NONE',  ( 5.242975984329111050, -1.603930480038592510, 0.9624218375651683033 ) ) ;
#163902 = CARTESIAN_POINT ( 'NONE',  ( 6.612626235163189925, 8.737816579155630592, -1.599625672291262513 ) ) ;
#163903 = CARTESIAN_POINT ( 'NONE',  ( -4.948889764188092677, 5.732458465429559169, 1.199719254218462483 ) ) ;
#163904 = CARTESIAN_POINT ( 'NONE',  ( -1.364683531250000748, 10.17187500034139802, 0.000000000000000000 ) ) ;
#163905 = CARTESIAN_POINT ( 'NONE',  ( -5.436983294280064882, 6.301900917203534291, 1.199719254218450271 ) ) ;
#163907 = CARTESIAN_POINT ( 'NONE',  ( -3.594320120954326292, 6.247105003538398371, 1.082531754730549967 ) ) ;
#163906 = CARTESIAN_POINT ( 'NONE',  ( 3.171717870593107058, 5.787755718078879674, -1.199719254218446718 ) ) ;
#163908 = CARTESIAN_POINT ( 'NONE',  ( -4.841670253411603397, 5.781608396135871075, 1.082531754730549078 ) ) ;
#163909 = CARTESIAN_POINT ( 'NONE',  ( -6.552668314106420588, 6.539201209412602189, -0.7998128361456291469 ) ) ;
#163910 = CARTESIAN_POINT ( 'NONE',  ( 1.639598513223254006, 1.914365469054382540, -0.7886191548351070280 ) ) ;
#163911 = CARTESIAN_POINT ( 'NONE',  ( 2.407945773967453462, -1.221608841751795405, -1.729074501506906225 ) ) ;
#163912 = CARTESIAN_POINT ( 'NONE',  ( 10.05067194643221207, 10.62020544712608938, 0.7998128361456462443 ) ) ;
#163913 = CARTESIAN_POINT ( 'NONE',  ( 5.884182030513498086E-16, 2.999999999999988898, -1.225000000000007638 ) ) ;
#163914 = CARTESIAN_POINT ( 'NONE',  ( 6.977413707831522593, -0.1558467299303326059, 2.036386162850227333 ) ) ;
#163915 = CARTESIAN_POINT ( 'NONE',  ( 4.226642156305554288, 7.541242530477547668, 0.9646342093552334740 ) ) ;
#163916 = CARTESIAN_POINT ( 'NONE',  ( 6.005898861173831094, 6.109229547565340646, 1.040834085586084257E-14 ) ) ;
#163918 = CARTESIAN_POINT ( 'NONE',  ( -5.398914348987532641, 6.259949555863199677, -2.420000000000000373 ) ) ;
#163917 = CARTESIAN_POINT ( 'NONE',  ( 11.48243876534946217, 9.799999999999998934, -3.200000000000001510 ) ) ;
#163919 = CARTESIAN_POINT ( 'NONE',  ( 2.150677785613893889, -1.770481577899532644, 1.455972101185269985 ) ) ;
#163920 = CARTESIAN_POINT ( 'NONE',  ( -9.488641820551102057, -8.233137084989836652, 0.4644097342743139234 ) ) ;
#163921 = CARTESIAN_POINT ( 'NONE',  ( 2.267699027020404490, 0.5063876334258295975, -1.844086191983687062 ) ) ;
#163922 = ORIENTED_EDGE ( 'NONE', *, *, #163291, .F. ) ;
#163923 = CARTESIAN_POINT ( 'NONE',  ( 7.415946836550714849, 9.675023947441092176, 1.443375672974076540 ) ) ;
#163924 =( BOUNDED_CURVE ( )  B_SPLINE_CURVE ( 3, ( #18397, #84474, #2126, #30419 ),
 .UNSPECIFIED., .F., .T. ) 
 B_SPLINE_CURVE_WITH_KNOTS ( ( 4, 4 ),
 ( 0.5000000000000008882, 1.000000000000000000 ),
 .UNSPECIFIED. ) 
 CURVE ( )  GEOMETRIC_REPRESENTATION_ITEM ( )  RATIONAL_B_SPLINE_CURVE ( ( 0.9999999999999990008, 0.3333333333333334259, 0.3333333333333345916, 1.000000000000000222 ) ) 
 REPRESENTATION_ITEM ( '' )  );
#163925 = CARTESIAN_POINT ( 'NONE',  ( 0.5100215303667603450, -0.7206480643048470691, 1.879988510241884292 ) ) ;
#163926 = CARTESIAN_POINT ( 'NONE',  ( 0.9890223832832998330, 0.1386981244183866091, 1.956888703154149312 ) ) ;
#163927 = CARTESIAN_POINT ( 'NONE',  ( -9.378489572351046633, 11.96465713920816043, -1.599625672291263179 ) ) ;
#163928 = CARTESIAN_POINT ( 'NONE',  ( -6.353967546298838087, 10.56471257065732416, 0.000000000000000000 ) ) ;
#163929 = CARTESIAN_POINT ( 'NONE',  ( -11.63140583992382560, 7.361097535320459961, -2.771579487483898596 ) ) ;
#163931 = CARTESIAN_POINT ( 'NONE',  ( 2.342341949348641261, 0.3848992280063111004, 1.727307115810622351 ) ) ;
#163930 = CARTESIAN_POINT ( 'NONE',  ( 3.697287448106700403, -0.6068447087972194121, 2.000623839779874125 ) ) ;
#163932 = CARTESIAN_POINT ( 'NONE',  ( 1.387358672533593129, 7.315968950352074174, -4.254625267140469624 ) ) ;
#163934 = CARTESIAN_POINT ( 'NONE',  ( 5.121132688944100231, -2.177879115872250360, 0.7152381750462534216 ) ) ;
#163933 = CARTESIAN_POINT ( 'NONE',  ( -1.225000000000004086, 1.979166666666657193, -0.7072540797572898219 ) ) ;
#163935 = CARTESIAN_POINT ( 'NONE',  ( 4.452888953083543377, 0.3777208849818362579, -1.698664142626307383 ) ) ;
#163936 = B_SPLINE_CURVE_WITH_KNOTS ( 'NONE', 3,
 ( #193897, #192820, #96435, #211205, #128990, #14060, #80147, #76942, #146249, #60698, #196049, #48730, #209061, #44477, #113792, #179795, #97489, #114843, #176596, #94301, #180842, #49780, #82268, #132140, #70266, #33528, #184034, #85475, #998, #214361, #119109, #69199, #148362, #181892, #151562, #149416, #152611, #32467, #17254, #166737, #182972, #35649, #135319, #50849, #150499, #101728, #54052, #84411, #67062, #4196, #99599, #65991, #167799, #98537, #16185, #118048, #201333, #133199, #185091, #168860, #164599, #19395, #2060, #83330, #198147, #100661, #115906, #165665, #3129, #52972, #199202, #116975, #34588, #134266, #18328, #36716, #102802, #20462, #68132, #200272, #86546, #136381, #51924, #202399, #188301, #5257, #186165, #153688, #6339, #124472, #23666, #205614, #139588, #122345, #7407, #90835, #38867, #39941, #207752, #37799, #8486, #71334, #106050, #42089, #21508, #189377, #120189, #9560, #103874, #138511, #204536, #56185, #73488, #190430, #156898, #41020, #89776, #169923, #87617, #172074, #155822, #104950, #57252, #170990, #74571, #137449, #107128, #206686, #140672, #154755, #123413, #173151, #58316, #75636, #141744, #22589, #203465, #55119, #24733, #108203, #174226, #121266, #187239, #25802, #88697, #91911, #72411, #157969, #45277, #61510, #127675, #79881, #195778, #59379, #194702, #163283, #44215, #144936, #94041, #192560, #208807, #62566, #191494, #109275, #210941, #13810, #27945, #212003, #47416, #125535, #128730, #78812, #179537, #160080, #143878, #14866, #46343, #60438, #112459, #43162, #10612, #175284, #12738, #26870, #145991, #30080, #63642, #11682, #209871, #129799, #178470, #96172, #193635, #162223, #113531, #31156, #97229, #142803, #80955, #177402, #147047, #92973, #111398, #161150, #159018, #110336, #29017, #76688, #126597, #176339, #77756, #95102, #183781, #67863, #151301, #135062, #118850, #101468, #52717, #36463, #201075, #84149, #99347, #150234, #15929, #213069, #66794, #83071, #214107, #2871, #131881, #50584, #197890, #35391, #64699, #134011, #85214, #167538, #33264, #116707, #132933, #182707, #184832, #49519, #19137, #68941, #102538, #16994, #82013, #149148, #198940, #168601, #1805, #65734, #196837, #148104, #114594, #164341, #20203, #115640, #200018, #34326, #181636, #728, #86290, #51669, #117791, #100400, #130843, #48477, #180585, #32208, #165398, #98282, #166468, #18061, #202135, #186981, #37538, #89516, #6080, #154502, #25550, #3936, #40764, #173977, #153431, #123167, #7152, #90584, #74319, #58058, #106869, #206434, #190184, #140416, #122084, #23403, #38612, #155570, #169670, #152361, #53795, #72151, #188045, #88439, #105786, #189128, #138260, #73223, #54862, #70006, #121015, #204273, #39675, #136121, #124224, #55928, #41840, #203217, #172897, #21256, #185902, #171812, #137194, #24471, #139331, #156644, #205360, #119927, #56994, #8237, #107951, #103617, #87362, #5001, #71076, #104690, #170739, #22325, #194457, #207504, #92722, #62332, #60188, #66292, #157712, #142548, #77506, #93791, #159828, #112219, #16486, #91660, #12498, #198439, #76441, #177150, #126347, #10364, #26621, #94851, #9309, #141496, #28768, #46102, #192307, #32762, #82566, #75382, #160902, #111150, #220, #43967, #176094, #50085, #78571, #158768, #144691, #59124, #42906, #125281, #45037, #191243, #181140, #128491, #98842 ),
 .UNSPECIFIED., .F., .F.,
 ( 4, 1, 1, 1, 1, 1, 1, 1, 1, 1, 1, 1, 1, 1, 1, 1, 1, 1, 1, 1, 1, 1, 1, 1, 1, 1, 1, 1, 1, 1, 1, 1, 1, 1, 1, 1, 1, 1, 1, 1, 1, 1, 1, 1, 1, 1, 1, 1, 1, 1, 1, 1, 1, 1, 1, 1, 1, 1, 1, 1, 1, 1, 1, 1, 1, 1, 1, 1, 1, 1, 1, 1, 1, 1, 1, 1, 1, 1, 1, 1, 1, 1, 1, 1, 1, 1, 1, 1, 1, 1, 1, 1, 1, 1, 1, 1, 1, 1, 1, 1, 1, 1, 1, 1, 1, 1, 1, 1, 1, 1, 1, 1, 1, 1, 1, 1, 1, 1, 1, 1, 1, 1, 1, 1, 1, 1, 1, 1, 1, 1, 1, 1, 1, 1, 1, 1, 1, 1, 1, 1, 1, 1, 1, 1, 1, 1, 1, 1, 1, 1, 1, 1, 1, 1, 1, 1, 1, 1, 1, 1, 1, 1, 1, 1, 1, 1, 1, 1, 1, 1, 1, 1, 1, 1, 1, 1, 1, 1, 1, 1, 1, 1, 1, 1, 1, 1, 1, 1, 1, 1, 1, 1, 1, 1, 1, 1, 1, 1, 1, 1, 1, 1, 1, 1, 1, 1, 1, 1, 1, 1, 1, 1, 1, 1, 1, 1, 1, 1, 1, 1, 1, 1, 1, 1, 1, 1, 1, 1, 1, 1, 1, 1, 1, 1, 1, 1, 1, 1, 1, 1, 1, 1, 1, 1, 1, 1, 1, 1, 1, 1, 1, 1, 1, 1, 1, 1, 1, 1, 1, 1, 1, 1, 1, 1, 1, 1, 1, 1, 1, 1, 1, 1, 1, 1, 1, 1, 1, 1, 1, 1, 1, 1, 1, 1, 1, 1, 1, 1, 1, 1, 1, 1, 1, 1, 1, 1, 1, 1, 1, 1, 1, 1, 1, 1, 1, 1, 1, 1, 1, 1, 1, 1, 1, 1, 1, 1, 1, 1, 1, 1, 1, 1, 1, 1, 1, 1, 1, 1, 1, 1, 1, 1, 1, 1, 1, 1, 1, 1, 1, 1, 1, 1, 1, 1, 1, 1, 1, 1, 1, 1, 1, 1, 1, 1, 1, 1, 1, 1, 1, 1, 1, 1, 1, 1, 1, 1, 1, 1, 1, 1, 1, 1, 1, 1, 1, 1, 1, 1, 1, 1, 1, 1, 1, 1, 4 ),
 ( 0.000000000000000000, 0.002600154539856827565, 0.005208839490340733125, 0.007813275572638063438, 0.01041576435696154809, 0.01302135854728175661, 0.01562456786780599440, 0.01822932761385693060, 0.02083324874646079461, 0.02343713590986815087, 0.02604192363554110393, 0.02864519953128016536, 0.03125045858075606309, 0.03385359029894085409, 0.03645870005206112291, 0.03906221013386886737, 0.04166657361863843057, 0.04427092160485841116, 0.04687444683368256759, 0.04947954930481244379, 0.05208268618576387260, 0.05468794662449812799, 0.05729120536831356497, 0.05989601299138836571, 0.06249988999545372931, 0.06510378435733490954, 0.06770858081828938502, 0.07031184975024351580, 0.07291710771924506118, 0.07552024060328325905, 0.07812534933470290099, 0.08072885870519988516, 0.08333322157114708695, 0.08593756915452624434, 0.08854109358761537429, 0.09114619558392741960, 0.09374933183658358538, 0.09635459170495851156, 0.09895784999447977681, 0.1015626569530685003, 0.1041665336043751944, 0.1067704272253022224, 0.1093752232910748662, 0.1119784915631429623, 0.1145837490571069844, 0.1171868814509031548, 0.1197919896162490533, 0.1223954986480551566, 0.1249998608471283579, 0.1276042081199000311, 0.1302077318846941445, 0.1328128334964322199, 0.1354159692195129883, 0.1380212286176593917, 0.1406244865514671982, 0.1432292929439143159, 0.1458331693420142072, 0.1484370623210626572, 0.1510418580899855479, 0.1536451258019158050, 0.1562503829188521542, 0.1588535149221727560, 0.1614586226195926788, 0.1640621314121666618, 0.1666664930431534797, 0.1692708401040713406, 0.1718743633000545112, 0.1744794646253388370, 0.1770825999186152189, 0.1796878589445308205, 0.1822911166222762891, 0.1848959225469683498, 0.1874997987909985397, 0.1901036912273387502, 0.1927084867977703619, 0.1953117540492253223, 0.1979170108871138589, 0.2005201425997050479, 0.2031252499273119572, 0.2057287585800815777, 0.2083331197417381819, 0.2109374666895270922, 0.2135409894161511279, 0.2161460905530729892, 0.2187492255162853672, 0.2213544842679382729, 0.2239577417892439637, 0.2265625473445374016, 0.2291664235336075273, 0.2317703155263790282, 0.2343751109966507595, 0.2369783778872631419, 0.2395836345440564008, 0.2421867660656364940, 0.2447918731215153465, 0.2473953817338825356, 0.2499997425249363969, 0.2526040894582959329, 0.2552076118149841921, 0.2578127128616094499, 0.2604158475944712281, 0.2630211061698037311, 0.2656243636342671688, 0.2682291689184919115, 0.2708330451516883230, 0.2734369368000036937, 0.2760417322684234342, 0.2786449988978000336, 0.2812502554714267355, 0.2838533869016899303, 0.2864584937839013135, 0.2890620024552456591, 0.2916663629743991848, 0.2942707099920074398, 0.2968742320781582733, 0.2994793331325310004, 0.3020824677347322962, 0.3046877262316646240, 0.3072909837388622112, 0.3098957888503254821, 0.3124996652267145181, 0.3151035566296633839, 0.3177083521945192612, 0.3203116186622446127, 0.3229168752506134110, 0.3255200066892336430, 0.3281251134958176330, 0.3307286223255002655, 0.3333329826714347410, 0.3359373298719517953, 0.3385408517869427647, 0.3411459529470890484, 0.3437490875183005223, 0.3463543460347343617, 0.3489576036842249041, 0.3515624087212146920, 0.3541662853398466204, 0.3567701765964986227, 0.3593749723560626386, 0.3619782387617029862, 0.3645834954627060198, 0.3671866270093405715, 0.3697917338383204244, 0.3723952429256875973, 0.3749996031970665444, 0.3776039506791386557, 0.3802074725223298923, 0.3828125738862612759, 0.3854157085261381011, 0.3880209671599602617, 0.3906242250512887426, 0.3932290301120778819, 0.3958329070719905363, 0.3984367982813996067, 0.4010415943339316058, 0.4036448607770379837, 0.4062501176885546794, 0.4088532494428480657, 0.4114583563922335485, 0.4140618658366201910, 0.4166662261320933647, 0.4192705739943561327, 0.4218740958650940009, 0.4244791975308115917, 0.4270823323389966175, 0.4296875911880828069, 0.4322908494207843844, 0.4348956546036337745, 0.4374995320038561619, 0.4401034232650644085, 0.4427082197088152427, 0.4453114862889279713, 0.4479167435088288185, 0.4505198755704162283, 0.4531249827382076711, 0.4557284926389418844, 0.4583328530571487147, 0.4609372013982309668, 0.4635407233958523388, 0.4661458254613498609, 0.4687489605374778323, 0.4713542196996960976, 0.4739574783732994345, 0.4765622837764619812, 0.4791661617160185016, 0.4817700531280592058, 0.4843748500612748420, 0.4869781168779269698, 0.4895833745040767959, 0.4921865069725880892, 0.4947916144567798824, 0.4973951249131855490, 0.4999994855527590265, 0.5026038344712867589, 0.5052073566951218453, 0.5078124592583899144, 0.5104155947020908579, 0.5130208542753056378, 0.5156241134893367883, 0.5182289192110610676, 0.5208327977889742888, 0.5234366894508762913, 0.5260414869718011976, 0.5286447541245218318, 0.5312500122547839654, 0.5338531452298473923, 0.5364582531284315392, 0.5390617642398328746, 0.5416661251994032700, 0.5442704747940029231, 0.5468739973433798252, 0.5494791005024090014, 0.5520822364133124438, 0.5546874964953879550, 0.5572907563493740835, 0.5598955624879079496, 0.5624994418032033261, 0.5651033338139942463, 0.5677081320208752224, 0.5703113996091939697, 0.5729166583414331271, 0.5755197919226788805, 0.5781249003336490500, 0.5807284121993739889, 0.5833327735775721834, 0.5859371239468746939, 0.5885406469211225122, 0.5911457507739076300, 0.5937488872516457628, 0.5963541479404496082, 0.5989574085339228748, 0.6015622151875171797, 0.6041660953392257172, 0.6067699877979360057, 0.6093747867890261238, 0.6119780549124759217, 0.6145833143445629254, 0.6171864486316270826, 0.6197915576529816617, 0.6223950703723655220, 0.6249994322678273928, 0.6276037835104713025, 0.6302073070089242446, 0.6328124116534677990, 0.6354155487976793637, 0.6380208101910863627, 0.6406240716235875876, 0.6432288788904997334, 0.6458327599776627626, 0.6484366529833293091, 0.6510414528568908565, 0.6536447216150126360, 0.6562499818448275235, 0.6588531169373553764, 0.6614582266671018562, 0.6640617403394915019, 0.6666661028508605868, 0.6692704550654967610, 0.6718739791874978051, 0.6744790847218130603, 0.6770822226321474568, 0.6796874848280434200, 0.6822907471991253026, 0.6848955551776233497, 0.6874994372992955238, 0.6901033309509650993, 0.6927081318052739078, 0.6953114012976200353, 0.6979166624230551674, 0.7005197984207056638, 0.7031249089568636368, 0.7057284236816204759, 0.7083327869075525252, 0.7109371401928469281, 0.7135406650377511539, 0.7161457715598668061, 0.7187489103359874232, 0.7213541734322722609, 0.7239574368415039318, 0.7265622456298695964, 0.7291661288851226663, 0.7317700232818561412, 0.7343748252152053624, 0.7369780955413426371, 0.7395833576603073611, 0.7421864946627563242, 0.7447916061033615920, 0.7473951219798656842, 0.7499994860190324353, 0.7526038404736700160, 0.7552073661408488237, 0.7578124737488122209, 0.7604156134903999886, 0.7630208775849919300, 0.7656241421319622820, 0.7682289518284949326, 0.7708328363164217434, 0.7734367315572975299, 0.7760415346680002990, 0.7786448059275148381, 0.7812500691379388185, 0.7838532072448821664, 0.7864583196879902927, 0.7890618368156444573, 0.7916662017667361884, 0.7942705574894247667, 0.7968740840782696511, 0.7994791928701499018, 0.8020823336769073997, 0.8046875988677468783, 0.8072908646520678966, 0.8098956753550886623, 0.8124995611748068169, 0.8151034573589240884, 0.8177082617453185209, 0.8203115340378186460, 0.8229167984376549727, 0.8255199377488137147, 0.8281250512925039109, 0.8307285697707365024, 0.8333329357324672504, 0.8359372928219411802, 0.8385408204318668401, 0.8411459305057594760, 0.8437490724774151518, 0.8463543388624672481, 0.8489576059837783406, 0.8515624177916331083, 0.8541663050422881875, 0.8567702022687715413, 0.8593750080292236193, 0.8619782814543437421, 0.8645835471415733720, 0.8671866877566964948, 0.8697918024990743957, 0.8723953224273439666, 0.8749996894984543028, 0.8776040480534781363, 0.8802075767839265819, 0.8828126882379567775, 0.8854158314742670566, 0.8880210991515266050, 0.8906243677094983768, 0.8932291807205616774, 0.8958330695013316802, 0.8984369678693342465, 0.9010417751022415933, 0.9036450497596462128, 0.9062503168322812996, 0.9088534588511494317, 0.9114585748903522022, 0.9140620963681507227, 0.9166664646474114164, 0.9192708247667824573, 0.9218743547172278952, 0.9244794676495572405, 0.9270826122503010858, 0.9296878813177945622, 0.9322911514121841048, 0.9348959657248061550, 0.9374998561347748227, 0.9401037557438677306, 0.9427085645475906661, 0.9453118405358371668, 0.9479171090940153865, 0.9505202526155902554, 0.9531253700418979014, 0.9557288931959170286, 0.9583332627756006028, 0.9609376244112938226, 0.9635411559431285022, 0.9661462708106475228, 0.9687494151757961580, 0.9713546862302190332, 0.9739579640138142924, 0.9765627705390533819, 0.9791666547386930208, 0.9817705986233274951, 0.9843753609709087193, 0.9869785915570626900, 0.9895841932699848131, 0.9921866851465583892, 0.9947911401134668097, 0.9973998225951543617, 1.000000000000000000 ),
 .UNSPECIFIED. ) ;
#163937 = CARTESIAN_POINT ( 'NONE',  ( 8.540746701604824409, 12.05162268759261224, -1.199719254218446718 ) ) ;
#163938 = CARTESIAN_POINT ( 'NONE',  ( -11.78331023100045627, 11.29999999999998117, 1.799999999999999600 ) ) ;
#163939 = CARTESIAN_POINT ( 'NONE',  ( 3.919074646851735455, 0.6231337533108800564, 1.618193163429545223 ) ) ;
#163940 = AXIS2_PLACEMENT_3D ( 'NONE', #9028, #205076, #137977 ) ;
#163941 = CARTESIAN_POINT ( 'NONE',  ( 4.492743645254620333, 2.128474237214292852, 0.4277247895240059994 ) ) ;
#163942 = CARTESIAN_POINT ( 'NONE',  ( 4.844340958784499662, 4.546152628203684820, 0.7998128361456341429 ) ) ;
#163943 = CARTESIAN_POINT ( 'NONE',  ( 6.210172754313918908, 1.157103754073171675, -1.651340222398114843 ) ) ;
#163944 = CARTESIAN_POINT ( 'NONE',  ( 6.750000000000005329, 3.748112931134527976E-13, 1.999999999999984901 ) ) ;
#163945 = CARTESIAN_POINT ( 'NONE',  ( 0.7499999999999902300, 4.097916667349481123, -1.299038105676658228 ) ) ;
#163946 = CARTESIAN_POINT ( 'NONE',  ( 3.030207491816420795, 1.071487476811390449, -1.600714694641630853 ) ) ;
#163947 = CARTESIAN_POINT ( 'NONE',  ( -0.7500000000000006661, 9.489583334016129967, -1.299038105676657340 ) ) ;
#163948 = CARTESIAN_POINT ( 'NONE',  ( 5.467086432746695479, -1.751203904306109838, 1.366580491753234039 ) ) ;
#163949 = ORIENTED_EDGE ( 'NONE', *, *, #36816, .F. ) ;
#163950 = CARTESIAN_POINT ( 'NONE',  ( 6.983263157960366563, -0.003091553303710344557, 1.945923119799706669 ) ) ;
#163951 = CARTESIAN_POINT ( 'NONE',  ( 0.7499999999999885647, 3.066666666666689522, -1.299038105676658228 ) ) ;
#163952 = CARTESIAN_POINT ( 'NONE',  ( 4.286349120214771879, 8.152491073559232859, -0.7998128361456221525 ) ) ;
#163953 = CARTESIAN_POINT ( 'NONE',  ( -3.475000000000000533, -1.006249999044084298, 0.000000000000000000 ) ) ;
#163954 = CARTESIAN_POINT ( 'NONE',  ( 7.510853912290742507, 8.825379654836435606, -1.082531754730537976 ) ) ;
#163955 = CARTESIAN_POINT ( 'NONE',  ( 0.7500000000000006661, 10.11458333401612997, 1.299038105676657340 ) ) ;
#163956 = CARTESIAN_POINT ( 'NONE',  ( 6.021229618244865023, 10.03886863134542828, -0.7216878364870458196 ) ) ;
#163957 = CARTESIAN_POINT ( 'NONE',  ( 0.01820432788856435335, -1.842448466851685840, 0.8197770699841927522 ) ) ;
#163959 = CARTESIAN_POINT ( 'NONE',  ( 4.932111759923301975, 1.184877397895794493, 1.688235060362786255 ) ) ;
#163958 = CARTESIAN_POINT ( 'NONE',  ( 10.37606763316019531, 10.99983374830873650, 0.7998128361456462443 ) ) ;
#163960 = CARTESIAN_POINT ( 'NONE',  ( -4.874319919312905647, 5.645460313075203018, -1.199719254218446718 ) ) ;
#163961 = EDGE_CURVE ( 'NONE', #160452, #144836, #88934, .T. ) ;
#163962 = CARTESIAN_POINT ( 'NONE',  ( -3.599999999999999201, -0.5000000000000004441, 0.000000000000000000 ) ) ;
#163963 = CARTESIAN_POINT ( 'NONE',  ( -1.402160292154681736E-14, 0.1968750003414221628, -1.575800808251665908 ) ) ;
#163964 = CARTESIAN_POINT ( 'NONE',  ( 5.430866635118035468, 0.1366067128489474591, 1.865587184704711632 ) ) ;
#163965 = CARTESIAN_POINT ( 'NONE',  ( 5.098194074801078557, -0.2466363661708069477, 1.716370243172520516 ) ) ;
#163966 = CARTESIAN_POINT ( 'NONE',  ( 4.317713577401066871, 1.066398661528572989, -1.375396103214795218 ) ) ;
#163967 = CARTESIAN_POINT ( 'NONE',  ( 3.310162060030825248, 7.013606170011280838, -0.7998128361456291469 ) ) ;
#163968 = CARTESIAN_POINT ( 'NONE',  ( 1.980407754855911140, -2.249062817636026779, -0.4427264618648701910 ) ) ;
#163969 = CARTESIAN_POINT ( 'NONE',  ( -1.364683531250012516, 4.801041667008083991, -0.7879004041258300672 ) ) ;
#163970 = CARTESIAN_POINT ( 'NONE',  ( 0.8844010234979463592, 1.624802019249080853, -0.8659260420235401767 ) ) ;
#163971 = DIRECTION ( 'NONE',  ( 1.000000000000000000, 0.000000000000000000, 0.000000000000000000 ) ) ;
#163972 = CARTESIAN_POINT ( 'NONE',  ( 1.940199132888191791, 1.805219978825555627, 0.2711003711317952480 ) ) ;
#163973 = CARTESIAN_POINT ( 'NONE',  ( 2.690077459517980163, 1.704938782060089864, 1.076316768488336351 ) ) ;
#163974 = CARTESIAN_POINT ( 'NONE',  ( 1.113517231965298837, -2.137359700923711081, 0.4831916906855234228 ) ) ;
#163975 = CARTESIAN_POINT ( 'NONE',  ( 8.736508494932113678, 15.13472907373737186, -7.593571698007603565 ) ) ;
#163976 = CARTESIAN_POINT ( 'NONE',  ( 3.997179113411051254, 1.780275165862042153, -1.124711807175354350 ) ) ;
#163977 = CARTESIAN_POINT ( 'NONE',  ( -6.093499974338126179, 9.196501505781426999, -1.199719254218440723 ) ) ;
#163978 = CARTESIAN_POINT ( 'NONE',  ( 1.205626512970816355, -1.630946839658468983, -1.275175305487465049 ) ) ;
#163979 = CARTESIAN_POINT ( 'NONE',  ( 4.320244504248938355, 8.192035688265757898, 1.040834085586084257E-14 ) ) ;
#163980 = CARTESIAN_POINT ( 'NONE',  ( -1.360316468750010666, 2.869791667008063651, -0.7853790794158961308 ) ) ;
#163981 = CARTESIAN_POINT ( 'NONE',  ( 3.141385665567609564, 0.05408136815227351790, 2.119969838212852675 ) ) ;
#163982 = CARTESIAN_POINT ( 'NONE',  ( 0.6823417656249882723, 0.4260416670080896528, -1.181850606188749264 ) ) ;
#163983 = CARTESIAN_POINT ( 'NONE',  ( 6.692070433991195166, -0.7751425012093198230, 1.651373049820707317 ) ) ;
#163984 = ORIENTED_EDGE ( 'NONE', *, *, #5066, .F. ) ;
#163985 = CARTESIAN_POINT ( 'NONE',  ( -4.118644803501354978, 8.027112380718707030, 0.7998128361456352531 ) ) ;
#163986 = CARTESIAN_POINT ( 'NONE',  ( 9.585778300061798873, 11.14216175728232550, -1.199719254218440723 ) ) ;
#163987 = CARTESIAN_POINT ( 'NONE',  ( 5.492461626867537916, 9.421972641405202964, -0.7216878364870458196 ) ) ;
#163988 = CARTESIAN_POINT ( 'NONE',  ( 1.737499999999999378, -3.572916665710752948, -3.009438278150925683 ) ) ;
#163989 = CARTESIAN_POINT ( 'NONE',  ( -5.343885102080728977, 9.386283052402845328, 0.7998128361456481317 ) ) ;
#163990 = CARTESIAN_POINT ( 'NONE',  ( 3.392836290029502155, -1.947660480455270404, -0.5347636834307776255 ) ) ;
#163991 = CARTESIAN_POINT ( 'NONE',  ( 0.6046866811788155216, -0.7097959115549393738, -1.982883793842766362 ) ) ;
#163992 = CARTESIAN_POINT ( 'NONE',  ( -7.130662446144611977, 7.283804040115648526, 0.000000000000000000 ) ) ;
#163993 = CARTESIAN_POINT ( 'NONE',  ( 8.914649696185335870, 10.35917838609310593, -1.199719254218446718 ) ) ;
#163994 = CARTESIAN_POINT ( 'NONE',  ( 5.207777014082533462, 0.5861155943000575519, -1.766266804033526094 ) ) ;
#163995 = CARTESIAN_POINT ( 'NONE',  ( 8.158255747121103241, 10.54105100977322174, 1.599625672291281386 ) ) ;
#163996 = FACE_OUTER_BOUND ( 'NONE', #164448, .T. ) ;
#163997 = CARTESIAN_POINT ( 'NONE',  ( -4.060830702492950195, 4.696389560118578999, -1.199719254218452047 ) ) ;
#163998 = CARTESIAN_POINT ( 'NONE',  ( -7.691553217654356622, 7.867900263551875994, -0.7998128361456291469 ) ) ;
#163999 = CARTESIAN_POINT ( 'NONE',  ( 6.508673417949426110, 1.528841652884159963, -1.382195874861185336 ) ) ;
#164001 = CARTESIAN_POINT ( 'NONE',  ( -4.661943307450316709, 7.086702294391122869, 1.392663581761391267 ) ) ;
#164000 = CARTESIAN_POINT ( 'NONE',  ( -5.855142236255304944, 7.924361590421551860, -1.599625672291271394 ) ) ;
#164002 = CARTESIAN_POINT ( 'NONE',  ( 1.364683531249986537, 0.1135416670080857532, 0.7879004041258500513 ) ) ;
#164003 = CARTESIAN_POINT ( 'NONE',  ( 3.286226705615200139, -1.671546763608670272, 0.4602933761382789202 ) ) ;
#164004 = CARTESIAN_POINT ( 'NONE',  ( 1.077605773158099023, -1.697095445269660496, -0.3847248992609655915 ) ) ;
#164006 = CARTESIAN_POINT ( 'NONE',  ( 6.317736394288131052, 9.354147645769410602, 1.082531754730558626 ) ) ;
#164005 = CARTESIAN_POINT ( 'NONE',  ( 0.3589920806752691096, 0.8874099113769757796, 2.130322803234908857 ) ) ;
#164007 = CARTESIAN_POINT ( 'NONE',  ( -11.13243988973272636, 5.430794512910079419, -4.010128837087161280 ) ) ;
#164008 = CARTESIAN_POINT ( 'NONE',  ( 2.231779466116891708, -1.343800923419868010, -1.562491722542774797 ) ) ;
#164009 = EDGE_CURVE ( 'NONE', #102475, #18521, #188865, .T. ) ;
#164010 = EDGE_CURVE ( 'NONE', #13120, #137516, #91396, .T. ) ;
#164011 = CARTESIAN_POINT ( 'NONE',  ( 1.493517298738750609, 1.942243344100362590, 0.5404107738020345053 ) ) ;
#164012 = CARTESIAN_POINT ( 'NONE',  ( 6.825078400183544503, 3.684911640780349718, 2.658296617506946458 ) ) ;
#164014 =( GEOMETRIC_REPRESENTATION_CONTEXT ( 3 ) GLOBAL_UNCERTAINTY_ASSIGNED_CONTEXT ( ( #211384 ) ) GLOBAL_UNIT_ASSIGNED_CONTEXT ( ( #123553, #141881, #139735 ) ) REPRESENTATION_CONTEXT ( 'NONE', 'WORKASPACE' ) );
#164013 = CARTESIAN_POINT ( 'NONE',  ( -5.635349125135588721, 6.603604063193491136, 1.199719254218452935 ) ) ;
#164015 = CARTESIAN_POINT ( 'NONE',  ( 1.709780583834107803, -1.956794704801574358, 0.2394988650771395777 ) ) ;
#164016 = CIRCLE ( 'NONE', #170949, 6.277139874739035008 ) ;
#164018 = CARTESIAN_POINT ( 'NONE',  ( -5.628043163448566588, 9.580151100749725757, 0.000000000000000000 ) ) ;
#164017 = CARTESIAN_POINT ( 'NONE',  ( 4.640819915729988310, 1.831716588661407963, 0.5496940206762624959 ) ) ;
#164019 = CARTESIAN_POINT ( 'NONE',  ( 5.742855475442601332, 0.4270144693867898300, 2.165010647329483895 ) ) ;
#164020 = CARTESIAN_POINT ( 'NONE',  ( -7.119440060507479018, 8.439006504414422238, 1.082531754730549078 ) ) ;
#164021 = CARTESIAN_POINT ( 'NONE',  ( 5.338878628731272613, 9.450718510153643948, -0.7998128361456481317 ) ) ;
#164022 = CARTESIAN_POINT ( 'NONE',  ( -7.228432174741334038, 8.462200954400218578, -1.199719254218452047 ) ) ;
#164023 = CARTESIAN_POINT ( 'NONE',  ( 0.3287785284849250034, 1.391158174000119097, -1.464406657780653820 ) ) ;
#164024 = CARTESIAN_POINT ( 'NONE',  ( -3.592547517496907705, 7.135129837147655252, -0.7216878364870090712 ) ) ;
#164025 = CARTESIAN_POINT ( 'NONE',  ( 4.120403395486138542, -1.183043222452788257, -1.981120964393435768 ) ) ;
#164026 = CARTESIAN_POINT ( 'NONE',  ( 4.510177812457000002, 1.961482754637720927, -0.04604004567236585910 ) ) ;
#164027 = EDGE_CURVE ( 'NONE', #206199, #55184, #118046, .T. ) ;
#164028 = CARTESIAN_POINT ( 'NONE',  ( 1.920681792755131845, -1.391007931628859939, 1.383589105726056756 ) ) ;
#164029 = CARTESIAN_POINT ( 'NONE',  ( 10.23370702021670020, 10.83374636654133383, 0.7998128361456462443 ) ) ;
#164030 = CARTESIAN_POINT ( 'NONE',  ( 1.712858683735189347, 1.037413707456548373, 1.381497717048131513 ) ) ;
#164031 = ORIENTED_EDGE ( 'NONE', *, *, #188144, .T. ) ;
#164032 = CARTESIAN_POINT ( 'NONE',  ( -0.1353153266233823870, -2.055576600424202649, -0.5074567962913156816 ) ) ;
#164034 = CARTESIAN_POINT ( 'NONE',  ( -7.588813295347149435, 9.876701482703580837, -1.599625672291263179 ) ) ;
#164033 = CARTESIAN_POINT ( 'NONE',  ( -4.412288926243578935, 7.235088616337731260, 1.199719254218464037 ) ) ;
#164035 = CARTESIAN_POINT ( 'NONE',  ( 1.007454599746326895, -0.8259622865525710900, -1.645551850779983116 ) ) ;
#164036 = EDGE_LOOP ( 'NONE', ( #134837, #32251, #150230, #87189, #142749 ) ) ;
#164037 = CARTESIAN_POINT ( 'NONE',  ( 3.749033319061449543, -0.4183670367851847205, -2.130223169982926379 ) ) ;
#164038 = FACE_OUTER_BOUND ( 'NONE', #208327, .T. ) ;
#164039 = CARTESIAN_POINT ( 'NONE',  ( 2.021885665735908333, -0.4598567139443253682, 2.069992740399699382 ) ) ;
#164040 = CARTESIAN_POINT ( 'NONE',  ( -1.499999999999997780, 3.681250000682819046, 1.214306433183764966E-14 ) ) ;
#164041 = CARTESIAN_POINT ( 'NONE',  ( 9.240045382913317340, 10.73880668727576015, -1.199719254218446718 ) ) ;
#164042 = DIRECTION ( 'NONE',  ( 0.000000000000000000, 1.000000000000000000, 0.000000000000000000 ) ) ;
#164043 = CARTESIAN_POINT ( 'NONE',  ( 6.472394699177205446, 6.854181287346997387, 0.6349317888264572884 ) ) ;
#164044 = CARTESIAN_POINT ( 'NONE',  ( 2.495449868850362574, 1.590812333473600626, 1.309970014422021212 ) ) ;
#164046 = CARTESIAN_POINT ( 'NONE',  ( -0.1296875068448159751, 0.001480089298542403009, -1.826395826379861864 ) ) ;
#164045 = CARTESIAN_POINT ( 'NONE',  ( -9.203287345578106127, 9.631590079462940324, 0.7998128361456462443 ) ) ;
#164047 = CARTESIAN_POINT ( 'NONE',  ( 1.364683531249988535, 2.863541667008082658, 0.7879004041258500513 ) ) ;
#164048 = CARTESIAN_POINT ( 'NONE',  ( -0.7500000000000179856, 9.291666666666669627, 1.299038105676658228 ) ) ;
#164049 = DIRECTION ( 'NONE',  ( 0.000000000000000000, 1.000000000000000000, -0.000000000000000000 ) ) ;
#164050 = CARTESIAN_POINT ( 'NONE',  ( 11.84668730067608600, 10.19999999999999929, -1.400000000000001910 ) ) ;
#164051 = CARTESIAN_POINT ( 'NONE',  ( 1.775094195334154135, -2.148033089049032895, -0.7103491116851842202 ) ) ;
#164052 = CARTESIAN_POINT ( 'NONE',  ( -9.544576954340667996, 11.19805653722800365, 1.082531754730558626 ) ) ;
#164053 = CARTESIAN_POINT ( 'NONE',  ( 1.652323331381430283, 1.792179557038487303, 0.2633440673391762576 ) ) ;
#164054 = CARTESIAN_POINT ( 'NONE',  ( 1.885809660653874120, -1.915224419731532901, 0.05109022710406836698 ) ) ;
#164055 = CARTESIAN_POINT ( 'NONE',  ( 3.648938843998358106, -0.4010542052625790110, -2.030977206718207473 ) ) ;
#164056 = CARTESIAN_POINT ( 'NONE',  ( -0.6823417656250003738, 1.780208333674752952, -1.181850606188749264 ) ) ;
#164057 = CARTESIAN_POINT ( 'NONE',  ( 1.217580299722145210, -1.923910348332603881, 0.4297500124877791650 ) ) ;
#164058 = CARTESIAN_POINT ( 'NONE',  ( 5.531840760993587125, -1.223730149660817501, -1.487915846976423984 ) ) ;
#164060 = CARTESIAN_POINT ( 'NONE',  ( 6.492506472431533560, 6.747478052702773788, -0.04572756507489894595 ) ) ;
#164059 = CARTESIAN_POINT ( 'NONE',  ( 1.559632053384899741, -1.981161107035840141, -1.183202272445786907 ) ) ;
#164061 = CARTESIAN_POINT ( 'NONE',  ( -1.364683531250012516, 2.988541667008091096, -0.7879004041258289570 ) ) ;
#164062 = CARTESIAN_POINT ( 'NONE',  ( 5.055161771162819839, 1.716784339331741682, -1.143088790766825236 ) ) ;
#164063 = CARTESIAN_POINT ( 'NONE',  ( -5.738125327081750271, 7.717565519727259904, 1.599625672291269396 ) ) ;
#164064 = CARTESIAN_POINT ( 'NONE',  ( 8.111855979677986994, 8.358253485912799263, 1.040834085586084257E-14 ) ) ;
#164065 = DIRECTION ( 'NONE',  ( 0.000000000000000000, 0.000000000000000000, 1.000000000000000000 ) ) ;
#164067 = CARTESIAN_POINT ( 'NONE',  ( 6.686557493494803772, -2.064527365108769885, -0.4147649638114383475 ) ) ;
#164066 = AXIS2_PLACEMENT_3D ( 'NONE', #198856, #48397, #16909 ) ;
#164068 = CARTESIAN_POINT ( 'NONE',  ( 0.6823417656249899377, 2.405208333674753618, 1.181850606188767472 ) ) ;
#164069 = CARTESIAN_POINT ( 'NONE',  ( 4.991577004318280331, 1.598001195387260154, 1.455802845438579407 ) ) ;
#164070 = CARTESIAN_POINT ( 'NONE',  ( 5.496742197731416368, -1.970900515782060936, -0.4404336293717215356 ) ) ;
#164071 = CARTESIAN_POINT ( 'NONE',  ( 0.000000000000000000, 4.518467169708413778, 0.000000000000000000 ) ) ;
#164072 = CARTESIAN_POINT ( 'NONE',  ( -6.100805936469506641, 6.219954468743612352, 0.7216878364870317197 ) ) ;
#164073 = EDGE_CURVE ( 'NONE', #13599, #133314, #11405, .T. ) ;
#164076 = CARTESIAN_POINT ( 'NONE',  ( 6.019457014787495730, 6.125047393447951016, -0.7216878364870257245 ) ) ;
#164075 = CARTESIAN_POINT ( 'NONE',  ( 3.285556943750000070, -1.334374999522040861, 0.000000000000000000 ) ) ;
#164074 = CARTESIAN_POINT ( 'NONE',  ( 7.713663051532233972, 7.963971413067895355, -0.7998128361456341429 ) ) ;
#164077 = CARTESIAN_POINT ( 'NONE',  ( -5.991777542596674166, 5.955104985976372944, 0.000000000000000000 ) ) ;
#164078 = CARTESIAN_POINT ( 'NONE',  ( 3.467982673848205355, -0.9896861206786079501, 1.756853968756578066 ) ) ;
#164079 = CARTESIAN_POINT ( 'NONE',  ( -7.395082721250053837, 10.71501471051202614, -1.199719254218446718 ) ) ;
#164081 = CYLINDRICAL_SURFACE ( 'NONE', #167749, 0.3999999999999997446 ) ;
#164080 = CARTESIAN_POINT ( 'NONE',  ( -2.591579918506545344, 6.175260338232929413, 1.040834085586084257E-14 ) ) ;
#164083 = CARTESIAN_POINT ( 'NONE',  ( 1.364683531250000748, 9.505208333674735499, -0.7879004041258355073 ) ) ;
#164082 = CARTESIAN_POINT ( 'NONE',  ( 4.750933126423753095, -1.738186171353903742, 1.284983810367075208 ) ) ;
#164084 = DIRECTION ( 'NONE',  ( -1.000000000000000000, 0.000000000000000000, 0.000000000000000000 ) ) ;
#164085 = CARTESIAN_POINT ( 'NONE',  ( -11.86402016121722269, 7.774204713095177688, -1.819606832628274384 ) ) ;
#164087 = CARTESIAN_POINT ( 'NONE',  ( 4.991814629660241920, -2.006445540622634915, 0.2004526995145126111 ) ) ;
#164086 = CARTESIAN_POINT ( 'NONE',  ( -6.683806541412762314, 9.781229484081471526, -1.082531754730537976 ) ) ;
#164088 = CARTESIAN_POINT ( 'NONE',  ( -1.364683531250000748, -1.178124999658580752, 0.000000000000000000 ) ) ;
#164089 = CARTESIAN_POINT ( 'NONE',  ( 0.9083514600924915694, 1.308824770132447135, -1.123559637378883203 ) ) ;
#164090 = CARTESIAN_POINT ( 'NONE',  ( 4.817943484809818600, 6.714296380401858499, 1.599625672291269396 ) ) ;
#164092 = CARTESIAN_POINT ( 'NONE',  ( 6.210516883511641772, 9.403297576475722508, 1.199719254218452047 ) ) ;
#164091 = CARTESIAN_POINT ( 'NONE',  ( 8.446366511633696561, 8.956441806435218922, 1.040834085586084257E-14 ) ) ;
#164093 = CARTESIAN_POINT ( 'NONE',  ( -11.56582117199599224, 8.167499266818545323, -3.209445363707945198 ) ) ;
#164094 = CARTESIAN_POINT ( 'NONE',  ( 6.380143124955812262, -1.000617425381218561, 1.580232162242324545 ) ) ;
#164095 = CARTESIAN_POINT ( 'NONE',  ( 1.172521868268823875, 0.8179054604866965450, 1.839630344048637678 ) ) ;
#164096 = CARTESIAN_POINT ( 'NONE',  ( 3.048105859194950362, 0.7956334958073747465, -2.058523145315640956 ) ) ;
#164097 = CARTESIAN_POINT ( 'NONE',  ( -5.926322542504864899, 8.967774495347393682, -1.082531754730549967 ) ) ;
#164098 = ORIENTED_EDGE ( 'NONE', *, *, #82220, .T. ) ;
#164099 = CARTESIAN_POINT ( 'NONE',  ( 9.422553571373278203, 11.05569592376608945, -1.082531754730543083 ) ) ;
#164101 = CARTESIAN_POINT ( 'NONE',  ( 2.284780001213771783, 1.617805504991537635, -1.203372706716873575 ) ) ;
#164100 = CARTESIAN_POINT ( 'NONE',  ( 2.227333921462580246, 1.895369558270381338, 0.9509248740046101211 ) ) ;
#164103 = EDGE_LOOP ( 'NONE', ( #52968, #82993, #171181, #134809 ) ) ;
#164102 = CARTESIAN_POINT ( 'NONE',  ( 2.830093135299842189, -0.8964878685940536052, -1.574152086365911529 ) ) ;
#164104 = CARTESIAN_POINT ( 'NONE',  ( 5.854088466050551887, 10.05179665369283981, 0.7998128361456341429 ) ) ;
#164105 = VERTEX_POINT ( 'NONE', #189932 ) ;
#164106 = CARTESIAN_POINT ( 'NONE',  ( 7.122110765880372618, 7.203550736482235095, 0.7998128361456341429 ) ) ;
#164108 = CARTESIAN_POINT ( 'NONE',  ( 0.02247297916271525850, 0.3300846716227764932, 1.886903735308493424 ) ) ;
#164107 = CARTESIAN_POINT ( 'NONE',  ( -3.741160322367112379, 6.452105245148518797, 1.199719254218464037 ) ) ;
#164109 = CARTESIAN_POINT ( 'NONE',  ( 0.1747926744264660381, 0.006858446013176254172, -1.855468577918440776 ) ) ;
#164110 = CARTESIAN_POINT ( 'NONE',  ( 1.451998047844732964, 7.315968950354620581, 4.301760722576522866 ) ) ;
#164111 = CARTESIAN_POINT ( 'NONE',  ( 6.331294547457450683, 7.449227062530913379, -1.082531754730543083 ) ) ;
#164112 = CARTESIAN_POINT ( 'NONE',  ( 0.6823417656249882723, 0.1552083336747514530, 1.181850606188755259 ) ) ;
#164113 = CARTESIAN_POINT ( 'NONE',  ( 0.000000000000000000, -7.154544010627095219, 0.000000000000000000 ) ) ;
#164114 = CARTESIAN_POINT ( 'NONE',  ( -9.996439331977562404, 10.55693406359564790, 0.7998128361456462443 ) ) ;
#164115 = ADVANCED_FACE ( 'NONE', ( #5816, #72968 ), #38351, .F. ) ;
#164116 = CARTESIAN_POINT ( 'NONE',  ( 4.698454014923811428, 1.387101836239763131, -1.463925544105355803 ) ) ;
#164117 = CARTESIAN_POINT ( 'NONE',  ( 5.612251347527116074, -0.9680786960581323486, -1.932885698521320306 ) ) ;
#164118 = CARTESIAN_POINT ( 'NONE',  ( -7.268579750702168774, 7.652633595340216921, -0.7216878364870338292 ) ) ;
#164119 = CARTESIAN_POINT ( 'NONE',  ( 4.855228407469603269, 7.718164671139588151, -1.082531754730548412 ) ) ;
#164120 = CARTESIAN_POINT ( 'NONE',  ( 1.828540510153942922, -1.004066958311781832, -1.867862179375394005 ) ) ;
#164121 = CARTESIAN_POINT ( 'NONE',  ( -1.225000000000019407, 2.500000000000009326, -1.387778780781445676E-14 ) ) ;
#164122 = CARTESIAN_POINT ( 'NONE',  ( 2.952367129307902793, 0.6606739728568145065, 1.857499748845674370 ) ) ;
#164123 = EDGE_LOOP ( 'NONE', ( #138267, #1, #166139, #142991 ) ) ;
#164125 = EDGE_CURVE ( 'NONE', #39263, #67222, #21002, .T. ) ;
#164124 = DIRECTION ( 'NONE',  ( 0.000000000000000000, 0.000000000000000000, -1.000000000000000000 ) ) ;
#164126 = CARTESIAN_POINT ( 'NONE',  ( 0.5376586404672692998, 1.932363751568724641, -0.7437053376125392079 ) ) ;
#164127 = CARTESIAN_POINT ( 'NONE',  ( 1.130689739129210336, -1.755767597885007136, 0.8300169520328912753 ) ) ;
#164128 = ORIENTED_EDGE ( 'NONE', *, *, #14587, .T. ) ;
#164129 = LINE ( 'NONE', #145781, #209631 ) ;
#164131 = CARTESIAN_POINT ( 'NONE',  ( -2.331034670843834533E-15, -6.124285368610726366, 10.93005900551663956 ) ) ;
#164130 = CARTESIAN_POINT ( 'NONE',  ( -5.289089323106922258, 9.184704953684462936, 0.7216878364870267237 ) ) ;
#164133 = CARTESIAN_POINT ( 'NONE',  ( 5.459129407796876166, 9.520734742405036144, 1.040834085586084257E-14 ) ) ;
#164132 = CARTESIAN_POINT ( 'NONE',  ( 2.132869701138325969, -1.867042483574256728, 0.9408474824332532238 ) ) ;
#164135 = CARTESIAN_POINT ( 'NONE',  ( 3.879041346841291649, 7.539648981374564407, 1.040834085586084257E-14 ) ) ;
#164134 = CARTESIAN_POINT ( 'NONE',  ( 7.253775878511261155, 8.421492265473332850, 1.199719254218462483 ) ) ;
#164137 = ORIENTED_EDGE ( 'NONE', *, *, #162333, .F. ) ;
#164136 = CARTESIAN_POINT ( 'NONE',  ( 6.199862383955294654, 1.322219258337012704, 1.381733411008022383 ) ) ;
#164138 = CARTESIAN_POINT ( 'NONE',  ( 3.985166894971280183, -0.2153072539897090687, -2.196357064762343825 ) ) ;
#164139 = CARTESIAN_POINT ( 'NONE',  ( 1.852830919558448697, 0.6925466627333075609, 2.095365425716289032 ) ) ;
#164140 = CARTESIAN_POINT ( 'NONE',  ( 0.08246951281144777879, -1.249137507218839094, 1.448023666807838117 ) ) ;
#164141 = CARTESIAN_POINT ( 'NONE',  ( -5.113031849284871200, 4.859625333787436219, 0.6539756689589106831 ) ) ;
#164142 = CARTESIAN_POINT ( 'NONE',  ( 9.856941372335116469, 11.45851867493453291, 1.199719254218450271 ) ) ;
#164143 = CARTESIAN_POINT ( 'NONE',  ( 4.650872726564402981, -0.4503784926754761386, -2.020631409805350387 ) ) ;
#164145 = CARTESIAN_POINT ( 'NONE',  ( 1.200320640528436789, -2.161883444890321915, 0.0006282887012112879947 ) ) ;
#164144 = CARTESIAN_POINT ( 'NONE',  ( 0.04208621775141611898, -6.437359833193938563, 10.89523958697327011 ) ) ;
#164146 = CARTESIAN_POINT ( 'NONE',  ( 3.245827600587628758, 2.191739723504753101, -0.002129563554123526260 ) ) ;
#164147 = DIRECTION ( 'NONE',  ( 0.000000000000000000, 1.000000000000000000, 0.000000000000000000 ) ) ;
#164148 = CARTESIAN_POINT ( 'NONE',  ( 1.499999999999822586, 7.267697830503921708, 4.207111467970846341 ) ) ;
#164149 = CARTESIAN_POINT ( 'NONE',  ( 0.6823417656249969321, 14.33854166700806232, -1.181850606188757036 ) ) ;
#164150 = CARTESIAN_POINT ( 'NONE',  ( -5.113360211009450040, 5.994616996712990975, -1.199719254218453823 ) ) ;
#164152 = CARTESIAN_POINT ( 'NONE',  ( 0.1588275700346117869, 1.163271727376416376, 1.646837250247008777 ) ) ;
#164151 = VECTOR ( 'NONE', #193176, 1000.000000000000000 ) ;
#164153 = EDGE_CURVE ( 'NONE', #136958, #47756, #104429, .T. ) ;
#164154 = CARTESIAN_POINT ( 'NONE',  ( -10.15469386695561482, 10.94949038764413096, 1.040834085586084257E-14 ) ) ;
#164155 = CARTESIAN_POINT ( 'NONE',  ( 5.014543041041934046, 0.7873211189074662553, 1.914903133430221338 ) ) ;
#164156 = CARTESIAN_POINT ( 'NONE',  ( 5.694942756591524713, 1.867452007164069672, 0.9975914146606623678 ) ) ;
#164157 = AXIS2_PLACEMENT_3D ( 'NONE', #45855, #164911, #99919 ) ;
#164158 = CARTESIAN_POINT ( 'NONE',  ( 6.636879889089462026, 7.701780277814560982, -1.199719254218446718 ) ) ;
#164159 = CARTESIAN_POINT ( 'NONE',  ( 1.364683531249992088, 5.384375000341417916, 1.214306433183764966E-14 ) ) ;
#164160 = CARTESIAN_POINT ( 'NONE',  ( 4.311352223092364433, -1.634989290354519342, -1.097634987119990191 ) ) ;
#164161 = CARTESIAN_POINT ( 'NONE',  ( 5.982448691606671254, -0.3306924304021444661, -2.268186543139012024 ) ) ;
#164162 = CARTESIAN_POINT ( 'NONE',  ( 3.896943178251357054, 1.541351720387572843, -0.9781566455248568159 ) ) ;
#164163 = CARTESIAN_POINT ( 'NONE',  ( 4.065465959251388206, 5.836405933916976707, -1.599625672291269396 ) ) ;
#164164 = CARTESIAN_POINT ( 'NONE',  ( 5.138177029454852551, 5.096887410559856946, 0.7216878364870317197 ) ) ;
#164165 = CARTESIAN_POINT ( 'NONE',  ( -5.824109505522200081, 8.952488968821326054, -1.199719254218452047 ) ) ;
#164166 = CARTESIAN_POINT ( 'NONE',  ( 5.017399365509065845, 8.011327138806002779, -1.199719254218450271 ) ) ;
#164167 = ORIENTED_EDGE ( 'NONE', *, *, #91785, .F. ) ;
#164168 = CARTESIAN_POINT ( 'NONE',  ( 5.554944837187737683, 0.3969321943368699368, 1.973527061375530023 ) ) ;
#164169 = VECTOR ( 'NONE', #211379, 1000.000000000000000 ) ;
#164170 = CARTESIAN_POINT ( 'NONE',  ( 6.486976479784771321, -2.298278054978039275, 0.05155775693151467415 ) ) ;
#164171 = CARTESIAN_POINT ( 'NONE',  ( 3.924618397835403893, -1.320764108826902428, 1.450678906977073579 ) ) ;
#164172 = CARTESIAN_POINT ( 'NONE',  ( -7.067878151425722955, 7.140279352951794500, 0.7998128361456341429 ) ) ;
#164173 = CARTESIAN_POINT ( 'NONE',  ( -3.815730167242251003, 6.539103397502874948, -1.199719254218452047 ) ) ;
#164174 = CARTESIAN_POINT ( 'NONE',  ( -9.899039292890925879, 2.972657967447106309, -6.161878781003700567 ) ) ;
#164175 = CARTESIAN_POINT ( 'NONE',  ( -6.784929528996132220, 6.880448970109080520, 0.000000000000000000 ) ) ;
#164177 = CARTESIAN_POINT ( 'NONE',  ( 6.157089704101026406, -1.520188931036812185, -0.9060637366671944193 ) ) ;
#164176 = CARTESIAN_POINT ( 'NONE',  ( 0.8024204784428441428, 1.580594792060415088, -1.368634514759473397 ) ) ;
#164178 = CARTESIAN_POINT ( 'NONE',  ( 10.99126615174919053, -5.166862915010145052, -0.4382560683119158251 ) ) ;
#164179 = CARTESIAN_POINT ( 'NONE',  ( 6.456980378258257325, 0.3295113258894696862, -1.913641714292084073 ) ) ;
#164180 = CARTESIAN_POINT ( 'NONE',  ( 2.115410589380119610, -2.125216164159982046, 0.5342070311455533460 ) ) ;
#164181 = CARTESIAN_POINT ( 'NONE',  ( 1.100653536641453156, -0.4241352534964801801, 1.687842229193817989 ) ) ;
#164182 = CARTESIAN_POINT ( 'NONE',  ( 5.289652487626049115, 9.323011668872403845, 0.7998128361456462443 ) ) ;
#164183 = CARTESIAN_POINT ( 'NONE',  ( 1.593959923740532414, -1.716304196509855329, -0.1716357895808154899 ) ) ;
#164184 = CARTESIAN_POINT ( 'NONE',  ( 2.156058135970494227, 0.9403143569667195001, 1.979733194660021622 ) ) ;
#164185 = CARTESIAN_POINT ( 'NONE',  ( 4.354274438496381627, 2.206422198305586058, -0.05263853172451230661 ) ) ;
#164186 = CARTESIAN_POINT ( 'NONE',  ( 0.9894204570943666566, 0.1578702891864954827, 2.165348367497366144 ) ) ;
#164187 = CARTESIAN_POINT ( 'NONE',  ( 0.4338677482375961070, 0.9413943332680120291, -1.564114433284753636 ) ) ;
#164188 = CARTESIAN_POINT ( 'NONE',  ( 2.343091305525629497, -1.844686447908544746, -1.039184121536258942 ) ) ;
#164189 = CARTESIAN_POINT ( 'NONE',  ( 6.775479680898690127, -7.217880409000396291, -6.775479680898708779 ) ) ;
#164190 = ORIENTED_EDGE ( 'NONE', *, *, #103518, .F. ) ;
#164192 = CARTESIAN_POINT ( 'NONE',  ( 1.364683531249988757, -0.3031249996585799744, 0.000000000000000000 ) ) ;
#164191 = CARTESIAN_POINT ( 'NONE',  ( 2.577988946098773049, -1.175687941515238588, 1.967785589457039741 ) ) ;
#164193 = CARTESIAN_POINT ( 'NONE',  ( 5.030238685870051185, 5.827365540725222282, -1.199719254218452047 ) ) ;
#164194 = CARTESIAN_POINT ( 'NONE',  ( 5.022253332556455341, -2.210719170837057934, 0.2167383629448139670 ) ) ;
#164195 = CARTESIAN_POINT ( 'NONE',  ( -5.585596099150174965, 9.460353182409786399, -0.7216878364870207285 ) ) ;
#164196 = CARTESIAN_POINT ( 'NONE',  ( -15.75000000000000000, 10.90000000000000036, -3.600000000000002309 ) ) ;
#164197 = CARTESIAN_POINT ( 'NONE',  ( 4.934804725694211136, 6.780358151441803649, -1.443375672974051449 ) ) ;
#164198 = CARTESIAN_POINT ( 'NONE',  ( -7.388830529323428209, 8.683019041374528513, 1.082531754730549967 ) ) ;
#164199 = CARTESIAN_POINT ( 'NONE',  ( 5.072158865288243668, 6.050511776658669127, 1.082531754730549078 ) ) ;
#164200 = PRESENTATION_LAYER_ASSIGNMENT (  '', '', ( #198792 ) ) ;
#164201 = ORIENTED_EDGE ( 'NONE', *, *, #195731, .T. ) ;
#164202 = CARTESIAN_POINT ( 'NONE',  ( 3.287732575140737801, 1.587837554856496691, -1.242726844152845178 ) ) ;
#164204 = CARTESIAN_POINT ( 'NONE',  ( 1.006769942787159033, 0.5948965838462864086, 1.974949077847313328 ) ) ;
#164203 = CARTESIAN_POINT ( 'NONE',  ( 8.125414133291656071, 8.374071331795406081, -0.7998128361456291469 ) ) ;
#164205 = CARTESIAN_POINT ( 'NONE',  ( -7.721398836998398352, 0.000000000000000000, -7.721398836998361936 ) ) ;
#164206 = CARTESIAN_POINT ( 'NONE',  ( 6.183927461164522299, 6.387205924212962849, 0.000000000000000000 ) ) ;
#164207 = CARTESIAN_POINT ( 'NONE',  ( -9.597420367780070904, -7.030163990561721477, 0.01387835396683562671 ) ) ;
#164208 = CARTESIAN_POINT ( 'NONE',  ( 1.364683531249990311, 3.634375000341416584, 1.214306433183764966E-14 ) ) ;
#164209 = CARTESIAN_POINT ( 'NONE',  ( 3.855584222106961612, 2.174980185927982923, -0.2676557845137442215 ) ) ;
#164210 = CARTESIAN_POINT ( 'NONE',  ( 2.162732623366144136, 1.242727809108796322, 1.587836805404294171 ) ) ;
#164211 = CARTESIAN_POINT ( 'NONE',  ( 1.469984750362408388, -1.748608032326857353, -0.5769476384821782267 ) ) ;
#164212 = CARTESIAN_POINT ( 'NONE',  ( 7.121056995675668411, 9.330985799753529264, -1.599625672291262513 ) ) ;
#164213 =( NAMED_UNIT ( * ) PLANE_ANGLE_UNIT ( ) SI_UNIT ( $, .RADIAN. ) );
#164214 = CARTESIAN_POINT ( 'NONE',  ( 4.840742024777624053, 0.3130767520662172121, 1.798364180563789327 ) ) ;
#164215 = CARTESIAN_POINT ( 'NONE',  ( 5.994767569012836361, -2.000857541758268354, 0.2496038112331094849 ) ) ;
#164216 = CARTESIAN_POINT ( 'NONE',  ( -8.362681821530818738, 8.650883634741092010, -0.7998128361456291469 ) ) ;
#164218 = CARTESIAN_POINT ( 'NONE',  ( -4.932134020321308654, 8.976183133675331050, 0.7998128361456291469 ) ) ;
#164217 = CARTESIAN_POINT ( 'NONE',  ( 4.680719170653036443, -2.193521624435289752, -0.5540208151394544478 ) ) ;
#164219 = CARTESIAN_POINT ( 'NONE',  ( 0.6628876427188118425, -1.523960678047535877, 1.453889595790233802 ) ) ;
#164220 = CARTESIAN_POINT ( 'NONE',  ( -5.738844160334429567, 9.917344963690652548, 0.000000000000000000 ) ) ;
#164221 = CARTESIAN_POINT ( 'NONE',  ( 4.580570967453869713, 1.276285970795057345, -1.630082184409971324 ) ) ;
#164222 = CARTESIAN_POINT ( 'NONE',  ( 7.567422294721922960, 11.98040977715095323, 0.7998128361456462443 ) ) ;
#164223 = DIRECTION ( 'NONE',  ( 0.000000000000000000, 1.000000000000000000, 0.000000000000000000 ) ) ;
#164224 = CARTESIAN_POINT ( 'NONE',  ( -7.883176251342026042, 11.28445716228600126, -1.199719254218446718 ) ) ;
#164225 = UNCERTAINTY_MEASURE_WITH_UNIT (LENGTH_MEASURE( 1.000000000000000082E-05 ), #31959, 'distance_accuracy_value', 'NONE');
#164226 = CARTESIAN_POINT ( 'NONE',  ( 6.230854113932139171, 9.427024345299638952, 1.199719254218452047 ) ) ;
#164227 = CARTESIAN_POINT ( 'NONE',  ( 4.472818454536469090, 7.041451798021368447, -1.136577435397856384 ) ) ;
#164228 = CARTESIAN_POINT ( 'NONE',  ( -2.252626078164912560, 5.779814191167667481, 0.7998128361456341429 ) ) ;
#164230 = CARTESIAN_POINT ( 'NONE',  ( 1.477127009259255219, -1.566406750307091533, 1.575387012651897622 ) ) ;
#164229 = CARTESIAN_POINT ( 'NONE',  ( 1.459403507577087700, -1.788631592985808538, 1.138920039206146928 ) ) ;
#164231 = CARTESIAN_POINT ( 'NONE',  ( -5.608470646763013434, 5.608483241851182299, 0.4208904006049640767 ) ) ;
#164232 = CARTESIAN_POINT ( 'NONE',  ( -6.454563648557663846, 9.688018802362710957, -1.199719254218452047 ) ) ;
#164233 = CARTESIAN_POINT ( 'NONE',  ( 6.823831386379729302, 6.855558127064808716, -0.7998128361456281477 ) ) ;
#164234 = CARTESIAN_POINT ( 'NONE',  ( 3.033595934319989418, 1.863777508880835487, -0.6128360024686765328 ) ) ;
#164235 = CARTESIAN_POINT ( 'NONE',  ( 5.015626762051672571, 7.938982758113895422, 1.199719254218462483 ) ) ;
#164236 = CARTESIAN_POINT ( 'NONE',  ( -4.067982317475717480, 7.550107770606433455, 0.4684429539664070608 ) ) ;
#164237 = CARTESIAN_POINT ( 'NONE',  ( 4.532503425670185493, 4.182342172903648070, 1.214306433183764966E-14 ) ) ;
#164238 = CARTESIAN_POINT ( 'NONE',  ( -4.990809943606273613, 7.876343129965691858, -1.082531754730549967 ) ) ;
#164239 = CARTESIAN_POINT ( 'NONE',  ( -6.073689629242158716, 9.069426419882418600, -1.082531754730538864 ) ) ;
#164240 = CARTESIAN_POINT ( 'NONE',  ( 2.057031522680652369, 0.4693188842763912905, 2.067847215655476134 ) ) ;
#164241 = CARTESIAN_POINT ( 'NONE',  ( -6.934069218746458318, 7.054445274817795486, -0.7998128361456362523 ) ) ;
#164242 = CARTESIAN_POINT ( 'NONE',  ( 5.723093114104088386, -1.772945450647535948, -0.8403097561825512152 ) ) ;
#164243 = CARTESIAN_POINT ( 'NONE',  ( 3.502937704049163159, 1.705309618848281472, -1.328393843302433153 ) ) ;
#164244 = CARTESIAN_POINT ( 'NONE',  ( 2.507154105146496725, -1.820902139252629448, 0.2722148935128121394 ) ) ;
#164245 = CARTESIAN_POINT ( 'NONE',  ( -4.044208510193211481, 7.583498396275582643, -0.3544512193057146598 ) ) ;
#164246 = CARTESIAN_POINT ( 'NONE',  ( -0.3591838038534946875, -8.233137084989865073, -9.493791972417884750 ) ) ;
#164247 = CARTESIAN_POINT ( 'NONE',  ( 4.804519235412550771, 1.516407796731779722, 0.8538163389757484900 ) ) ;
#164248 = CARTESIAN_POINT ( 'NONE',  ( 11.43209210103587914, 9.944039240160840620, -3.649125173352125273 ) ) ;
#164249 = CARTESIAN_POINT ( 'NONE',  ( 3.524756749872944628, 7.056040608253000279, -0.7216878364870267237 ) ) ;
#164250 = CARTESIAN_POINT ( 'NONE',  ( 5.301814855701348250, 1.000000000000000888, 1.561251128379126385E-14 ) ) ;
#164251 = ADVANCED_FACE ( 'NONE', ( #106608 ), #140150, .T. ) ;
#164252 = CARTESIAN_POINT ( 'NONE',  ( 1.622176833581047806, -1.201014165160016356, -1.797165035535647659 ) ) ;
#164253 = CARTESIAN_POINT ( 'NONE',  ( 4.411482401463855396, 0.5350073857553553358, 1.943773423102819864 ) ) ;
#164254 = CARTESIAN_POINT ( 'NONE',  ( -8.636180661780658241, 12.05899929117736846, -1.082531754730543083 ) ) ;
#164255 = CARTESIAN_POINT ( 'NONE',  ( 1.815512348505427642, -0.2646426633909418347, 2.145385951886819242 ) ) ;
#164256 = CARTESIAN_POINT ( 'NONE',  ( 2.829319923597766628, -1.840754522440336327, 0.7060794426061881568 ) ) ;
#164257 = CARTESIAN_POINT ( 'NONE',  ( 2.835173002801576914, -1.651343842416473917, -1.157098616274463865 ) ) ;
#164258 = CARTESIAN_POINT ( 'NONE',  ( -1.737500000000000266, -2.814583332377419644, -3.009438278150923907 ) ) ;
#164259 = CARTESIAN_POINT ( 'NONE',  ( 3.474105628906531518, -1.872487600191057755, -0.5149888314514885490 ) ) ;
#164262 = VERTEX_POINT ( 'NONE', #135862 ) ;
#164261 = FILL_AREA_STYLE_COLOUR ( '', #63448 ) ;
#164260 = CARTESIAN_POINT ( 'NONE',  ( -8.636180661780651135, 13.01936850547871138, -0.7216878364870257245 ) ) ;
#164263 = CARTESIAN_POINT ( 'NONE',  ( -7.014364370223741929, 9.276787413384745662, -1.599625672291271394 ) ) ;
#164264 = CARTESIAN_POINT ( 'NONE',  ( 4.492547798081839794, 6.334668079219206049, 1.599625672291262513 ) ) ;
#164266 = ORIENTED_EDGE ( 'NONE', *, *, #15780, .F. ) ;
#164265 = CARTESIAN_POINT ( 'NONE',  ( -6.954406449166956605, 7.078172043641714595, -0.7998128361456362523 ) ) ;
#164267 = CARTESIAN_POINT ( 'NONE',  ( -9.042925270190641740, 11.57316545335434199, 1.443375672974064550 ) ) ;
#164268 = CARTESIAN_POINT ( 'NONE',  ( 1.184930176456780115, -2.153272645635353033, -0.4822455307981614592 ) ) ;
#164269 = CARTESIAN_POINT ( 'NONE',  ( 1.001543065824772753E-15, -1.771874999522040861, 3.793834371823811669 ) ) ;
#164270 = ADVANCED_FACE ( 'NONE', ( #136934 ), #170476, .T. ) ;
#164271 = CARTESIAN_POINT ( 'NONE',  ( 5.664887785843471413, 1.487927489739075959, -1.278645765186999128 ) ) ;
#164272 = CARTESIAN_POINT ( 'NONE',  ( 3.503210936237437068, -0.1516218309994079028, 2.111938774394610974 ) ) ;
#164273 = CARTESIAN_POINT ( 'NONE',  ( 1.499999999999987121, 2.577083334016147198, -0.8660254037844262731 ) ) ;
#164274 = CARTESIAN_POINT ( 'NONE',  ( 0.07479286986302942364, 7.629137130509078268, -2.455503679634089220 ) ) ;
#164275 = CARTESIAN_POINT ( 'NONE',  ( 4.593604542485023146, -1.840816577468977533, -0.04244875611379012037 ) ) ;
#164276 = ORIENTED_EDGE ( 'NONE', *, *, #24925, .F. ) ;
#164277 = CARTESIAN_POINT ( 'NONE',  ( -8.667740277838301921, 9.006785167099828016, -0.7998128361456291469 ) ) ;
#164278 = LINE ( 'NONE', #15868, #110414 ) ;
#164280 = CIRCLE ( 'NONE', #195512, 10.24999999999998934 ) ;
#164279 = CARTESIAN_POINT ( 'NONE',  ( 5.431924468521282634, -2.068440459917933794, 0.4666711972392265650 ) ) ;
#164281 =( NAMED_UNIT ( * ) PLANE_ANGLE_UNIT ( ) SI_UNIT ( $, .RADIAN. ) );
#164282 = CARTESIAN_POINT ( 'NONE',  ( 4.950698647284403009, 8.927565521807144577, 1.040834085586084257E-14 ) ) ;
#164283 = EDGE_LOOP ( 'NONE', ( #172605, #55116, #128883, #74245, #123088, #103375 ) ) ;
#164284 = CARTESIAN_POINT ( 'NONE',  ( 0.2157906144764632494, -2.021207876486079691, 0.4015242071495705445 ) ) ;
#164287 = CARTESIAN_POINT ( 'NONE',  ( 3.438839575862782549, -1.396446551253815782, -1.200180114512699792 ) ) ;
#164286 = CARTESIAN_POINT ( 'NONE',  ( 0.5021285002191768765, 1.855665429770089636, 0.1426183976328247727 ) ) ;
#164285 = LINE ( 'NONE', #15873, #211465 ) ;
#164288 = CARTESIAN_POINT ( 'NONE',  ( 7.446452682403650769, 9.710614100936176385, -1.599625672291262513 ) ) ;
#164289 = CARTESIAN_POINT ( 'NONE',  ( -10.91914056351827256, 3.934209603697781166, 3.813461610467995921 ) ) ;
#164290 = CARTESIAN_POINT ( 'NONE',  ( -7.306918443122272677, 7.489436036589583345, 0.7998128361456341429 ) ) ;
#164291 = CARTESIAN_POINT ( 'NONE',  ( -0.3870642018030946430, -8.176227079964629496, -9.516228778038646752 ) ) ;
#164292 = CARTESIAN_POINT ( 'NONE',  ( 3.826972293661185187, 2.095320012007126476, 0.6930106488920934060 ) ) ;
#164293 = CARTESIAN_POINT ( 'NONE',  ( 4.569752015286022484, 2.196007708051894269, -0.5437172964835658151 ) ) ;
#164294 = CARTESIAN_POINT ( 'NONE',  ( -6.182154858151506893, 9.195969186943299789, 1.082531754730548412 ) ) ;
#164295 = CARTESIAN_POINT ( 'NONE',  ( 4.588045372560112689, 1.048790434826195384, 1.476901585074356316 ) ) ;
#164296 = CARTESIAN_POINT ( 'NONE',  ( 5.594928181924037069, 1.692849881775596366, 0.8967378362389683000 ) ) ;
#164297 = CARTESIAN_POINT ( 'NONE',  ( -1.364683531249997417, 5.821875000341418804, 1.214306433183764966E-14 ) ) ;
#164298 = CARTESIAN_POINT ( 'NONE',  ( 5.752782329262380756, -1.473788443143897675, 1.151991621687727507 ) ) ;
#164299 = CARTESIAN_POINT ( 'NONE',  ( 6.461375281700972195, 1.547960615844719667, 1.032782510450443114 ) ) ;
#164300 = CARTESIAN_POINT ( 'NONE',  ( 0.000000000000000000, -8.233137084989849086, 0.000000000000000000 ) ) ;
#164301 = CIRCLE ( 'NONE', #88223, 6.277139874739035008 ) ;
#164302 = CARTESIAN_POINT ( 'NONE',  ( 6.350471991779750525, 0.5597436608810264502, 1.679089333223187985 ) ) ;
#164303 = CARTESIAN_POINT ( 'NONE',  ( 1.341030165941111241, -1.731997234073547220, -1.032477317303444053 ) ) ;
#164305 = CARTESIAN_POINT ( 'NONE',  ( 3.176497522518567873, -1.254329069944852382, 1.691643483388256985 ) ) ;
#164304 = CARTESIAN_POINT ( 'NONE',  ( -4.080641047588918546, 4.823464646017586510, -1.082531754730548412 ) ) ;
#164306 = AXIS2_PLACEMENT_3D ( 'NONE', #148164, #129854, #133000 ) ;
#164307 = CARTESIAN_POINT ( 'NONE',  ( 9.103410076571945453, 12.70806329172093818, 1.199719254218450271 ) ) ;
#164309 = CARTESIAN_POINT ( 'NONE',  ( -9.073431116043565225, 11.60875560684942265, -1.599625672291263179 ) ) ;
#164308 = CARTESIAN_POINT ( 'NONE',  ( 0.000000000000000000, 1.000000000000000888, 0.000000000000000000 ) ) ;
#164310 = CARTESIAN_POINT ( 'NONE',  ( 1.740496097130298958, 1.159487406938706888, -1.653631796535762755 ) ) ;
#164311 = CARTESIAN_POINT ( 'NONE',  ( -1.364683531250012516, 2.530208333674753174, 0.7879004041258379498 ) ) ;
#164312 = CARTESIAN_POINT ( 'NONE',  ( 5.332434488876471868, 5.115595079977664383, 0.7998128361456341429 ) ) ;
#164313 = CARTESIAN_POINT ( 'NONE',  ( 3.392016793147753617, -0.8794390384766533897, 1.974801309016629869 ) ) ;
#164314 = CARTESIAN_POINT ( 'NONE',  ( 6.620655732516673275, 1.290356161719278028, 1.942653802560645460 ) ) ;
#164317 = DIRECTION ( 'NONE',  ( 0.000000000000000000, 0.000000000000000000, -1.000000000000000000 ) ) ;
#164316 = CARTESIAN_POINT ( 'NONE',  ( 11.86685672517501899, 9.990810821401886699, -1.056525322636012065 ) ) ;
#164315 = CARTESIAN_POINT ( 'NONE',  ( 4.435452530326143616, 5.203724702582467998, -1.199719254218452047 ) ) ;
#164318 = CARTESIAN_POINT ( 'NONE',  ( 9.449669878600614581, 12.04770082983265844, -1.443375672974058777 ) ) ;
#164319 = CARTESIAN_POINT ( 'NONE',  ( -8.002408263929950749, -6.836568542494915413, 7.346809171966868668 ) ) ;
#164320 =( BOUNDED_CURVE ( )  B_SPLINE_CURVE ( 2, ( #179078, #148703, #164944, #162832, #14410, #16536, #80500, #130398, #48031 ),
 .UNSPECIFIED., .F., .T. ) 
 B_SPLINE_CURVE_WITH_KNOTS ( ( 3, 2, 2, 2, 3 ),
 ( 0.6041666666666667407, 0.6111111111111111605, 0.6250000000000000000, 0.6388888888888888395, 0.6458333333333333703 ),
 .UNSPECIFIED. ) 
 CURVE ( )  GEOMETRIC_REPRESENTATION_ITEM ( )  RATIONAL_B_SPLINE_CURVE ( ( 0.9330127018922192983, 0.9330127018922198534, 1.000000000000000000, 0.8660254037844387076, 1.000000000000000000, 0.8660254037844387076, 1.000000000000000000, 0.9330127018922187432, 0.9330127018922192983 ) ) 
 REPRESENTATION_ITEM ( '' )  );
#164321 = CARTESIAN_POINT ( 'NONE',  ( -7.537970219518083326, 9.817384560903001045, -1.443375672974059665 ) ) ;
#164322 = CARTESIAN_POINT ( 'NONE',  ( -0.6823417656250246877, 0.3010416670080895418, 1.181850606188755259 ) ) ;
#164323 = CARTESIAN_POINT ( 'NONE',  ( 0.8729168595149154886, -0.05911722906676297740, -2.190938979806676734 ) ) ;
#164324 = LINE ( 'NONE', #197872, #208966 ) ;
#164325 = CARTESIAN_POINT ( 'NONE',  ( 1.534417833908331863, 1.113959020207640593, -1.969227013157865303 ) ) ;
#164326 = CARTESIAN_POINT ( 'NONE',  ( -6.997979842947967377, 11.31606025008131233, -0.7998128361456291469 ) ) ;
#164327 = CARTESIAN_POINT ( 'NONE',  ( -4.080641047588918546, 4.823464646017586510, -1.082531754730548412 ) ) ;
#164328 = CARTESIAN_POINT ( 'NONE',  ( -0.6823417656249969321, 3.780208333674754506, -1.181850606188749264 ) ) ;
#164329 = CARTESIAN_POINT ( 'NONE',  ( 4.746850994788568201, 8.189453717816405742, 0.7312505120831546135 ) ) ;
#164330 = CARTESIAN_POINT ( 'NONE',  ( 0.7500000000000006661, 11.41666666666666607, -1.299038105676657340 ) ) ;
#164331 = CARTESIAN_POINT ( 'NONE',  ( 7.349928672384119288, 8.707909884937221179, 1.082531754730549967 ) ) ;
#164332 =( BOUNDED_SURFACE ( )  B_SPLINE_SURFACE ( 3, 2, ( 
 ( #196583, #80706, #129539 ),
 ( #61247, #161964, #195520 ),
 ( #113273, #130594, #13555 ),
 ( #62316, #11416, #128475 ),
 ( #47157, #143610, #213861 ),
 ( #131631, #210688, #48226 ),
 ( #81761, #178211, #28752 ),
 ( #179278, #164093, #145745 ),
 ( #197630, #96978, #15674 ),
 ( #79626, #209603, #49275 ),
 ( #211746, #30902, #114338 ),
 ( #12482, #180333, #194443 ),
 ( #127404, #46085, #146796 ),
 ( #78556, #29827, #115396 ),
 ( #212812, #181389, #144674 ),
 ( #112204, #95910, #94836 ),
 ( #31956, #45021, #64449 ),
 ( #193377, #98040, #33012 ),
 ( #177135, #152099, #2611 ),
 ( #66538, #18869, #182442 ),
 ( #69746, #3670, #199757 ),
 ( #52460, #169407, #87089 ),
 ( #68680, #67603, #183516 ),
 ( #135852, #168344, #84953 ),
 ( #86025, #153159, #4734 ),
 ( #201874, #134804, #185641 ),
 ( #133749, #198685, #36193 ),
 ( #200810, #118586, #83881 ) ),
 .UNSPECIFIED., .F., .F., .F. ) 
 B_SPLINE_SURFACE_WITH_KNOTS ( ( 4, 2, 2, 2, 2, 2, 2, 2, 2, 2, 2, 2, 2, 4 ),
 ( 3, 3 ),
 ( 8.673617379884035472E-19, 0.001863568725704640170, 0.002795353088556959929, 0.003727137451409279472, 0.004658921814261599015, 0.005590706177113918991, 0.007454274902818558077, 0.008386059265670878921, 0.009317843628523198030, 0.01024962799137551714, 0.01118141235422783625, 0.01211319671708015536, 0.01304498107993247620, 0.01490854980563711615 ),
 ( 0.000000000000000000, 1.000000000000000000 ),
 .UNSPECIFIED. ) 
 GEOMETRIC_REPRESENTATION_ITEM ( )  RATIONAL_B_SPLINE_SURFACE ( (
 ( 1.000000000000000000, 0.8462382765735652068, 1.000000000000000000),
 ( 1.000000000000000000, 0.8465420404195402870, 1.000000000000000000),
 ( 1.000000000000000000, 0.8466805660004343981, 1.000000000000000000),
 ( 1.000000000000000000, 0.8469123506191252870, 1.000000000000000000),
 ( 1.000000000000000000, 0.8470220173784553941, 1.000000000000000000),
 ( 1.000000000000000000, 0.8471957003534210662, 1.000000000000000000),
 ( 1.000000000000000000, 0.8472535244121295328, 1.000000000000000000),
 ( 1.000000000000000000, 0.8472797654243715559, 1.000000000000000000),
 ( 1.000000000000000000, 0.8469106832326384060, 1.000000000000000000),
 ( 1.000000000000000000, 0.8463026754876442626, 1.000000000000000000),
 ( 1.000000000000000000, 0.8460620800516406304, 1.000000000000000000),
 ( 1.000000000000000000, 0.8460269503523500934, 1.000000000000000000),
 ( 1.000000000000000000, 0.8472022497197664315, 1.000000000000000000),
 ( 1.000000000000000000, 0.8472231902808619042, 1.000000000000000000),
 ( 1.000000000000000000, 0.8468169758819515947, 1.000000000000000000),
 ( 1.000000000000000000, 0.8461442878182255933, 1.000000000000000000),
 ( 1.000000000000000000, 0.8458919886175331193, 1.000000000000000000),
 ( 1.000000000000000000, 0.8458966812448689421, 1.000000000000000000),
 ( 1.000000000000000000, 0.8461525964263839628, 1.000000000000000000),
 ( 1.000000000000000000, 0.8468439809311968380, 1.000000000000000000),
 ( 1.000000000000000000, 0.8472723393077549181, 1.000000000000000000),
 ( 1.000000000000000000, 0.8472611234995456320, 1.000000000000000000),
 ( 1.000000000000000000, 0.8471603390332783645, 1.000000000000000000),
 ( 1.000000000000000000, 0.8469206950638731302, 1.000000000000000000),
 ( 1.000000000000000000, 0.8467815351080468789, 1.000000000000000000),
 ( 1.000000000000000000, 0.8465568167268769928, 1.000000000000000000),
 ( 1.000000000000000000, 0.8465337723686136018, 1.000000000000000000),
 ( 1.000000000000000000, 0.8462384754710241541, 1.000000000000000000) ) ) 
 REPRESENTATION_ITEM ( '' )  SURFACE ( )  );
#164333 = CARTESIAN_POINT ( 'NONE',  ( 3.497073372749549769, 1.393195626148287403, 1.091155617269304878 ) ) ;
#164335 = AXIS2_PLACEMENT_3D ( 'NONE', #119408, #150795, #99900 ) ;
#164334 = CARTESIAN_POINT ( 'NONE',  ( 6.458075443588827014, 2.201329523236052577, -0.1558686762383256763 ) ) ;
#164336 = CARTESIAN_POINT ( 'NONE',  ( 0.6823417656249934904, 9.442708333674735499, 1.181850606188764807 ) ) ;
#164337 = ORIENTED_EDGE ( 'NONE', *, *, #54609, .T. ) ;
#164338 = CARTESIAN_POINT ( 'NONE',  ( -5.906512197408906317, 6.919960980845699439, -1.199719254218453823 ) ) ;
#164339 = CARTESIAN_POINT ( 'NONE',  ( 4.798453934790239295, 1.388474963651475269, -1.462457531588717830 ) ) ;
#164340 = EDGE_LOOP ( 'NONE', ( #8626, #164899, #91322, #60976 ) ) ;
#164341 = CARTESIAN_POINT ( 'NONE',  ( 2.324885834233282988, -0.002380789299309681549, 1.870836310375329381 ) ) ;
#164342 = CARTESIAN_POINT ( 'NONE',  ( 2.957943426865859760, -0.6537446763684885420, 1.964363857337739105 ) ) ;
#164343 = CARTESIAN_POINT ( 'NONE',  ( -7.905812970100109638, 8.396072351304486148, 0.7216878364870317197 ) ) ;
#164344 = CARTESIAN_POINT ( 'NONE',  ( 1.423922367354793606, -1.897583212610975734, 0.2371896777705190806 ) ) ;
#164345 = B_SPLINE_CURVE_WITH_KNOTS ( 'NONE', 3,
 ( #86909, #152977, #4552, #156192, #108558, #172435, #89061, #205978, #187597, #22946, #39224, #137809, #104235, #138877 ),
 .UNSPECIFIED., .F., .F.,
 ( 4, 2, 2, 2, 2, 2, 4 ),
 ( 0.003709280639842195849, 0.003956362438780343382, 0.004203444237718490482, 0.004697607835594785550, 0.004944689634532933517, 0.005191771433471080617, 0.005685935031347376552 ),
 .UNSPECIFIED. ) ;
#164347 = AXIS2_PLACEMENT_3D ( 'NONE', #9573, #83087, #48489 ) ;
#164346 = SURFACE_STYLE_USAGE ( .BOTH. , #78815 ) ;
#164348 = CARTESIAN_POINT ( 'NONE',  ( -9.912197829101469182, 5.385002637010017246, -6.113573717307969169 ) ) ;
#164349 = CARTESIAN_POINT ( 'NONE',  ( -4.344821003001812620, 7.342528190309904446, 0.9996755505292649335 ) ) ;
#164350 = EDGE_CURVE ( 'NONE', #201589, #148930, #119665, .T. ) ;
#164351 = CARTESIAN_POINT ( 'NONE',  ( 1.364683531249988535, 4.467708333674754506, -0.7879004041258300672 ) ) ;
#164352 = CARTESIAN_POINT ( 'NONE',  ( 0.9492982845318719276, -1.727743609841876138, 0.8201845251225792222 ) ) ;
#164353 = CIRCLE ( 'NONE', #143535, 11.92000000000000171 ) ;
#164354 = CARTESIAN_POINT ( 'NONE',  ( 3.016010921186715432, 1.952665002612500533, -0.1895750030070641190 ) ) ;
#164355 = CARTESIAN_POINT ( 'NONE',  ( 0.2278875137335881484, -1.799627942332830965, -0.9090566646320766830 ) ) ;
#164356 = CARTESIAN_POINT ( 'NONE',  ( -4.098307573080856692, 8.003385611894792362, 0.7998128361456352531 ) ) ;
#164358 = CARTESIAN_POINT ( 'NONE',  ( -1.279995097189637887, 3.683921063351213387, -0.4728108786798664309 ) ) ;
#164357 = CARTESIAN_POINT ( 'NONE',  ( 9.420217803396747414, 9.884675613584706255, 0.7998128361456462443 ) ) ;
#164359 = CARTESIAN_POINT ( 'NONE',  ( 6.661403070661808812, 0.3393488462513394310, -1.941789718247180607 ) ) ;
#164360 = CARTESIAN_POINT ( 'NONE',  ( -0.6823417656250003738, 2.217708333674753174, -1.181850606188749264 ) ) ;
#164361 = CARTESIAN_POINT ( 'NONE',  ( 1.635022589147613115, 1.879998146294536543, 0.7206230416607807276 ) ) ;
#164363 = CARTESIAN_POINT ( 'NONE',  ( 1.704857254432812219, 1.976886250939764889, 0.7584849220025058347 ) ) ;
#164362 = CARTESIAN_POINT ( 'NONE',  ( -5.734735788900501952, 9.634349487118505806, 0.000000000000000000 ) ) ;
#164365 = EDGE_CURVE ( 'NONE', #110637, #95923, #7250, .T. ) ;
#164364 = CARTESIAN_POINT ( 'NONE',  ( 8.810048391696772896, 13.28851571758704253, -8.147727092588480602 ) ) ;
#164366 = CARTESIAN_POINT ( 'NONE',  ( 3.262232429473245432, -2.068111870375147987, 0.09887451149894616043 ) ) ;
#164367 = CARTESIAN_POINT ( 'NONE',  ( 5.411639590510088027, 6.342609606130419131, -1.199719254218452047 ) ) ;
#164369 = CARTESIAN_POINT ( 'NONE',  ( 4.111146893441827821, 5.819424013814004759, 1.599625672291267398 ) ) ;
#164368 = CARTESIAN_POINT ( 'NONE',  ( 5.595677694052432649, -2.090823719441712747, -0.0008997866532325231618 ) ) ;
#164371 = ORIENTED_EDGE ( 'NONE', *, *, #142087, .T. ) ;
#164370 = CARTESIAN_POINT ( 'NONE',  ( 4.489149150750438189, 1.630474666268775685, -0.8212668906743822994 ) ) ;
#164372 = CARTESIAN_POINT ( 'NONE',  ( 10.40318394038753702, 11.03146944007395724, -0.7998128361456281477 ) ) ;
#164373 = CARTESIAN_POINT ( 'NONE',  ( 8.831150071590936790, 13.23551488323715830, -7.656846099933870775 ) ) ;
#164374 = CARTESIAN_POINT ( 'NONE',  ( 5.754950181447250124, -1.742976869204535761, 1.353379275444612784 ) ) ;
#164375 = CARTESIAN_POINT ( 'NONE',  ( -1.402160292154681736E-14, 10.98437500034139802, 1.575800808251682339 ) ) ;
#164376 = ORIENTED_EDGE ( 'NONE', *, *, #103129, .F. ) ;
#164377 = CARTESIAN_POINT ( 'NONE',  ( 4.688094572372190960, 1.103980140559155831, 1.561224650464939190 ) ) ;
#164378 = CARTESIAN_POINT ( 'NONE',  ( -8.299562589859897699, 12.83457345481192036, -0.7998128361456281477 ) ) ;
#164379 =( BOUNDED_SURFACE ( )  B_SPLINE_SURFACE ( 3, 3, ( 
 ( #81457, #150736, #213556, #164836, #1237, #32699, #34816, #85709, #2296, #117212, #199445, #51088, #183210, #198378, #100891, #114035, #65178, #31650, #163785, #48967, #148593, #50019, #162, #116143, #166978, #84645, #68373, #134504, #33761, #52152, #66229, #19637, #118280, #15364, #17488, #115085, #131332, #101967, #184265, #168034, #165904, #99838, #132376, #181081, #147534, #151796, #98781, #64144, #47923, #97727, #149656, #154987, #24967, #6572, #203703, #41253, #119347, #189607, #53216, #185334, #54289, #56418, #137682, #91069, #204766, #136614, #3371, #40171, #107363, #123644, #120426, #173384, #21744, #22819, #187473, #36957, #186400, #73726, #69439, #135545, #170156, #87852, #4428, #205852, #106285, #90001, #201570, #39103, #103037, #70498, #122580, #55349, #169092, #188541, #202639, #20691, #38038, #121501, #172306, #156052, #23895, #86782, #152852, #7642, #104107, #139823, #71574, #153924, #5493, #57484, #105188, #171224, #88933, #72652, #138748, #94272, #157130, #108435, #10839, #193866, #192790, #174455, #190659, #160313, #44448, #159238, #110565, #76913, #111630, #77990, #141968, #177643, #176567, #28176, #210106, #12977, #26031, #42320, #207980, #92143, #158196, #60669, #194940, #59608, #161393, #27100, #191726, #144112, #9787, #8719, #140904, #143039, #46577, #209034, #125764, #30321, #11917, #126833, #61746, #127913, #75859, #93208, #74803, #45515, #29251, #43382, #124700, #95343, #109503, #79052, #145169, #175510, #211174, #62799, #128961, #112696, #206916, #58546, #178706, #2034, #64929, #163518, #147271, #131079, #213304, #80118, #48705, #47656, #83304, #32444, #214336, #118021, #100634, #17229, #115883, #184010, #96406, #65966, #196020, #132115, #68104, #97462, #148336, #50822, #182947, #149391, #14032, #212241, #116948, #63874, #34563, #164575, #15105, #98513, #166711, #114819, #31387, #973, #16159, #198125, #33504, #162456, #113767, #82245, #133176, #49756, #179770, #130029, #99576, #181868, #165641, #67039, #199176, #18301, #84387, #81194, #150474, #134240, #200247, #51898, #146223, #197067, #180817, #86520, #52948, #185066, #153666, #73464, #20437, #39919, #120163, #70241, #22567, #36691, #35624, #19370, #103848, #139565, #87594, #152585, #123389, #137422, #5234, #37774, #169896, #102777, #186139, #101702, #88672, #6315, #4171, #3103, #71309, #136356, #21485, #138488, #168833, #201308, #188279, #202376, #54025, #85450, #151535, #203441, #155800, #55095, #121244, #187214, #38843, #104926, #69174, #170967, #119086, #154732, #72389, #204510, #57229, #106028, #56159, #122322, #167772, #135293, #172050, #23643, #89751, #7384, #205592, #191473, #90811, #174205, #96954, #189354, #40994, #9537, #75611, #124450, #80679, #44192, #163002, #24709, #175262, #107105, #42065, #110312, #109254, #196558, #126578, #108179, #26847, #59354, #125510, #25778, #141722, #156875, #60418, #179252, #91890, #74549, #92951, #157945, #43141, #30875, #207731, #206661, #14583, #158997, #10591, #8462, #140648, #76667, #64424, #142781, #208787, #192538, #146770, #212787, #58294, #130568, #190409, #173128, #104537, #71996, #192971, #172741, #89361, #187895, #44623, #168455, #138107, #53639, #204118, #186830, #39524, #55770, #135966, #137036, #24317, #20053, #86142, #120856, #38460, #169522, #156492, #205202, #40610, #152213, #121927 ),
 ( #106715, #155409, #3783, #69857, #123016, #201983, #90423, #22167, #21102, #170583, #188968, #88281, #103460, #6992, #154346, #5924, #105623, #119772, #185752, #171651, #56844, #23249, #37385, #87206, #73071, #139171, #8081, #74170, #140262, #206283, #60849, #153270, #127012, #4846, #70926, #203062, #54706, #194039, #144290, #161568, #128083, #45693, #14203, #148506, #95520, #114992, #195122, #145351, #97638, #111808, #110738, #94447, #178885, #73, #162629, #13157, #198288, #212410, #80299, #163695, #113943, #196190, #177813, #197234, #29429, #211352, #47833, #79234, #81364, #132283, #48873, #15277, #179939, #31563, #147444, #30499, #213468, #160486, #62977, #12093, #210284, #129146, #46760, #96581, #112871, #146396, #65091, #131248, #180990, #32610, #64053, #98687, #130196, #66136, #164744, #61924, #16335, #82417, #176738, #28352, #78160, #102946, #151710, #85622, #68282, #50999, #67211, #86690, #100800, #21652, #37947, #136526, #133346, #201480, #71483, #53122, #35800, #87759, #165815, #153835, #99745, #17398, #166887, #169006, #184180, #137594, #36862, #183123, #49930, #152758, #5405, #170065, #18476, #116051, #150645, #182039, #117120, #202546, #3279, #19545, #83481, #34729, #84556, #69346, #186312, #119255, #199352, #33669, #2206, #134415, #185239, #200419, #149564, #1148, #118192, #20604, #135457, #4341, #52066, #70408, #104019, #54195, #120335, #101877, #167944, #67948, #201161, #39764, #203298, #135145, #188133, #2957, #53879, #170824, #88524, #54945, #134093, #117873, #22415, #183863, #154586, #70092, #69028, #152444, #6163, #20290, #169753, #37622, #121097, #72232, #85301, #35477, #52800, #19223, #151387, #120012, #105869, #118939, #138339, #86375, #36543, #187064, #184919, #1888, #200101, #136207, #171895, #185988, #102630, #89598, #103702, #21341, #4023, #202226, #168686, #87449, #51750, #38697, #104775, #153517, #101555, #5086, #71161, #137278, #204356, #56013, #167624, #122166, #23492, #108031, #139410, #205444, #190262, #61346, #124303, #8317, #206513, #41920, #58144, #57080, #174056, #106954, #142628, #91741, #59201, #177233, #159910, #76516, #175114, #28846, #155648, #125358, #40846, #191321, #25629, #26701, #42988, #123244, #157794, #11516, #7231, #73308, #9390, #75461, #156726, #143710, #192390, #27775, #189208, #109100, #208637, #141574, #172978, #140502, #193476, #60270, #74402, #127505, #207581, #92802, #110164, #93872, #126427, #24557, #90664, #176175, #158847, #77587, #10444, #44045, #209702, #45120, #111230, #29919, #147933, #30994, #146888, #32043, #94934, #46180, #163122, #131717, #130685, #112294, #128568, #98130, #196674, #97069, #48314, #14704, #49361, #15766, #79717, #115481, #81851, #164181, #180425, #178310, #181473, #96002, #195617, #213948, #63476, #65570, #116537, #33103, #197720, #99177, #165229, #16821, #80798, #82906, #144772, #162055, #210782, #194533, #145833, #179372, #212908, #47253, #64541, #148979, #553, #66618, #132765, #114425, #198768, #50418, #182527, #160983, #13645, #12574, #211838, #129630, #78646, #62405, #113367, #135935, #69827, #52540, #35210, #51487, #70895, #85040, #5892, #22135, #120822, #117610, #185722, #55740, #37355, #20023, #71964, #150057, #138074, #83968, #1629, #151128, #87173, #168427, #121895, #21073, #167368, #34156, #137006, #204087, #154318 ),
 ( #201953, #170551, #103429, #183602, #166294, #18956, #101286, #169491, #2695, #100226, #17883, #102355, #153241, #119743, #4814, #67688, #203033, #88248, #54674, #186799, #38428, #104507, #86112, #133834, #53610, #199845, #68767, #134887, #200894, #118674, #184658, #36278, #152183, #3753, #122981, #42728, #156461, #90392, #108836, #207327, #143445, #24286, #140231, #91473, #57878, #39491, #174862, #158590, #8047, #155377, #25372, #74138, #190006, #76264, #40579, #139141, #126167, #172709, #206252, #171623, #23217, #124040, #93611, #41657, #106685, #107770, #173796, #157534, #89330, #9129, #205170, #26441, #75204, #141315, #209442, #192131, #92551, #58948, #61087, #187864, #125106, #73043, #191063, #10190, #142373, #208383, #6962, #60014, #43796, #105589, #56812, #109909, #175920, #188940, #27511, #159656, #11253, #77332, #96817, #114180, #95749, #193216, #112047, #164981, #180174, #45927, #98927, #128319, #179113, #81597, #213699, #31800, #44863, #28592, #147682, #94680, #65322, #195359, #194282, #63216, #131470, #145585, #62161, #97875, #129380, #30735, #64290, #127246, #78397, #46991, #163935, #162866, #144517, #160723, #130436, #14446, #113108, #80536, #146632, #197472, #48068, #178048, #49115, #212649, #196423, #15511, #115235, #210525, #12316, #29665, #161801, #13391, #181225, #16573, #79468, #32853, #211582, #82656, #148740, #308, #110967, #176975, #134648, #104259, #118431, #183360, #154075, #168185, #184418, #68521, #200652, #133591, #34965, #132527, #51238, #170305, #53363, #199595, #38188, #67446, #36036, #20836, #153000, #119497, #198525, #182282, #86935, #33907, #4577, #52302, #117362, #2447, #70651, #84796, #1385, #185483, #102116, #19784, #3515, #66379, #17636, #85866, #103187, #151942, #83721, #99984, #69585, #135696, #201721, #37109, #169248, #136762, #202790, #101036, #54440, #120582, #186559, #21893, #88004, #149811, #166051, #167126, #18712, #150884, #50172, #116292, #204923, #9943, #90152, #40333, #207072, #6725, #5642, #203856, #73889, #43542, #57639, #122735, #93362, #107519, #123799, #7796, #139982, #72803, #156220, #71723, #58703, #190816, #188698, #187622, #189757, #106439, #206004, #108586, #138905, #171380, #158349, #56576, #172462, #55501, #121655, #24049, #125924, #41410, #173548, #25122, #91226, #157286, #39250, #8875, #22971, #124851, #74954, #141065, #27254, #76018, #42476, #174614, #137835, #105342, #26190, #89089, #92305, #142121, #208135, #59763, #155143, #191882, #109665, #175667, #10997, #111789, #177795, #160468, #147427, #196173, #31544, #143202, #129127, #146378, #162611, #30479, #130180, #126993, #80280, #213451, #212392, #47813, #96564, #64034, #79214, #77073, #112853, #113926, #195104, #194022, #15260, #114971, #209192, #46740, #45673, #29412, #94428, #14187, #128066, #61905, #179922, #178868, #180971, #210267, #95503, #62958, #97620, #163677, #81347, #176719, #65074, #12075, #161550, #131229, #13137, #197217, #32594, #48857, #159398, #60832, #192952, #44604, #145332, #110719, #28332, #78143, #144274, #211333, #83464, #183102, #84536, #50978, #150626, #69326, #101857, #135436, #119235, #18459, #36842, #34712, #54175, #185218, #49913, #52047, #149544, #165797, #136506, #201458, #151688, #200398, #134395, #117100, #99725, #116034, #53102, #1130, #70389, #86671, #102924, #182021, #35781 ),
 ( #133329, #4319, #67192, #17381, #199333, #100782, #166864, #82399, #2187, #33651, #85600, #68263, #118173, #120315, #168985, #19524, #184160, #186289, #98670, #167925, #198270, #3258, #20585, #152737, #202526, #66120, #164725, #16314, #148489, #57, #132263, #87738, #187365, #153814, #137575, #22712, #122472, #23791, #204661, #89898, #8610, #41147, #74693, #58441, #172203, #190554, #188432, #207875, #124596, #203593, #205741, #88826, #105080, #125654, #92033, #158091, #5385, #139717, #155949, #40067, #106177, #171118, #7534, #104001, #24857, #140797, #154881, #71462, #73618, #6464, #57374, #206808, #72541, #55245, #42210, #138639, #56311, #21630, #121392, #123537, #9679, #189502, #107257, #173277, #90959, #157025, #38995, #108327, #174347, #25925, #75755, #141865, #59497, #37927, #170044, #211065, #67723, #191616, #95228, #76808, #12865, #209996, #62689, #161278, #159136, #160205, #50454, #43278, #109399, #144004, #61638, #192683, #182566, #16860, #66656, #175404, #78939, #178599, #11807, #26988, #176459, #17920, #33136, #110458, #166330, #44336, #29141, #149014, #132803, #99216, #93095, #10738, #590, #142928, #198806, #45406, #28071, #127805, #116572, #193759, #126722, #165265, #111522, #145061, #128848, #208928, #60563, #177528, #82941, #194831, #94165, #77882, #46465, #112588, #34189, #100263, #84006, #150096, #1667, #105629, #201989, #137042, #4854, #104544, #101323, #54712, #187901, #186836, #170589, #70933, #120863, #53646, #199881, #87213, #38468, #169529, #168461, #204125, #89368, #51524, #21109, #20059, #3789, #68804, #203069, #102394, #36315, #22174, #153277, #155416, #184695, #86149, #37392, #88289, #154353, #5931, #151162, #72003, #134924, #152220, #138114, #69864, #55777, #6999, #121934, #39531, #171658, #23255, #133874, #119779, #117649, #183642, #200930, #35248, #18995, #118707, #135973, #185759, #103467, #167405, #85077, #2732, #52578, #93644, #207365, #11288, #157571, #28626, #159687, #24324, #26477, #124079, #140270, #44898, #208416, #205209, #107806, #108874, #91512, #74178, #90431, #109944, #190043, #111005, #61119, #77367, #156500, #10226, #94714, #76300, #58985, #177009, #188974, #160756, #123023, #40618, #41695, #126205, #125141, #73077, #60050, #206290, #139178, #175953, #56851, #193251, #173831, #106722, #25408, #172749, #57914, #143481, #92587, #42767, #8090, #9164, #75240, #174898, #209477, #142408, #141350, #191099, #158629, #192167, #43828, #27549, #127280, #16611, #96852, #47027, #213735, #13427, #12351, #210561, #80571, #100022, #66416, #132561, #62196, #114214, #64325, #14482, #146670, #79503, #162900, #78431, #65359, #197509, #129414, #194319, #130469, #195397, #212684, #115269, #145622, #178083, #165016, #211617, #179149, #128352, #45960, #113142, #198561, #30773, #63253, #196459, #48102, #180212, #112081, #31835, #29700, #131505, #97910, #163970, #33947, #82692, #147717, #15546, #144553, #95782, #81631, #161839, #49152, #181261, #32888, #98965, #148774, #343, #50209, #116327, #182318, #118469, #184455, #167162, #154110, #202825, #38223, #149852, #135734, #153039, #134687, #17674, #150923, #203893, #4613, #84834, #137873, #18749, #3554, #120618, #104296, #70687, #83760, #67484, #186596, #133629, #170344, #19821, #2484, #102155, #21929, #36073, #101075, #136800, #168221, #69624, #103226 ),
 ( #85906, #88038, #86970, #68560, #5679, #119535, #201756, #54474, #71757, #35003, #199631, #200690, #183398, #52341, #53397, #55538, #1421, #185520, #121692, #151980, #51277, #37144, #187659, #39286, #169285, #166086, #20871, #117401, #59800, #191913, #92340, #23007, #6763, #125957, #72838, #43577, #173590, #106474, #41448, #109696, #123835, #40372, #158382, #107556, #157321, #42515, #105380, #56610, #25160, #142154, #141100, #122774, #138942, #108621, #207111, #91262, #58738, #8912, #175700, #26225, #90192, #27290, #124890, #190854, #9975, #93397, #188734, #204963, #156255, #172501, #24087, #74992, #143234, #7834, #159433, #189797, #140018, #76053, #73925, #171419, #89125, #174649, #192986, #11032, #77110, #155179, #208169, #209224, #60866, #127028, #206043, #57677, #110755, #31580, #15295, #161586, #12108, #96597, #13174, #46776, #147464, #111827, #210300, #197252, #29446, #211369, #28368, #94463, #79252, #164764, #145370, #177829, #95537, #62994, #129163, #160503, #195140, #61940, #97654, #112890, #162647, #66155, #48891, #179957, #64070, #132300, #44640, #14220, #144306, #80315, #178902, #130214, #146415, #78178, #30516, #115011, #176753, #128098, #212428, #196207, #45708, #32628, #81380, #47849, #113960, #163713, #98705, #213485, #131265, #194056, #65109, #181008, #16354, #82434, #148524, #90, #185259, #117138, #170086, #199371, #35820, #152779, #70430, #36883, #116068, #99765, #4361, #165832, #136546, #52083, #51017, #134434, #202566, #2225, #133364, #102966, #200436, #101896, #135476, #198307, #149582, #118210, #20622, #19567, #1166, #17416, #201498, #85641, #184197, #151727, #167961, #54218, #119274, #183141, #120356, #3299, #69367, #169024, #186333, #67230, #83500, #34746, #100819, #166904, #53144, #21673, #18497, #37967, #68300, #84575, #86710, #150663, #49947, #182058, #104040, #71505, #87781, #153855, #33688, #5426, #189539, #139759, #205783, #204700, #7574, #203632, #124637, #108364, #40104, #105118, #41187, #106216, #57412, #25966, #56350, #88866, #75796, #122512, #89935, #121433, #187402, #172242, #43319, #23830, #188473, #155986, #73659, #123577, #39034, #107294, #154921, #190594, #173316, #24895, #159175, #141904, #58481, #157064, #10775, #137616, #91001, #22748, #8652, #74731, #140836, #206849, #171158, #42251, #207914, #55284, #6505, #9720, #174388, #72580, #138681, #92071, #158129, #59535, #125695, #191654, #109437, #175443, #27028, #93136, #129963, #12903, #128891, #13968, #76849, #28109, #145102, #113701, #112629, #94204, #110499, #80052, #178639, #78983, #30251, #211106, #31322, #212171, #61677, #97398, #96335, #162391, #195951, #147211, #160244, #176498, #127845, #11844, #77921, #194872, #114758, #193797, #81126, #161319, #111561, #63805, #144040, #142968, #60603, #62730, #164512, #131013, #197005, #126762, #146155, #46506, #47587, #179705, #210037, #163454, #208971, #15034, #213236, #45446, #44376, #64868, #177569, #48640, #180755, #29182, #95271, #32382, #98448, #192722, #214273, #65906, #50755, #136292, #199110, #83242, #66974, #116884, #133113, #132052, #182883, #181806, #3044, #166646, #134177, #37712, #20377, #151473, #35561, #103788, #16096, #200185, #115819, #51838, #34499, #101642, #117956, #198062, #100573, #86462, #82180, #148274, #18237, #84321, #17168, #4111, #52889, #102715, #49691 ),
 ( #185006, #33439, #150407, #99516, #165573, #183951, #53962, #905, #152526, #1974, #68037, #69113, #149327, #167708, #19310, #85389, #135235, #70180, #202313, #201248, #119024, #36630, #168772, #120100, #186078, #39854, #21426, #156811, #140587, #72320, #137363, #7319, #138426, #171984, #58227, #22498, #121181, #108113, #154665, #122255, #153602, #5174, #204445, #75546, #56099, #88610, #6251, #188214, #105960, #71247, #23576, #187150, #8398, #89685, #73397, #191406, #174140, #90751, #189289, #43073, #169839, #139500, #55033, #205528, #155734, #40931, #57163, #203380, #123326, #25714, #87535, #38779, #107035, #173061, #170905, #157880, #206599, #42005, #104861, #24641, #74482, #124385, #190343, #91823, #207667, #9473, #141655, #59286, #125445, #161065, #63558, #195699, #96085, #26781, #10527, #129714, #76601, #47333, #177316, #110247, #45200, #113448, #127590, #44127, #162139, #111313, #12656, #46259, #109186, #60349, #28931, #145912, #144854, #126512, #142714, #112377, #210861, #95015, #62487, #78729, #179453, #30000, #93954, #31076, #128651, #194617, #13727, #97150, #192474, #143790, #14787, #77670, #176256, #159995, #209786, #11596, #92886, #61423, #27857, #79800, #178389, #211924, #130762, #163204, #80878, #146968, #196758, #175198, #212984, #208723, #64623, #193557, #158931, #17973, #15847, #16910, #118757, #114511, #180507, #642, #66707, #49442, #36369, #85127, #134974, #32127, #84060, #35301, #82990, #98208, #33185, #86198, #101378, #181557, #20112, #115561, #100315, #2783, #200982, #167453, #164259, #81932, #68854, #148018, #52629, #116626, #99267, #198857, #184742, #132852, #197809, #19048, #50504, #166381, #199931, #48398, #214028, #182620, #151213, #150149, #65653, #131800, #51578, #1719, #34243, #67776, #133925, #102446, #183694, #165315, #168512, #117703, #152270, #3842, #69915, #149065, #136026, #38518, #4906, #137096, #105682, #28410, #186886, #209262, #72054, #22227, #191949, #203122, #202039, #185811, #55830, #78221, #44681, #110793, #37443, #92377, #39580, #204173, #121986, #54765, #138166, #53700, #43615, #175740, #104596, #169579, #171711, #170642, #187952, #93435, #120913, #153332, #143272, #88341, #154405, #103521, #21162, #10014, #119832, #87266, #23308, #70983, #158413, #5983, #76090, #142192, #208207, #59838, #60908, #125991, #109733, #27333, #159475, #11073, #193028, #77151, #127066, #176795, #94504, #160542, #12148, #210343, #129207, #182101, #131305, #63040, #116110, #145410, #196248, #98749, #16399, #197296, #61983, #45749, #164806, #111868, #82477, #212471, #211409, #80357, #148566, #162691, #79292, #48937, #146456, #47892, #81424, #144343, #95576, #64115, #181053, #179999, #161626, #177872, #147505, #31623, #130257, #97697, #114004, #133, #65149, #195184, #66201, #163755, #15335, #115056, #132346, #13219, #29484, #46817, #112931, #178944, #213526, #33732, #30558, #198351, #14265, #96637, #32669, #49991, #128137, #194101, #99809, #17460, #165874, #120397, #67271, #3340, #19610, #184236, #35860, #166948, #52126, #149626, #185302, #169064, #2268, #199414, #85682, #68344, #101939, #86753, #18540, #117183, #70470, #84617, #200480, #133409, #1208, #134478, #186372, #118255, #150706, #168004, #151770, #69410, #51059, #135517, #183184, #36925, #201539, #53187, #21713, #136587, #119315, #103008, #20661 ),
 ( #87824, #152823, #38007, #104079, #4399, #170128, #202607, #83545, #54260, #34788, #100863, #32291, #30158, #47499, #63718, #98357, #199022, #131961, #212079, #194782, #195859, #146066, #65814, #129876, #62642, #34410, #130921, #197972, #148185, #33346, #96246, #49602, #116795, #115726, #99428, #214186, #181717, #196914, #128800, #16006, #165482, #164422, #97307, #133023, #18146, #46419, #82092, #163366, #147124, #113608, #17078, #31234, #179612, #83156, #149236, #84234, #14942, #81038, #180666, #810, #66879, #50669, #79963, #182792, #213150, #64780, #100482, #48554, #166558, #150322, #112536, #178548, #162298, #13884, #114673, #56124, #188240, #208752, #89712, #42030, #124412, #141684, #158960, #172011, #122282, #139526, #105991, #23603, #206626, #126541, #73425, #92914, #173089, #123351, #75575, #155762, #88635, #72348, #156837, #176284, #142744, #60378, #138450, #190370, #140614, #90776, #8424, #7346, #24670, #154693, #207697, #59318, #205552, #39880, #57191, #189318, #58256, #40956, #74510, #191435, #107064, #108142, #26812, #174168, #25740, #204471, #91851, #157908, #192503, #9503, #125475, #43102, #109216, #175227, #10555, #76629, #44154, #110275, #6276, #145939, #49469, #32154, #163232, #47362, #115588, #27886, #211951, #127618, #63586, #46289, #113476, #129743, #209816, #210888, #98232, #93983, #160025, #194647, #112406, #28958, #15875, #64649, #114538, #11624, #195726, #14814, #62513, #77698, #12682, #65681, #80905, #161093, #214053, #95043, #79829, #196784, #180532, #146996, #143819, #61451, #48425, #193582, #164287, #96112, #78758, #178417, #81960, #30027, #177346, #213013, #162168, #179483, #31105, #45226, #111341, #13755, #130789, #97178, #144882, #128678, #148045, #131828, #197837, #68883, #183722, #149091, #66739, #87295, #182650, #135002, #2811, #20141, #37472, #50530, #673, #18003, #198884, #116653, #85159, #4935, #166408, #185840, #51609, #1748, #168544, #34272, #181582, #165342, #35331, #54797, #21192, #153364, #16937, #201013, #19078, #101410, #167483, #100344, #117733, #33211, #86228, #152299, #137124, #84093, #133954, #151242, #3872, #184774, #52660, #150180, #53730, #67805, #199961, #118788, #36400, #69945, #203153, #119862, #136057, #102478, #202070, #103550, #169610, #71011, #83018, #99295, #132882, #6016, #105713, #205292, #106800, #73155, #172829, #91593, #124157, #157645, #141430, #40697, #59056, #56930, #76373, #207437, #72085, #74255, #171741, #187984, #92659, #41773, #38548, #155500, #156578, #139262, #122016, #138197, #9242, #23338, #158701, #108949, #125213, #204207, #57994, #142480, #190119, #24400, #10300, #22261, #208488, #170673, #88370, #89448, #173913, #90513, #120946, #107885, #39610, #186918, #75314, #104626, #26551, #7083, #154436, #123103, #55860, #189060, #191175, #140349, #8171, #206368, #25487, #42842, #174969, #196534, #129490, #209552, #192241, #193324, #143558, #63330, #61196, #60124, #31910, #128425, #195472, #145696, #30849, #27623, #47104, #114289, #113219, #96927, #211694, #179224, #194392, #126283, #13504, #162978, #95858, #94786, #130542, #15621, #43903, #161914, #160835, #144624, #127355, #14556, #28701, #177084, #80654, #79577, #78506, #146744, #29774, #93723, #12426, #48176, #110017, #176030, #210638, #62265, #44972, #180287, #212763, #64398, #159762, #97987, #164046 ) ),
 .UNSPECIFIED., .T., .F., .T. ) 
 B_SPLINE_SURFACE_WITH_KNOTS ( ( 4, 3, 4 ),
 ( 4, 1, 1, 1, 1, 1, 1, 1, 1, 1, 1, 1, 1, 1, 1, 1, 1, 1, 1, 1, 1, 1, 1, 1, 1, 1, 1, 1, 1, 1, 1, 1, 1, 1, 1, 1, 1, 1, 1, 1, 1, 1, 1, 1, 1, 1, 1, 1, 1, 1, 1, 1, 1, 1, 1, 1, 1, 1, 1, 1, 1, 1, 1, 1, 1, 1, 1, 1, 1, 1, 1, 1, 1, 1, 1, 1, 1, 1, 1, 1, 1, 1, 1, 1, 1, 1, 1, 1, 1, 1, 1, 1, 1, 1, 1, 1, 1, 1, 1, 1, 1, 1, 1, 1, 1, 1, 1, 1, 1, 1, 1, 1, 1, 1, 1, 1, 1, 1, 1, 1, 1, 1, 1, 1, 1, 1, 1, 1, 1, 1, 1, 1, 1, 1, 1, 1, 1, 1, 1, 1, 1, 1, 1, 1, 1, 1, 1, 1, 1, 1, 1, 1, 1, 1, 1, 1, 1, 1, 1, 1, 1, 1, 1, 1, 1, 1, 1, 1, 1, 1, 1, 1, 1, 1, 1, 1, 1, 1, 1, 1, 1, 1, 1, 1, 1, 1, 1, 1, 1, 1, 1, 1, 1, 1, 1, 1, 1, 1, 1, 1, 1, 1, 1, 1, 1, 1, 1, 1, 1, 1, 1, 1, 1, 1, 1, 1, 1, 1, 1, 1, 1, 1, 1, 1, 1, 1, 1, 1, 1, 1, 1, 1, 1, 1, 1, 1, 1, 1, 1, 1, 1, 1, 1, 1, 1, 1, 1, 1, 1, 1, 1, 1, 1, 1, 1, 1, 1, 1, 1, 1, 1, 1, 1, 1, 1, 1, 1, 1, 1, 1, 1, 1, 1, 1, 1, 1, 1, 1, 1, 1, 1, 1, 1, 1, 1, 1, 1, 1, 1, 1, 1, 1, 1, 1, 1, 1, 1, 1, 1, 1, 1, 1, 1, 1, 1, 1, 1, 1, 1, 1, 1, 1, 1, 1, 1, 1, 1, 1, 1, 1, 1, 1, 1, 1, 1, 1, 1, 1, 1, 1, 1, 1, 1, 1, 1, 1, 1, 1, 1, 1, 1, 1, 1, 1, 1, 1, 1, 1, 1, 1, 1, 1, 1, 1, 1, 1, 1, 1, 1, 1, 1, 1, 1, 1, 1, 1, 1, 1, 1, 1, 1, 1, 1, 1, 1, 1, 1, 1, 1, 1, 1, 1, 1, 1, 4 ),
 ( 0.000000000000000000, 0.5000000000000000000, 1.000000000000000000 ),
 ( 0.000000000000000000, 0.002600209826155936224, 0.005208878553436857226, 0.007813350965615119270, 0.01041570154746907992, 0.01302155883015148306, 0.01562460066207539862, 0.01822947720112986364, 0.02083337797298438765, 0.02343721533725894035, 0.02604213897589890969, 0.02864525980212044229, 0.03125073504456635232, 0.03385369766904555017, 0.03645898980682723417, 0.03906240375024701977, 0.04166680464497042602, 0.04427120869897264999, 0.04687461886132015393, 0.04947991130494613921, 0.05208287402783655373, 0.05468834688957619622, 0.05729146186993632622, 0.05989639238693608009, 0.06250023923939096449, 0.06510408216679804128, 0.06770901469741306966, 0.07031212675311915294, 0.07291759917081726272, 0.07552056149378454097, 0.07812585104223603027, 0.08072926279340975064, 0.08333366149866272554, 0.08593806365491549193, 0.08854147146176674643, 0.09114676191340240208, 0.09374972248801059782, 0.09635519323906190092, 0.09895830628708340848, 0.1015632345865536273, 0.1041670796237980645, 0.1067709202568039306, 0.1093758509056654005, 0.1119789607794838548, 0.1145844312107493490, 0.1171873915655986947, 0.1197926790194954738, 0.1223960889855860712, 0.1250004854864837645, 0.1276048858798866925, 0.1302082914968497596, 0.1328135800830011481, 0.1354165386474412147, 0.1380220074263333041, 0.1406251186789811980, 0.1432300448973659046, 0.1458338882574615747, 0.1484377267335943440, 0.1510426556371624596, 0.1536457634674935069, 0.1562512320483212536, 0.1588541905735017246, 0.1614594760690261366, 0.1640628843880489185, 0.1666672788216651824, 0.1692716775892487424, 0.1718750811543677814, 0.1744803680111783883, 0.1770833247038955116, 0.1796887916465979840, 0.1822919012421508056, 0.1848968255159594287, 0.1875006673364670307, 0.1901045037933276616, 0.1927094310880738681, 0.1953125370132051675, 0.1979180038795354257, 0.2005209607134520455, 0.2031262443867272172, 0.2057296511966431873, 0.2083340436999963075, 0.2109384409787386505, 0.2135418426300015604, 0.2161471278935624962, 0.2187500828529475860, 0.2213555480953768861, 0.2239586561720615654, 0.2265635786377499516, 0.2291674190561798496, 0.2317712536313151217, 0.2343761794536610432, 0.2369792836118274071, 0.2395847488995502261, 0.2421877041805577391, 0.2447929861676560459, 0.2473963916063780244, 0.2500007823164346887, 0.2526051782432667259, 0.2552085781186103075, 0.2578138619249652486, 0.2604168152893601151, 0.2630222789673848927, 0.2656253856633817301, 0.2682303064573571261, 0.2708341456111751366, 0.2734379784420828963, 0.2760429029284052760, 0.2786460054577940548, 0.2812514693027542978, 0.2838544231691620401, 0.2864597036061101165, 0.2890631078115080133, 0.2916674968651886135, 0.2942718915769991783, 0.2968752898143142138, 0.2994805722994643427, 0.3020835242071668869, 0.3046889864566129091, 0.3072920919100609050, 0.3098970111686871198, 0.3125008491953192857, 0.3151046804194536644, 0.3177096037060897493, 0.3203127047448455222, 0.3229181672828482230, 0.3255211198729257016, 0.3281263988957095479, 0.3307298020056156362, 0.3333341895397992083, 0.3359385831734401084, 0.3385419799105768290, 0.3411472612104861635, 0.3437502117997557338, 0.3463556727564109927, 0.3489587771054129539, 0.3515636949650152721, 0.3541675320018531359, 0.3567713617566292128, 0.3593762839798815834, 0.3619793836661120978, 0.3645848450329270407, 0.3671877964849088460, 0.3697930742294792128, 0.3723964763816929868, 0.3750008625332226786, 0.3776052552255140804, 0.3802086506002868016, 0.3828139308508870520, 0.3854168802599494681, 0.3880223400595693151, 0.3906254434421968513, 0.3932303600390676390, 0.3958341962234732669, 0.3984380246462727593, 0.4010429459424146859, 0.4036460444141952153, 0.4062515047455624306, 0.4088544551976535102, 0.4114597317999305615, 0.4140631331322238151, 0.4166675180379114662, 0.4192719099256467796, 0.4218753040758395079, 0.4244805834130354061, 0.4270835317800880659, 0.4296889905584002634, 0.4322920931126992272, 0.4348970085831024290, 0.4375008440524135733, 0.4401046712805898320, 0.4427095917858701601, 0.4453126891812490551, 0.4479181486128839262, 0.4505210982032648026, 0.4531263737991432228, 0.4557297744492659897, 0.4583341582458977381, 0.4609385494658484461, 0.4635419425292200413, 0.4661472210888942258, 0.4687501685521111572, 0.4713556264448209299, 0.4739587283088163017, 0.4765636427889929916, 0.4791674776805284197, 0.4817713038514113699, 0.4843762237020596273, 0.4869793201590638665, 0.4895847788266616818, 0.4921877276934932821, 0.4947930024188478271, 0.4973964025245324327, 0.5000007853488734888, 0.5026051760377950872, 0.5052085681520839255, 0.5078138460701020485, 0.5104167927676396266, 0.5130222499104345468, 0.5156253512221359303, 0.5182302648483090302, 0.5208340992993732987, 0.5234379245502747136, 0.5260428438825063280, 0.5286459395391455152, 0.5312513975783873521, 0.5338543458598166147, 0.5364596198505067193, 0.5390630195494738874, 0.5416674015382738627, 0.5442717918329101900, 0.5468751831358398263, 0.5494804605480556603, 0.5520834066180569932, 0.5546888631466128095, 0.5572919640440190392, 0.5598968769523987588, 0.5625007111002878757, 0.5651045355685063720, 0.5677094545185276120, 0.5703125495128006373, 0.5729180070593572482, 0.5755209548935220631, 0.5781262282853970591, 0.5807296277153600750, 0.5833340090053582561, 0.5859383990424469335, 0.5885417896717308750, 0.5911470667139914204, 0.5937500122945923442, 0.5963554683445766447, 0.5989585689656815592, 0.6015634812924701702, 0.6041673152744758690, 0.6067711390973024033, 0.6093760578013157625, 0.6119791522712144660, 0.6145846094607528842, 0.6171875569857874222, 0.6197928299146914233, 0.6223962292133623508, 0.6250006099412922511, 0.6276049998575695676, 0.6302083899509167697, 0.6328136667590675835, 0.6354166119884008257, 0.6380220676954796444, 0.6406251681782773044, 0.6432300800596744139, 0.6458339140130902045, 0.6484377373278128465, 0.6510426559220214848, 0.6536457500055372627, 0.6562512069737248543, 0.6588541543277639523, 0.6614594269295416273, 0.6640628262346358612, 0.6666672065372305500, 0.6692715964694370134, 0.6718749861645568755, 0.6744802628744462902, 0.6770832078906477980, 0.6796886633904898334, 0.6822917638729786294, 0.6848966754451861760, 0.6875005095073121186, 0.6901043324512210475, 0.6927092510718347862, 0.6953123449069624762, 0.6979178017894718256, 0.7005207491106575368, 0.7031260215211581066, 0.7057294209703992571, 0.7083338009843969107, 0.7109381910692819107, 0.7135415805038890502, 0.7161468572513741693, 0.7187498021925872171, 0.7213552576208688283, 0.7239583582410578089, 0.7265632696402853918, 0.7291671039484327599, 0.7317709266588259265, 0.7343758454420658000, 0.7369789391668094547, 0.7395843960993241373, 0.7421873435258099505, 0.7447926158808931829, 0.7473960156120186271, 0.7500003954741673029, 0.7526047858484943287, 0.7552081751603144655, 0.7578134520812660480, 0.7604163970856469001, 0.7630218525780576577, 0.7656249534739711926, 0.7682298648364407345, 0.7708336995279378989, 0.7734375221421257995, 0.7760424412242287184, 0.7786455349766069345, 0.7812509920948264019, 0.7838539397647821261, 0.7864592122003229990, 0.7890626123510894319, 0.7916669921981516200, 0.7942713829987035901, 0.7968747723254782089, 0.7994800495557851105, 0.8020829947615083499, 0.8046884504537559213, 0.8072915517634385862, 0.8098964632253897733, 0.8125002984375870874, 0.8151041210928977598, 0.8177090406101226172, 0.8203121345281733090, 0.8229175919678175521, 0.8255205400194353116, 0.8281258126713292311, 0.8307292133795166622, 0.8333335933482756142, 0.8359379847118599827, 0.8385413741913512187, 0.8411466518669262760, 0.8437495974121898001, 0.8463550534400045011, 0.8489581553015269622, 0.8515630669992224622, 0.8541669028694969246, 0.8567707257032814994, 0.8593756457919137226, 0.8619787400136992295, 0.8645841979105142183, 0.8671871464820134490, 0.8697924194861808012, 0.8723958208895988831, 0.8750002011168627192, 0.8776045931803160283, 0.8802079829503125508, 0.8828132612070975771, 0.8854162072301272612, 0.8880216637292678294, 0.8906247662807315058, 0.8932296783504612980, 0.8958335150162225480, 0.8984373381658604663, 0.9010422589622166800, 0.9036453536258294283, 0.9062508121155921081, 0.9088537613452241093, 0.9114590348376164775, 0.9140624370741091687, 0.9166668176967164294, 0.9192712105969091940, 0.9218746007952320909, 0.9244798797692056480, 0.9270828264082496828, 0.9296882835145078294, 0.9322913868941045124, 0.9348962994721256026, 0.9375001370706889103, 0.9401039606740361210, 0.9427088823143441321, 0.9453119775565693717, 0.9479174367776000976, 0.9505203868030935865, 0.9531256609099927335, 0.9557290641454977420, 0.9583334452981105978, 0.9609378390199675435, 0.9635412300619400350, 0.9661465102466426647, 0.9687494557931184413, 0.9713549143510965544, 0.9739580252604012056, 0.9765629275426017664, 0.9791667581373608709, 0.9817706348486141543, 0.9843755007711335603, 0.9869785191422796311, 0.9895843624858681187, 0.9921867025132995455, 0.9947911529560371502, 0.9973998138561904758, 1.000000000000000000 ),
 .UNSPECIFIED. ) 
 GEOMETRIC_REPRESENTATION_ITEM ( )  RATIONAL_B_SPLINE_SURFACE ( (
 ( 1.000000000000000222, 1.000000000000000222, 0.9999999999999997780, 1.000000000000000222, 1.000000000000000000, 1.000000000000000000, 0.9999999999999997780, 1.000000000000000000, 1.000000000000000000, 1.000000000000000000, 1.000000000000000000, 1.000000000000000222, 1.000000000000000000, 1.000000000000000000, 1.000000000000000222, 0.9999999999999994449, 1.000000000000000222, 1.000000000000000000, 0.9999999999999997780, 1.000000000000000444, 1.000000000000000000, 1.000000000000000222, 1.000000000000000000, 1.000000000000000000, 0.9999999999999996669, 1.000000000000000000, 1.000000000000000222, 0.9999999999999996669, 1.000000000000000222, 1.000000000000000000, 1.000000000000000222, 1.000000000000000000, 1.000000000000000222, 0.9999999999999997780, 1.000000000000000444, 1.000000000000000000, 1.000000000000000222, 0.9999999999999997780, 1.000000000000000222, 1.000000000000000000, 1.000000000000000000, 0.9999999999999997780, 1.000000000000000000, 0.9999999999999997780, 1.000000000000000000, 0.9999999999999997780, 1.000000000000000000, 1.000000000000000000, 0.9999999999999997780, 1.000000000000000000, 1.000000000000000222, 0.9999999999999996669, 1.000000000000000000, 1.000000000000000000, 1.000000000000000222, 0.9999999999999997780, 1.000000000000000444, 1.000000000000000000, 0.9999999999999997780, 1.000000000000000000, 1.000000000000000000, 1.000000000000000000, 1.000000000000000222, 1.000000000000000000, 1.000000000000000000, 1.000000000000000222, 1.000000000000000000, 1.000000000000000000, 0.9999999999999997780, 1.000000000000000222, 1.000000000000000000, 0.9999999999999997780, 1.000000000000000000, 1.000000000000000000, 1.000000000000000000, 1.000000000000000000, 1.000000000000000222, 0.9999999999999996669, 1.000000000000000444, 0.9999999999999996669, 1.000000000000000000, 0.9999999999999996669, 1.000000000000000444, 1.000000000000000000, 1.000000000000000000, 1.000000000000000222, 1.000000000000000000, 1.000000000000000000, 1.000000000000000222, 0.9999999999999997780, 1.000000000000000000, 1.000000000000000444, 0.9999999999999997780, 1.000000000000000444, 0.9999999999999997780, 1.000000000000000000, 1.000000000000000222, 1.000000000000000000, 0.9999999999999997780, 1.000000000000000222, 1.000000000000000222, 0.9999999999999997780, 1.000000000000000000, 1.000000000000000222, 0.9999999999999997780, 1.000000000000000444, 0.9999999999999997780, 1.000000000000000444, 0.9999999999999997780, 1.000000000000000000, 1.000000000000000222, 0.9999999999999996669, 1.000000000000000000, 1.000000000000000000, 1.000000000000000444, 1.000000000000000222, 0.9999999999999997780, 1.000000000000000222, 1.000000000000000222, 1.000000000000000000, 1.000000000000000222, 0.9999999999999997780, 1.000000000000000000, 1.000000000000000222, 0.9999999999999996669, 1.000000000000000000, 1.000000000000000000, 1.000000000000000000, 1.000000000000000000, 1.000000000000000000, 1.000000000000000000, 1.000000000000000000, 0.9999999999999997780, 1.000000000000000222, 0.9999999999999997780, 1.000000000000000000, 0.9999999999999997780, 1.000000000000000222, 1.000000000000000000, 1.000000000000000000, 1.000000000000000000, 1.000000000000000222, 0.9999999999999997780, 0.9999999999999997780, 1.000000000000000222, 1.000000000000000222, 1.000000000000000000, 1.000000000000000444, 0.9999999999999996669, 1.000000000000000444, 0.9999999999999997780, 1.000000000000000222, 1.000000000000000000, 1.000000000000000000, 1.000000000000000000, 1.000000000000000222, 0.9999999999999997780, 0.9999999999999997780, 1.000000000000000444, 1.000000000000000444, 0.9999999999999997780, 1.000000000000000000, 1.000000000000000000, 1.000000000000000000, 1.000000000000000222, 1.000000000000000000, 1.000000000000000000, 1.000000000000000222, 1.000000000000000222, 1.000000000000000000, 1.000000000000000444, 1.000000000000000000, 1.000000000000000222, 1.000000000000000000, 1.000000000000000000, 1.000000000000000444, 1.000000000000000000, 1.000000000000000222, 1.000000000000000000, 1.000000000000000222, 0.9999999999999997780, 1.000000000000000222, 1.000000000000000222, 1.000000000000000000, 0.9999999999999996669, 1.000000000000000222, 1.000000000000000000, 1.000000000000000000, 1.000000000000000222, 1.000000000000000222, 1.000000000000000222, 0.9999999999999997780, 1.000000000000000000, 1.000000000000000222, 1.000000000000000000, 1.000000000000000000, 1.000000000000000000, 0.9999999999999996669, 1.000000000000000444, 1.000000000000000222, 0.9999999999999996669, 1.000000000000000444, 1.000000000000000000, 1.000000000000000000, 1.000000000000000222, 0.9999999999999997780, 1.000000000000000444, 0.9999999999999997780, 0.9999999999999997780, 1.000000000000000444, 0.9999999999999997780, 1.000000000000000222, 1.000000000000000000, 1.000000000000000000, 1.000000000000000000, 0.9999999999999997780, 1.000000000000000000, 1.000000000000000222, 0.9999999999999996669, 1.000000000000000222, 1.000000000000000000, 1.000000000000000222, 0.9999999999999996669, 0.9999999999999997780, 1.000000000000000444, 0.9999999999999997780, 0.9999999999999997780, 1.000000000000000000, 1.000000000000000222, 1.000000000000000000, 1.000000000000000000, 0.9999999999999996669, 1.000000000000000222, 1.000000000000000000, 0.9999999999999997780, 1.000000000000000000, 1.000000000000000000, 0.9999999999999997780, 1.000000000000000444, 0.9999999999999996669, 1.000000000000000444, 0.9999999999999997780, 1.000000000000000000, 1.000000000000000222, 0.9999999999999997780, 1.000000000000000222, 1.000000000000000222, 0.9999999999999997780, 1.000000000000000000, 1.000000000000000000, 1.000000000000000000, 1.000000000000000222, 1.000000000000000000, 1.000000000000000000, 1.000000000000000222, 1.000000000000000222, 1.000000000000000000, 1.000000000000000000, 1.000000000000000222, 0.9999999999999997780, 1.000000000000000000, 1.000000000000000222, 1.000000000000000000, 1.000000000000000222, 0.9999999999999997780, 1.000000000000000222, 0.9999999999999997780, 1.000000000000000222, 0.9999999999999997780, 1.000000000000000222, 1.000000000000000000, 1.000000000000000000, 1.000000000000000444, 0.9999999999999996669, 1.000000000000000222, 0.9999999999999997780, 1.000000000000000000, 1.000000000000000222, 1.000000000000000000, 1.000000000000000222, 0.9999999999999997780, 0.9999999999999997780, 1.000000000000000000, 0.9999999999999997780, 1.000000000000000000, 1.000000000000000000, 1.000000000000000222, 1.000000000000000000, 1.000000000000000000, 1.000000000000000222, 1.000000000000000000, 1.000000000000000000, 1.000000000000000000, 1.000000000000000000, 0.9999999999999997780, 1.000000000000000222, 1.000000000000000222, 0.9999999999999997780, 1.000000000000000444, 1.000000000000000444, 0.9999999999999997780, 1.000000000000000000, 0.9999999999999997780, 1.000000000000000000, 1.000000000000000000, 1.000000000000000000, 1.000000000000000000, 0.9999999999999997780, 1.000000000000000222, 1.000000000000000000, 0.9999999999999997780, 1.000000000000000222, 1.000000000000000000, 1.000000000000000000, 1.000000000000000000, 1.000000000000000444, 1.000000000000000000, 0.9999999999999997780, 0.9999999999999997780, 0.9999999999999997780, 1.000000000000000222, 1.000000000000000222, 0.9999999999999996669, 1.000000000000000222, 0.9999999999999997780, 1.000000000000000222, 1.000000000000000000, 1.000000000000000000, 0.9999999999999996669, 1.000000000000000222, 1.000000000000000222, 1.000000000000000000, 1.000000000000000000, 1.000000000000000222, 0.9999999999999997780, 1.000000000000000000, 1.000000000000000222, 0.9999999999999994449, 1.000000000000000222, 1.000000000000000000, 1.000000000000000222, 0.9999999999999997780, 1.000000000000000000, 1.000000000000000000, 0.9999999999999997780, 1.000000000000000000, 1.000000000000000222, 0.9999999999999997780, 1.000000000000000000, 1.000000000000000000, 1.000000000000000000, 1.000000000000000000, 1.000000000000000222, 1.000000000000000000, 0.9999999999999996669, 0.9999999999999996669, 1.000000000000000222, 0.9999999999999997780, 1.000000000000000222, 1.000000000000000000, 0.9999999999999997780, 1.000000000000000222, 0.9999999999999997780, 1.000000000000000444, 1.000000000000000222, 1.000000000000000000, 1.000000000000000222, 1.000000000000000222, 1.000000000000000000, 1.000000000000000000, 1.000000000000000000, 1.000000000000000000, 1.000000000000000000, 1.000000000000000000, 1.000000000000000000, 0.9999999999999997780, 1.000000000000000000, 0.9999999999999996669, 1.000000000000000444, 0.9999999999999996669, 1.000000000000000000, 1.000000000000000000, 0.9999999999999997780, 1.000000000000000444, 1.000000000000000000, 1.000000000000000000, 1.000000000000000000),
 ( 0.3333333333333334259, 0.3333333333333334259, 0.3333333333333333703, 0.3333333333333333703, 0.3333333333333334259, 0.3333333333333333703, 0.3333333333333333703, 0.3333333333333334259, 0.3333333333333333148, 0.3333333333333334814, 0.3333333333333332593, 0.3333333333333335369, 0.3333333333333333148, 0.3333333333333333703, 0.3333333333333334259, 0.3333333333333332593, 0.3333333333333333703, 0.3333333333333333703, 0.3333333333333334259, 0.3333333333333334814, 0.3333333333333333148, 0.3333333333333334259, 0.3333333333333333703, 0.3333333333333333703, 0.3333333333333333148, 0.3333333333333333703, 0.3333333333333334259, 0.3333333333333332038, 0.3333333333333334259, 0.3333333333333333703, 0.3333333333333334259, 0.3333333333333333703, 0.3333333333333333148, 0.3333333333333334259, 0.3333333333333334259, 0.3333333333333333703, 0.3333333333333334814, 0.3333333333333332593, 0.3333333333333334259, 0.3333333333333334259, 0.3333333333333333148, 0.3333333333333333703, 0.3333333333333333148, 0.3333333333333333703, 0.3333333333333333148, 0.3333333333333333703, 0.3333333333333333703, 0.3333333333333333703, 0.3333333333333333148, 0.3333333333333333148, 0.3333333333333334259, 0.3333333333333332593, 0.3333333333333333703, 0.3333333333333333703, 0.3333333333333333703, 0.3333333333333332593, 0.3333333333333334259, 0.3333333333333333148, 0.3333333333333333148, 0.3333333333333333703, 0.3333333333333333703, 0.3333333333333333703, 0.3333333333333334259, 0.3333333333333333148, 0.3333333333333334259, 0.3333333333333334259, 0.3333333333333333703, 0.3333333333333333703, 0.3333333333333333148, 0.3333333333333333703, 0.3333333333333333703, 0.3333333333333333148, 0.3333333333333333703, 0.3333333333333332593, 0.3333333333333334814, 0.3333333333333333148, 0.3333333333333333703, 0.3333333333333332593, 0.3333333333333335369, 0.3333333333333333703, 0.3333333333333333703, 0.3333333333333333703, 0.3333333333333334259, 0.3333333333333334259, 0.3333333333333333148, 0.3333333333333334259, 0.3333333333333333148, 0.3333333333333333703, 0.3333333333333335369, 0.3333333333333333148, 0.3333333333333334259, 0.3333333333333334814, 0.3333333333333333148, 0.3333333333333335369, 0.3333333333333332593, 0.3333333333333333703, 0.3333333333333333148, 0.3333333333333334259, 0.3333333333333333148, 0.3333333333333334814, 0.3333333333333333703, 0.3333333333333333148, 0.3333333333333333703, 0.3333333333333334259, 0.3333333333333333703, 0.3333333333333334259, 0.3333333333333332593, 0.3333333333333335924, 0.3333333333333333148, 0.3333333333333333148, 0.3333333333333334259, 0.3333333333333332593, 0.3333333333333333703, 0.3333333333333333148, 0.3333333333333335369, 0.3333333333333333703, 0.3333333333333333703, 0.3333333333333334259, 0.3333333333333334259, 0.3333333333333333703, 0.3333333333333333703, 0.3333333333333333703, 0.3333333333333333703, 0.3333333333333334259, 0.3333333333333333703, 0.3333333333333333703, 0.3333333333333333703, 0.3333333333333334259, 0.3333333333333333148, 0.3333333333333333703, 0.3333333333333333703, 0.3333333333333334259, 0.3333333333333333148, 0.3333333333333333703, 0.3333333333333333703, 0.3333333333333333703, 0.3333333333333333148, 0.3333333333333334259, 0.3333333333333333148, 0.3333333333333333703, 0.3333333333333334259, 0.3333333333333333703, 0.3333333333333333703, 0.3333333333333333703, 0.3333333333333333703, 0.3333333333333334259, 0.3333333333333334259, 0.3333333333333334259, 0.3333333333333333148, 0.3333333333333334259, 0.3333333333333333148, 0.3333333333333334259, 0.3333333333333334259, 0.3333333333333333703, 0.3333333333333333148, 0.3333333333333333703, 0.3333333333333333703, 0.3333333333333333148, 0.3333333333333334259, 0.3333333333333335369, 0.3333333333333333148, 0.3333333333333332593, 0.3333333333333334814, 0.3333333333333332593, 0.3333333333333333703, 0.3333333333333333703, 0.3333333333333333703, 0.3333333333333334259, 0.3333333333333334259, 0.3333333333333334259, 0.3333333333333335369, 0.3333333333333333703, 0.3333333333333333703, 0.3333333333333333703, 0.3333333333333334259, 0.3333333333333333703, 0.3333333333333333703, 0.3333333333333334259, 0.3333333333333333703, 0.3333333333333334259, 0.3333333333333332593, 0.3333333333333334259, 0.3333333333333334259, 0.3333333333333333148, 0.3333333333333333703, 0.3333333333333333703, 0.3333333333333333703, 0.3333333333333333703, 0.3333333333333334259, 0.3333333333333334259, 0.3333333333333334259, 0.3333333333333333148, 0.3333333333333333703, 0.3333333333333334259, 0.3333333333333332593, 0.3333333333333334814, 0.3333333333333333148, 0.3333333333333332593, 0.3333333333333335369, 0.3333333333333333148, 0.3333333333333333703, 0.3333333333333334259, 0.3333333333333333148, 0.3333333333333333703, 0.3333333333333334259, 0.3333333333333333148, 0.3333333333333335369, 0.3333333333333332593, 0.3333333333333333703, 0.3333333333333334259, 0.3333333333333333148, 0.3333333333333334259, 0.3333333333333333148, 0.3333333333333333703, 0.3333333333333333703, 0.3333333333333333703, 0.3333333333333333703, 0.3333333333333334259, 0.3333333333333332593, 0.3333333333333334259, 0.3333333333333334259, 0.3333333333333333703, 0.3333333333333333703, 0.3333333333333333148, 0.3333333333333334814, 0.3333333333333333703, 0.3333333333333332593, 0.3333333333333334259, 0.3333333333333334259, 0.3333333333333334259, 0.3333333333333333703, 0.3333333333333332038, 0.3333333333333335369, 0.3333333333333333148, 0.3333333333333333148, 0.3333333333333333703, 0.3333333333333333703, 0.3333333333333333703, 0.3333333333333334259, 0.3333333333333333148, 0.3333333333333334814, 0.3333333333333333148, 0.3333333333333333703, 0.3333333333333334259, 0.3333333333333333148, 0.3333333333333334259, 0.3333333333333333148, 0.3333333333333334259, 0.3333333333333333148, 0.3333333333333333703, 0.3333333333333333703, 0.3333333333333334259, 0.3333333333333333703, 0.3333333333333333148, 0.3333333333333334814, 0.3333333333333334259, 0.3333333333333333703, 0.3333333333333333148, 0.3333333333333334259, 0.3333333333333333703, 0.3333333333333333703, 0.3333333333333334259, 0.3333333333333333703, 0.3333333333333334814, 0.3333333333333333148, 0.3333333333333334259, 0.3333333333333333703, 0.3333333333333334259, 0.3333333333333333148, 0.3333333333333333703, 0.3333333333333334259, 0.3333333333333333703, 0.3333333333333334259, 0.3333333333333332593, 0.3333333333333333703, 0.3333333333333332593, 0.3333333333333334259, 0.3333333333333333703, 0.3333333333333334259, 0.3333333333333334259, 0.3333333333333333148, 0.3333333333333333148, 0.3333333333333334259, 0.3333333333333333148, 0.3333333333333333148, 0.3333333333333333703, 0.3333333333333333703, 0.3333333333333334259, 0.3333333333333333703, 0.3333333333333334814, 0.3333333333333332593, 0.3333333333333334259, 0.3333333333333333703, 0.3333333333333333703, 0.3333333333333334259, 0.3333333333333333703, 0.3333333333333333703, 0.3333333333333334259, 0.3333333333333334259, 0.3333333333333334814, 0.3333333333333333148, 0.3333333333333333148, 0.3333333333333333703, 0.3333333333333333148, 0.3333333333333334259, 0.3333333333333333703, 0.3333333333333333148, 0.3333333333333332593, 0.3333333333333334259, 0.3333333333333334259, 0.3333333333333333148, 0.3333333333333333703, 0.3333333333333334259, 0.3333333333333333148, 0.3333333333333334259, 0.3333333333333334259, 0.3333333333333334814, 0.3333333333333333148, 0.3333333333333333703, 0.3333333333333332593, 0.3333333333333334814, 0.3333333333333333703, 0.3333333333333332593, 0.3333333333333334814, 0.3333333333333332593, 0.3333333333333334259, 0.3333333333333333703, 0.3333333333333333148, 0.3333333333333333148, 0.3333333333333334259, 0.3333333333333333703, 0.3333333333333333703, 0.3333333333333333703, 0.3333333333333333703, 0.3333333333333334259, 0.3333333333333333148, 0.3333333333333334259, 0.3333333333333332038, 0.3333333333333334259, 0.3333333333333333148, 0.3333333333333334814, 0.3333333333333333703, 0.3333333333333333703, 0.3333333333333334259, 0.3333333333333333148, 0.3333333333333333703, 0.3333333333333333703, 0.3333333333333333703, 0.3333333333333333703, 0.3333333333333333703, 0.3333333333333334259, 0.3333333333333333148, 0.3333333333333334814, 0.3333333333333334259, 0.3333333333333332593, 0.3333333333333333703, 0.3333333333333333703, 0.3333333333333333703, 0.3333333333333333703, 0.3333333333333333703, 0.3333333333333334259, 0.3333333333333333148, 0.3333333333333333703, 0.3333333333333334259, 0.3333333333333335369, 0.3333333333333333148, 0.3333333333333333703, 0.3333333333333334259, 0.3333333333333333703, 0.3333333333333333703, 0.3333333333333333703, 0.3333333333333333703, 0.3333333333333333703, 0.3333333333333333703, 0.3333333333333333703, 0.3333333333333333703, 0.3333333333333334259, 0.3333333333333332593, 0.3333333333333334814, 0.3333333333333332593, 0.3333333333333334259, 0.3333333333333333703, 0.3333333333333333703, 0.3333333333333334814, 0.3333333333333333148, 0.3333333333333333703, 0.3333333333333333703),
 ( 0.3333333333333334259, 0.3333333333333334259, 0.3333333333333333703, 0.3333333333333333703, 0.3333333333333334259, 0.3333333333333333703, 0.3333333333333333703, 0.3333333333333334259, 0.3333333333333333148, 0.3333333333333334814, 0.3333333333333332593, 0.3333333333333335369, 0.3333333333333333148, 0.3333333333333333703, 0.3333333333333334259, 0.3333333333333332593, 0.3333333333333333703, 0.3333333333333333703, 0.3333333333333334259, 0.3333333333333334814, 0.3333333333333333148, 0.3333333333333334259, 0.3333333333333333703, 0.3333333333333333703, 0.3333333333333333148, 0.3333333333333333703, 0.3333333333333334259, 0.3333333333333332038, 0.3333333333333334259, 0.3333333333333333703, 0.3333333333333334259, 0.3333333333333333703, 0.3333333333333333148, 0.3333333333333334259, 0.3333333333333334259, 0.3333333333333333703, 0.3333333333333334814, 0.3333333333333332593, 0.3333333333333334259, 0.3333333333333334259, 0.3333333333333333148, 0.3333333333333333703, 0.3333333333333333148, 0.3333333333333333703, 0.3333333333333333148, 0.3333333333333333703, 0.3333333333333333703, 0.3333333333333333703, 0.3333333333333333148, 0.3333333333333333148, 0.3333333333333334259, 0.3333333333333332593, 0.3333333333333333703, 0.3333333333333333703, 0.3333333333333333703, 0.3333333333333332593, 0.3333333333333334259, 0.3333333333333333148, 0.3333333333333333148, 0.3333333333333333703, 0.3333333333333333703, 0.3333333333333333703, 0.3333333333333334259, 0.3333333333333333148, 0.3333333333333334259, 0.3333333333333334259, 0.3333333333333333703, 0.3333333333333333703, 0.3333333333333333148, 0.3333333333333333703, 0.3333333333333333703, 0.3333333333333333148, 0.3333333333333333703, 0.3333333333333332593, 0.3333333333333334814, 0.3333333333333333148, 0.3333333333333333703, 0.3333333333333332593, 0.3333333333333335369, 0.3333333333333333703, 0.3333333333333333703, 0.3333333333333333703, 0.3333333333333334259, 0.3333333333333334259, 0.3333333333333333148, 0.3333333333333334259, 0.3333333333333333148, 0.3333333333333333703, 0.3333333333333335369, 0.3333333333333333148, 0.3333333333333334259, 0.3333333333333334814, 0.3333333333333333148, 0.3333333333333335369, 0.3333333333333332593, 0.3333333333333333703, 0.3333333333333333148, 0.3333333333333334259, 0.3333333333333333148, 0.3333333333333334814, 0.3333333333333333703, 0.3333333333333333148, 0.3333333333333333703, 0.3333333333333334259, 0.3333333333333333703, 0.3333333333333334259, 0.3333333333333332593, 0.3333333333333335924, 0.3333333333333333148, 0.3333333333333333148, 0.3333333333333334259, 0.3333333333333332593, 0.3333333333333333703, 0.3333333333333333148, 0.3333333333333335369, 0.3333333333333333703, 0.3333333333333333703, 0.3333333333333334259, 0.3333333333333334259, 0.3333333333333333703, 0.3333333333333333703, 0.3333333333333333703, 0.3333333333333333703, 0.3333333333333334259, 0.3333333333333333703, 0.3333333333333333703, 0.3333333333333333703, 0.3333333333333334259, 0.3333333333333333148, 0.3333333333333333703, 0.3333333333333333703, 0.3333333333333334259, 0.3333333333333333148, 0.3333333333333333703, 0.3333333333333333703, 0.3333333333333333703, 0.3333333333333333148, 0.3333333333333334259, 0.3333333333333333148, 0.3333333333333333703, 0.3333333333333334259, 0.3333333333333333703, 0.3333333333333333703, 0.3333333333333333703, 0.3333333333333333703, 0.3333333333333334259, 0.3333333333333334259, 0.3333333333333334259, 0.3333333333333333148, 0.3333333333333334259, 0.3333333333333333148, 0.3333333333333334259, 0.3333333333333334259, 0.3333333333333333703, 0.3333333333333333148, 0.3333333333333333703, 0.3333333333333333703, 0.3333333333333333148, 0.3333333333333334259, 0.3333333333333335369, 0.3333333333333333148, 0.3333333333333332593, 0.3333333333333334814, 0.3333333333333332593, 0.3333333333333333703, 0.3333333333333333703, 0.3333333333333333703, 0.3333333333333334259, 0.3333333333333334259, 0.3333333333333334259, 0.3333333333333335369, 0.3333333333333333703, 0.3333333333333333703, 0.3333333333333333703, 0.3333333333333334259, 0.3333333333333333703, 0.3333333333333333703, 0.3333333333333334259, 0.3333333333333333703, 0.3333333333333334259, 0.3333333333333332593, 0.3333333333333334259, 0.3333333333333334259, 0.3333333333333333148, 0.3333333333333333703, 0.3333333333333333703, 0.3333333333333333703, 0.3333333333333333703, 0.3333333333333334259, 0.3333333333333334259, 0.3333333333333334259, 0.3333333333333333148, 0.3333333333333333703, 0.3333333333333334259, 0.3333333333333332593, 0.3333333333333334814, 0.3333333333333333148, 0.3333333333333332593, 0.3333333333333335369, 0.3333333333333333148, 0.3333333333333333703, 0.3333333333333334259, 0.3333333333333333148, 0.3333333333333333703, 0.3333333333333334259, 0.3333333333333333148, 0.3333333333333335369, 0.3333333333333332593, 0.3333333333333333703, 0.3333333333333334259, 0.3333333333333333148, 0.3333333333333334259, 0.3333333333333333148, 0.3333333333333333703, 0.3333333333333333703, 0.3333333333333333703, 0.3333333333333333703, 0.3333333333333334259, 0.3333333333333332593, 0.3333333333333334259, 0.3333333333333334259, 0.3333333333333333703, 0.3333333333333333703, 0.3333333333333333148, 0.3333333333333334814, 0.3333333333333333703, 0.3333333333333332593, 0.3333333333333334259, 0.3333333333333334259, 0.3333333333333334259, 0.3333333333333333703, 0.3333333333333332038, 0.3333333333333335369, 0.3333333333333333148, 0.3333333333333333148, 0.3333333333333333703, 0.3333333333333333703, 0.3333333333333333703, 0.3333333333333334259, 0.3333333333333333148, 0.3333333333333334814, 0.3333333333333333148, 0.3333333333333333703, 0.3333333333333334259, 0.3333333333333333148, 0.3333333333333334259, 0.3333333333333333148, 0.3333333333333334259, 0.3333333333333333148, 0.3333333333333333703, 0.3333333333333333703, 0.3333333333333334259, 0.3333333333333333703, 0.3333333333333333148, 0.3333333333333334814, 0.3333333333333334259, 0.3333333333333333703, 0.3333333333333333148, 0.3333333333333334259, 0.3333333333333333703, 0.3333333333333333703, 0.3333333333333334259, 0.3333333333333333703, 0.3333333333333334814, 0.3333333333333333148, 0.3333333333333334259, 0.3333333333333333703, 0.3333333333333334259, 0.3333333333333333148, 0.3333333333333333703, 0.3333333333333334259, 0.3333333333333333703, 0.3333333333333334259, 0.3333333333333332593, 0.3333333333333333703, 0.3333333333333332593, 0.3333333333333334259, 0.3333333333333333703, 0.3333333333333334259, 0.3333333333333334259, 0.3333333333333333148, 0.3333333333333333148, 0.3333333333333334259, 0.3333333333333333148, 0.3333333333333333148, 0.3333333333333333703, 0.3333333333333333703, 0.3333333333333334259, 0.3333333333333333703, 0.3333333333333334814, 0.3333333333333332593, 0.3333333333333334259, 0.3333333333333333703, 0.3333333333333333703, 0.3333333333333334259, 0.3333333333333333703, 0.3333333333333333703, 0.3333333333333334259, 0.3333333333333334259, 0.3333333333333334814, 0.3333333333333333148, 0.3333333333333333148, 0.3333333333333333703, 0.3333333333333333148, 0.3333333333333334259, 0.3333333333333333703, 0.3333333333333333148, 0.3333333333333332593, 0.3333333333333334259, 0.3333333333333334259, 0.3333333333333333148, 0.3333333333333333703, 0.3333333333333334259, 0.3333333333333333148, 0.3333333333333334259, 0.3333333333333334259, 0.3333333333333334814, 0.3333333333333333148, 0.3333333333333333703, 0.3333333333333332593, 0.3333333333333334814, 0.3333333333333333703, 0.3333333333333332593, 0.3333333333333334814, 0.3333333333333332593, 0.3333333333333334259, 0.3333333333333333703, 0.3333333333333333148, 0.3333333333333333148, 0.3333333333333334259, 0.3333333333333333703, 0.3333333333333333703, 0.3333333333333333703, 0.3333333333333333703, 0.3333333333333334259, 0.3333333333333333148, 0.3333333333333334259, 0.3333333333333332038, 0.3333333333333334259, 0.3333333333333333148, 0.3333333333333334814, 0.3333333333333333703, 0.3333333333333333703, 0.3333333333333334259, 0.3333333333333333148, 0.3333333333333333703, 0.3333333333333333703, 0.3333333333333333703, 0.3333333333333333703, 0.3333333333333333703, 0.3333333333333334259, 0.3333333333333333148, 0.3333333333333334814, 0.3333333333333334259, 0.3333333333333332593, 0.3333333333333333703, 0.3333333333333333703, 0.3333333333333333703, 0.3333333333333333703, 0.3333333333333333703, 0.3333333333333334259, 0.3333333333333333148, 0.3333333333333333703, 0.3333333333333334259, 0.3333333333333335369, 0.3333333333333333148, 0.3333333333333333703, 0.3333333333333334259, 0.3333333333333333703, 0.3333333333333333703, 0.3333333333333333703, 0.3333333333333333703, 0.3333333333333333703, 0.3333333333333333703, 0.3333333333333333703, 0.3333333333333333703, 0.3333333333333334259, 0.3333333333333332593, 0.3333333333333334814, 0.3333333333333332593, 0.3333333333333334259, 0.3333333333333333703, 0.3333333333333333703, 0.3333333333333334814, 0.3333333333333333148, 0.3333333333333333703, 0.3333333333333333703),
 ( 1.000000000000000222, 1.000000000000000222, 0.9999999999999997780, 1.000000000000000222, 1.000000000000000000, 1.000000000000000000, 0.9999999999999997780, 1.000000000000000000, 1.000000000000000000, 1.000000000000000000, 1.000000000000000000, 1.000000000000000222, 1.000000000000000000, 1.000000000000000000, 1.000000000000000222, 0.9999999999999994449, 1.000000000000000222, 1.000000000000000000, 0.9999999999999997780, 1.000000000000000444, 1.000000000000000000, 1.000000000000000222, 1.000000000000000000, 1.000000000000000000, 0.9999999999999996669, 1.000000000000000000, 1.000000000000000222, 0.9999999999999996669, 1.000000000000000222, 1.000000000000000000, 1.000000000000000222, 1.000000000000000000, 1.000000000000000222, 0.9999999999999997780, 1.000000000000000444, 1.000000000000000000, 1.000000000000000222, 0.9999999999999997780, 1.000000000000000222, 1.000000000000000000, 1.000000000000000000, 0.9999999999999997780, 1.000000000000000000, 0.9999999999999997780, 1.000000000000000000, 0.9999999999999997780, 1.000000000000000000, 1.000000000000000000, 0.9999999999999997780, 1.000000000000000000, 1.000000000000000222, 0.9999999999999996669, 1.000000000000000000, 1.000000000000000000, 1.000000000000000222, 0.9999999999999997780, 1.000000000000000444, 1.000000000000000000, 0.9999999999999997780, 1.000000000000000000, 1.000000000000000000, 1.000000000000000000, 1.000000000000000222, 1.000000000000000000, 1.000000000000000000, 1.000000000000000222, 1.000000000000000000, 1.000000000000000000, 0.9999999999999997780, 1.000000000000000222, 1.000000000000000000, 0.9999999999999997780, 1.000000000000000000, 1.000000000000000000, 1.000000000000000000, 1.000000000000000000, 1.000000000000000222, 0.9999999999999996669, 1.000000000000000444, 0.9999999999999996669, 1.000000000000000000, 0.9999999999999996669, 1.000000000000000444, 1.000000000000000000, 1.000000000000000000, 1.000000000000000222, 1.000000000000000000, 1.000000000000000000, 1.000000000000000222, 0.9999999999999997780, 1.000000000000000000, 1.000000000000000444, 0.9999999999999997780, 1.000000000000000444, 0.9999999999999997780, 1.000000000000000000, 1.000000000000000222, 1.000000000000000000, 0.9999999999999997780, 1.000000000000000222, 1.000000000000000222, 0.9999999999999997780, 1.000000000000000000, 1.000000000000000222, 0.9999999999999997780, 1.000000000000000444, 0.9999999999999997780, 1.000000000000000444, 0.9999999999999997780, 1.000000000000000000, 1.000000000000000222, 0.9999999999999996669, 1.000000000000000000, 1.000000000000000000, 1.000000000000000444, 1.000000000000000222, 0.9999999999999997780, 1.000000000000000222, 1.000000000000000222, 1.000000000000000000, 1.000000000000000222, 0.9999999999999997780, 1.000000000000000000, 1.000000000000000222, 0.9999999999999996669, 1.000000000000000000, 1.000000000000000000, 1.000000000000000000, 1.000000000000000000, 1.000000000000000000, 1.000000000000000000, 1.000000000000000000, 0.9999999999999997780, 1.000000000000000222, 0.9999999999999997780, 1.000000000000000000, 0.9999999999999997780, 1.000000000000000222, 1.000000000000000000, 1.000000000000000000, 1.000000000000000000, 1.000000000000000222, 0.9999999999999997780, 0.9999999999999997780, 1.000000000000000222, 1.000000000000000222, 1.000000000000000000, 1.000000000000000444, 0.9999999999999996669, 1.000000000000000444, 0.9999999999999997780, 1.000000000000000222, 1.000000000000000000, 1.000000000000000000, 1.000000000000000000, 1.000000000000000222, 0.9999999999999997780, 0.9999999999999997780, 1.000000000000000444, 1.000000000000000444, 0.9999999999999997780, 1.000000000000000000, 1.000000000000000000, 1.000000000000000000, 1.000000000000000222, 1.000000000000000000, 1.000000000000000000, 1.000000000000000222, 1.000000000000000222, 1.000000000000000000, 1.000000000000000444, 1.000000000000000000, 1.000000000000000222, 1.000000000000000000, 1.000000000000000000, 1.000000000000000444, 1.000000000000000000, 1.000000000000000222, 1.000000000000000000, 1.000000000000000222, 0.9999999999999997780, 1.000000000000000222, 1.000000000000000222, 1.000000000000000000, 0.9999999999999996669, 1.000000000000000222, 1.000000000000000000, 1.000000000000000000, 1.000000000000000222, 1.000000000000000222, 1.000000000000000222, 0.9999999999999997780, 1.000000000000000000, 1.000000000000000222, 1.000000000000000000, 1.000000000000000000, 1.000000000000000000, 0.9999999999999996669, 1.000000000000000444, 1.000000000000000222, 0.9999999999999996669, 1.000000000000000444, 1.000000000000000000, 1.000000000000000000, 1.000000000000000222, 0.9999999999999997780, 1.000000000000000444, 0.9999999999999997780, 0.9999999999999997780, 1.000000000000000444, 0.9999999999999997780, 1.000000000000000222, 1.000000000000000000, 1.000000000000000000, 1.000000000000000000, 0.9999999999999997780, 1.000000000000000000, 1.000000000000000222, 0.9999999999999996669, 1.000000000000000222, 1.000000000000000000, 1.000000000000000222, 0.9999999999999996669, 0.9999999999999997780, 1.000000000000000444, 0.9999999999999997780, 0.9999999999999997780, 1.000000000000000000, 1.000000000000000222, 1.000000000000000000, 1.000000000000000000, 0.9999999999999996669, 1.000000000000000222, 1.000000000000000000, 0.9999999999999997780, 1.000000000000000000, 1.000000000000000000, 0.9999999999999997780, 1.000000000000000444, 0.9999999999999996669, 1.000000000000000444, 0.9999999999999997780, 1.000000000000000000, 1.000000000000000222, 0.9999999999999997780, 1.000000000000000222, 1.000000000000000222, 0.9999999999999997780, 1.000000000000000000, 1.000000000000000000, 1.000000000000000000, 1.000000000000000222, 1.000000000000000000, 1.000000000000000000, 1.000000000000000222, 1.000000000000000222, 1.000000000000000000, 1.000000000000000000, 1.000000000000000222, 0.9999999999999997780, 1.000000000000000000, 1.000000000000000222, 1.000000000000000000, 1.000000000000000222, 0.9999999999999997780, 1.000000000000000222, 0.9999999999999997780, 1.000000000000000222, 0.9999999999999997780, 1.000000000000000222, 1.000000000000000000, 1.000000000000000000, 1.000000000000000444, 0.9999999999999996669, 1.000000000000000222, 0.9999999999999997780, 1.000000000000000000, 1.000000000000000222, 1.000000000000000000, 1.000000000000000222, 0.9999999999999997780, 0.9999999999999997780, 1.000000000000000000, 0.9999999999999997780, 1.000000000000000000, 1.000000000000000000, 1.000000000000000222, 1.000000000000000000, 1.000000000000000000, 1.000000000000000222, 1.000000000000000000, 1.000000000000000000, 1.000000000000000000, 1.000000000000000000, 0.9999999999999997780, 1.000000000000000222, 1.000000000000000222, 0.9999999999999997780, 1.000000000000000444, 1.000000000000000444, 0.9999999999999997780, 1.000000000000000000, 0.9999999999999997780, 1.000000000000000000, 1.000000000000000000, 1.000000000000000000, 1.000000000000000000, 0.9999999999999997780, 1.000000000000000222, 1.000000000000000000, 0.9999999999999997780, 1.000000000000000222, 1.000000000000000000, 1.000000000000000000, 1.000000000000000000, 1.000000000000000444, 1.000000000000000000, 0.9999999999999997780, 0.9999999999999997780, 0.9999999999999997780, 1.000000000000000222, 1.000000000000000222, 0.9999999999999996669, 1.000000000000000222, 0.9999999999999997780, 1.000000000000000222, 1.000000000000000000, 1.000000000000000000, 0.9999999999999996669, 1.000000000000000222, 1.000000000000000222, 1.000000000000000000, 1.000000000000000000, 1.000000000000000222, 0.9999999999999997780, 1.000000000000000000, 1.000000000000000222, 0.9999999999999994449, 1.000000000000000222, 1.000000000000000000, 1.000000000000000222, 0.9999999999999997780, 1.000000000000000000, 1.000000000000000000, 0.9999999999999997780, 1.000000000000000000, 1.000000000000000222, 0.9999999999999997780, 1.000000000000000000, 1.000000000000000000, 1.000000000000000000, 1.000000000000000000, 1.000000000000000222, 1.000000000000000000, 0.9999999999999996669, 0.9999999999999996669, 1.000000000000000222, 0.9999999999999997780, 1.000000000000000222, 1.000000000000000000, 0.9999999999999997780, 1.000000000000000222, 0.9999999999999997780, 1.000000000000000444, 1.000000000000000222, 1.000000000000000000, 1.000000000000000222, 1.000000000000000222, 1.000000000000000000, 1.000000000000000000, 1.000000000000000000, 1.000000000000000000, 1.000000000000000000, 1.000000000000000000, 1.000000000000000000, 0.9999999999999997780, 1.000000000000000000, 0.9999999999999996669, 1.000000000000000444, 0.9999999999999996669, 1.000000000000000000, 1.000000000000000000, 0.9999999999999997780, 1.000000000000000444, 1.000000000000000000, 1.000000000000000000, 1.000000000000000000),
 ( 0.3333333333333334259, 0.3333333333333334259, 0.3333333333333333703, 0.3333333333333333703, 0.3333333333333334259, 0.3333333333333333703, 0.3333333333333333703, 0.3333333333333334259, 0.3333333333333333148, 0.3333333333333334814, 0.3333333333333332593, 0.3333333333333335369, 0.3333333333333333148, 0.3333333333333333703, 0.3333333333333334259, 0.3333333333333332593, 0.3333333333333333703, 0.3333333333333333703, 0.3333333333333334259, 0.3333333333333334814, 0.3333333333333333148, 0.3333333333333334259, 0.3333333333333333703, 0.3333333333333333703, 0.3333333333333333148, 0.3333333333333333703, 0.3333333333333334259, 0.3333333333333332038, 0.3333333333333334259, 0.3333333333333333703, 0.3333333333333334259, 0.3333333333333333703, 0.3333333333333333148, 0.3333333333333334259, 0.3333333333333334259, 0.3333333333333333703, 0.3333333333333334814, 0.3333333333333332593, 0.3333333333333334259, 0.3333333333333334259, 0.3333333333333333148, 0.3333333333333333703, 0.3333333333333333148, 0.3333333333333333703, 0.3333333333333333148, 0.3333333333333333703, 0.3333333333333333703, 0.3333333333333333703, 0.3333333333333333148, 0.3333333333333333148, 0.3333333333333334259, 0.3333333333333332593, 0.3333333333333333703, 0.3333333333333333703, 0.3333333333333333703, 0.3333333333333332593, 0.3333333333333334259, 0.3333333333333333148, 0.3333333333333333148, 0.3333333333333333703, 0.3333333333333333703, 0.3333333333333333703, 0.3333333333333334259, 0.3333333333333333148, 0.3333333333333334259, 0.3333333333333334259, 0.3333333333333333703, 0.3333333333333333703, 0.3333333333333333148, 0.3333333333333333703, 0.3333333333333333703, 0.3333333333333333148, 0.3333333333333333703, 0.3333333333333332593, 0.3333333333333334814, 0.3333333333333333148, 0.3333333333333333703, 0.3333333333333332593, 0.3333333333333335369, 0.3333333333333333703, 0.3333333333333333703, 0.3333333333333333703, 0.3333333333333334259, 0.3333333333333334259, 0.3333333333333333148, 0.3333333333333334259, 0.3333333333333333148, 0.3333333333333333703, 0.3333333333333335369, 0.3333333333333333148, 0.3333333333333334259, 0.3333333333333334814, 0.3333333333333333148, 0.3333333333333335369, 0.3333333333333332593, 0.3333333333333333703, 0.3333333333333333148, 0.3333333333333334259, 0.3333333333333333148, 0.3333333333333334814, 0.3333333333333333703, 0.3333333333333333148, 0.3333333333333333703, 0.3333333333333334259, 0.3333333333333333703, 0.3333333333333334259, 0.3333333333333332593, 0.3333333333333335924, 0.3333333333333333148, 0.3333333333333333148, 0.3333333333333334259, 0.3333333333333332593, 0.3333333333333333703, 0.3333333333333333148, 0.3333333333333335369, 0.3333333333333333703, 0.3333333333333333703, 0.3333333333333334259, 0.3333333333333334259, 0.3333333333333333703, 0.3333333333333333703, 0.3333333333333333703, 0.3333333333333333703, 0.3333333333333334259, 0.3333333333333333703, 0.3333333333333333703, 0.3333333333333333703, 0.3333333333333334259, 0.3333333333333333148, 0.3333333333333333703, 0.3333333333333333703, 0.3333333333333334259, 0.3333333333333333148, 0.3333333333333333703, 0.3333333333333333703, 0.3333333333333333703, 0.3333333333333333148, 0.3333333333333334259, 0.3333333333333333148, 0.3333333333333333703, 0.3333333333333334259, 0.3333333333333333703, 0.3333333333333333703, 0.3333333333333333703, 0.3333333333333333703, 0.3333333333333334259, 0.3333333333333334259, 0.3333333333333334259, 0.3333333333333333148, 0.3333333333333334259, 0.3333333333333333148, 0.3333333333333334259, 0.3333333333333334259, 0.3333333333333333703, 0.3333333333333333148, 0.3333333333333333703, 0.3333333333333333703, 0.3333333333333333148, 0.3333333333333334259, 0.3333333333333335369, 0.3333333333333333148, 0.3333333333333332593, 0.3333333333333334814, 0.3333333333333332593, 0.3333333333333333703, 0.3333333333333333703, 0.3333333333333333703, 0.3333333333333334259, 0.3333333333333334259, 0.3333333333333334259, 0.3333333333333335369, 0.3333333333333333703, 0.3333333333333333703, 0.3333333333333333703, 0.3333333333333334259, 0.3333333333333333703, 0.3333333333333333703, 0.3333333333333334259, 0.3333333333333333703, 0.3333333333333334259, 0.3333333333333332593, 0.3333333333333334259, 0.3333333333333334259, 0.3333333333333333148, 0.3333333333333333703, 0.3333333333333333703, 0.3333333333333333703, 0.3333333333333333703, 0.3333333333333334259, 0.3333333333333334259, 0.3333333333333334259, 0.3333333333333333148, 0.3333333333333333703, 0.3333333333333334259, 0.3333333333333332593, 0.3333333333333334814, 0.3333333333333333148, 0.3333333333333332593, 0.3333333333333335369, 0.3333333333333333148, 0.3333333333333333703, 0.3333333333333334259, 0.3333333333333333148, 0.3333333333333333703, 0.3333333333333334259, 0.3333333333333333148, 0.3333333333333335369, 0.3333333333333332593, 0.3333333333333333703, 0.3333333333333334259, 0.3333333333333333148, 0.3333333333333334259, 0.3333333333333333148, 0.3333333333333333703, 0.3333333333333333703, 0.3333333333333333703, 0.3333333333333333703, 0.3333333333333334259, 0.3333333333333332593, 0.3333333333333334259, 0.3333333333333334259, 0.3333333333333333703, 0.3333333333333333703, 0.3333333333333333148, 0.3333333333333334814, 0.3333333333333333703, 0.3333333333333332593, 0.3333333333333334259, 0.3333333333333334259, 0.3333333333333334259, 0.3333333333333333703, 0.3333333333333332038, 0.3333333333333335369, 0.3333333333333333148, 0.3333333333333333148, 0.3333333333333333703, 0.3333333333333333703, 0.3333333333333333703, 0.3333333333333334259, 0.3333333333333333148, 0.3333333333333334814, 0.3333333333333333148, 0.3333333333333333703, 0.3333333333333334259, 0.3333333333333333148, 0.3333333333333334259, 0.3333333333333333148, 0.3333333333333334259, 0.3333333333333333148, 0.3333333333333333703, 0.3333333333333333703, 0.3333333333333334259, 0.3333333333333333703, 0.3333333333333333148, 0.3333333333333334814, 0.3333333333333334259, 0.3333333333333333703, 0.3333333333333333148, 0.3333333333333334259, 0.3333333333333333703, 0.3333333333333333703, 0.3333333333333334259, 0.3333333333333333703, 0.3333333333333334814, 0.3333333333333333148, 0.3333333333333334259, 0.3333333333333333703, 0.3333333333333334259, 0.3333333333333333148, 0.3333333333333333703, 0.3333333333333334259, 0.3333333333333333703, 0.3333333333333334259, 0.3333333333333332593, 0.3333333333333333703, 0.3333333333333332593, 0.3333333333333334259, 0.3333333333333333703, 0.3333333333333334259, 0.3333333333333334259, 0.3333333333333333148, 0.3333333333333333148, 0.3333333333333334259, 0.3333333333333333148, 0.3333333333333333148, 0.3333333333333333703, 0.3333333333333333703, 0.3333333333333334259, 0.3333333333333333703, 0.3333333333333334814, 0.3333333333333332593, 0.3333333333333334259, 0.3333333333333333703, 0.3333333333333333703, 0.3333333333333334259, 0.3333333333333333703, 0.3333333333333333703, 0.3333333333333334259, 0.3333333333333334259, 0.3333333333333334814, 0.3333333333333333148, 0.3333333333333333148, 0.3333333333333333703, 0.3333333333333333148, 0.3333333333333334259, 0.3333333333333333703, 0.3333333333333333148, 0.3333333333333332593, 0.3333333333333334259, 0.3333333333333334259, 0.3333333333333333148, 0.3333333333333333703, 0.3333333333333334259, 0.3333333333333333148, 0.3333333333333334259, 0.3333333333333334259, 0.3333333333333334814, 0.3333333333333333148, 0.3333333333333333703, 0.3333333333333332593, 0.3333333333333334814, 0.3333333333333333703, 0.3333333333333332593, 0.3333333333333334814, 0.3333333333333332593, 0.3333333333333334259, 0.3333333333333333703, 0.3333333333333333148, 0.3333333333333333148, 0.3333333333333334259, 0.3333333333333333703, 0.3333333333333333703, 0.3333333333333333703, 0.3333333333333333703, 0.3333333333333334259, 0.3333333333333333148, 0.3333333333333334259, 0.3333333333333332038, 0.3333333333333334259, 0.3333333333333333148, 0.3333333333333334814, 0.3333333333333333703, 0.3333333333333333703, 0.3333333333333334259, 0.3333333333333333148, 0.3333333333333333703, 0.3333333333333333703, 0.3333333333333333703, 0.3333333333333333703, 0.3333333333333333703, 0.3333333333333334259, 0.3333333333333333148, 0.3333333333333334814, 0.3333333333333334259, 0.3333333333333332593, 0.3333333333333333703, 0.3333333333333333703, 0.3333333333333333703, 0.3333333333333333703, 0.3333333333333333703, 0.3333333333333334259, 0.3333333333333333148, 0.3333333333333333703, 0.3333333333333334259, 0.3333333333333335369, 0.3333333333333333148, 0.3333333333333333703, 0.3333333333333334259, 0.3333333333333333703, 0.3333333333333333703, 0.3333333333333333703, 0.3333333333333333703, 0.3333333333333333703, 0.3333333333333333703, 0.3333333333333333703, 0.3333333333333333703, 0.3333333333333334259, 0.3333333333333332593, 0.3333333333333334814, 0.3333333333333332593, 0.3333333333333334259, 0.3333333333333333703, 0.3333333333333333703, 0.3333333333333334814, 0.3333333333333333148, 0.3333333333333333703, 0.3333333333333333703),
 ( 0.3333333333333334259, 0.3333333333333334259, 0.3333333333333333703, 0.3333333333333333703, 0.3333333333333334259, 0.3333333333333333703, 0.3333333333333333703, 0.3333333333333334259, 0.3333333333333333148, 0.3333333333333334814, 0.3333333333333332593, 0.3333333333333335369, 0.3333333333333333148, 0.3333333333333333703, 0.3333333333333334259, 0.3333333333333332593, 0.3333333333333333703, 0.3333333333333333703, 0.3333333333333334259, 0.3333333333333334814, 0.3333333333333333148, 0.3333333333333334259, 0.3333333333333333703, 0.3333333333333333703, 0.3333333333333333148, 0.3333333333333333703, 0.3333333333333334259, 0.3333333333333332038, 0.3333333333333334259, 0.3333333333333333703, 0.3333333333333334259, 0.3333333333333333703, 0.3333333333333333148, 0.3333333333333334259, 0.3333333333333334259, 0.3333333333333333703, 0.3333333333333334814, 0.3333333333333332593, 0.3333333333333334259, 0.3333333333333334259, 0.3333333333333333148, 0.3333333333333333703, 0.3333333333333333148, 0.3333333333333333703, 0.3333333333333333148, 0.3333333333333333703, 0.3333333333333333703, 0.3333333333333333703, 0.3333333333333333148, 0.3333333333333333148, 0.3333333333333334259, 0.3333333333333332593, 0.3333333333333333703, 0.3333333333333333703, 0.3333333333333333703, 0.3333333333333332593, 0.3333333333333334259, 0.3333333333333333148, 0.3333333333333333148, 0.3333333333333333703, 0.3333333333333333703, 0.3333333333333333703, 0.3333333333333334259, 0.3333333333333333148, 0.3333333333333334259, 0.3333333333333334259, 0.3333333333333333703, 0.3333333333333333703, 0.3333333333333333148, 0.3333333333333333703, 0.3333333333333333703, 0.3333333333333333148, 0.3333333333333333703, 0.3333333333333332593, 0.3333333333333334814, 0.3333333333333333148, 0.3333333333333333703, 0.3333333333333332593, 0.3333333333333335369, 0.3333333333333333703, 0.3333333333333333703, 0.3333333333333333703, 0.3333333333333334259, 0.3333333333333334259, 0.3333333333333333148, 0.3333333333333334259, 0.3333333333333333148, 0.3333333333333333703, 0.3333333333333335369, 0.3333333333333333148, 0.3333333333333334259, 0.3333333333333334814, 0.3333333333333333148, 0.3333333333333335369, 0.3333333333333332593, 0.3333333333333333703, 0.3333333333333333148, 0.3333333333333334259, 0.3333333333333333148, 0.3333333333333334814, 0.3333333333333333703, 0.3333333333333333148, 0.3333333333333333703, 0.3333333333333334259, 0.3333333333333333703, 0.3333333333333334259, 0.3333333333333332593, 0.3333333333333335924, 0.3333333333333333148, 0.3333333333333333148, 0.3333333333333334259, 0.3333333333333332593, 0.3333333333333333703, 0.3333333333333333148, 0.3333333333333335369, 0.3333333333333333703, 0.3333333333333333703, 0.3333333333333334259, 0.3333333333333334259, 0.3333333333333333703, 0.3333333333333333703, 0.3333333333333333703, 0.3333333333333333703, 0.3333333333333334259, 0.3333333333333333703, 0.3333333333333333703, 0.3333333333333333703, 0.3333333333333334259, 0.3333333333333333148, 0.3333333333333333703, 0.3333333333333333703, 0.3333333333333334259, 0.3333333333333333148, 0.3333333333333333703, 0.3333333333333333703, 0.3333333333333333703, 0.3333333333333333148, 0.3333333333333334259, 0.3333333333333333148, 0.3333333333333333703, 0.3333333333333334259, 0.3333333333333333703, 0.3333333333333333703, 0.3333333333333333703, 0.3333333333333333703, 0.3333333333333334259, 0.3333333333333334259, 0.3333333333333334259, 0.3333333333333333148, 0.3333333333333334259, 0.3333333333333333148, 0.3333333333333334259, 0.3333333333333334259, 0.3333333333333333703, 0.3333333333333333148, 0.3333333333333333703, 0.3333333333333333703, 0.3333333333333333148, 0.3333333333333334259, 0.3333333333333335369, 0.3333333333333333148, 0.3333333333333332593, 0.3333333333333334814, 0.3333333333333332593, 0.3333333333333333703, 0.3333333333333333703, 0.3333333333333333703, 0.3333333333333334259, 0.3333333333333334259, 0.3333333333333334259, 0.3333333333333335369, 0.3333333333333333703, 0.3333333333333333703, 0.3333333333333333703, 0.3333333333333334259, 0.3333333333333333703, 0.3333333333333333703, 0.3333333333333334259, 0.3333333333333333703, 0.3333333333333334259, 0.3333333333333332593, 0.3333333333333334259, 0.3333333333333334259, 0.3333333333333333148, 0.3333333333333333703, 0.3333333333333333703, 0.3333333333333333703, 0.3333333333333333703, 0.3333333333333334259, 0.3333333333333334259, 0.3333333333333334259, 0.3333333333333333148, 0.3333333333333333703, 0.3333333333333334259, 0.3333333333333332593, 0.3333333333333334814, 0.3333333333333333148, 0.3333333333333332593, 0.3333333333333335369, 0.3333333333333333148, 0.3333333333333333703, 0.3333333333333334259, 0.3333333333333333148, 0.3333333333333333703, 0.3333333333333334259, 0.3333333333333333148, 0.3333333333333335369, 0.3333333333333332593, 0.3333333333333333703, 0.3333333333333334259, 0.3333333333333333148, 0.3333333333333334259, 0.3333333333333333148, 0.3333333333333333703, 0.3333333333333333703, 0.3333333333333333703, 0.3333333333333333703, 0.3333333333333334259, 0.3333333333333332593, 0.3333333333333334259, 0.3333333333333334259, 0.3333333333333333703, 0.3333333333333333703, 0.3333333333333333148, 0.3333333333333334814, 0.3333333333333333703, 0.3333333333333332593, 0.3333333333333334259, 0.3333333333333334259, 0.3333333333333334259, 0.3333333333333333703, 0.3333333333333332038, 0.3333333333333335369, 0.3333333333333333148, 0.3333333333333333148, 0.3333333333333333703, 0.3333333333333333703, 0.3333333333333333703, 0.3333333333333334259, 0.3333333333333333148, 0.3333333333333334814, 0.3333333333333333148, 0.3333333333333333703, 0.3333333333333334259, 0.3333333333333333148, 0.3333333333333334259, 0.3333333333333333148, 0.3333333333333334259, 0.3333333333333333148, 0.3333333333333333703, 0.3333333333333333703, 0.3333333333333334259, 0.3333333333333333703, 0.3333333333333333148, 0.3333333333333334814, 0.3333333333333334259, 0.3333333333333333703, 0.3333333333333333148, 0.3333333333333334259, 0.3333333333333333703, 0.3333333333333333703, 0.3333333333333334259, 0.3333333333333333703, 0.3333333333333334814, 0.3333333333333333148, 0.3333333333333334259, 0.3333333333333333703, 0.3333333333333334259, 0.3333333333333333148, 0.3333333333333333703, 0.3333333333333334259, 0.3333333333333333703, 0.3333333333333334259, 0.3333333333333332593, 0.3333333333333333703, 0.3333333333333332593, 0.3333333333333334259, 0.3333333333333333703, 0.3333333333333334259, 0.3333333333333334259, 0.3333333333333333148, 0.3333333333333333148, 0.3333333333333334259, 0.3333333333333333148, 0.3333333333333333148, 0.3333333333333333703, 0.3333333333333333703, 0.3333333333333334259, 0.3333333333333333703, 0.3333333333333334814, 0.3333333333333332593, 0.3333333333333334259, 0.3333333333333333703, 0.3333333333333333703, 0.3333333333333334259, 0.3333333333333333703, 0.3333333333333333703, 0.3333333333333334259, 0.3333333333333334259, 0.3333333333333334814, 0.3333333333333333148, 0.3333333333333333148, 0.3333333333333333703, 0.3333333333333333148, 0.3333333333333334259, 0.3333333333333333703, 0.3333333333333333148, 0.3333333333333332593, 0.3333333333333334259, 0.3333333333333334259, 0.3333333333333333148, 0.3333333333333333703, 0.3333333333333334259, 0.3333333333333333148, 0.3333333333333334259, 0.3333333333333334259, 0.3333333333333334814, 0.3333333333333333148, 0.3333333333333333703, 0.3333333333333332593, 0.3333333333333334814, 0.3333333333333333703, 0.3333333333333332593, 0.3333333333333334814, 0.3333333333333332593, 0.3333333333333334259, 0.3333333333333333703, 0.3333333333333333148, 0.3333333333333333148, 0.3333333333333334259, 0.3333333333333333703, 0.3333333333333333703, 0.3333333333333333703, 0.3333333333333333703, 0.3333333333333334259, 0.3333333333333333148, 0.3333333333333334259, 0.3333333333333332038, 0.3333333333333334259, 0.3333333333333333148, 0.3333333333333334814, 0.3333333333333333703, 0.3333333333333333703, 0.3333333333333334259, 0.3333333333333333148, 0.3333333333333333703, 0.3333333333333333703, 0.3333333333333333703, 0.3333333333333333703, 0.3333333333333333703, 0.3333333333333334259, 0.3333333333333333148, 0.3333333333333334814, 0.3333333333333334259, 0.3333333333333332593, 0.3333333333333333703, 0.3333333333333333703, 0.3333333333333333703, 0.3333333333333333703, 0.3333333333333333703, 0.3333333333333334259, 0.3333333333333333148, 0.3333333333333333703, 0.3333333333333334259, 0.3333333333333335369, 0.3333333333333333148, 0.3333333333333333703, 0.3333333333333334259, 0.3333333333333333703, 0.3333333333333333703, 0.3333333333333333703, 0.3333333333333333703, 0.3333333333333333703, 0.3333333333333333703, 0.3333333333333333703, 0.3333333333333333703, 0.3333333333333334259, 0.3333333333333332593, 0.3333333333333334814, 0.3333333333333332593, 0.3333333333333334259, 0.3333333333333333703, 0.3333333333333333703, 0.3333333333333334814, 0.3333333333333333148, 0.3333333333333333703, 0.3333333333333333703),
 ( 1.000000000000000222, 1.000000000000000222, 0.9999999999999997780, 1.000000000000000222, 1.000000000000000000, 1.000000000000000000, 0.9999999999999997780, 1.000000000000000000, 1.000000000000000000, 1.000000000000000000, 1.000000000000000000, 1.000000000000000222, 1.000000000000000000, 1.000000000000000000, 1.000000000000000222, 0.9999999999999994449, 1.000000000000000222, 1.000000000000000000, 0.9999999999999997780, 1.000000000000000444, 1.000000000000000000, 1.000000000000000222, 1.000000000000000000, 1.000000000000000000, 0.9999999999999996669, 1.000000000000000000, 1.000000000000000222, 0.9999999999999996669, 1.000000000000000222, 1.000000000000000000, 1.000000000000000222, 1.000000000000000000, 1.000000000000000222, 0.9999999999999997780, 1.000000000000000444, 1.000000000000000000, 1.000000000000000222, 0.9999999999999997780, 1.000000000000000222, 1.000000000000000000, 1.000000000000000000, 0.9999999999999997780, 1.000000000000000000, 0.9999999999999997780, 1.000000000000000000, 0.9999999999999997780, 1.000000000000000000, 1.000000000000000000, 0.9999999999999997780, 1.000000000000000000, 1.000000000000000222, 0.9999999999999996669, 1.000000000000000000, 1.000000000000000000, 1.000000000000000222, 0.9999999999999997780, 1.000000000000000444, 1.000000000000000000, 0.9999999999999997780, 1.000000000000000000, 1.000000000000000000, 1.000000000000000000, 1.000000000000000222, 1.000000000000000000, 1.000000000000000000, 1.000000000000000222, 1.000000000000000000, 1.000000000000000000, 0.9999999999999997780, 1.000000000000000222, 1.000000000000000000, 0.9999999999999997780, 1.000000000000000000, 1.000000000000000000, 1.000000000000000000, 1.000000000000000000, 1.000000000000000222, 0.9999999999999996669, 1.000000000000000444, 0.9999999999999996669, 1.000000000000000000, 0.9999999999999996669, 1.000000000000000444, 1.000000000000000000, 1.000000000000000000, 1.000000000000000222, 1.000000000000000000, 1.000000000000000000, 1.000000000000000222, 0.9999999999999997780, 1.000000000000000000, 1.000000000000000444, 0.9999999999999997780, 1.000000000000000444, 0.9999999999999997780, 1.000000000000000000, 1.000000000000000222, 1.000000000000000000, 0.9999999999999997780, 1.000000000000000222, 1.000000000000000222, 0.9999999999999997780, 1.000000000000000000, 1.000000000000000222, 0.9999999999999997780, 1.000000000000000444, 0.9999999999999997780, 1.000000000000000444, 0.9999999999999997780, 1.000000000000000000, 1.000000000000000222, 0.9999999999999996669, 1.000000000000000000, 1.000000000000000000, 1.000000000000000444, 1.000000000000000222, 0.9999999999999997780, 1.000000000000000222, 1.000000000000000222, 1.000000000000000000, 1.000000000000000222, 0.9999999999999997780, 1.000000000000000000, 1.000000000000000222, 0.9999999999999996669, 1.000000000000000000, 1.000000000000000000, 1.000000000000000000, 1.000000000000000000, 1.000000000000000000, 1.000000000000000000, 1.000000000000000000, 0.9999999999999997780, 1.000000000000000222, 0.9999999999999997780, 1.000000000000000000, 0.9999999999999997780, 1.000000000000000222, 1.000000000000000000, 1.000000000000000000, 1.000000000000000000, 1.000000000000000222, 0.9999999999999997780, 0.9999999999999997780, 1.000000000000000222, 1.000000000000000222, 1.000000000000000000, 1.000000000000000444, 0.9999999999999996669, 1.000000000000000444, 0.9999999999999997780, 1.000000000000000222, 1.000000000000000000, 1.000000000000000000, 1.000000000000000000, 1.000000000000000222, 0.9999999999999997780, 0.9999999999999997780, 1.000000000000000444, 1.000000000000000444, 0.9999999999999997780, 1.000000000000000000, 1.000000000000000000, 1.000000000000000000, 1.000000000000000222, 1.000000000000000000, 1.000000000000000000, 1.000000000000000222, 1.000000000000000222, 1.000000000000000000, 1.000000000000000444, 1.000000000000000000, 1.000000000000000222, 1.000000000000000000, 1.000000000000000000, 1.000000000000000444, 1.000000000000000000, 1.000000000000000222, 1.000000000000000000, 1.000000000000000222, 0.9999999999999997780, 1.000000000000000222, 1.000000000000000222, 1.000000000000000000, 0.9999999999999996669, 1.000000000000000222, 1.000000000000000000, 1.000000000000000000, 1.000000000000000222, 1.000000000000000222, 1.000000000000000222, 0.9999999999999997780, 1.000000000000000000, 1.000000000000000222, 1.000000000000000000, 1.000000000000000000, 1.000000000000000000, 0.9999999999999996669, 1.000000000000000444, 1.000000000000000222, 0.9999999999999996669, 1.000000000000000444, 1.000000000000000000, 1.000000000000000000, 1.000000000000000222, 0.9999999999999997780, 1.000000000000000444, 0.9999999999999997780, 0.9999999999999997780, 1.000000000000000444, 0.9999999999999997780, 1.000000000000000222, 1.000000000000000000, 1.000000000000000000, 1.000000000000000000, 0.9999999999999997780, 1.000000000000000000, 1.000000000000000222, 0.9999999999999996669, 1.000000000000000222, 1.000000000000000000, 1.000000000000000222, 0.9999999999999996669, 0.9999999999999997780, 1.000000000000000444, 0.9999999999999997780, 0.9999999999999997780, 1.000000000000000000, 1.000000000000000222, 1.000000000000000000, 1.000000000000000000, 0.9999999999999996669, 1.000000000000000222, 1.000000000000000000, 0.9999999999999997780, 1.000000000000000000, 1.000000000000000000, 0.9999999999999997780, 1.000000000000000444, 0.9999999999999996669, 1.000000000000000444, 0.9999999999999997780, 1.000000000000000000, 1.000000000000000222, 0.9999999999999997780, 1.000000000000000222, 1.000000000000000222, 0.9999999999999997780, 1.000000000000000000, 1.000000000000000000, 1.000000000000000000, 1.000000000000000222, 1.000000000000000000, 1.000000000000000000, 1.000000000000000222, 1.000000000000000222, 1.000000000000000000, 1.000000000000000000, 1.000000000000000222, 0.9999999999999997780, 1.000000000000000000, 1.000000000000000222, 1.000000000000000000, 1.000000000000000222, 0.9999999999999997780, 1.000000000000000222, 0.9999999999999997780, 1.000000000000000222, 0.9999999999999997780, 1.000000000000000222, 1.000000000000000000, 1.000000000000000000, 1.000000000000000444, 0.9999999999999996669, 1.000000000000000222, 0.9999999999999997780, 1.000000000000000000, 1.000000000000000222, 1.000000000000000000, 1.000000000000000222, 0.9999999999999997780, 0.9999999999999997780, 1.000000000000000000, 0.9999999999999997780, 1.000000000000000000, 1.000000000000000000, 1.000000000000000222, 1.000000000000000000, 1.000000000000000000, 1.000000000000000222, 1.000000000000000000, 1.000000000000000000, 1.000000000000000000, 1.000000000000000000, 0.9999999999999997780, 1.000000000000000222, 1.000000000000000222, 0.9999999999999997780, 1.000000000000000444, 1.000000000000000444, 0.9999999999999997780, 1.000000000000000000, 0.9999999999999997780, 1.000000000000000000, 1.000000000000000000, 1.000000000000000000, 1.000000000000000000, 0.9999999999999997780, 1.000000000000000222, 1.000000000000000000, 0.9999999999999997780, 1.000000000000000222, 1.000000000000000000, 1.000000000000000000, 1.000000000000000000, 1.000000000000000444, 1.000000000000000000, 0.9999999999999997780, 0.9999999999999997780, 0.9999999999999997780, 1.000000000000000222, 1.000000000000000222, 0.9999999999999996669, 1.000000000000000222, 0.9999999999999997780, 1.000000000000000222, 1.000000000000000000, 1.000000000000000000, 0.9999999999999996669, 1.000000000000000222, 1.000000000000000222, 1.000000000000000000, 1.000000000000000000, 1.000000000000000222, 0.9999999999999997780, 1.000000000000000000, 1.000000000000000222, 0.9999999999999994449, 1.000000000000000222, 1.000000000000000000, 1.000000000000000222, 0.9999999999999997780, 1.000000000000000000, 1.000000000000000000, 0.9999999999999997780, 1.000000000000000000, 1.000000000000000222, 0.9999999999999997780, 1.000000000000000000, 1.000000000000000000, 1.000000000000000000, 1.000000000000000000, 1.000000000000000222, 1.000000000000000000, 0.9999999999999996669, 0.9999999999999996669, 1.000000000000000222, 0.9999999999999997780, 1.000000000000000222, 1.000000000000000000, 0.9999999999999997780, 1.000000000000000222, 0.9999999999999997780, 1.000000000000000444, 1.000000000000000222, 1.000000000000000000, 1.000000000000000222, 1.000000000000000222, 1.000000000000000000, 1.000000000000000000, 1.000000000000000000, 1.000000000000000000, 1.000000000000000000, 1.000000000000000000, 1.000000000000000000, 0.9999999999999997780, 1.000000000000000000, 0.9999999999999996669, 1.000000000000000444, 0.9999999999999996669, 1.000000000000000000, 1.000000000000000000, 0.9999999999999997780, 1.000000000000000444, 1.000000000000000000, 1.000000000000000000, 1.000000000000000000) ) ) 
 REPRESENTATION_ITEM ( '' )  SURFACE ( )  );
#164380 = CARTESIAN_POINT ( 'NONE',  ( 6.771407655021410399, 9.987393799911945536, -1.199719254218441611 ) ) ;
#164381 = CARTESIAN_POINT ( 'NONE',  ( 0.6801582343749900117, 1.588541667008100511, -1.178068619123890270 ) ) ;
#164382 = CARTESIAN_POINT ( 'NONE',  ( 4.731432421044862835, 6.543090462684225450, -1.443375672974051449 ) ) ;
#164383 = CARTESIAN_POINT ( 'NONE',  ( 10.99915817693633713, -6.765468805240992367, -0.1539349733294627931 ) ) ;
#164384 = DIRECTION ( 'NONE',  ( 1.000000000000000000, -4.985516615831701596E-16, 0.000000000000000000 ) ) ;
#164385 = CARTESIAN_POINT ( 'NONE',  ( 0.2218712608162629052, 1.761692264604281633, 0.5354471447000588302 ) ) ;
#164386 = ORIENTED_EDGE ( 'NONE', *, *, #206253, .F. ) ;
#164387 = CARTESIAN_POINT ( 'NONE',  ( -7.587723245503481095, 8.881373870289390737, 1.199719254218452047 ) ) ;
#164388 = CARTESIAN_POINT ( 'NONE',  ( 4.710133486059870478, -0.7981590245086762625, -1.691823354513532163 ) ) ;
#164389 = CARTESIAN_POINT ( 'NONE',  ( -1.850000000000000089, 0.09855238430052820631, 0.5999999999999969802 ) ) ;
#164390 = CARTESIAN_POINT ( 'NONE',  ( 5.969332771766739931, 10.18624834369502885, -0.7998128361456481317 ) ) ;
#164391 = CARTESIAN_POINT ( 'NONE',  ( -1.734723475976807094E-15, 2.999999999999988898, -6.938893903907228378E-15 ) ) ;
#164392 = EDGE_CURVE ( 'NONE', #116972, #55552, #127753, .T. ) ;
#164393 = CARTESIAN_POINT ( 'NONE',  ( -7.565086526745425033, 7.928281824065535055, 0.7216878364870317197 ) ) ;
#164394 = CARTESIAN_POINT ( 'NONE',  ( 4.150767584078112193, 7.994312614733129152, 0.7998128361456321445 ) ) ;
#164395 = CARTESIAN_POINT ( 'NONE',  ( 1.463649477047322733, -0.4837646206634453883, 1.908952741056660685 ) ) ;
#164396 = CARTESIAN_POINT ( 'NONE',  ( 2.003530013310977242, -1.955168117277843898, 0.4926643476272293820 ) ) ;
#164397 = CARTESIAN_POINT ( 'NONE',  ( -7.323375529675950624, 11.69568855126397011, -0.7998128361456291469 ) ) ;
#164398 = CARTESIAN_POINT ( 'NONE',  ( 4.366607992053101128, 7.252070536440704096, -1.199719254218448494 ) ) ;
#164399 = FACE_OUTER_BOUND ( 'NONE', #28469, .T. ) ;
#164400 = CARTESIAN_POINT ( 'NONE',  ( 2.502122453320880346, -0.8398649383675671487, -2.024319193490734303 ) ) ;
#164401 = CARTESIAN_POINT ( 'NONE',  ( 2.609770642201841184, 0.3830433331901660354, -0.1872689674646474400 ) ) ;
#164402 = CARTESIAN_POINT ( 'NONE',  ( -8.462260433223891098, 13.02438760540324481, -0.7998128361456281477 ) ) ;
#164403 = CARTESIAN_POINT ( 'NONE',  ( -2.788906526875773208E-15, 10.21875000068279782, -1.499999999999998446 ) ) ;
#164404 = CARTESIAN_POINT ( 'NONE',  ( 3.933273961740296087, 6.642551151122080277, 1.082531754730549078 ) ) ;
#164405 = CARTESIAN_POINT ( 'NONE',  ( 7.964525173024008531, 11.37936423758166526, 1.199719254218460707 ) ) ;
#164406 = CARTESIAN_POINT ( 'NONE',  ( -1.579999999999996074, 8.674529973577525865, -2.499999999999995115 ) ) ;
#164407 = CARTESIAN_POINT ( 'NONE',  ( 7.214347136247488912, 7.589362211809770997, -0.7216878364870317197 ) ) ;
#164408 = VERTEX_POINT ( 'NONE', #94597 ) ;
#164410 = CARTESIAN_POINT ( 'NONE',  ( 1.770182950735105898, 2.007541250849652847, -0.1504272076729237795 ) ) ;
#164409 = CARTESIAN_POINT ( 'NONE',  ( 5.179192671508887180, 1.240781939916297372, 1.360553736468192554 ) ) ;
#164411 = CARTESIAN_POINT ( 'NONE',  ( 3.409784427348498070, 0.5549599139818006677, 2.230294995599948926 ) ) ;
#164413 = CARTESIAN_POINT ( 'NONE',  ( 0.9361096364171941353, -1.039984170849604039, 1.543015978488631923 ) ) ;
#164412 = DIRECTION ( 'NONE',  ( 0.000000000000000000, 0.000000000000000000, 1.000000000000000000 ) ) ;
#164414 = CARTESIAN_POINT ( 'NONE',  ( 3.285556943749998737, -2.705208332855374209, -1.896917185911906500 ) ) ;
#164415 = CARTESIAN_POINT ( 'NONE',  ( 4.204028478337375829E-16, -0.02876672507444788529, -3.432849766368870181 ) ) ;
#164416 = CARTESIAN_POINT ( 'NONE',  ( 5.326388512780113160, -0.8654452107222168067, -1.705464787417856787 ) ) ;
#164417 = CARTESIAN_POINT ( 'NONE',  ( -8.565000355531095622, 11.01558638625153286, -1.599625672291263179 ) ) ;
#164418 = CARTESIAN_POINT ( 'NONE',  ( -5.465345320084574965, 9.390336950158399532, 0.000000000000000000 ) ) ;
#164420 = CARTESIAN_POINT ( 'NONE',  ( 3.625732356982212412, -1.113523340526129335, -1.502988901547596567 ) ) ;
#164419 = CARTESIAN_POINT ( 'NONE',  ( 3.474242889556743652, -2.015522812629696237, -0.5555695364270489822 ) ) ;
#164421 = CARTESIAN_POINT ( 'NONE',  ( 7.809133291791403586, 8.213003049952529722, -0.7216878364870257245 ) ) ;
#164422 = CARTESIAN_POINT ( 'NONE',  ( 5.917501325027624048, -1.028386522942719816, -1.527094029191010893 ) ) ;
#164423 = CARTESIAN_POINT ( 'NONE',  ( 2.672928840188529609, 6.270167413528593414, 0.000000000000000000 ) ) ;
#164425 = CARTESIAN_POINT ( 'NONE',  ( 5.138703914779377158, 5.953908307786102583, 1.199719254218462483 ) ) ;
#164424 = CARTESIAN_POINT ( 'NONE',  ( 0.4373225248172875057, -7.723431457505085085, -10.96785329849812385 ) ) ;
#164426 = CARTESIAN_POINT ( 'NONE',  ( 4.564925566169513615, -1.542601567919573258, -0.7719000744037025630 ) ) ;
#164427 = CARTESIAN_POINT ( 'NONE',  ( -7.389357414647957256, 8.579670724299436557, 1.199719254218450271 ) ) ;
#164428 = CARTESIAN_POINT ( 'NONE',  ( 0.4000000000000019096, 3.964661556059719594, -0.9099571394229579724 ) ) ;
#164429 = CARTESIAN_POINT ( 'NONE',  ( 4.101444922696781070, 3.685019076479660427, 2.500000000000011102 ) ) ;
#164430 = CARTESIAN_POINT ( 'NONE',  ( 4.715793416201278454, 0.4818634375548909166, -2.116767182733831021 ) ) ;
#164431 = CARTESIAN_POINT ( 'NONE',  ( 3.105874302609371362, -1.823586186413633126, 0.09019715141062728536 ) ) ;
#164432 = CARTESIAN_POINT ( 'NONE',  ( 0.9362904128984714802, -1.094497954693674391, 1.627855050370475620 ) ) ;
#164433 = CARTESIAN_POINT ( 'NONE',  ( 5.928941916292417957, -1.787427330561262906, 1.134758347235584885 ) ) ;
#164435 = CARTESIAN_POINT ( 'NONE',  ( 1.364683531249988535, 4.217708333674752730, -0.7879004041258239610 ) ) ;
#164434 = CARTESIAN_POINT ( 'NONE',  ( 5.618756969397510126, -0.05950314066365805510, 2.291748599322357194 ) ) ;
#164436 = CARTESIAN_POINT ( 'NONE',  ( 4.952636518945290334, 6.537114055554089198, 2.442608363190974963 ) ) ;
#164437 = CARTESIAN_POINT ( 'NONE',  ( 9.752392566931574081, 10.27221283770866300, -0.7998128361456281477 ) ) ;
#164438 = CARTESIAN_POINT ( 'NONE',  ( 1.700013272279196963, 1.464590769506744161, 1.533662747278791816 ) ) ;
#164439 = CARTESIAN_POINT ( 'NONE',  ( -5.097502569058225852, 5.049433873430440478, -0.7216878364870207285 ) ) ;
#164440 = STYLED_ITEM ( 'NONE', ( #81277 ), #121890 ) ;
#164441 = FACE_OUTER_BOUND ( 'NONE', #11427, .T. ) ;
#164442 = CARTESIAN_POINT ( 'NONE',  ( -5.083944415000202888, 5.033616027029415463, 0.7216878364870317197 ) ) ;
#164443 = CARTESIAN_POINT ( 'NONE',  ( 6.508646264616319677, 0.6728166153291449403, 2.064291235436790384 ) ) ;
#164445 = CARTESIAN_POINT ( 'NONE',  ( -1.500000000000001110, 12.80208333401612997, 0.8660254037844419273 ) ) ;
#164444 = CARTESIAN_POINT ( 'NONE',  ( 6.983263157960365675, 7.629137130509070275, 2.653810918356712900 ) ) ;
#164448 = EDGE_LOOP ( 'NONE', ( #197088, #27123, #58168, #126520, #211098 ) ) ;
#164447 = CARTESIAN_POINT ( 'NONE',  ( 1.911064425300706526, -0.5960121562160587416, -2.139774337300159424 ) ) ;
#164446 = AXIS2_PLACEMENT_3D ( 'NONE', #110701, #195083, #29391 ) ;
#164449 = CARTESIAN_POINT ( 'NONE',  ( 6.240861317752083970, 2.010826688392798101, -0.1511364921914087889 ) ) ;
#164451 = CARTESIAN_POINT ( 'NONE',  ( 6.104357437187505120, 2.059938769829409377, 0.1070097549743902060 ) ) ;
#164450 = CARTESIAN_POINT ( 'NONE',  ( 3.499976210622149253, 7.235056012367825140, 0.7998128361456321445 ) ) ;
#164453 = CARTESIAN_POINT ( 'NONE',  ( -4.285785955251283141, 8.014184357852876417, 0.000000000000000000 ) ) ;
#164452 = CARTESIAN_POINT ( 'NONE',  ( 4.694866332082116678, 8.699370830729650450, 0.7998128361456341429 ) ) ;
#164454 = CARTESIAN_POINT ( 'NONE',  ( 5.200434439293556643, 8.224868058221247225, -1.199719254218452047 ) ) ;
#164455 = CARTESIAN_POINT ( 'NONE',  ( 0.000000000000000000, -2.734374999522040550, -3.793834371823813001 ) ) ;
#164456 = CARTESIAN_POINT ( 'NONE',  ( 0.1329588055935578272, 2.045323036463253086, -2.262667038281248377 ) ) ;
#164457 = CARTESIAN_POINT ( 'NONE',  ( 4.159580895514263688, 0.8717668643758098579, 1.621812032879976329 ) ) ;
#164459 = ORIENTED_EDGE ( 'NONE', *, *, #155215, .F. ) ;
#164458 = CARTESIAN_POINT ( 'NONE',  ( 5.691725559638619814, 5.534767995866836543, 1.040834085586084257E-14 ) ) ;
#164460 =( LENGTH_UNIT ( ) NAMED_UNIT ( * ) SI_UNIT ( .MILLI., .METRE. ) );
#164461 = CARTESIAN_POINT ( 'NONE',  ( 2.150978262527812213, -1.382985381756835608, -1.030390371524889659 ) ) ;
#164462 = CARTESIAN_POINT ( 'NONE',  ( 0.4797043241997685503, -0.7212876333932433104, 1.883314553594167107 ) ) ;
#164463 = CARTESIAN_POINT ( 'NONE',  ( 2.426789430794534130, -1.706071328008453625, -1.540741829672709118 ) ) ;
#164464 = CARTESIAN_POINT ( 'NONE',  ( -0.6823417656250212460, 4.613541667008086655, 1.181850606188767472 ) ) ;
#164465 = CARTESIAN_POINT ( 'NONE',  ( 0.9840795919474578657, 1.519885296779641681, 1.676025758627389450 ) ) ;
#164466 = CARTESIAN_POINT ( 'NONE',  ( 4.231157339275457119, 0.1028475037690677746, 2.103686673710772670 ) ) ;
#164467 = CARTESIAN_POINT ( 'NONE',  ( -2.810282979782591006, 6.500690253046801814, 0.000000000000000000 ) ) ;
#164468 = CARTESIAN_POINT ( 'NONE',  ( 2.143481220494340533, 0.6824282661134513095, -1.633078482676100007 ) ) ;
#164469 = CARTESIAN_POINT ( 'NONE',  ( 7.135668919494039031, 7.219368582364847242, 1.040834085586084257E-14 ) ) ;
#164470 = CARTESIAN_POINT ( 'NONE',  ( 5.112833325684902341, 7.058334528089426740, -1.443375672974078761 ) ) ;
#164471 = CARTESIAN_POINT ( 'NONE',  ( -6.749261541504576911, 6.768559974710451677, 1.040834085586084257E-14 ) ) ;
#164472 = CARTESIAN_POINT ( 'NONE',  ( -1.500000000000013101, 1.670833333333355153, 0.8660254037844403729 ) ) ;
#164473 = CARTESIAN_POINT ( 'NONE',  ( 5.361676289133297857, -1.751401506552331400, -1.366425036640180446 ) ) ;
#164474 = CARTESIAN_POINT ( 'NONE',  ( 3.908297495596550597, 1.550167135825938569, -1.549264980215167231 ) ) ;
#164475 = CARTESIAN_POINT ( 'NONE',  ( -4.466521540698216164, 7.298359999868178960, -1.199719254218452047 ) ) ;
#164476 = CARTESIAN_POINT ( 'NONE',  ( 0.2935777296394709857, 7.111227605955068753, -1.979479841891092162 ) ) ;
#164477 = DIRECTION ( 'NONE',  ( -0.000000000000000000, -1.000000000000000000, 0.000000000000000000 ) ) ;
#164478 = CARTESIAN_POINT ( 'NONE',  ( -1.364683531250012516, 3.238541667008084879, -0.7879004041258289570 ) ) ;
#164479 = CARTESIAN_POINT ( 'NONE',  ( 6.889999999999973035, 7.629137130509070275, 2.319999999999996287 ) ) ;
#164481 = CARTESIAN_POINT ( 'NONE',  ( -3.877268743828284681, 5.546566172598190292, 1.443375672974064550 ) ) ;
#164480 = COLOUR_RGB ( '', 0.08235294, 0.09019608, 0.10196078) ;
#164482 = CARTESIAN_POINT ( 'NONE',  ( 5.801066647469003357, -0.3129311994157328303, -2.097281602037828208 ) ) ;
#164483 = CARTESIAN_POINT ( 'NONE',  ( -5.966997003790221576, 9.015228033513643879, -1.082531754730549967 ) ) ;
#164484 = ORIENTED_EDGE ( 'NONE', *, *, #56424, .T. ) ;
#164486 = CARTESIAN_POINT ( 'NONE',  ( -1.445103857048105844, 8.688264192037886247, -2.625611233228243968 ) ) ;
#164485 = CARTESIAN_POINT ( 'NONE',  ( -5.804299160426249493, 5.944306240018289778, -0.7216878364870338292 ) ) ;
#164487 = CARTESIAN_POINT ( 'NONE',  ( 5.464099601507359516, 6.333536608968757697, 1.199719254218462483 ) ) ;
#164488 = CARTESIAN_POINT ( 'NONE',  ( 6.480030769895370746, -1.807141314969593848, -0.3518929191878711338 ) ) ;
#164489 = CARTESIAN_POINT ( 'NONE',  ( -0.4019237886466802689, 9.479914550367428916, -1.500000000000002887 ) ) ;
#164490 = CARTESIAN_POINT ( 'NONE',  ( 0.5625979914390633052, 6.581402780318009960, -3.408537040423953446 ) ) ;
#164491 = CARTESIAN_POINT ( 'NONE',  ( -0.6823417656250212460, 3.863541667008085767, 1.181850606188767472 ) ) ;
#164492 = CARTESIAN_POINT ( 'NONE',  ( 1.786251233324965826, 1.514223802825481302, -0.8579289008448316434 ) ) ;
#164493 = CARTESIAN_POINT ( 'NONE',  ( 2.846322183865124700, 5.408127416896231665, -1.199719254218446718 ) ) ;
#164494 = CARTESIAN_POINT ( 'NONE',  ( -9.499386779316207452, -9.999529051968231386, 0.1207253440360574054 ) ) ;
#164495 = CARTESIAN_POINT ( 'NONE',  ( -0.6823417656250003738, -0.2197916663252488800, -1.181850606188749264 ) ) ;
#164496 = CARTESIAN_POINT ( 'NONE',  ( 8.500000000000000000, 6.216000000000041048, -2.921333333333334004 ) ) ;
#164497 = EDGE_CURVE ( 'NONE', #35662, #38381, #26747, .T. ) ;
#164498 = CARTESIAN_POINT ( 'NONE',  ( 6.332923096303629151, 0.2067577541180857514, 2.151790036905242953 ) ) ;
#164499 = CARTESIAN_POINT ( 'NONE',  ( -5.108724954250998707, 4.854600622914589714, -0.7998128361456221525 ) ) ;
#164500 = CARTESIAN_POINT ( 'NONE',  ( -5.951666246274811556, 7.966696592119163256, 1.443375672974064550 ) ) ;
#164501 = VECTOR ( 'NONE', #200032, 1000.000000000000000 ) ;
#164502 = CARTESIAN_POINT ( 'NONE',  ( 6.245025451202089073, -1.828886558906620774, 1.152162773130911644 ) ) ;
#164504 = ORIENTED_EDGE ( 'NONE', *, *, #183495, .F. ) ;
#164503 = DIRECTION ( 'NONE',  ( 0.000000000000000000, 0.000000000000000000, 1.000000000000000000 ) ) ;
#164505 = CARTESIAN_POINT ( 'NONE',  ( -1.364683531249997417, 2.509375000341422357, 1.214306433183764966E-14 ) ) ;
#164506 = CARTESIAN_POINT ( 'NONE',  ( 5.624284779170636739, 1.176309258369928390, -1.581782371169083712 ) ) ;
#164507 = CARTESIAN_POINT ( 'NONE',  ( 5.571581879130038217, 1.311117947217877555, -1.134664832369073117 ) ) ;
#164509 = CARTESIAN_POINT ( 'NONE',  ( 2.472451708263478931, -2.098117355222902436, -0.6331711661175795092 ) ) ;
#164508 = CARTESIAN_POINT ( 'NONE',  ( -1.360316468750044860, -0.8385416663252739378, 0.7853790794158720390 ) ) ;
#164510 = CARTESIAN_POINT ( 'NONE',  ( 3.891899753260852801, 1.669126095664546838, 1.593640439619238514 ) ) ;
#164511 = CARTESIAN_POINT ( 'NONE',  ( 4.727839713825126466, -1.264755334911156881, -1.626962714342747196 ) ) ;
#164512 = CARTESIAN_POINT ( 'NONE',  ( 1.042798325077255450, -1.530655164913260702, -1.195007349728629764 ) ) ;
#164513 = CARTESIAN_POINT ( 'NONE',  ( -6.344852701071109102, 10.34615255131755163, 0.000000000000000000 ) ) ;
#164514 = CARTESIAN_POINT ( 'NONE',  ( -4.197131071882288289, 7.054347462908075350, -1.199719254218455378 ) ) ;
#164515 = CARTESIAN_POINT ( 'NONE',  ( -0.1110810684432985002, 0.002541288824218451356, -1.796853612742685069 ) ) ;
#164516 = CARTESIAN_POINT ( 'NONE',  ( 3.656581996618038843, 2.110704406498860486, 0.2042969539849878724 ) ) ;
#164517 = CARTESIAN_POINT ( 'NONE',  ( 0.000000000000000000, 4.000000000000003553, 0.000000000000000000 ) ) ;
#164518 = CARTESIAN_POINT ( 'NONE',  ( 0.8971115437808926396, -0.9091470795906559932, -1.799921601489597123 ) ) ;
#164519 = CARTESIAN_POINT ( 'NONE',  ( -5.544921637864824504, 8.452530429942200385, -1.082531754730543971 ) ) ;
#164520 = CARTESIAN_POINT ( 'NONE',  ( 4.858537417550492954, 0.8407558337346630051, 2.040536144146696707 ) ) ;
#164521 = CARTESIAN_POINT ( 'NONE',  ( -5.649528891068317016, 5.555814892526615090, 0.2055412888010339778 ) ) ;
#164522 = CARTESIAN_POINT ( 'NONE',  ( 2.843981590737003629, 6.431529745484265703, 0.1377261510360130170 ) ) ;
#164523 = CARTESIAN_POINT ( 'NONE',  ( -7.435720902452096936, 7.639705572474380091, 0.000000000000000000 ) ) ;
#164525 = CARTESIAN_POINT ( 'NONE',  ( 6.825078400183579141, 1.241995729952071637, 2.258014901253778461 ) ) ;
#164524 = CARTESIAN_POINT ( 'NONE',  ( -5.747140441703231240, 7.374164810257596514, -1.320148062302946013 ) ) ;
#164526 = CARTESIAN_POINT ( 'NONE',  ( 1.448804818547306139, 8.711467014680348342, -2.592604518246271361 ) ) ;
#164527 = VERTEX_POINT ( 'NONE', #77246 ) ;
#164528 = CARTESIAN_POINT ( 'NONE',  ( 4.926665654204026801, 1.971471998011574467, 0.6004258549221918040 ) ) ;
#164529 = CARTESIAN_POINT ( 'NONE',  ( -5.758872628492444169E-14, 2.203125000341452200, 1.570758158831754070 ) ) ;
#164530 = CARTESIAN_POINT ( 'NONE',  ( -3.744022975668147790, 7.519777238254810925, -0.7998128361456281477 ) ) ;
#164531 = B_SPLINE_CURVE_WITH_KNOTS ( 'NONE', 3,
 ( #84243, #213157, #180674, #19231, #134100, #85311, #133029, #50677, #116802, #48561, #196924, #200109, #98366, #130931, #65823, #199029 ),
 .UNSPECIFIED., .F., .F.,
 ( 4, 3, 3, 3, 3, 4 ),
 ( 0.000000000000000000, 3.357822776042542455E-05, 6.715700932737186327E-05, 0.0001007352753633149715, 0.0001343124815392907664, 0.0001562160020015795762 ),
 .UNSPECIFIED. ) ;
#164532 = CARTESIAN_POINT ( 'NONE',  ( 3.826823269871942657, 1.426704988148481901, -1.429811943454310397 ) ) ;
#164533 = CARTESIAN_POINT ( 'NONE',  ( 0.7499999999999885647, -0.2666666666666442365, 1.299038105676657340 ) ) ;
#164534 = CARTESIAN_POINT ( 'NONE',  ( 4.220665892555866883, 3.818531717603609987, -0.7998128361456211532 ) ) ;
#164535 = CARTESIAN_POINT ( 'NONE',  ( 8.446893396513862839, 9.813462703143045474, -1.199719254218445830 ) ) ;
#164536 = CARTESIAN_POINT ( 'NONE',  ( 2.870052109166462362, 1.101224123558439905, 1.741800865840010593 ) ) ;
#164537 = CARTESIAN_POINT ( 'NONE',  ( 3.673896439623290266, 4.156855427197417185, 1.000000000000011324 ) ) ;
#164538 = CARTESIAN_POINT ( 'NONE',  ( 5.867981556616276073, 5.740399992340775803, -0.7998128361456281477 ) ) ;
#164539 = CARTESIAN_POINT ( 'NONE',  ( -2.123823618835070537, 5.629544655282869847, 1.040834085586084257E-14 ) ) ;
#164540 = CARTESIAN_POINT ( 'NONE',  ( 0.7613493127172387132, 0.9053670157611827252, 1.603083849714491027 ) ) ;
#164541 = EDGE_CURVE ( 'NONE', #162523, #31095, #68159, .T. ) ;
#164542 = CARTESIAN_POINT ( 'NONE',  ( 6.445939570963194143, 0.8488519614954292969, -2.037301952897092594 ) ) ;
#164543 = CARTESIAN_POINT ( 'NONE',  ( 5.794130544993763898, 7.853181283949808744, 1.599625672291269396 ) ) ;
#164544 = CARTESIAN_POINT ( 'NONE',  ( 0.9312127099814873077, 0.1580370610147242560, 2.155845405312675211 ) ) ;
#164545 = CARTESIAN_POINT ( 'NONE',  ( -3.090895834235680262, 5.589500325708124606, 1.082531754730560403 ) ) ;
#164546 = CARTESIAN_POINT ( 'NONE',  ( 1.657435761918718331, 1.928256795251210631, -0.5899901959932273288 ) ) ;
#164547 = CARTESIAN_POINT ( 'NONE',  ( 1.775234297868668376, -2.280957755244545027, 0.2818987734495673192 ) ) ;
#164548 = CARTESIAN_POINT ( 'NONE',  ( 5.905025204069010769, 4.805319369725367551, -2.499999999999995115 ) ) ;
#164549 = CARTESIAN_POINT ( 'NONE',  ( 0.4087956859853311142, 1.625333209436867321, 0.9259686016569528277 ) ) ;
#164550 = CARTESIAN_POINT ( 'NONE',  ( 4.662937792257120684, -1.760523130880174314, -0.8874255463059472770 ) ) ;
#164551 = CARTESIAN_POINT ( 'NONE',  ( 4.223842396274177347, 0.8578445224393380641, -1.825075645057252505 ) ) ;
#164554 = EDGE_CURVE ( 'NONE', #37173, #66261, #93530, .T. ) ;
#164553 = CARTESIAN_POINT ( 'NONE',  ( 9.910647101465253073, 11.62513837554007168, -1.082531754730537088 ) ) ;
#164552 = CARTESIAN_POINT ( 'NONE',  ( 1.364683531249988535, 2.363541667008088432, 0.7879004041258500513 ) ) ;
#164556 = CARTESIAN_POINT ( 'NONE',  ( 6.270163029207718175, 1.081028068854476665, 1.807315287263556280 ) ) ;
#164555 = CARTESIAN_POINT ( 'NONE',  ( -7.576308911938196999, 7.733448573549685179, 0.7998128361456462443 ) ) ;
#164557 = CARTESIAN_POINT ( 'NONE',  ( 5.617656447048144486, 0.4075009240860455462, -2.029694874052537568 ) ) ;
#164558 = CARTESIAN_POINT ( 'NONE',  ( 5.738125327081736060, 7.717565519727259904, 1.599625672291267398 ) ) ;
#164559 = CARTESIAN_POINT ( 'NONE',  ( -7.562750758324527922, 7.717630727667075696, 1.040834085586084257E-14 ) ) ;
#164560 = CARTESIAN_POINT ( 'NONE',  ( 1.826099658463333775, 3.981846818257634979, -0.4000000000000274447 ) ) ;
#164561 = CARTESIAN_POINT ( 'NONE',  ( 5.431901110126942989, -1.969610648168946376, 0.4466083225366457854 ) ) ;
#164562 = CARTESIAN_POINT ( 'NONE',  ( 1.499999999999985123, -0.9229166659838452524, -0.8660254037844323793 ) ) ;
#164563 = CARTESIAN_POINT ( 'NONE',  ( 3.897355454345535097, 1.950357463199345442, -1.233256315927799607 ) ) ;
#164564 = CARTESIAN_POINT ( 'NONE',  ( 1.516546868092843781, 0.8322427235708649285, 1.887369835301610621 ) ) ;
#164565 = CARTESIAN_POINT ( 'NONE',  ( 6.643132081016105417, 10.69414516125339887, 0.7216878364870438212 ) ) ;
#164566 = CARTESIAN_POINT ( 'NONE',  ( 7.340813827156391191, 7.528980651296110160, 0.7998128361456281477 ) ) ;
#164567 = CARTESIAN_POINT ( 'NONE',  ( 5.712781623311797397, 7.758274208654143855, -1.599625672291283607 ) ) ;
#164568 = CARTESIAN_POINT ( 'NONE',  ( -0.6823417656250003738, 1.280208333674752508, -1.181850606188749264 ) ) ;
#164569 = CARTESIAN_POINT ( 'NONE',  ( 5.890091390494168522, 5.836471141856793388, 0.000000000000000000 ) ) ;
#164570 = CARTESIAN_POINT ( 'NONE',  ( 5.734735788456138295, 8.673980272298743799, -1.082531754730537976 ) ) ;
#164572 = CARTESIAN_POINT ( 'NONE',  ( -2.713063801223519089, 3.002997225240221280, -2.500000000000000444 ) ) ;
#164571 = CARTESIAN_POINT ( 'NONE',  ( 3.666621648402784484, -0.8769701800699877259, -1.986351817242467677 ) ) ;
#164573 = CARTESIAN_POINT ( 'NONE',  ( -3.192880356576565770, 6.433770387723418693, -0.7510166236791281369 ) ) ;
#164575 = CARTESIAN_POINT ( 'NONE',  ( 2.929072846782492245, -1.238530643895646488, -1.362589426554157157 ) ) ;
#164574 = CARTESIAN_POINT ( 'NONE',  ( -5.111060722671894929, 5.065251719313053513, 0.000000000000000000 ) ) ;
#164576 = CARTESIAN_POINT ( 'NONE',  ( -1.364683531249997417, 5.009375000341425022, 1.214306433183764966E-14 ) ) ;
#164577 = CARTESIAN_POINT ( 'NONE',  ( 3.843468145482428877, 0.7371271433744167600, -2.064019554291535830 ) ) ;
#164578 = CARTESIAN_POINT ( 'NONE',  ( 8.568388180517228392, 13.84533258836909475, 8.337145738167963671 ) ) ;
#164579 = CARTESIAN_POINT ( 'NONE',  ( 5.436487035374818255, 2.228047177662040301, 0.3926572465528885281 ) ) ;
#164580 = CARTESIAN_POINT ( 'NONE',  ( -5.444063778538836829, 6.456803583937833046, -1.314021404191120901 ) ) ;
#164581 = CARTESIAN_POINT ( 'NONE',  ( 4.893454165248502186, 8.027304163657891678, -0.9628252682179049282 ) ) ;
#164582 = CARTESIAN_POINT ( 'NONE',  ( -5.655159470231558849, 6.730679149092498648, 1.082531754730549078 ) ) ;
#164583 = CARTESIAN_POINT ( 'NONE',  ( 3.418064124421011041, 7.001842221884225559, -0.7216878364870338292 ) ) ;
#164584 = CARTESIAN_POINT ( 'NONE',  ( 6.344957943996793581, -1.493715166628902580, 0.9487403735100213842 ) ) ;
#164585 = CARTESIAN_POINT ( 'NONE',  ( 3.598294619042395226, -0.9903900195140210583, 1.752531985089557098 ) ) ;
#164586 = CARTESIAN_POINT ( 'NONE',  ( 6.337546739384100292, 9.481222731668410120, 1.199719254218460707 ) ) ;
#164587 = CARTESIAN_POINT ( 'NONE',  ( 2.872209793879555217, 1.125368584265328264, 1.779858853945482489 ) ) ;
#164588 = CARTESIAN_POINT ( 'NONE',  ( 1.686979003181095615, 1.593666142434764454, 1.062572995559516009 ) ) ;
#164589 = CARTESIAN_POINT ( 'NONE',  ( 3.497113557321089861, 6.167384019261527683, -1.199719254218446718 ) ) ;
#164590 = CARTESIAN_POINT ( 'NONE',  ( 3.279706249791583872, -1.898816934168370496, 0.5228806403664593150 ) ) ;
#164591 = CARTESIAN_POINT ( 'NONE',  ( 4.851822172175670467, -1.431287984025449100, -1.425384875499214443 ) ) ;
#164592 = CARTESIAN_POINT ( 'NONE',  ( 0.2505829665140328899, -1.505242420826727656, 1.110479572284161831 ) ) ;
#164593 = CARTESIAN_POINT ( 'NONE',  ( 0.7659737006216191801, -1.952758744216346765, 0.1886366088557633325 ) ) ;
#164595 = VERTEX_POINT ( 'NONE', #176894 ) ;
#164594 = CARTESIAN_POINT ( 'NONE',  ( 0.2813230411330031044, 0.1852680230450229892, -1.903361379684164412 ) ) ;
#164596 = CARTESIAN_POINT ( 'NONE',  ( 5.016153647376205171, 6.875265226737464985, 1.443375672974062551 ) ) ;
#164597 = CARTESIAN_POINT ( 'NONE',  ( 0.6823417656249882723, 0.4052083336747516751, 1.181850606188755259 ) ) ;
#164599 = CARTESIAN_POINT ( 'NONE',  ( 5.787941465827733722, -0.8397648285632768328, 1.671655200917811168 ) ) ;
#164598 = AXIS2_PLACEMENT_3D ( 'NONE', #159717, #93675, #14510 ) ;
#164600 = CARTESIAN_POINT ( 'NONE',  ( 2.703961570921634028, 5.242040035128820108, -1.199719254218446718 ) ) ;
#164601 = CARTESIAN_POINT ( 'NONE',  ( 1.419999999999990603, 6.200000000000045475, 2.900000000000001688 ) ) ;
#164602 = ORIENTED_EDGE ( 'NONE', *, *, #184990, .T. ) ;
#164603 = CARTESIAN_POINT ( 'NONE',  ( 1.419999999999990603, 6.264000000000040203, 2.852000000000002089 ) ) ;
#164604 = DIRECTION ( 'NONE',  ( 0.000000000000000000, -1.000000000000000000, 0.000000000000000000 ) ) ;
#164605 = CARTESIAN_POINT ( 'NONE',  ( 0.6255436495894195481, 0.2045281481408110225, -2.060252820462626477 ) ) ;
#164607 = CARTESIAN_POINT ( 'NONE',  ( -1.499999999999997780, 2.400000000000020339, 1.214306433183764966E-14 ) ) ;
#164606 = COLOUR_RGB ( '', 0.08235294, 0.09019608, 0.10196078) ;
#164608 = CARTESIAN_POINT ( 'NONE',  ( 7.949158136313996259, 8.168439335321471262, 1.040834085586084257E-14 ) ) ;
#164609 = CARTESIAN_POINT ( 'NONE',  ( -7.181014916732457287, 11.52960116949655678, -0.7998128361456291469 ) ) ;
#164610 = CARTESIAN_POINT ( 'NONE',  ( 5.448397627845284141, 7.449826213943242514, 1.599625672291268286 ) ) ;
#164611 = CARTESIAN_POINT ( 'NONE',  ( 5.479186192515411946, -1.917069751554843160, -0.9065152316691318379 ) ) ;
#164612 = CARTESIAN_POINT ( 'NONE',  ( 5.246079093845007257, 5.085123462432798114, 0.7998128361456352531 ) ) ;
#164613 = CARTESIAN_POINT ( 'NONE',  ( -0.6823417656250003738, 1.467708333674752730, -1.181850606188749264 ) ) ;
#164614 = CARTESIAN_POINT ( 'NONE',  ( 0.7499999999999902300, 2.733333333333351600, 1.299038105676669330 ) ) ;
#164616 = CARTESIAN_POINT ( 'NONE',  ( 3.334415713957098681, 5.977569868670206787, -1.199719254218446718 ) ) ;
#164615 = CARTESIAN_POINT ( 'NONE',  ( 6.004347769543215030, 1.959566550440184907, 0.09775035808561728656 ) ) ;
#164617 = CARTESIAN_POINT ( 'NONE',  ( 4.077499844852236599, 1.427718728413525318, -1.423743541103118737 ) ) ;
#164618 = CARTESIAN_POINT ( 'NONE',  ( 3.678834806144789749, 1.615436204272060472, -1.029439157428935658 ) ) ;
#164619 = CARTESIAN_POINT ( 'NONE',  ( 11.80235830595198543, 9.799999999999998934, -1.696088231482801856 ) ) ;
#164620 = CARTESIAN_POINT ( 'NONE',  ( 1.786939262935317130, 1.904797134731281538, -1.083727916527020607 ) ) ;
#164621 = CARTESIAN_POINT ( 'NONE',  ( 0.1331715793776314105, 6.947497095909970000, -2.548608419791003055 ) ) ;
#164622 = CARTESIAN_POINT ( 'NONE',  ( 3.268673085221412311, -1.727008210369033847, -0.7190761260571986169 ) ) ;
#164623 = CARTESIAN_POINT ( 'NONE',  ( 1.499999999999987121, -0.9645833326505173222, 0.8660254037844524744 ) ) ;
#164624 = CARTESIAN_POINT ( 'NONE',  ( -7.802881099864745984, 9.062115023719057305, -1.199719254218446718 ) ) ;
#164626 = CARTESIAN_POINT ( 'NONE',  ( 5.097310499321968003, -0.3096355862501755096, 2.094337834851481617 ) ) ;
#164625 = CARTESIAN_POINT ( 'NONE',  ( -3.294268138440636928, 6.787137228248626641, 1.040834085586084257E-14 ) ) ;
#164628 = EDGE_CURVE ( 'NONE', #67975, #85030, #156961, .T. ) ;
#164627 = CARTESIAN_POINT ( 'NONE',  ( 1.364683531249997417, 8.796875000341403350, 2.602085213965210642E-15 ) ) ;
#164629 = CARTESIAN_POINT ( 'NONE',  ( -10.98997987423604172, -6.893137084989842123, 0.4694063952341877011 ) ) ;
#164631 = CARTESIAN_POINT ( 'NONE',  ( 4.033414559382754838, 7.548954524214963158, -0.4004916564768338794 ) ) ;
#164630 = CARTESIAN_POINT ( 'NONE',  ( 2.296528860280427686, 1.677371239548936854, -1.247825592998616617 ) ) ;
#164633 = ORIENTED_EDGE ( 'NONE', *, *, #111938, .T. ) ;
#164632 = CARTESIAN_POINT ( 'NONE',  ( 1.043494860557155679, 0.7046062621528689229, -1.574481895975497592 ) ) ;
#164634 = CARTESIAN_POINT ( 'NONE',  ( 6.775324078527185989, 8.927630729746953264, -1.599625672291262513 ) ) ;
#164635 = SURFACE_STYLE_FILL_AREA ( #197125 ) ;
#164636 = DIRECTION ( 'NONE',  ( -1.000000000000000000, 5.578564026256490882E-16, -1.264049978315544409E-61 ) ) ;
#164637 = CARTESIAN_POINT ( 'NONE',  ( 0.000000000000000000, 0.5000000000000004441, 0.000000000000000000 ) ) ;
#164639 = CARTESIAN_POINT ( 'NONE',  ( 9.883530794237934458, 10.63313346947350269, -0.7216878364870257245 ) ) ;
#164638 = CARTESIAN_POINT ( 'NONE',  ( 6.551614543901692400, 8.666636272683888365, 1.599625672291281386 ) ) ;
#164640 = CARTESIAN_POINT ( 'NONE',  ( -1.893304937267642707, 3.295344712542805254, 0.4038802767148285677 ) ) ;
#164642 = CARTESIAN_POINT ( 'NONE',  ( 1.928074960669722504, -0.8543848903827315766, -1.597334059258429972 ) ) ;
#164641 = CARTESIAN_POINT ( 'NONE',  ( 6.378184920586140727, 6.405913593630768510, 0.000000000000000000 ) ) ;
#164644 = CARTESIAN_POINT ( 'NONE',  ( -5.371001409308059138, 9.417918744168066070, -0.7998128361456231517 ) ) ;
#164643 = TOROIDAL_SURFACE ( 'NONE', #133449, 10.92000000000000171, 0.08000000000000000167 ) ;
#164645 = CARTESIAN_POINT ( 'NONE',  ( 5.840865249388943248, 5.708764300575555062, 0.7998128361456341429 ) ) ;
#164646 = CARTESIAN_POINT ( 'NONE',  ( -6.497792602234238934, 6.760263899176822022, -0.1076752790035370722 ) ) ;
#164647 = CARTESIAN_POINT ( 'NONE',  ( 7.049313524462606395, 7.188896964819984525, 0.000000000000000000 ) ) ;
#164648 = LINE ( 'NONE', #83378, #135948 ) ;
#164649 = CARTESIAN_POINT ( 'NONE',  ( 1.836970198721030181E-16, 13.49999999999999822, 1.500000000000000222 ) ) ;
#164650 = CARTESIAN_POINT ( 'NONE',  ( 3.998873522394119195, 7.597518543056763995, -0.1390531931140040478 ) ) ;
#164651 = CARTESIAN_POINT ( 'NONE',  ( 9.164948653157988900, 11.71552606681625619, -1.443375672974057666 ) ) ;
#164652 = VERTEX_POINT ( 'NONE', #113032 ) ;
#164653 = CARTESIAN_POINT ( 'NONE',  ( 3.420197418661593769, 0.8345380353566893561, 1.663503485505882118 ) ) ;
#164654 = CARTESIAN_POINT ( 'NONE',  ( 0.8080361750046762825, 1.140156559909396128, -1.539198610912548171 ) ) ;
#164655 = CARTESIAN_POINT ( 'NONE',  ( 6.616243401494351417, -0.9090183210780745648, -1.698415751782512695 ) ) ;
#164656 = CARTESIAN_POINT ( 'NONE',  ( 5.898901817742317810, 0.4001337562283372451, 2.031160294743330486 ) ) ;
#164657 = CARTESIAN_POINT ( 'NONE',  ( -0.4500000000000389244, 3.999999999999948042, 0.4999999999999779066 ) ) ;
#164658 = CARTESIAN_POINT ( 'NONE',  ( 4.611577566919329740, 8.352668595566711929, -0.2595669225248058432 ) ) ;
#164659 = DIRECTION ( 'NONE',  ( -0.000000000000000000, -1.000000000000000000, -0.000000000000000000 ) ) ;
#164660 = CARTESIAN_POINT ( 'NONE',  ( -3.307826292054310890, 5.842585859829892314, -1.082531754730549967 ) ) ;
#164661 = CARTESIAN_POINT ( 'NONE',  ( 8.351459436338029008, 10.76645531385962862, -1.443375672974063439 ) ) ;
#164662 = CARTESIAN_POINT ( 'NONE',  ( 4.170725306337518923, 1.395817779951594950, -1.389658704579323611 ) ) ;
#164663 = CARTESIAN_POINT ( 'NONE',  ( 1.576976220782677185, -1.497206391897941691, 1.501870991332490357 ) ) ;
#164664 = CARTESIAN_POINT ( 'NONE',  ( -4.706651882238427120, 8.642844295920152575, 1.040834085586084257E-14 ) ) ;
#164665 = DIRECTION ( 'NONE',  ( 0.000000000000000000, 1.000000000000000000, 0.000000000000000000 ) ) ;
#164666 = FACE_OUTER_BOUND ( 'NONE', #138302, .T. ) ;
#164667 = CARTESIAN_POINT ( 'NONE',  ( 5.472676780243426187, -0.05103125619924236966, -2.191024458042860168 ) ) ;
#164668 =( LENGTH_UNIT ( ) NAMED_UNIT ( * ) SI_UNIT ( .MILLI., .METRE. ) );
#164669 = CARTESIAN_POINT ( 'NONE',  ( 3.961874236345910294, 1.911929771648058995, -0.2350156305768891229 ) ) ;
#164670 = CARTESIAN_POINT ( 'NONE',  ( -6.718228810771495141, 7.796687353110217877, 1.199719254218450271 ) ) ;
#164671 = CARTESIAN_POINT ( 'NONE',  ( 0.3229203692996869823, -0.09522068211164493035, 1.823229820405058099 ) ) ;
#164672 = CARTESIAN_POINT ( 'NONE',  ( 0.5400322017136415242, -1.563516176313231920, -1.557742479837947558 ) ) ;
#164673 = SURFACE_STYLE_USAGE ( .BOTH. , #95443 ) ;
#164674 = VERTEX_POINT ( 'NONE', #83643 ) ;
#164675 = ORIENTED_EDGE ( 'NONE', *, *, #38065, .F. ) ;
#164676 = CARTESIAN_POINT ( 'NONE',  ( 5.998876245820001785, 0.3805640578184403822, 1.932138370648580628 ) ) ;
#164677 = CARTESIAN_POINT ( 'NONE',  ( 1.487729058832359952, -1.932848847819462756, -0.1887428500492206451 ) ) ;
#164678 = CARTESIAN_POINT ( 'NONE',  ( 6.415373042369045820, 0.7112672321729663905, 2.185653275185605704 ) ) ;
#164680 = CARTESIAN_POINT ( 'NONE',  ( 5.612096381091351560, 1.858897858770152789, -0.08933831184920922042 ) ) ;
#164679 = CARTESIAN_POINT ( 'NONE',  ( -6.149505192250180663, 9.332117270003974951, -1.199719254218452047 ) ) ;
#164681 = CARTESIAN_POINT ( 'NONE',  ( 7.035755370848908896, 7.173079118937375931, 0.7998128361456352531 ) ) ;
#164682 = DIRECTION ( 'NONE',  ( -0.6507913734559640506, -0.7592566023653003482, 0.000000000000000000 ) ) ;
#164683 = SURFACE_SIDE_STYLE ('',( #98622 ) ) ;
#164684 = B_SPLINE_CURVE_WITH_KNOTS ( 'NONE', 3,
 ( #13072, #79151, #46674, #145268, #211275, #62898, #162556, #214410, #44547, #129068, #12013, #110662, #82341, #94368, #131172, #112794, #30421, #96506, #213395, #146319, #212334, #63972, #130128, #66065, #192890, #144211, #47753, #15201, #113868, #179863, #176663 ),
 .UNSPECIFIED., .F., .F.,
 ( 4, 2, 2, 2, 2, 2, 2, 2, 2, 2, 2, 2, 1, 2, 2, 4 ),
 ( 0.1193258592806614310, 0.1284789785326313494, 0.1376320977846012539, 0.1422086574105862200, 0.1467852170365712139, 0.1559383362885412294, 0.1582266161015338513, 0.1605148959145265009, 0.1650914555405115225, 0.1696680151664965996, 0.1708121550729926885, 0.1719562949794887774, 0.1742445747924811217, 0.1833976940444502213, 0.1879742536704346878, 0.1925508132964191543 ),
 .UNSPECIFIED. ) ;
#164685 = CARTESIAN_POINT ( 'NONE',  ( -7.054319997812058318, 7.124461507069184130, 1.040834085586084257E-14 ) ) ;
#164686 = CARTESIAN_POINT ( 'NONE',  ( -3.320873661936399657, -0.9167811538275831840, 0.1393910267247679413 ) ) ;
#164687 = CARTESIAN_POINT ( 'NONE',  ( 1.031118135130421498, -1.979082047791239418, 0.9416876394413642437 ) ) ;
#164688 = CARTESIAN_POINT ( 'NONE',  ( 3.362058906508953449, 6.866226457661676719, -0.7216878364870267237 ) ) ;
#164689 = CARTESIAN_POINT ( 'NONE',  ( 10.85699613887011772, -6.836286050428144634, -0.3891817118475866533 ) ) ;
#164690 = CARTESIAN_POINT ( 'NONE',  ( 1.277666653898035021, 1.085793613588705853, 1.467558327050644484 ) ) ;
#164691 = CARTESIAN_POINT ( 'NONE',  ( -4.796887421136680985, 4.490790167614548523, 1.214306433183764966E-14 ) ) ;
#164692 = CARTESIAN_POINT ( 'NONE',  ( -6.402982088906444602, 6.898597865962027065, -0.7910698893406533649 ) ) ;
#164693 = CARTESIAN_POINT ( 'NONE',  ( 6.609000000000047947, 2.032467779867861868, 2.404707446487294842 ) ) ;
#164694 = CARTESIAN_POINT ( 'NONE',  ( -10.85353573482952072, -6.836568542495036205, 0.4635785636673775967 ) ) ;
#164695 = CARTESIAN_POINT ( 'NONE',  ( 6.463509179248937642, 0.3066564278407272748, -1.799597105106438777 ) ) ;
#164696 = CARTESIAN_POINT ( 'NONE',  ( 4.381663332995835880, -1.878531202089319896, 0.5654445158327011667 ) ) ;
#164697 = CARTESIAN_POINT ( 'NONE',  ( -7.609150525767646833, 9.900428251527500834, -1.599625672291263179 ) ) ;
#164698 = CARTESIAN_POINT ( 'NONE',  ( 5.262536180398716290, 9.291375977107183104, -0.7998128361456291469 ) ) ;
#164699 = CARTESIAN_POINT ( 'NONE',  ( 5.127636373287420390, -0.3106611864900839515, 2.097473367668806876 ) ) ;
#164700 = CARTESIAN_POINT ( 'NONE',  ( -8.941766003412679353, 10.39081407785832845, -1.199719254218446718 ) ) ;
#164701 = CARTESIAN_POINT ( 'NONE',  ( 6.609000000000036401, 0.5823242425131782696, 2.053003180352876100 ) ) ;
#164702 = CARTESIAN_POINT ( 'NONE',  ( 2.870052101067874339, -2.048368873657464118, 0.2992715783270774588 ) ) ;
#164704 = CARTESIAN_POINT ( 'NONE',  ( -0.6823417656250003738, -0.2197916663252488800, -1.181850606188749264 ) ) ;
#164703 = CARTESIAN_POINT ( 'NONE',  ( -0.09500528524172231759, -5.338246727548288995, -10.99984294789629935 ) ) ;
#164705 = VERTEX_POINT ( 'NONE', #82578 ) ;
#164706 = CARTESIAN_POINT ( 'NONE',  ( 2.813438166105670657, 1.274540910030600216, -1.912834453734891804 ) ) ;
#164707 = CARTESIAN_POINT ( 'NONE',  ( 7.131225611108079399, 11.26358761302737754, 0.7216878364870438212 ) ) ;
#164709 = CARTESIAN_POINT ( 'NONE',  ( -3.285556943750000514, -1.538541666188708357, -1.896917185911906500 ) ) ;
#164708 = CARTESIAN_POINT ( 'NONE',  ( 6.888951449519509218, 7.209733910627123876, -0.7216878364870317197 ) ) ;
#164710 = SPHERICAL_SURFACE ( 'NONE', #196208, 0.05000000000000000278 ) ;
#164711 = CARTESIAN_POINT ( 'NONE',  ( 1.464175926609780964E-14, -2.187499999999999112, -3.475000000000000533 ) ) ;
#164712 = VERTEX_POINT ( 'NONE', #98853 ) ;
#164713 = CARTESIAN_POINT ( 'NONE',  ( -0.1817359287055335115, -9.181675805132242019, 9.625413980971107009 ) ) ;
#164714 = CARTESIAN_POINT ( 'NONE',  ( 4.447458312869024155, -1.746245811230532130, 0.7801085911468002010 ) ) ;
#164715 = FILL_AREA_STYLE_COLOUR ( '', #162119 ) ;
#164716 = CARTESIAN_POINT ( 'NONE',  ( 4.963727558602625933, 1.705580761961351444, -0.2555711148431466517 ) ) ;
#164717 = CARTESIAN_POINT ( 'NONE',  ( 2.993375309983861143, -0.3886322325962355273, 1.978555244300662874 ) ) ;
#164718 = CARTESIAN_POINT ( 'NONE',  ( 5.309350125645185159, 1.371050412704700516, -1.844953357796705218 ) ) ;
#164719 = CARTESIAN_POINT ( 'NONE',  ( -11.55950211276791251, 12.22000000000000064, -3.221476510067115662 ) ) ;
#164720 = CARTESIAN_POINT ( 'NONE',  ( 0.6278963055918493907, -2.094311335337955882, 0.6960538111202837497 ) ) ;
#164721 = CARTESIAN_POINT ( 'NONE',  ( -4.828112100242294424, 5.765790550771681566, -1.082531754730549967 ) ) ;
#164722 = CARTESIAN_POINT ( 'NONE',  ( 5.624192029756354572, 1.053330351427090639, -1.421934073773284180 ) ) ;
#164724 = CARTESIAN_POINT ( 'NONE',  ( 2.115536061532933942, -2.222870945405757137, 0.5592890022133433225 ) ) ;
#164723 = CARTESIAN_POINT ( 'NONE',  ( 6.119526231721748033, 8.232809585132461194, 1.599625672291269396 ) ) ;
#164725 = CARTESIAN_POINT ( 'NONE',  ( 6.281194495005370193, 1.273289214079580622, 1.330099835651930684 ) ) ;
#164726 = CARTESIAN_POINT ( 'NONE',  ( 0.5723599497803509850, 4.245284329187786199, -0.3124809264750579851 ) ) ;
#164727 = PLANE ( 'NONE',  #142093 ) ;
#164728 = CARTESIAN_POINT ( 'NONE',  ( -3.494969737272722643, 7.299491470118629088, -0.7998128361456481317 ) ) ;
#164729 = CARTESIAN_POINT ( 'NONE',  ( -0.6801582343750334214, 1.213541667008023683, 1.178068619123810334 ) ) ;
#164730 = DIRECTION ( 'NONE',  ( -0.000000000000000000, 1.000000000000000000, 0.000000000000000000 ) ) ;
#164731 = CARTESIAN_POINT ( 'NONE',  ( 0.1511277727459575393, -0.4806850054440474085, -2.125521221522770787 ) ) ;
#164732 = CARTESIAN_POINT ( 'NONE',  ( 2.237517880698642880, 0.5331670712399002587, -1.944730990508992008 ) ) ;
#164733 = CARTESIAN_POINT ( 'NONE',  ( -0.7500000000000006661, 0.3895833340161539149, -1.299038105676652011 ) ) ;
#164734 = CARTESIAN_POINT ( 'NONE',  ( 5.654890666209754002, -1.517393486936137403, 1.186882646050735346 ) ) ;
#164735 = CARTESIAN_POINT ( 'NONE',  ( -1.364683531250010295, 12.38020833367473372, 0.7879004041258445001 ) ) ;
#164736 = CARTESIAN_POINT ( 'NONE',  ( 2.057158355326561772, 0.4919409011131297138, 2.166103627455501890 ) ) ;
#164737 = ORIENTED_EDGE ( 'NONE', *, *, #157427, .T. ) ;
#164738 = CARTESIAN_POINT ( 'NONE',  ( 6.637758778446686492, -7.996947095390841476, 6.849430810391425872 ) ) ;
#164739 = CARTESIAN_POINT ( 'NONE',  ( -5.194182247366913252, 7.153241603385088965, 1.443375672974058777 ) ) ;
#164740 = CARTESIAN_POINT ( 'NONE',  ( 8.191097360950562845, 12.70803068775103739, -0.7998128361456352531 ) ) ;
#164741 = DIRECTION ( 'NONE',  ( 0.000000000000000000, 1.000000000000000000, 0.000000000000000000 ) ) ;
#164742 = EDGE_CURVE ( 'NONE', #96990, #104450, #42530, .T. ) ;
#164743 = SURFACE_STYLE_FILL_AREA ( #113942 ) ;
#164744 = CARTESIAN_POINT ( 'NONE',  ( 4.985792865680892305, -1.728136641771714777, -0.2059490554011476626 ) ) ;
#164745 = CARTESIAN_POINT ( 'NONE',  ( 3.033595934319989418, 1.863777508880835487, -0.6128360024686765328 ) ) ;
#164747 = CARTESIAN_POINT ( 'NONE',  ( -7.592202833972775622, 8.920286730132099606, 1.082531754730558626 ) ) ;
#164746 = CARTESIAN_POINT ( 'NONE',  ( 5.183294799126148433, 4.941598775268944976, 1.040834085586084257E-14 ) ) ;
#164748 = EDGE_CURVE ( 'NONE', #105884, #32900, #65472, .T. ) ;
#164749 = CARTESIAN_POINT ( 'NONE',  ( -5.796211742468360129, 6.069872997065163922, -0.5622600474686073602 ) ) ;
#164750 = CARTESIAN_POINT ( 'NONE',  ( 5.079486683540675784, 2.113528219476542347, -0.8076395688127128158 ) ) ;
#164751 = AXIS2_PLACEMENT_3D ( 'NONE', #55376, #204795, #174485 ) ;
#164752 = CARTESIAN_POINT ( 'NONE',  ( 1.539586554034046539, 1.906627302964102988, -0.7874849336161419133 ) ) ;
#164753 = CARTESIAN_POINT ( 'NONE',  ( -6.170932472514347289, 10.35117165124207972, 0.000000000000000000 ) ) ;
#164754 = CARTESIAN_POINT ( 'NONE',  ( -3.050221372950322252, 5.542046787541873520, 1.082531754730560403 ) ) ;
#164755 = AXIS2_PLACEMENT_3D ( 'NONE', #196667, #46174, #98122 ) ;
#164756 = CARTESIAN_POINT ( 'NONE',  ( 1.868429791336771340, 1.163878172895687069, 1.940057763798187951 ) ) ;
#164757 = ORIENTED_EDGE ( 'NONE', *, *, #33674, .T. ) ;
#164758 = CARTESIAN_POINT ( 'NONE',  ( -1.402160292154681736E-14, -0.2562499993171780122, 1.732050807568877637 ) ) ;
#164759 = CARTESIAN_POINT ( 'NONE',  ( 2.196370303256788503, -0.4943915968025693330, -1.803980227719769847 ) ) ;
#164760 = CARTESIAN_POINT ( 'NONE',  ( 0.8438932004057161373, 0.3398822538093429491, -1.700291973301551129 ) ) ;
#164761 = CARTESIAN_POINT ( 'NONE',  ( 5.812113132715003516, 1.472855484078567700, -1.623034594306454137 ) ) ;
#164762 = CARTESIAN_POINT ( 'NONE',  ( 6.299901696735699552, -0.7855725015378700604, 2.169893659913350259 ) ) ;
#164763 = CARTESIAN_POINT ( 'NONE',  ( 0.7079729303958534059, -2.051031625230379074, 0.2011725655505970656 ) ) ;
#164764 = CARTESIAN_POINT ( 'NONE',  ( 4.822180446859828606, 1.858854579410177843, 0.5619951038204271665 ) ) ;
#164765 = CARTESIAN_POINT ( 'NONE',  ( -8.482597663644387609, 13.04811437422715414, -0.7998128361456281477 ) ) ;
#164766 = ADVANCED_FACE ( 'NONE', ( #81525 ), #130356, .T. ) ;
#164767 = CARTESIAN_POINT ( 'NONE',  ( 6.643822754079466542, 0.7155741859487285694, -1.728458771772640512 ) ) ;
#164768 = CARTESIAN_POINT ( 'NONE',  ( 1.000000000000000666, -5.752119711681284071E-14, -2.052068128417952053 ) ) ;
#164769 = CARTESIAN_POINT ( 'NONE',  ( 1.500000000000035971, 8.500000000000000000, 9.886859966642587594 ) ) ;
#164770 = CARTESIAN_POINT ( 'NONE',  ( 6.872432811717262169, -0.4447407475622888740, 1.973694069355651282 ) ) ;
#164771 = CARTESIAN_POINT ( 'NONE',  ( 11.89197369110779334, 12.30000000000000249, 0.8056055387119843703 ) ) ;
#164772 = CARTESIAN_POINT ( 'NONE',  ( 1.360316468749966257, 1.765625000341414230, -3.642919299551294898E-14 ) ) ;
#164773 = CARTESIAN_POINT ( 'NONE',  ( 6.065077313367789102, -1.076319894221990259, 1.704936797084610101 ) ) ;
#164774 = CARTESIAN_POINT ( 'NONE',  ( -8.642432853707342488, 12.17025653171218558, 1.199719254218462483 ) ) ;
#164775 = CARTESIAN_POINT ( 'NONE',  ( 8.284195553149872993, 9.623648552551724578, -1.199719254218445830 ) ) ;
#164776 = CARTESIAN_POINT ( 'NONE',  ( 5.239300017038202917, 5.077214539491492928, 0.000000000000000000 ) ) ;
#164777 = CARTESIAN_POINT ( 'NONE',  ( 2.209345402013741300, -0.4006574107652469130, 1.781019818369505847 ) ) ;
#164778 = CARTESIAN_POINT ( 'NONE',  ( -1.001543065824772872E-14, 5.212500000000019895, 1.732050807568877637 ) ) ;
#164779 = CARTESIAN_POINT ( 'NONE',  ( -9.429696025003076798, 5.003427382976973981, 6.891771494149568689 ) ) ;
#164780 = ORIENTED_EDGE ( 'NONE', *, *, #3407, .F. ) ;
#164781 = CARTESIAN_POINT ( 'NONE',  ( -3.784134271545645412, 7.428924060196286483, 0.7216878364870338292 ) ) ;
#164782 = CARTESIAN_POINT ( 'NONE',  ( -3.285556943750000514, -3.376041666188708490, -1.896917185911906500 ) ) ;
#164783 = CARTESIAN_POINT ( 'NONE',  ( -7.784352752540590004, 12.23349531127272094, 0.7998128361456481317 ) ) ;
#164784 = CARTESIAN_POINT ( 'NONE',  ( 0.3869806665078223129, -1.903265420633104332, -0.6765555904410057719 ) ) ;
#164785 = CARTESIAN_POINT ( 'NONE',  ( 0.2938078718510480081, 1.976988316466289142, -0.7672523047414223640 ) ) ;
#164786 = EDGE_LOOP ( 'NONE', ( #203356, #212537, #29864, #87394 ) ) ;
#164787 = CARTESIAN_POINT ( 'NONE',  ( -7.611976899429754084, 7.845337568948314022, 0.7998128361456341429 ) ) ;
#164788 = CARTESIAN_POINT ( 'NONE',  ( 5.054492339796319733, 4.791329239384148231, -0.7998128361456211532 ) ) ;
#164789 = CARTESIAN_POINT ( 'NONE',  ( 6.121960869219821966, -1.142753529713343763, -1.714830629803126616 ) ) ;
#164790 = CARTESIAN_POINT ( 'NONE',  ( 4.729138786257041538, 2.011204126674607462, 0.1455352507326590494 ) ) ;
#164791 = ORIENTED_EDGE ( 'NONE', *, *, #153405, .T. ) ;
#164792 = CARTESIAN_POINT ( 'NONE',  ( 4.743677682280330821, 4.888648074256856546, -0.7989307584942272333 ) ) ;
#164793 = CARTESIAN_POINT ( 'NONE',  ( 5.969332771766739931, 10.18624834369502885, -0.7998128361456481317 ) ) ;
#164794 = AXIS2_PLACEMENT_3D ( 'NONE', #133498, #117269, #199501 ) ;
#164797 = ORIENTED_EDGE ( 'NONE', *, *, #48830, .T. ) ;
#164796 = DIRECTION ( 'NONE',  ( -1.276756478318932191E-15, 1.000000000000000000, -3.330669073875483426E-16 ) ) ;
#164795 = CARTESIAN_POINT ( 'NONE',  ( -5.631432701629818460, 7.663367133358481631, 1.599625672291263179 ) ) ;
#164798 = CARTESIAN_POINT ( 'NONE',  ( 5.820234798683411981, 7.319712794923219690, 1.284739950006764220 ) ) ;
#164799 = CARTESIAN_POINT ( 'NONE',  ( 5.009138659175729202, 2.010518709310470609, 0.1511151588593287465 ) ) ;
#164800 = CARTESIAN_POINT ( 'NONE',  ( 4.505690185649424251, -0.7896136771840707169, -1.663358820747300237 ) ) ;
#164801 = CARTESIAN_POINT ( 'NONE',  ( -0.02338929933909470252, 5.726375320706490690, -2.305055744220934066 ) ) ;
#164802 = CARTESIAN_POINT ( 'NONE',  ( 3.563348594130168578, -2.034784092110089926, -1.088618498840478566 ) ) ;
#164803 = CARTESIAN_POINT ( 'NONE',  ( 5.830888582329017744, 8.960397891762626799, -1.199719254218452047 ) ) ;
#164804 = CARTESIAN_POINT ( 'NONE',  ( 6.011032505573889573, 1.903242638633116712, 1.024824547371510075 ) ) ;
#164805 = CARTESIAN_POINT ( 'NONE',  ( 6.337546739384100292, 9.481222731668410120, 1.199719254218460707 ) ) ;
#164806 = CARTESIAN_POINT ( 'NONE',  ( 1.470153547685297823, -1.844723335029124112, -0.6073778784492619431 ) ) ;
#164807 = CARTESIAN_POINT ( 'NONE',  ( -5.298539104842322267, 5.076050465271134016, 0.7998128361456341429 ) ) ;
#164808 = VECTOR ( 'NONE', #125450, 1000.000000000000000 ) ;
#164809 = CARTESIAN_POINT ( 'NONE',  ( 4.974093195743899187, 1.996273031041963408, 1.139003188958290780 ) ) ;
#164810 = CARTESIAN_POINT ( 'NONE',  ( -9.417646481058939756, 15.36155943915161259, -7.338279069507036567 ) ) ;
#164811 = CARTESIAN_POINT ( 'NONE',  ( -3.644109427023046521, 7.473487774827342278, 0.000000000000000000 ) ) ;
#164812 = CARTESIAN_POINT ( 'NONE',  ( 2.975316878787794828, 1.776827963633962559, -0.5852370025475408521 ) ) ;
#164816 = ADVANCED_FACE ( 'NONE', ( #17557 ), #47991, .T. ) ;
#164815 = CARTESIAN_POINT ( 'NONE',  ( -7.286581212701773502, 7.465709267765667789, 0.7998128361456341429 ) ) ;
#164814 = CARTESIAN_POINT ( 'NONE',  ( -1.402160292154681736E-14, -0.006249999317184824418, 1.732050807568877637 ) ) ;
#164813 = CARTESIAN_POINT ( 'NONE',  ( 1.441514601552947417, -1.799640695080907182, 0.6472408003148700795 ) ) ;
#164817 = CARTESIAN_POINT ( 'NONE',  ( 2.368051099418837069, 2.164043333312406503, -0.4318774905316472013 ) ) ;
#164818 = CARTESIAN_POINT ( 'NONE',  ( -1.499999999999998002, 8.673756432004008587, -2.614717076620595382 ) ) ;
#164819 = CARTESIAN_POINT ( 'NONE',  ( 4.552840656090682891, 4.206068941727564514, 1.214306433183764966E-14 ) ) ;
#164820 = CARTESIAN_POINT ( 'NONE',  ( 7.485510208076452621, 7.905719128943566432, 0.000000000000000000 ) ) ;
#164821 = CARTESIAN_POINT ( 'NONE',  ( -4.298098390732130625, 4.973201863064262263, 1.199719254218462483 ) ) ;
#164822 = CARTESIAN_POINT ( 'NONE',  ( -6.414416072596845986, 8.576847732820027659, -1.443375672974066548 ) ) ;
#164823 = CARTESIAN_POINT ( 'NONE',  ( 0.4210825541404016326, -0.1013260788591107547, 1.968891031686560211 ) ) ;
#164824 = ADVANCED_FACE ( 'NONE', ( #199516 ), #67082, .T. ) ;
#164825 = CARTESIAN_POINT ( 'NONE',  ( 0.07775346131144458828, -0.005211914751935413023, -2.288974916015192651 ) ) ;
#164826 = CARTESIAN_POINT ( 'NONE',  ( 1.469116868872882620, 1.728625619535430369, 0.9278086228877155950 ) ) ;
#164827 = CARTESIAN_POINT ( 'NONE',  ( 5.207907603007337016, 0.6519758639490059737, -1.956853833162349066 ) ) ;
#164828 = CARTESIAN_POINT ( 'NONE',  ( 4.528060117284232966, 6.305822774963486310, 1.443375672974062551 ) ) ;
#164829 = CARTESIAN_POINT ( 'NONE',  ( 5.182959862174088883, 9.268813282503625572, 0.7998128361456331437 ) ) ;
#164830 = ORIENTED_EDGE ( 'NONE', *, *, #31247, .T. ) ;
#164831 = CARTESIAN_POINT ( 'NONE',  ( -0.6823417656249969321, 5.280208333674756283, -1.181850606188749264 ) ) ;
#164832 = CARTESIAN_POINT ( 'NONE',  ( 6.776587425048107960, -7.030236945366980628, 6.796206128891409293 ) ) ;
#164833 = CARTESIAN_POINT ( 'NONE',  ( 3.185802909086945967, 5.700225246367978116, 1.082531754730546636 ) ) ;
#164834 = CARTESIAN_POINT ( 'NONE',  ( 0.6554289830566867314, 1.805916262795668192, -1.204791683884984810 ) ) ;
#164836 = CARTESIAN_POINT ( 'NONE',  ( 6.585540641348407220, -0.7802508550805786758, 1.666130356082275998 ) ) ;
#164835 = LINE ( 'NONE', #198377, #184243 ) ;
#164837 = CARTESIAN_POINT ( 'NONE',  ( 11.55950211276791251, 11.29999999999999893, -3.221476510067115662 ) ) ;
#164838 = PLANE ( 'NONE',  #42809 ) ;
#164839 = CARTESIAN_POINT ( 'NONE',  ( 1.422894040683621242, -0.05142188859055820543, 1.870020055627517275 ) ) ;
#164840 = CARTESIAN_POINT ( 'NONE',  ( 5.483715611629243369, 1.447241891022777560, 1.605803905980404123 ) ) ;
#164841 = CARTESIAN_POINT ( 'NONE',  ( -5.789194372615304118, 6.219231786955013774, 1.015549131865096211 ) ) ;
#164842 = DIRECTION ( 'NONE',  ( 0.000000000000000000, 0.000000000000000000, 1.000000000000000000 ) ) ;
#164843 = CARTESIAN_POINT ( 'NONE',  ( -0.6823417656249969321, 5.030208333674755394, -1.181850606188749264 ) ) ;
#164844 = CARTESIAN_POINT ( 'NONE',  ( 1.330556988563241561, 1.283596529665396169, -1.417643162000304935 ) ) ;
#164845 = CARTESIAN_POINT ( 'NONE',  ( 3.238855601640895809, -1.561498447111120402, 0.8330696194922878606 ) ) ;
#164846 = CARTESIAN_POINT ( 'NONE',  ( 0.3813228709106940006, 0.1872568833237615027, -1.903067810102520241 ) ) ;
#164848 = CARTESIAN_POINT ( 'NONE',  ( 5.149962951811881240, 0.9480454039230011842, 1.664493911490998679 ) ) ;
#164847 = CARTESIAN_POINT ( 'NONE',  ( -5.606595252507366567, 5.572856915785063592, -0.3451608010808376870 ) ) ;
#164849 = CARTESIAN_POINT ( 'NONE',  ( 6.848121164528643945, -0.8440317545377834518, 1.778091661420333702 ) ) ;
#164850 = CARTESIAN_POINT ( 'NONE',  ( -0.7499999999999972244, 4.358333333333352932, -1.299038105676652011 ) ) ;
#164851 = CARTESIAN_POINT ( 'NONE',  ( 1.494549364340029163, -1.129948290531690658, 1.794289463044356436 ) ) ;
#164852 = CARTESIAN_POINT ( 'NONE',  ( -0.07999999999999847511, 19.00000000000000000, 11.91973154060107376 ) ) ;
#164853 = CARTESIAN_POINT ( 'NONE',  ( 4.082764389539480732, -0.1829629792115642917, -1.861669828791753467 ) ) ;
#164855 = VERTEX_POINT ( 'NONE', #16497 ) ;
#164854 = CARTESIAN_POINT ( 'NONE',  ( 0.08226035653636187828, -1.769965142718381124, -0.4472663993063328847 ) ) ;
#164856 = CARTESIAN_POINT ( 'NONE',  ( 5.004599478379411437, -0.7411955310945415043, -2.078817424605138964 ) ) ;
#164857 = CARTESIAN_POINT ( 'NONE',  ( -1.001543065824772872E-14, 4.884375000341420581, 1.575800808251672791 ) ) ;
#164858 = CARTESIAN_POINT ( 'NONE',  ( 1.838405449727827268, -1.105357634037696046, 1.741336484761913272 ) ) ;
#164859 = CARTESIAN_POINT ( 'NONE',  ( 6.796715079152391148, 6.823922435299587974, 0.7998128361456341429 ) ) ;
#164860 = CARTESIAN_POINT ( 'NONE',  ( -8.690940161559884913, 10.09818392903003748, 1.199719254218462483 ) ) ;
#164861 = CYLINDRICAL_SURFACE ( 'NONE', #81728, 3.475000000000000089 ) ;
#164862 = DIRECTION ( 'NONE',  ( -0.000000000000000000, -1.000000000000000000, -0.000000000000000000 ) ) ;
#164863 = CARTESIAN_POINT ( 'NONE',  ( 1.500000000000053291, 7.750000000000000000, 15.74999999999999289 ) ) ;
#164864 = ORIENTED_EDGE ( 'NONE', *, *, #95230, .F. ) ;
#164865 = CARTESIAN_POINT ( 'NONE',  ( 3.947765587739564097, 1.497496809916948779, 1.429883829622953462 ) ) ;
#164866 = CARTESIAN_POINT ( 'NONE',  ( -1.201851678989727383E-14, 5.337500000000020783, -1.732050807568863648 ) ) ;
#164867 = CARTESIAN_POINT ( 'NONE',  ( 0.9663661119345480222, 1.064502738163356721, 1.881203019380036867 ) ) ;
#164868 = CARTESIAN_POINT ( 'NONE',  ( -6.146561906247310247, 6.992958819738270826, -0.9370148970899976337 ) ) ;
#164869 = CARTESIAN_POINT ( 'NONE',  ( 2.490883850439883140, -1.933321517186505245, -0.5842891067564592866 ) ) ;
#164870 = CARTESIAN_POINT ( 'NONE',  ( -6.471393748265563239, 5.229711127717889596, 2.499999999999998668 ) ) ;
#164871 = EDGE_LOOP ( 'NONE', ( #80479, #83218, #12213, #143773 ) ) ;
#164873 = CARTESIAN_POINT ( 'NONE',  ( 8.270110514656026979, 10.67154823856396817, 1.443375672974076540 ) ) ;
#164872 = CARTESIAN_POINT ( 'NONE',  ( 1.737499999999999378, -3.616666666666667140, -3.009438278150925683 ) ) ;
#164874 = CARTESIAN_POINT ( 'NONE',  ( 0.4288785890452679883, 3.049942316455285685, 0.3999999999999715450 ) ) ;
#164875 = CARTESIAN_POINT ( 'NONE',  ( -0.1003747550864658999, -1.976661868047492998, 0.3981153667176607902 ) ) ;
#164876 = CARTESIAN_POINT ( 'NONE',  ( 6.539320575229233157, 0.001224430076711413356, 2.103502572931112091 ) ) ;
#164877 = CARTESIAN_POINT ( 'NONE',  ( 5.425378541715013547, -1.389685604419872655, -1.694579525865949066 ) ) ;
#164879 = MECHANICAL_DESIGN_GEOMETRIC_PRESENTATION_REPRESENTATION (  '', ( #64532 ), #57738 ) ;
#164878 = CARTESIAN_POINT ( 'NONE',  ( -1.201851678989727383E-14, 3.243750000682814161, 1.732050807568877637 ) ) ;
#164880 = CARTESIAN_POINT ( 'NONE',  ( 3.410326831400651404, -1.910418641682644969, -0.08914582809275289899 ) ) ;
#164881 = CARTESIAN_POINT ( 'NONE',  ( -4.090809663021341969, 5.795697244990093644, 1.599625672291267398 ) ) ;
#164882 = CARTESIAN_POINT ( 'NONE',  ( 3.321384445223597659, 6.818772919495430074, -0.7216878364870267237 ) ) ;
#164884 = CARTESIAN_POINT ( 'NONE',  ( 2.653922917551009952, 1.081085551080329443, 1.701936510390424928 ) ) ;
#164883 = CARTESIAN_POINT ( 'NONE',  ( -10.61567108937589765, 11.48729714713446803, 0.7216878364870438212 ) ) ;
#164885 = CARTESIAN_POINT ( 'NONE',  ( -1.364683531250014514, 12.65104166700806232, -0.7879004041258335089 ) ) ;
#164887 = CARTESIAN_POINT ( 'NONE',  ( -3.492107083971660586, 6.231819477012331632, 1.199719254218452935 ) ) ;
#164886 = CARTESIAN_POINT ( 'NONE',  ( -0.07607780150072247782, -1.417851297177070258, -1.802264747598992800 ) ) ;
#164888 = CARTESIAN_POINT ( 'NONE',  ( 3.821100691872282518, -0.1266977344972844144, 1.720184112200423332 ) ) ;
#164889 = CARTESIAN_POINT ( 'NONE',  ( -0.1399997263889611598, 6.947783040739049731, -2.595329734540325006 ) ) ;
#164890 = CARTESIAN_POINT ( 'NONE',  ( 4.546061579283848353, 4.198160018786257552, -0.7998128361456211532 ) ) ;
#164891 = CARTESIAN_POINT ( 'NONE',  ( -3.904385050611244079, 7.498940292447679568, 1.040834085586084257E-14 ) ) ;
#164892 = CARTESIAN_POINT ( 'NONE',  ( -9.905860218026552033, -6.920331743278818060, 1.138412281109779656E-15 ) ) ;
#164893 = CARTESIAN_POINT ( 'NONE',  ( 3.517450787741589036, 6.191110788085444128, -1.199719254218446718 ) ) ;
#164894 = CARTESIAN_POINT ( 'NONE',  ( 0.07516593201275456604, 0.0004601587237917924593, -2.044269526395313452 ) ) ;
#164895 = EDGE_LOOP ( 'NONE', ( #195186, #179536, #133683, #93552 ) ) ;
#164896 = CARTESIAN_POINT ( 'NONE',  ( 0.2509399751232620490, -0.4509356589572112162, -2.027996233343106081 ) ) ;
#164897 = ORIENTED_EDGE ( 'NONE', *, *, #16861, .F. ) ;
#164898 = CARTESIAN_POINT ( 'NONE',  ( 5.092358660276916638, -1.001593112396873098, 1.509162939045370466 ) ) ;
#164899 = ORIENTED_EDGE ( 'NONE', *, *, #82708, .F. ) ;
#164900 = CARTESIAN_POINT ( 'NONE',  ( 5.879395890181562834, 6.888325289080478697, -1.199719254218452047 ) ) ;
#164901 = FACE_OUTER_BOUND ( 'NONE', #170836, .T. ) ;
#164902 = CARTESIAN_POINT ( 'NONE',  ( 6.287769681992382509, 1.731225344711059266, -0.5331814487182000573 ) ) ;
#164903 = CARTESIAN_POINT ( 'NONE',  ( 7.173672674962134899, 7.541908673643526129, -0.7216878364870317197 ) ) ;
#164904 = CARTESIAN_POINT ( 'NONE',  ( -11.86239285000045918, 9.719999999999998863, -1.812080536912753059 ) ) ;
#164905 = CARTESIAN_POINT ( 'NONE',  ( 3.222796723461582413, 0.05406831605479084368, 2.190948157972896659 ) ) ;
#164907 = CARTESIAN_POINT ( 'NONE',  ( 8.052653171512838881, 11.48218023581863001, -1.199719254218446718 ) ) ;
#164906 = CARTESIAN_POINT ( 'NONE',  ( 6.478945253086064504, 1.736940705955980269, 0.6686975948369151546 ) ) ;
#164908 = CARTESIAN_POINT ( 'NONE',  ( 3.726117878570588626, 1.906711264527670258, 0.1841570787439601176 ) ) ;
#164909 = CARTESIAN_POINT ( 'NONE',  ( -6.773846765316632990, -7.473374494057232198, -6.773846765316600127 ) ) ;
#164910 = AXIS2_PLACEMENT_3D ( 'NONE', #53062, #201423, #183064 ) ;
#164911 = DIRECTION ( 'NONE',  ( 2.949029909160572061E-17, 1.000000000000000000, -8.673600428462503284E-15 ) ) ;
#164912 = CARTESIAN_POINT ( 'NONE',  ( -0.6823417656250003738, 0.2177083336747515085, -1.181850606188749264 ) ) ;
#164913 = CARTESIAN_POINT ( 'NONE',  ( 7.321039761699430493, 7.643560598178549270, -0.7216878364870257245 ) ) ;
#164915 = CARTESIAN_POINT ( 'NONE',  ( 5.243409334377605369, 0.4101777817676309223, -2.077071965933465769 ) ) ;
#164914 = CARTESIAN_POINT ( 'NONE',  ( -9.246297574839990929, 11.81043314211192019, 1.443375672974076540 ) ) ;
#164916 = CARTESIAN_POINT ( 'NONE',  ( 0.5323697292517782786, 1.110078392871534314, -1.854780036684190669 ) ) ;
#164917 = CARTESIAN_POINT ( 'NONE',  ( -6.310394152517827315, 6.326824364217716656, 0.7998128361456281477 ) ) ;
#164918 = CARTESIAN_POINT ( 'NONE',  ( 4.095444919779759552, 6.935713618788495793, 1.199719254218451159 ) ) ;
#164919 = CARTESIAN_POINT ( 'NONE',  ( 1.061231560844998034, 0.3605832424212577769, -1.789441408372116182 ) ) ;
#164920 = CARTESIAN_POINT ( 'NONE',  ( -4.711622075948912247, 5.455646162483875017, -1.199719254218446718 ) ) ;
#164921 = CARTESIAN_POINT ( 'NONE',  ( 3.592628304870106870, -0.3553021837224104584, -1.790491875447843606 ) ) ;
#164922 = CARTESIAN_POINT ( 'NONE',  ( 12.05321605296785492, 8.347302252938671785, -5.364299177381870898 ) ) ;
#164923 = CARTESIAN_POINT ( 'NONE',  ( 2.970861089138316036, -1.445268511421276214, 1.252435071843561731 ) ) ;
#164924 = ORIENTED_EDGE ( 'NONE', *, *, #183495, .T. ) ;
#164925 = CARTESIAN_POINT ( 'NONE',  ( 2.488665619784910188, 1.909654154697162598, 0.4814545106021291265 ) ) ;
#164926 = EDGE_LOOP ( 'NONE', ( #133341, #89003, #165865, #202208 ) ) ;
#164927 = CARTESIAN_POINT ( 'NONE',  ( 5.355005569747676830, 0.3749256243090701712, -1.905367961469102811 ) ) ;
#164928 = CARTESIAN_POINT ( 'NONE',  ( -7.262327558775498737, 8.501745569106741840, 1.199719254218452047 ) ) ;
#164930 = CARTESIAN_POINT ( 'NONE',  ( 5.080389167821143026, 1.047295930500062866, 1.843893106414703054 ) ) ;
#164929 = CARTESIAN_POINT ( 'NONE',  ( 5.855142236255289845, 7.924361590421551860, -1.599625672291281386 ) ) ;
#164931 = MANIFOLD_SOLID_BREP ( 'Sweep1[4]', #36059 ) ;
#164932 = CARTESIAN_POINT ( 'NONE',  ( -2.679285714285713826, -0.4970443252110337551, 0.000000000000000000 ) ) ;
#164933 = CARTESIAN_POINT ( 'NONE',  ( 2.859904825981678833, 0.6862549603197342085, -1.785085608301796523 ) ) ;
#164934 = CARTESIAN_POINT ( 'NONE',  ( 5.997902985473373860, 6.089292839903872157, -0.6134941253506603909 ) ) ;
#164935 = CARTESIAN_POINT ( 'NONE',  ( 7.334597915313080918, 9.580116872663850813, 1.040834085586084257E-14 ) ) ;
#164936 = CARTESIAN_POINT ( 'NONE',  ( 3.691562964670865199, 7.528850235416478576, -0.7998128361456362523 ) ) ;
#164937 = CARTESIAN_POINT ( 'NONE',  ( 3.809243135778153100, 1.699416117590052622, -1.078869421455890709 ) ) ;
#164938 = CARTESIAN_POINT ( 'NONE',  ( 3.469446951953614189E-15, 5.900000000000023448, 1.214306433183764966E-14 ) ) ;
#164939 = CARTESIAN_POINT ( 'NONE',  ( 4.670415550810885996, -1.190324863180821646, 1.384379922071424351 ) ) ;
#164940 = CARTESIAN_POINT ( 'NONE',  ( 0.3970419974134198338, 0.3524218036512065111, 2.039982198586967943 ) ) ;
#164941 = CARTESIAN_POINT ( 'NONE',  ( -8.676855123066022912, 10.18571440074093282, -1.082531754730543971 ) ) ;
#164942 = STYLED_ITEM ( 'NONE', ( #196864 ), #99975 ) ;
#164943 = CARTESIAN_POINT ( 'NONE',  ( -5.739830873228516595, 7.379802178037835780, 1.322642659050039970 ) ) ;
#164944 = CARTESIAN_POINT ( 'NONE',  ( 1.737499999999999378, -2.872916665710750106, -3.009438278150925683 ) ) ;
#164945 = CARTESIAN_POINT ( 'NONE',  ( 5.647288160985431738, -1.475499438119257878, -1.149758287351684949 ) ) ;
#164946 = CARTESIAN_POINT ( 'NONE',  ( 5.126954644262057492, 9.133197518281081173, 0.7998128361456462443 ) ) ;
#164947 = CARTESIAN_POINT ( 'NONE',  ( -4.141125853970233806, 6.918731698685530063, -1.199719254218452047 ) ) ;
#164948 = TOROIDAL_SURFACE ( 'NONE', #171755, 10.92000000000000348, 0.08000000000000000167 ) ;
#164949 = CARTESIAN_POINT ( 'NONE',  ( 0.6823417656249934904, 11.00520833367472839, 1.181850606188764807 ) ) ;
#164950 = CARTESIAN_POINT ( 'NONE',  ( -6.274726165026268454, 6.214935368819085149, 0.7998128361456341429 ) ) ;
#164951 = CARTESIAN_POINT ( 'NONE',  ( 2.846322183865124700, 5.408127416896231665, -1.199719254218446718 ) ) ;
#164952 = EDGE_CURVE ( 'NONE', #77536, #78316, #153996, .T. ) ;
#164953 = CARTESIAN_POINT ( 'NONE',  ( -7.095713291905736853, 9.371694488680407886, 1.599625672291269396 ) ) ;
#164954 = CARTESIAN_POINT ( 'NONE',  ( -4.055860508782465068, 7.883587693554856557, 1.040834085586084257E-14 ) ) ;
#164955 = CARTESIAN_POINT ( 'NONE',  ( 0.2685318824256071601, -0.8817220219094963340, -1.871193708407721035 ) ) ;
#164956 = CARTESIAN_POINT ( 'NONE',  ( 2.706785462534053277, 1.994624666228937526, 0.7104243659002054123 ) ) ;
#164957 = CARTESIAN_POINT ( 'NONE',  ( 8.402302512167096893, 10.82577223566020841, -1.599625672291268286 ) ) ;
#164958 = CARTESIAN_POINT ( 'NONE',  ( 0.2771623952736271268, 7.029701766580681799, 4.006269022107524336 ) ) ;
#164959 = CARTESIAN_POINT ( 'NONE',  ( 5.946161111532238586, -0.9360204806616537754, 1.846680006623670156 ) ) ;
#164960 = CARTESIAN_POINT ( 'NONE',  ( 4.540820729390463661, 6.975461451583557348, -1.175308324676842542 ) ) ;
#164961 = CARTESIAN_POINT ( 'NONE',  ( 5.016153647376201619, 7.835634441038803466, 1.082531754730558626 ) ) ;
#164963 = CARTESIAN_POINT ( 'NONE',  ( 0.000000000000000000, 0.000000000000000000, 0.000000000000000000 ) ) ;
#164962 = CARTESIAN_POINT ( 'NONE',  ( 2.665787487727776295, -3.982249430249628297, -2.473491247225932721 ) ) ;
#164964 = CARTESIAN_POINT ( 'NONE',  ( 2.748291532463055020, 0.7732563850255981253, 2.158024254592408209 ) ) ;
#164966 = CARTESIAN_POINT ( 'NONE',  ( 0.000000000000000000, 2.000000000000001776, 0.000000000000000000 ) ) ;
#164965 = CARTESIAN_POINT ( 'NONE',  ( -9.499668754385632852, -7.473374494045003757, -0.07933194154487524519 ) ) ;
#164967 = CARTESIAN_POINT ( 'NONE',  ( 2.250135261179100343, 0.8981609309555339538, -1.688322754368525747 ) ) ;
#164968 = AXIS2_PLACEMENT_3D ( 'NONE', #36307, #119770, #3781 ) ;
#164969 = ORIENTED_EDGE ( 'NONE', *, *, #80620, .T. ) ;
#164970 = CARTESIAN_POINT ( 'NONE',  ( 7.958272981097359811, 9.347368568444167636, -1.082531754730537976 ) ) ;
#164971 = CARTESIAN_POINT ( 'NONE',  ( 0.5451820649361303062, 0.1524121550021810545, 2.007518037476815564 ) ) ;
#164972 = CARTESIAN_POINT ( 'NONE',  ( 0.9362904128984714802, -1.094497954693674391, 1.627855050370475620 ) ) ;
#164973 = CARTESIAN_POINT ( 'NONE',  ( -6.194862797504346652, 7.033616388598824543, -1.131386643195183339 ) ) ;
#164974 = CARTESIAN_POINT ( 'NONE',  ( -5.852315862593199469, 9.979452273000736895, 0.7998128361456481317 ) ) ;
#164975 = CARTESIAN_POINT ( 'NONE',  ( 0.000000000000000000, -0.2843749995220433702, -3.793834371823813001 ) ) ;
#164977 = CARTESIAN_POINT ( 'NONE',  ( 2.148939158097754376, -1.419410118233652485, -1.056944606630695560 ) ) ;
#164976 = CARTESIAN_POINT ( 'NONE',  ( 3.556657146437085970, -1.843967315269653628, -0.9851420625589295543 ) ) ;
#164978 = CARTESIAN_POINT ( 'NONE',  ( 0.4499999999999851341, 4.000000000000003553, 0.8338124244295520571 ) ) ;
#164980 = CARTESIAN_POINT ( 'NONE',  ( 5.718756930148481743, -0.06150597819632765140, 2.291595365457484323 ) ) ;
#164979 = DIRECTION ( 'NONE',  ( 0.9999160831030532437, -0.01240418662285098193, -0.003736697214576322184 ) ) ;
#164981 = CARTESIAN_POINT ( 'NONE',  ( 4.927569761290923722, 0.8905454123377859466, -1.495065219958094938 ) ) ;
#164982 = EDGE_CURVE ( 'NONE', #156566, #85656, #200975, .T. ) ;
#164983 = CARTESIAN_POINT ( 'NONE',  ( 8.041957671200231417, 12.53403438304231976, 1.040834085586084257E-14 ) ) ;
#164984 = CARTESIAN_POINT ( 'NONE',  ( 4.603875680292229156, 7.528882839386387360, 1.199719254218452047 ) ) ;
#164985 = CARTESIAN_POINT ( 'NONE',  ( 3.057622914094188626, 1.488722154369751083, -0.8884403576015533766 ) ) ;
#164986 =( BOUNDED_SURFACE ( )  B_SPLINE_SURFACE ( 3, 3, ( 
 ( #56776, #140189, #206210, #157495, #208342, #109865, #77291, #13352, #207283, #189968, #93567, #144475, #194239, #143402, #159612, #41617, #43751, #59973, #191022, #125066, #12276, #91433, #112005, #145545, #42689, #9089, #29623, #27469, #141273, #107730, #209398, #210480, #211542, #79427, #174822, #63177, #45884, #161761, #110926, #26398, #62118, #11209, #178006, #173756, #176930, #25333, #10146, #95707, #58911, #175879, #75164, #28548, #61043, #78352, #108796, #94637, #92511, #158548, #76221, #142330, #126126, #192086, #127204, #193171, #44821, #160681, #128278, #180133, #84755, #31760, #167085, #48025, #150842, #166009, #18676, #34922, #97831, #2403, #15472, #129342, #195320, #100995, #98887, #130393, #1343, #46951, #163896, #80496, #212611, #81556, #199553, #16532, #181186, #197432, #113068, #50131, #146593, #198486, #64251, #17594, #133546, #196384, #147639, #114141, #131430, #213658, #65283, #66338, #116253, #49073, #179074, #115193, #30695, #33866, #96777, #32812, #162828, #14405, #164939, #82614, #148699, #67405, #268, #132484, #182241, #99944, #83677, #51198, #149767, #117320, #183318, #52260, #203812, #85822, #137793, #19742, #171334, #72762, #69544, #37062, #135652, #70607, #152958, #151901, #5598, #55457, #202746, #134609, #20796, #200613, #187580, #40286, #156176, #24008, #90110, #201675, #122693, #22929, #136721, #89044, #4533, #188654, #39207, #118386, #68482, #119455, #86892, #186514, #35994, #54398, #120538, #170265, #106395, #3476, #184374, #38145, #155101, #138861, #21851, #104218, #102075, #87958, #154032, #53322, #185442, #105298, #168142, #204876, #103144, #169203, #71679, #172419, #121610, #6685, #56531, #27215, #176679, #177752, #111746, #207031, #45629, #12031, #193981, #143158, #58660, #28292, #43503, #78103, #29367, #209152, #139938, #42437, #144230, #173505, #75977, #57597, #60791, #191840, #44564, #25079, #126950, #124813, #190775, #91182, #108543, #205965, #74914, #141022, #157242, #142080, #8836, #174573, #26149, #95462, #92264, #7756, #158309, #73843, #110679, #123755, #128027, #9901, #189717, #208095, #41369, #59722, #107481, #125881, #109623, #175628, #93321, #94386, #159357, #10955, #77029, #192907, #160426, #210224, #61862, #213414, #15221, #145288, #82360, #178828, #16276, #112814, #49871, #165758, #162573, #130145, #14147, #163639, #31507, #30440, #98630, #148450, #81311, #13092, #113888, #79172, #66083, #133287, #34674, #117063, #183061, #80241, #1090, #115997, #147387, #181985, #97581, #67152, #132226, #211293, #161511, #212353, #179883, #65036, #129086, #131193, #197181, #48818, #199294, #96525, #62918, #114934, #33617, #17343, #180931, #32554, #195058, #164690, #19, #146339, #63993, #198235, #46697, #83425, #196135, #47774, #99687, #50939, #149506, #52008, #100744, #120274, #55203, #56271, #204619, #85558, #138596, #105035, #72497, #21591, #151648, #121348, #136467, #171073, #122429, #87695, #18420, #135397, #22669, #118134, #168945, #150585, #153770, #70350, #137532, #184120, #5338, #3218, #69285, #35740, #201420, #84495, #167883, #19483, #101815, #20547, #53058, #119193, #185179, #188386, #36803, #166826, #102886, #2147, #203548, #68224, #6423, #134355, #202486, #86631, #187324, #200360, #152698, #4279, #54138, #186248, #88781, #37883, #103960, #170003, #71421, #38953, #154838 ),
 ( #26948, #174306, #106135, #206767, #172158, #159094, #11763, #127762, #209954, #61591, #173236, #94125, #208888, #42171, #142887, #124556, #160163, #10694, #23751, #40023, #90918, #58401, #158050, #7491, #190514, #25881, #141828, #77837, #57334, #89855, #9636, #60519, #44295, #207830, #75714, #155906, #108287, #91991, #41105, #189462, #76765, #73575, #176420, #139676, #107214, #205699, #143959, #59458, #123498, #24816, #125616, #126680, #156982, #8571, #74651, #140756, #110417, #191575, #175366, #43238, #192642, #109355, #28027, #93056, #114676, #111478, #13887, #197976, #145016, #47503, #29099, #32295, #163370, #16010, #211021, #180669, #30161, #96249, #62645, #162302, #177485, #46422, #112539, #128804, #113612, #194786, #178551, #79966, #149239, #146070, #17082, #212083, #814, #82095, #83159, #99432, #63721, #66882, #129879, #193718, #45361, #148188, #49605, #147127, #97311, #95183, #179617, #195862, #31237, #14945, #214190, #161232, #115729, #12819, #81042, #78893, #33350, #213153, #64783, #130925, #196918, #65817, #48557, #98361, #164426, #131964, #181720, #165485, #53882, #117877, #87454, #168690, #137282, #104780, #120016, #50672, #167626, #203301, #84238, #201165, #182796, #185992, #102633, #169757, #150325, #37626, #183867, #35482, #1892, #101559, #116798, #200104, #51755, #67951, #52805, #134096, #19227, #85305, #88528, #151391, #170827, #2961, #154589, #21344, #22418, #38701, #69032, #6167, #135149, #133026, #199025, #34415, #20294, #118943, #5090, #100487, #184923, #36546, #86380, #152448, #54948, #4026, #70096, #136211, #166562, #103706, #202230, #153521, #71165, #121101, #187068, #18151, #40851, #139415, #74406, #156731, #89602, #9394, #59205, #206517, #138344, #24562, #204361, #191325, #44049, #159914, #27779, #93877, #205448, #126431, #26705, #140506, #175118, #8321, #192394, #42991, #56017, #72236, #123248, #90668, #190266, #39768, #58149, #124307, #174061, #110169, #155653, #122171, #41924, #108035, #176179, #189211, #109104, #60274, #91745, #188137, #157798, #25633, #75466, #105873, #141578, #171898, #23496, #7235, #73312, #57083, #106958, #172983, #207585, #125361, #92807, #10448, #158851, #76521, #208642, #142632, #211842, #180428, #128573, #78650, #177237, #48317, #193480, #127510, #77590, #131720, #146891, #79721, #99180, #194537, #144777, #62409, #46184, #112298, #209706, #178314, #28850, #179376, #197724, #63480, #11521, #29923, #160986, #45124, #163125, #195621, #96006, #212911, #12578, #162060, #210786, #94938, #143714, #164183, #13649, #61350, #145838, #64544, #114428, #33106, #129634, #47256, #65573, #113370, #130688, #196678, #30997, #111234, #97072, #14707, #32045, #80801, #98133, #15769, #81854, #181476, #147936, #213952, #49364, #115483, #7786, #188688, #168430, #40324, #82909, #101289, #106429, #183605, #100228, #133837, #68770, #167371, #189747, #132768, #205994, #102358, #20026, #198771, #36281, #86116, #557, #41399, #66621, #18959, #200897, #50420, #116540, #73879, #166296, #52544, #182530, #34159, #172452, #69830, #17887, #53613, #123789, #199848, #134890, #165232, #16825, #117613, #83971, #148982, #139972, #24039, #152186, #90142, #150060, #85043, #156210, #35214, #1632, #51491, #118677, #151131, #67691, #2698, #57630, #3755, #135938, #184661, #201956, #119746, #157276, #195092, #8865 ),
 ( #141055, #210256, #62947, #159388, #161539, #158339, #144263, #95492, #126982, #129116, #192941, #191872, #175657, #79204, #44593, #107509, #13126, #145321, #74944, #58692, #211322, #174604, #110708, #190806, #92295, #45660, #60821, #61894, #29400, #207062, #93351, #128055, #9933, #26180, #124840, #194011, #42466, #108576, #173538, #25112, #28321, #27245, #91215, #76008, #142111, #208124, #59753, #125913, #43532, #109655, #10986, #176708, #77060, #143190, #209181, #94417, #160456, #12064, #78133, #111778, #177784, #182011, #47803, #15250, #113916, #212382, #46729, #199322, #81337, #112841, #114962, #33642, #83455, #68253, #147416, #196162, #100772, #16305, #99716, #165788, #213441, #178857, #31535, #48848, #17371, #65064, #149535, #18450, #1121, #30468, #131220, #50969, #64024, #180962, #96553, #67183, #82390, #133320, #130170, #117091, #97610, #163667, #179912, #197208, #162600, #32584, #98661, #164716, #148479, #47, #66111, #132254, #2177, #198261, #84527, #49904, #134386, #183091, #150616, #166854, #116026, #14176, #34703, #80269, #146367, #172193, #170035, #201448, #72531, #23782, #36832, #151678, #69316, #102915, #56301, #87729, #37917, #54167, #184148, #121382, #3248, #55235, #135426, #88813, #204652, #53091, #168975, #119224, #202517, #70380, #185208, #137566, #187355, #120305, #52037, #152727, #118163, #105070, #89888, #73608, #155939, #7525, #20576, #40057, #154871, #186280, #6454, #136496, #106166, #171108, #35772, #200389, #86660, #4308, #103991, #167916, #21621, #153801, #5374, #101846, #71453, #19513, #203583, #138628, #122463, #38985, #22701, #85590, #188421, #9669, #140785, #74684, #176450, #41137, #61627, #95217, #206799, #107247, #193748, #191607, #90949, #139707, #159127, #94155, #161267, #29130, #124585, #177517, #143993, #111511, #60553, #190545, #160194, #175394, #209985, #126713, #108317, #109389, #12853, #205730, #92024, #173268, #57366, #45394, #11796, #142919, #77870, #123528, #75745, #127793, #158082, #58432, #174338, #43269, #141857, #189493, #24848, #157016, #76798, #208919, #8600, #10728, #192673, #42202, #25916, #207864, #59488, #26980, #125645, #93085, #44327, #110449, #28062, #30196, #112576, #165524, #198013, #178588, #181753, #34452, #130962, #133064, #129914, #115764, #66922, #98397, #100524, #164461, #163405, #147162, #50708, #16047, #166599, #199062, #116834, #128837, #96285, #182835, #146106, #82131, #162337, #63754, #17115, #32328, #33387, #856, #194819, #64816, #99465, #195900, #212116, #13920, #83193, #46454, #80000, #145051, #78928, #214225, #213189, #211053, #47535, #113649, #179653, #31273, #97348, #62677, #14980, #81076, #148223, #196954, #48592, #114710, #180705, #65853, #132003, #49641, #149275, #201201, #153554, #19261, #52840, #85343, #183904, #18188, #170861, #118976, #84273, #86414, #5125, #54985, #39804, #184955, #167660, #72271, #202265, #71200, #137316, #36581, #150360, #2997, #20328, #203332, #102669, #21380, #67990, #105911, #134132, #152481, #53916, #200140, #117912, #138380, #151424, #120053, #35514, #51793, #104815, #121138, #101592, #187100, #188170, #70132, #204398, #69066, #38734, #6202, #37664, #1930, #103740, #168726, #4063, #56051, #169791, #135186, #122207, #136245, #186027, #87488, #22452, #88564, #154622, #40886, #156767, #110200, #125393, #208675, #93910 ),
 ( #8353, #209741, #90705, #193513, #60305, #61384, #77624, #74438, #127542, #58181, #45154, #23528, #143746, #141610, #173015, #44082, #171937, #140538, #123284, #106990, #206553, #27812, #59235, #9428, #25667, #155687, #92840, #189247, #26738, #24596, #126464, #176210, #124340, #190297, #41955, #174094, #108067, #91774, #109138, #158885, #157832, #89636, #75498, #7271, #76555, #73347, #139449, #205483, #57115, #207619, #11554, #192427, #191360, #159951, #43026, #175151, #142665, #10481, #66659, #162094, #63517, #14742, #78685, #129670, #31031, #212941, #149018, #128605, #111268, #80833, #65603, #115515, #64578, #13683, #132806, #79753, #593, #29955, #198810, #147973, #177271, #16864, #145869, #28886, #211877, #94970, #161017, #82944, #146924, #112335, #197758, #12612, #195655, #62442, #194572, #47289, #181510, #130719, #163157, #179410, #144810, #32078, #46217, #180462, #178347, #213983, #33139, #96041, #113404, #97105, #196710, #48351, #114462, #98166, #164214, #15801, #210817, #81887, #131753, #49396, #99219, #165269, #5934, #72005, #183646, #104547, #4857, #52581, #153281, #134928, #170592, #21111, #34192, #138118, #101326, #2735, #168464, #17924, #68806, #184697, #152222, #88294, #67725, #50456, #20062, #70936, #54716, #3793, #86151, #116575, #118709, #200933, #51528, #199883, #87217, #166332, #186839, #182570, #117653, #84008, #22178, #102396, #1671, #100267, #69867, #137046, #150099, #154355, #35250, #133876, #120865, #167407, #185762, #18999, #203072, #135976, #38471, #85080, #37394, #151164, #36318, #201991, #53649, #119781, #103469, #169531, #173833, #26480, #7003, #191102, #40622, #106725, #73080, #172752, #187903, #56853, #123027, #139181, #124083, #205211, #188978, #204127, #24327, #90435, #105634, #141354, #25410, #156503, #125145, #8092, #74181, #140274, #155419, #55780, #142411, #206293, #121937, #57918, #42770, #92590, #11290, #190046, #41698, #43831, #91515, #108877, #174901, #107808, #39533, #157574, #9167, #158632, #75242, #10229, #207368, #58988, #159691, #171662, #76304, #23258, #89370, #109947, #208419, #60053, #126208, #192170, #175956, #27552, #93648, #77370, #128354, #145625, #95785, #147720, #44900, #15548, #113146, #30776, #111008, #47031, #179152, #127282, #213737, #193253, #161842, #63256, #177013, #28630, #97913, #160760, #129418, #94717, #12354, #130471, #14485, #78433, #146673, #143484, #211620, #163972, #62198, #212688, #31837, #96855, #209481, #162903, #13430, #79506, #81635, #80574, #61122, #144555, #210564, #178086, #195401, #194322, #64330, #45964, #196462, #48104, #112085, #29704, #114216, #180215, #172388, #108511, #76995, #25049, #189685, #73807, #159323, #90078, #23976, #188621, #28259, #43467, #190740, #210189, #91151, #41337, #173470, #157205, #8802, #106364, #74881, #139901, #75942, #94352, #174537, #206997, #123722, #57565, #10919, #156141, #44528, #78069, #107445, #7725, #176647, #26113, #205932, #122658, #142043, #143122, #144195, #11994, #140988, #160393, #126915, #40253, #109586, #58628, #209114, #158276, #192872, #124781, #175591, #42404, #92225, #110646, #9866, #208058, #59685, #27181, #125845, #60752, #191802, #93287, #112779, #178791, #79136, #30404, #45596, #129050, #195025, #145252, #196100, #62881, #46658, #96491, #17308, #162541, #99651, #14111, #83386, #98592, #165720 ),
 ( #80200, #13055, #211258, #146304, #132191, #163601, #113851, #130107, #111712, #197144, #212316, #131154, #63952, #164655, #66048, #47733, #179846, #31470, #97543, #15183, #81272, #213377, #48782, #147350, #127994, #65000, #193949, #180896, #33578, #149468, #61827, #177721, #114898, #115959, #16239, #32518, #82323, #148416, #181949, #156065, #29330, #95424, #198200, #49834, #161477, #36291, #181484, #70908, #33113, #148990, #4828, #118686, #102368, #565, #52554, #184670, #16834, #54686, #99190, #137018, #165241, #66632, #203045, #168438, #20037, #132777, #86123, #152197, #82917, #198780, #50429, #183616, #2706, #116548, #182540, #87188, #34167, #68780, #100238, #166306, #53623, #3764, #17895, #69839, #83981, #18969, #21085, #150069, #135950, #169503, #200905, #1641, #201965, #51498, #35223, #153253, #119755, #67699, #133846, #199856, #117625, #101299, #167379, #85052, #185734, #151139, #134899, #37367, #103442, #157545, #42741, #170565, #106697, #75215, #23231, #187877, #71977, #9141, #88262, #22147, #186812, #26452, #41670, #188952, #208392, #89343, #39504, #171634, #155391, #6974, #104520, #73055, #138086, #74149, #92561, #172722, #120836, #139154, #55752, #154330, #57889, #90404, #205184, #107781, #121908, #56825, #105603, #204100, #38440, #58961, #122995, #5904, #40592, #173806, #141326, #142383, #24300, #156474, #174872, #8063, #25385, #91484, #140243, #206264, #124052, #190018, #207339, #125116, #191074, #108846, #158601, #76275, #10200, #12326, #93621, #192141, #114188, #80546, #63227, #146643, #43805, #210536, #212658, #78406, #64300, #196433, #129390, #109918, #147691, #175929, #62170, #95758, #27522, #159663, #180187, #61096, #161811, #11264, #77342, #130445, #179123, #143454, #162875, #15521, #112056, #31809, #110978, #96826, #48077, #79477, #81607, #145595, #144527, #128329, #97885, #211591, #60026, #163946, #126177, #209452, #127255, #193226, #44873, #195369, #176984, #28602, #94691, #13401, #14455, #160732, #194292, #45937, #178056, #29674, #47001, #113117, #30745, #181234, #115244, #65332, #119507, #134659, #67454, #86944, #182292, #66389, #50181, #33919, #116302, #197483, #166060, #164992, #167136, #185493, #199605, #213709, #99994, #148749, #32862, #150894, #183370, #17647, #200662, #319, #83731, #132537, #16583, #131479, #151953, #149823, #49126, #133600, #52311, #36045, #20845, #1393, #198535, #53372, #34975, #118441, #184428, #51248, #98938, #117373, #101046, #102125, #18721, #168194, #84805, #2455, #169259, #82665, #68531, #19793, #85876, #37118, #3523, #69597, #135705, #201731, #103197, #6736, #74964, #54449, #7808, #153011, #42487, #4587, #120592, #190828, #90165, #73901, #186569, #24062, #139994, #189771, #174624, #187633, #88013, #207082, #122747, #206015, #57651, #121666, #70661, #137846, #155155, #123810, #39260, #41422, #105354, #188709, #108596, #136771, #171391, #38197, #202800, #58713, #173561, #156231, #25133, #104270, #170315, #72815, #141074, #21903, #107530, #154084, #26200, #5652, #71732, #203867, #91235, #157295, #55511, #8885, #124862, #22982, #89101, #138917, #204936, #40345, #56587, #106451, #172475, #93372, #194032, #43553, #125933, #178877, #211343, #191891, #195113, #47823, #144283, #146387, #143212, #129137, #80289, #111799, #113934, #177805, #176730, #160478, #64043, #29421, #179930 ),
 ( #46750, #14196, #142131, #78152, #112862, #209202, #159408, #109674, #30489, #59774, #208145, #158359, #212401, #13148, #12085, #92318, #60842, #11008, #127004, #192962, #44615, #76028, #110730, #175676, #45683, #130188, #210276, #9952, #28344, #27265, #77085, #95512, #61916, #94439, #79225, #128076, #161560, #145342, #62968, #96573, #162620, #196181, #31554, #99734, #119244, #85611, #151699, #81355, #197226, #135446, #98678, #34720, #114982, #16325, #184170, #199342, #68273, #167934, #147435, #17390, #200409, #148497, #164734, #48866, #134405, #213459, #65083, #97629, #3268, #166875, #165806, #163686, #65, #82408, #66129, #132273, #198281, #15268, #49922, #180982, #50989, #69335, #83473, #131238, #116043, #32603, #182031, #183112, #1139, #33660, #18467, #149554, #67201, #133338, #117110, #100791, #35790, #84545, #150635, #2196, #52055, #118182, #53111, #101866, #19534, #201468, #154893, #23801, #172212, #153823, #36851, #170055, #187374, #89906, #5394, #155958, #71472, #6474, #140806, #102935, #137585, #4329, #168995, #24867, #205751, #188441, #57382, #20594, #70398, #39005, #107265, #86680, #40075, #185228, #74702, #152747, #136516, #8620, #122480, #106187, #202535, #56320, #7544, #54184, #58452, #120324, #105089, #72551, #186300, #37936, #90971, #104010, #138649, #21640, #87747, #123546, #73629, #203602, #139728, #206818, #22721, #157033, #55255, #189511, #173285, #204671, #121402, #41156, #171127, #88835, #96303, #61648, #192693, #605, #93105, #191626, #175415, #159147, #26999, #108338, #76819, #75767, #77892, #162359, #110469, #124607, #10748, #59507, #25936, #127815, #94176, #142939, #45416, #125664, #208939, #43289, #141875, #190565, #62698, #60574, #42221, #44347, #111532, #161288, #146124, #126733, #109410, #178609, #160215, #177539, #29150, #176470, #174358, #28080, #11816, #95239, #144013, #12874, #210006, #193770, #80021, #92044, #78950, #158101, #9690, #30219, #145072, #211075, #128859, #207884, #194841, #46474, #112597, #13938, #135989, #66670, #170605, #132819, #34204, #104561, #3805, #202004, #100278, #152234, #69879, #116587, #154370, #182582, #68817, #102409, #166344, #17935, #186852, #67737, #168476, #84020, #150111, #153293, #185775, #1683, #169545, #22192, #118721, #120878, #117665, #103482, #54728, #86163, #88306, #53662, #151176, #134939, #38484, #119795, #198822, #50468, #133887, #199894, #51540, #183657, #35262, #37408, #101338, #167420, #4870, #20074, #21124, #203083, #19011, #52594, #87230, #85092, #2747, #200945, #70948, #184708, #36330, #137059, #126220, #141367, #91528, #90448, #74194, #192181, #157587, #93661, #60064, #43844, #55793, #171675, #109959, #73093, #9182, #89383, #205224, #158642, #173846, #42781, #142421, #121949, #206307, #174912, #123040, #139193, #23271, #108890, #187915, #39546, #72017, #175969, #207379, #140287, #5947, #188992, #56865, #40634, #106737, #172765, #204139, #24339, #155431, #25422, #27563, #57931, #138130, #156515, #7017, #105647, #75253, #190059, #8105, #59000, #124095, #41711, #107821, #125156, #191115, #10240, #26493, #92600, #76315, #208430, #196474, #181273, #194333, #94728, #213747, #129429, #212700, #146684, #128366, #11302, #144565, #161853, #64341, #45975, #130486, #112096, #195413, #115281, #77380, #178098, #193265, #143496, #65370, #180226, #162915 ),
 ( #159702, #63268, #114228, #163983, #113159, #47042, #209492, #13442, #29715, #160774, #12367, #48116, #61133, #81645, #32899, #78447, #127294, #131517, #211632, #111019, #44911, #179163, #31848, #177024, #49164, #210577, #197520, #15558, #28641, #97925, #62209, #147732, #95797, #30787, #79518, #145637, #96866, #14496, #80588, #54484, #184464, #183408, #167172, #70695, #36082, #186605, #153049, #4624, #148784, #50220, #202835, #166096, #102165, #182330, #83770, #37158, #52352, #135744, #20880, #354, #84844, #53407, #1431, #17684, #116339, #201767, #66427, #132570, #165030, #136809, #19831, #18759, #98977, #67496, #149863, #133640, #199641, #51287, #82705, #117412, #33958, #118479, #120629, #150933, #16623, #35012, #100034, #198571, #168233, #68569, #101083, #85915, #2495, #134696, #200700, #151989, #3563, #103235, #69636, #119545, #185530, #169295, #86979, #59812, #72847, #187668, #92351, #7846, #91273, #25172, #6771, #104307, #23019, #40382, #157330, #138952, #8922, #204973, #73933, #208180, #170355, #56619, #71768, #21940, #158389, #58748, #41457, #124901, #88050, #137884, #106485, #174658, #154121, #107565, #38232, #142163, #5691, #203904, #76064, #189805, #173600, #55550, #123844, #75003, #121704, #125967, #39298, #172512, #140027, #105391, #171431, #9986, #89136, #206052, #155190, #122783, #190864, #141112, #188743, #207123, #24098, #57687, #90201, #156265, #42527, #108632, #26234, #31592, #212441, #195154, #64083, #109705, #11042, #45721, #113973, #93407, #46788, #191923, #81393, #43588, #159444, #15305, #129177, #112902, #77121, #63007, #178913, #27300, #65120, #143244, #194068, #13187, #209233, #60878, #97667, #192997, #79265, #127037, #44650, #130226, #96608, #110764, #80326, #147478, #29457, #163725, #28379, #14231, #179970, #211380, #213498, #30528, #61951, #111840, #175710, #162662, #176763, #94473, #160514, #12117, #78191, #144317, #210315, #146427, #128110, #177844, #196220, #145382, #47862, #95546, #161598, #117151, #85651, #33701, #198320, #82445, #167973, #98718, #32641, #197264, #36894, #52094, #199382, #4369, #99778, #49960, #182069, #165843, #17429, #115024, #83512, #148535, #84589, #102976, #183154, #131276, #149595, #66168, #164777, #68314, #100831, #1179, #118221, #132315, #67243, #116079, #102, #48904, #69378, #133377, #181021, #51029, #184207, #19579, #152789, #34757, #166916, #185271, #18510, #35830, #101908, #150676, #16367, #2237, #134445, #200448, #151738, #3308, #135486, #201508, #53156, #119285, #169034, #20631, #86720, #189548, #42261, #158138, #25975, #92081, #203642, #124646, #24905, #72590, #173327, #154929, #190603, #41196, #54228, #70439, #71513, #107303, #139767, #8662, #206858, #108374, #91011, #174397, #87791, #136555, #188484, #157073, #74742, #23838, #40114, #202576, #138691, #6514, #137625, #5434, #140846, #186341, #58490, #120366, #55293, #37976, #104049, #122521, #21681, #170095, #89946, #153865, #121443, #187412, #39043, #105128, #171168, #22758, #205793, #88875, #204708, #106225, #56358, #172251, #57423, #155996, #7583, #73668, #123585, #77933, #59546, #62741, #193807, #46519, #27037, #211117, #60615, #126774, #93146, #192732, #207924, #76859, #142978, #159183, #144054, #10784, #208978, #44387, #179716, #110508, #47598, #176508, #31333, #112641, #113712, #129976, #28120 ) ),
 .UNSPECIFIED., .T., .F., .T. ) 
 B_SPLINE_SURFACE_WITH_KNOTS ( ( 4, 3, 4 ),
 ( 4, 1, 1, 1, 1, 1, 1, 1, 1, 1, 1, 1, 1, 1, 1, 1, 1, 1, 1, 1, 1, 1, 1, 1, 1, 1, 1, 1, 1, 1, 1, 1, 1, 1, 1, 1, 1, 1, 1, 1, 1, 1, 1, 1, 1, 1, 1, 1, 1, 1, 1, 1, 1, 1, 1, 1, 1, 1, 1, 1, 1, 1, 1, 1, 1, 1, 1, 1, 1, 1, 1, 1, 1, 1, 1, 1, 1, 1, 1, 1, 1, 1, 1, 1, 1, 1, 1, 1, 1, 1, 1, 1, 1, 1, 1, 1, 1, 1, 1, 1, 1, 1, 1, 1, 1, 1, 1, 1, 1, 1, 1, 1, 1, 1, 1, 1, 1, 1, 1, 1, 1, 1, 1, 1, 1, 1, 1, 1, 1, 1, 1, 1, 1, 1, 1, 1, 1, 1, 1, 1, 1, 1, 1, 1, 1, 1, 1, 1, 1, 1, 1, 1, 1, 1, 1, 1, 1, 1, 1, 1, 1, 1, 1, 1, 1, 1, 1, 1, 1, 1, 1, 1, 1, 1, 1, 1, 1, 1, 1, 1, 1, 1, 1, 1, 1, 1, 1, 1, 1, 1, 1, 1, 1, 1, 1, 1, 1, 1, 1, 1, 1, 1, 1, 1, 1, 1, 1, 1, 1, 1, 1, 1, 1, 1, 1, 1, 1, 1, 1, 1, 1, 1, 1, 1, 1, 1, 1, 1, 1, 1, 1, 1, 1, 1, 1, 1, 1, 1, 1, 1, 1, 1, 1, 1, 1, 1, 1, 1, 1, 1, 1, 1, 1, 1, 1, 1, 1, 1, 1, 1, 1, 1, 1, 1, 1, 1, 1, 1, 1, 1, 1, 1, 1, 1, 1, 1, 1, 1, 1, 1, 1, 1, 1, 1, 1, 1, 1, 1, 1, 1, 1, 1, 1, 1, 1, 1, 1, 1, 1, 1, 1, 1, 1, 1, 1, 1, 1, 1, 1, 1, 1, 1, 1, 1, 1, 1, 1, 1, 1, 1, 1, 1, 1, 1, 1, 1, 1, 1, 1, 1, 1, 1, 1, 1, 1, 1, 1, 1, 1, 1, 1, 1, 1, 1, 1, 1, 1, 1, 1, 1, 1, 1, 1, 1, 1, 1, 1, 1, 1, 1, 1, 1, 1, 1, 1, 1, 1, 1, 1, 1, 1, 1, 1, 1, 1, 1, 1, 1, 1, 1, 1, 1, 1, 1, 4 ),
 ( 0.000000000000000000, 0.5000000000000000000, 1.000000000000000000 ),
 ( 0.000000000000000000, 0.002600214693118923798, 0.005208871813129847643, 0.007813341859462101871, 0.01041561011214237054, 0.01302159838915000617, 0.01562452542669844589, 0.01822945805747129902, 0.02083332260852943998, 0.02343713088342555886, 0.02604210653276634729, 0.02864513693292065552, 0.03125071383394792401, 0.03385356881896259273, 0.03645895053148855841, 0.03906228851054763251, 0.04166670673482164577, 0.04427111720854654681, 0.04687446234244373178, 0.04947983976256019323, 0.05208269766733494843, 0.05468827385445936690, 0.05729129101459448647, 0.05989628262864687969, 0.06250008845252298662, 0.06510390268380349121, 0.06770888856031336001, 0.07031191025079500112, 0.07291748459129859805, 0.07552033970978830335, 0.07812571920045624507, 0.08072905536012038585, 0.08333347174482363950, 0.08593788071299547637, 0.08854122383090638759, 0.09114659965375219997, 0.09374945576594469199, 0.09635503022752239799, 0.09895804583665256116, 0.1015630356028039000, 0.1041668400134527495, 0.1067706523020897913, 0.1093756367037285043, 0.1119786565701353653, 0.1145842293264338063, 0.1171870828570002881, 0.1197924606432616973, 0.1223957954228293843, 0.1250002099740243899, 0.1276046175975352470, 0.1302079588893767237, 0.1328133332639841735, 0.1354161877457908392, 0.1380217606440506395, 0.1406247748629219918, 0.1432297629411592166, 0.1458335661004374617, 0.1484373766077259071, 0.1510423596945167368, 0.1536453778991425101, 0.1562509492307036785, 0.1588538013357113088, 0.1614591775772540871, 0.1640625111385781432, 0.1666669240170048083, 0.1692713304565471311, 0.1718746700842041231, 0.1744800431702197008, 0.1770828961840006377, 0.1796884676783837009, 0.1822914806691622869, 0.1848964672195632097, 0.1875002692887918765, 0.1901040781760970355, 0.1927090601080766463, 0.1953120768130981733, 0.1979176468793322763, 0.2005204977210985895, 0.2031258725775486607, 0.2057292050824250096, 0.2083336164487647746, 0.2109380218649763994, 0.2135413599902747928, 0.2161467319472901716, 0.2187495836553486062, 0.2213551539052408534, 0.2239581658300387468, 0.2265631510126252801, 0.2291669521530730058, 0.2317707595817034838, 0.2343757405188569010, 0.2369787558863956922, 0.2395843248466610342, 0.2421871745874512594, 0.2447925482183819501, 0.2473958798285567084, 0.2500002898434375842, 0.2526046943969075254, 0.2552080311816201097, 0.2578134021691782518, 0.2604162527337665622, 0.2630218218985046486, 0.2656248329193858781, 0.2682298168941298910, 0.2708336172670197106, 0.2734374233982336255, 0.2760424035005001331, 0.2786454176926287940, 0.2812509857062375773, 0.2838538345082703418, 0.2864592070732082663, 0.2890625379503836689, 0.2916669467743862043, 0.2942713506256608436, 0.2968746862315132518, 0.2994800564091141259, 0.3020829059924399762, 0.3046884742313171190, 0.3072914845103039694, 0.3098964674371332273, 0.3125002672036480411, 0.3151040721986592130, 0.3177090516259382103, 0.3203120648046862140, 0.3229176320309106729, 0.3255204800563645251, 0.3281258517147956355, 0.3307291820206363919, 0.3333335898142997245, 0.3359379931238887229, 0.3385413277125659537, 0.3411466972396727249, 0.3437495460039050044, 0.3463551134761772565, 0.3489581231752558743, 0.3515631052140602009, 0.3541669045353489920, 0.3567707085553323276, 0.3593756874674896018, 0.3619786997948497009, 0.3645842663929277916, 0.3671871138039469185, 0.3697924847153226668, 0.3723958146114617063, 0.3750002215352895019, 0.3776046244636719340, 0.3802079581968237365, 0.3828133272328684833, 0.3854161753401436075, 0.3880217422050354359, 0.3906247514861621029, 0.3932297327967993472, 0.3958335318339832876, 0.3984373350400814418, 0.4010423135969549691, 0.4036453252348887744, 0.4062508913640303643, 0.4088537383227308641, 0.4114591086464738368, 0.4140624382945181647, 0.4166668445089845574, 0.4192712472166146842, 0.4218745802558619973, 0.4244799489602520959, 0.4270827965726798348, 0.4296883629893904488, 0.4322913720144979099, 0.4348963527567997200, 0.4375001516709778882, 0.4401039542243071478, 0.4427089325857130886, 0.4453119436961573974, 0.4479175095155500941, 0.4505203561840259718, 0.4531257260795358843, 0.4557290556410732441, 0.4583334613066292196, 0.4609378639539425948, 0.4635411964608836533, 0.4661465649930071620, 0.4687494122726767465, 0.4713549784003855381, 0.4739579873313886638, 0.4765629676651664814, 0.4791667666174222462, 0.4817705686790782482, 0.4843755470048167200, 0.4869785577496898998, 0.4895841234185048796, 0.4921869699588339309, 0.4947923395854939010, 0.4973956692220981579, 0.5000000744991768276, 0.5026044772465965149, 0.5052078093828125116, 0.5078131779020444991, 0.5104160250110306718, 0.5130215910089035436, 0.5156246000077054914, 0.5182295800927568807, 0.5208333792441637300, 0.5234371809752277338, 0.5260421594250891397, 0.5286451699662961801, 0.5312507356436946271, 0.5338535822179446555, 0.5364589517351265879, 0.5390622816083643354, 0.5416666866573878192, 0.5442710896653298880, 0.5468744215923915242, 0.5494797902580997873, 0.5520826373584690749, 0.5546882033856646022, 0.5572912126141627009, 0.5598961926102767883, 0.5624999921219043797, 0.5651037936834493181, 0.5677087724172201755, 0.5703117829166597375, 0.5729173487617980065, 0.5755201955320329299, 0.5781255650991041772, 0.5807288953705399548, 0.5833333003519244331, 0.5859377037808047861, 0.5885410356602774895, 0.5911464046318289922, 0.5937492518856454238, 0.5963548181013198501, 0.5989578277214122615, 0.6015628077883760083, 0.6041666078212959423, 0.6067704093743923055, 0.6093753885518610192, 0.6119783991714310423, 0.6145839653434672645, 0.6171868124717531101, 0.6197921822480817466, 0.6223955130792849788, 0.6249999181534476866, 0.6276043221636865566, 0.6302076541571374202, 0.6328130235939036785, 0.6354158711632348355, 0.6380214377265494008, 0.6406244479001403924, 0.6432294281977445349, 0.6458332289130368498, 0.6484370306187589028, 0.6510420103997216490, 0.6536450213013255128, 0.6562505879594253688, 0.6588534356078361576, 0.6614588057527972520, 0.6640621373053481324, 0.6666665426327121891, 0.6692709473847417989, 0.6718742796537453543, 0.6744796497151083203, 0.6770824977620315543, 0.6796880648321572682, 0.6822910757211636534, 0.6848960564092084757, 0.6874998579679674204, 0.6901036599873985322, 0.6927086405316660311, 0.6953116518772185506, 0.6979172191805607106, 0.7005200675111846742, 0.7031254381841663958, 0.7057287706196612165, 0.7083331763606625087, 0.7109375820149322900, 0.7135409147210758363, 0.7161462855664346705, 0.7187491342530435423, 0.7213547019891674017, 0.7239577137555243125, 0.7265626949938263079, 0.7291664975571658935, 0.7317703000514055311, 0.7343752815188082650, 0.7369782934702413524, 0.7395838615780243597, 0.7421867107529701579, 0.7447920821133793279, 0.7473954155934371402, 0.7499998219085300954, 0.7526042286255122393, 0.7552075619304030596, 0.7578129337191791270, 0.7604157832075884027, 0.7630213517689198310, 0.7656243645745874904, 0.7682293465229839136, 0.7708331502520449074, 0.7734369533822141873, 0.7760419359326080624, 0.7786449486518774998, 0.7812505177233250997, 0.7838533679047272607, 0.7864587401119955690, 0.7890620747982641792, 0.7916664818479275390, 0.7942708897881238794, 0.7968742238533942368, 0.7994795967450375462, 0.8020824471973901915, 0.8046880167431663677, 0.8072910307501349747, 0.8098960135684915018, 0.8124998186244467568, 0.8151036225516941069, 0.8177086063449673370, 0.8203116199940584385, 0.8229171901884252405, 0.8255200415384508217, 0.8281254147520410447, 0.8307287508062024539, 0.8333331587509454907, 0.8359375680748931670, 0.8385409030622068549, 0.8411462772162020540, 0.8437491287946751184, 0.8463546994841673055, 0.8489577148544642515, 0.8515626987026798655, 0.8541665052467400931, 0.8567703101322480252, 0.8593752953283267937, 0.8619783100692604005, 0.8645838815458386506, 0.8671867342266933454, 0.8697921086061042306, 0.8723954461898817403, 0.8749998551902504751, 0.8776042660585271493, 0.8802076021295854868, 0.8828129777054576355, 0.8854158305722678035, 0.8880214025647872322, 0.8906244194604823194, 0.8932294044984951942, 0.8958332126919159588, 0.8984370186969063976, 0.9010420054557602976, 0.9036450214505988843, 0.9062505943687239052, 0.9088534485426573717, 0.9114588242474312985, 0.9140621635225948394, 0.9166665737391771485, 0.9192709863124074454, 0.9218743236289563825, 0.9244797007862803895, 0.9270825551036790957, 0.9296881285585824051, 0.9322911471418501295, 0.9348961335295734587, 0.9374999435335269471, 0.9401037508197458425, 0.9427087393012421046, 0.9453117567106092967, 0.9479173312323898593, 0.9505201870615167525, 0.9531255642405720430, 0.9557289053967781278, 0.9583333169903581750, 0.9609377312744702415, 0.9635410702737328137, 0.9661464495301401723, 0.9687493035862174695, 0.9713548794777306927, 0.9739579066090123804, 0.9765628826531806972, 0.9791666865793459129, 0.9817705523293528413, 0.9843754818126480011, 0.9869784094881522973, 0.9895843956701340094, 0.9921866610829068733, 0.9947911313000845634, 0.9973997837621362272, 1.000000000000000000 ),
 .UNSPECIFIED. ) 
 GEOMETRIC_REPRESENTATION_ITEM ( )  RATIONAL_B_SPLINE_SURFACE ( (
 ( 1.000000000000000222, 1.000000000000000222, 1.000000000000000000, 1.000000000000000222, 1.000000000000000000, 0.9999999999999997780, 1.000000000000000222, 1.000000000000000000, 1.000000000000000222, 1.000000000000000222, 1.000000000000000000, 0.9999999999999997780, 1.000000000000000000, 1.000000000000000222, 0.9999999999999997780, 1.000000000000000222, 0.9999999999999994449, 1.000000000000000444, 0.9999999999999996669, 1.000000000000000000, 1.000000000000000222, 1.000000000000000000, 1.000000000000000000, 0.9999999999999997780, 1.000000000000000444, 0.9999999999999996669, 1.000000000000000000, 1.000000000000000222, 0.9999999999999997780, 1.000000000000000000, 0.9999999999999997780, 0.9999999999999997780, 1.000000000000000444, 0.9999999999999994449, 1.000000000000000444, 0.9999999999999997780, 0.9999999999999997780, 0.9999999999999996669, 1.000000000000000222, 1.000000000000000000, 0.9999999999999997780, 1.000000000000000222, 0.9999999999999997780, 1.000000000000000222, 1.000000000000000000, 1.000000000000000222, 1.000000000000000000, 1.000000000000000000, 1.000000000000000444, 0.9999999999999996669, 0.9999999999999997780, 1.000000000000000000, 0.9999999999999997780, 0.9999999999999997780, 1.000000000000000000, 1.000000000000000000, 0.9999999999999997780, 1.000000000000000444, 1.000000000000000000, 0.9999999999999997780, 1.000000000000000222, 0.9999999999999996669, 1.000000000000000222, 1.000000000000000000, 0.9999999999999997780, 1.000000000000000222, 0.9999999999999997780, 1.000000000000000000, 0.9999999999999997780, 1.000000000000000222, 0.9999999999999996669, 1.000000000000000000, 1.000000000000000222, 0.9999999999999997780, 1.000000000000000222, 0.9999999999999996669, 1.000000000000000444, 1.000000000000000000, 1.000000000000000000, 1.000000000000000222, 1.000000000000000222, 1.000000000000000000, 0.9999999999999997780, 1.000000000000000222, 0.9999999999999997780, 1.000000000000000000, 1.000000000000000000, 1.000000000000000000, 0.9999999999999997780, 1.000000000000000000, 0.9999999999999997780, 1.000000000000000222, 0.9999999999999997780, 1.000000000000000000, 1.000000000000000222, 0.9999999999999997780, 1.000000000000000000, 0.9999999999999996669, 1.000000000000000444, 0.9999999999999997780, 1.000000000000000000, 1.000000000000000000, 1.000000000000000000, 0.9999999999999997780, 0.9999999999999997780, 1.000000000000000222, 1.000000000000000222, 0.9999999999999997780, 1.000000000000000000, 1.000000000000000000, 1.000000000000000222, 1.000000000000000222, 1.000000000000000000, 0.9999999999999997780, 1.000000000000000222, 1.000000000000000000, 1.000000000000000000, 0.9999999999999997780, 0.9999999999999997780, 1.000000000000000222, 1.000000000000000000, 1.000000000000000000, 1.000000000000000000, 0.9999999999999997780, 1.000000000000000222, 1.000000000000000000, 1.000000000000000000, 1.000000000000000000, 1.000000000000000444, 0.9999999999999997780, 0.9999999999999997780, 1.000000000000000000, 1.000000000000000000, 0.9999999999999997780, 1.000000000000000222, 0.9999999999999997780, 1.000000000000000222, 1.000000000000000000, 1.000000000000000222, 1.000000000000000222, 1.000000000000000000, 1.000000000000000222, 1.000000000000000000, 0.9999999999999996669, 1.000000000000000222, 0.9999999999999997780, 1.000000000000000444, 0.9999999999999997780, 1.000000000000000000, 0.9999999999999997780, 1.000000000000000222, 1.000000000000000000, 0.9999999999999997780, 1.000000000000000222, 0.9999999999999994449, 1.000000000000000000, 1.000000000000000222, 1.000000000000000222, 0.9999999999999997780, 1.000000000000000444, 0.9999999999999997780, 1.000000000000000222, 0.9999999999999997780, 1.000000000000000222, 0.9999999999999997780, 1.000000000000000000, 1.000000000000000000, 1.000000000000000222, 0.9999999999999997780, 0.9999999999999996669, 1.000000000000000444, 0.9999999999999997780, 1.000000000000000222, 1.000000000000000000, 1.000000000000000222, 0.9999999999999994449, 1.000000000000000444, 0.9999999999999997780, 1.000000000000000000, 1.000000000000000222, 1.000000000000000000, 1.000000000000000000, 0.9999999999999997780, 1.000000000000000444, 0.9999999999999997780, 1.000000000000000444, 0.9999999999999997780, 1.000000000000000000, 1.000000000000000222, 0.9999999999999996669, 1.000000000000000222, 1.000000000000000000, 1.000000000000000000, 0.9999999999999996669, 1.000000000000000222, 1.000000000000000444, 0.9999999999999997780, 1.000000000000000222, 0.9999999999999996669, 1.000000000000000444, 0.9999999999999997780, 1.000000000000000444, 0.9999999999999996669, 0.9999999999999997780, 1.000000000000000000, 0.9999999999999997780, 1.000000000000000000, 1.000000000000000000, 1.000000000000000000, 1.000000000000000000, 0.9999999999999997780, 1.000000000000000000, 0.9999999999999997780, 1.000000000000000000, 1.000000000000000000, 1.000000000000000000, 1.000000000000000000, 0.9999999999999997780, 1.000000000000000222, 0.9999999999999997780, 1.000000000000000222, 0.9999999999999997780, 1.000000000000000222, 0.9999999999999994449, 1.000000000000000444, 1.000000000000000000, 1.000000000000000222, 0.9999999999999997780, 1.000000000000000000, 0.9999999999999997780, 1.000000000000000222, 1.000000000000000000, 1.000000000000000000, 1.000000000000000222, 1.000000000000000222, 0.9999999999999996669, 1.000000000000000444, 0.9999999999999996669, 1.000000000000000444, 0.9999999999999996669, 1.000000000000000000, 1.000000000000000000, 1.000000000000000000, 0.9999999999999997780, 1.000000000000000222, 0.9999999999999997780, 1.000000000000000222, 1.000000000000000000, 0.9999999999999997780, 1.000000000000000000, 1.000000000000000222, 1.000000000000000222, 1.000000000000000000, 1.000000000000000000, 1.000000000000000000, 1.000000000000000000, 0.9999999999999997780, 1.000000000000000444, 1.000000000000000000, 0.9999999999999997780, 1.000000000000000222, 0.9999999999999996669, 1.000000000000000444, 1.000000000000000000, 1.000000000000000222, 1.000000000000000222, 0.9999999999999997780, 1.000000000000000222, 0.9999999999999997780, 1.000000000000000000, 1.000000000000000000, 0.9999999999999997780, 1.000000000000000000, 1.000000000000000000, 0.9999999999999997780, 1.000000000000000222, 1.000000000000000000, 1.000000000000000000, 1.000000000000000222, 1.000000000000000000, 1.000000000000000000, 1.000000000000000000, 1.000000000000000222, 0.9999999999999997780, 1.000000000000000222, 1.000000000000000000, 0.9999999999999997780, 1.000000000000000222, 0.9999999999999997780, 1.000000000000000222, 1.000000000000000222, 1.000000000000000000, 0.9999999999999997780, 1.000000000000000000, 1.000000000000000222, 1.000000000000000000, 1.000000000000000000, 0.9999999999999996669, 1.000000000000000444, 0.9999999999999994449, 1.000000000000000444, 0.9999999999999997780, 1.000000000000000000, 1.000000000000000000, 0.9999999999999997780, 1.000000000000000222, 0.9999999999999997780, 1.000000000000000000, 1.000000000000000444, 0.9999999999999997780, 1.000000000000000000, 0.9999999999999997780, 1.000000000000000000, 1.000000000000000000, 0.9999999999999997780, 0.9999999999999997780, 1.000000000000000000, 1.000000000000000444, 1.000000000000000000, 1.000000000000000444, 1.000000000000000000, 1.000000000000000000, 1.000000000000000000, 0.9999999999999997780, 1.000000000000000000, 1.000000000000000000, 1.000000000000000000, 1.000000000000000000, 0.9999999999999997780, 1.000000000000000222, 1.000000000000000000, 0.9999999999999997780, 1.000000000000000444, 0.9999999999999997780, 1.000000000000000222, 0.9999999999999996669, 1.000000000000000444, 1.000000000000000000, 0.9999999999999997780, 1.000000000000000000, 1.000000000000000000, 1.000000000000000000, 0.9999999999999997780, 1.000000000000000000, 1.000000000000000000, 0.9999999999999997780, 1.000000000000000444, 0.9999999999999997780, 0.9999999999999997780, 1.000000000000000000, 1.000000000000000000, 1.000000000000000222, 1.000000000000000222, 0.9999999999999997780, 1.000000000000000000, 1.000000000000000222, 1.000000000000000000, 0.9999999999999997780, 1.000000000000000222, 1.000000000000000000, 1.000000000000000000, 1.000000000000000000, 0.9999999999999997780, 1.000000000000000000, 1.000000000000000000, 1.000000000000000000, 1.000000000000000000, 0.9999999999999997780, 1.000000000000000666, 0.9999999999999996669, 0.9999999999999996669, 1.000000000000000444, 0.9999999999999996669, 1.000000000000000222, 1.000000000000000000, 1.000000000000000000, 1.000000000000000000, 1.000000000000000000, 1.000000000000000000, 0.9999999999999997780, 1.000000000000000222, 1.000000000000000222, 0.9999999999999996669, 0.9999999999999997780, 1.000000000000000000, 1.000000000000000222, 1.000000000000000222),
 ( 0.3333333333333334259, 0.3333333333333334259, 0.3333333333333333703, 0.3333333333333334259, 0.3333333333333333703, 0.3333333333333332593, 0.3333333333333334814, 0.3333333333333333703, 0.3333333333333334814, 0.3333333333333334259, 0.3333333333333333148, 0.3333333333333333148, 0.3333333333333333703, 0.3333333333333334259, 0.3333333333333332593, 0.3333333333333334814, 0.3333333333333331483, 0.3333333333333334814, 0.3333333333333333148, 0.3333333333333333148, 0.3333333333333334259, 0.3333333333333333703, 0.3333333333333333703, 0.3333333333333333148, 0.3333333333333335369, 0.3333333333333332593, 0.3333333333333333703, 0.3333333333333333703, 0.3333333333333334259, 0.3333333333333333148, 0.3333333333333333148, 0.3333333333333333148, 0.3333333333333334259, 0.3333333333333332593, 0.3333333333333334259, 0.3333333333333334259, 0.3333333333333333148, 0.3333333333333332593, 0.3333333333333333703, 0.3333333333333333703, 0.3333333333333332593, 0.3333333333333334814, 0.3333333333333333703, 0.3333333333333333703, 0.3333333333333333148, 0.3333333333333334259, 0.3333333333333333703, 0.3333333333333333703, 0.3333333333333334814, 0.3333333333333332038, 0.3333333333333334259, 0.3333333333333333703, 0.3333333333333333148, 0.3333333333333333148, 0.3333333333333333703, 0.3333333333333333703, 0.3333333333333333148, 0.3333333333333334814, 0.3333333333333333148, 0.3333333333333333703, 0.3333333333333333148, 0.3333333333333333148, 0.3333333333333334259, 0.3333333333333333703, 0.3333333333333333703, 0.3333333333333334259, 0.3333333333333333148, 0.3333333333333333148, 0.3333333333333333703, 0.3333333333333333703, 0.3333333333333332593, 0.3333333333333333703, 0.3333333333333333703, 0.3333333333333333703, 0.3333333333333333148, 0.3333333333333333148, 0.3333333333333334814, 0.3333333333333333703, 0.3333333333333334259, 0.3333333333333334259, 0.3333333333333334814, 0.3333333333333333148, 0.3333333333333333703, 0.3333333333333334259, 0.3333333333333333148, 0.3333333333333333703, 0.3333333333333333703, 0.3333333333333333703, 0.3333333333333333703, 0.3333333333333333703, 0.3333333333333333148, 0.3333333333333334814, 0.3333333333333332593, 0.3333333333333334259, 0.3333333333333333703, 0.3333333333333333703, 0.3333333333333333148, 0.3333333333333333703, 0.3333333333333334259, 0.3333333333333332593, 0.3333333333333334259, 0.3333333333333333703, 0.3333333333333333148, 0.3333333333333333148, 0.3333333333333332593, 0.3333333333333334259, 0.3333333333333333703, 0.3333333333333333703, 0.3333333333333333148, 0.3333333333333334259, 0.3333333333333333148, 0.3333333333333335369, 0.3333333333333333148, 0.3333333333333333703, 0.3333333333333333703, 0.3333333333333333703, 0.3333333333333334259, 0.3333333333333332593, 0.3333333333333333703, 0.3333333333333333703, 0.3333333333333333703, 0.3333333333333333703, 0.3333333333333333148, 0.3333333333333333703, 0.3333333333333333703, 0.3333333333333334259, 0.3333333333333333703, 0.3333333333333333703, 0.3333333333333335369, 0.3333333333333333148, 0.3333333333333333148, 0.3333333333333333703, 0.3333333333333333703, 0.3333333333333333148, 0.3333333333333334259, 0.3333333333333333148, 0.3333333333333333703, 0.3333333333333333148, 0.3333333333333334814, 0.3333333333333334259, 0.3333333333333333703, 0.3333333333333334259, 0.3333333333333334259, 0.3333333333333332593, 0.3333333333333333703, 0.3333333333333334259, 0.3333333333333334259, 0.3333333333333333148, 0.3333333333333334259, 0.3333333333333333148, 0.3333333333333334259, 0.3333333333333333703, 0.3333333333333333148, 0.3333333333333334814, 0.3333333333333332038, 0.3333333333333333703, 0.3333333333333334259, 0.3333333333333333703, 0.3333333333333333703, 0.3333333333333334814, 0.3333333333333332593, 0.3333333333333334814, 0.3333333333333332593, 0.3333333333333334259, 0.3333333333333334259, 0.3333333333333332593, 0.3333333333333334259, 0.3333333333333334259, 0.3333333333333333148, 0.3333333333333332593, 0.3333333333333334259, 0.3333333333333333148, 0.3333333333333334259, 0.3333333333333333703, 0.3333333333333334259, 0.3333333333333332038, 0.3333333333333334814, 0.3333333333333333148, 0.3333333333333333703, 0.3333333333333334259, 0.3333333333333333703, 0.3333333333333333703, 0.3333333333333334259, 0.3333333333333334259, 0.3333333333333333148, 0.3333333333333334259, 0.3333333333333333148, 0.3333333333333333703, 0.3333333333333333703, 0.3333333333333333148, 0.3333333333333335369, 0.3333333333333333148, 0.3333333333333334259, 0.3333333333333333148, 0.3333333333333334259, 0.3333333333333335369, 0.3333333333333332593, 0.3333333333333333703, 0.3333333333333333148, 0.3333333333333334259, 0.3333333333333333148, 0.3333333333333334814, 0.3333333333333332593, 0.3333333333333333703, 0.3333333333333333148, 0.3333333333333334259, 0.3333333333333333703, 0.3333333333333333148, 0.3333333333333333703, 0.3333333333333334814, 0.3333333333333333148, 0.3333333333333333703, 0.3333333333333333148, 0.3333333333333333703, 0.3333333333333333148, 0.3333333333333333703, 0.3333333333333333148, 0.3333333333333332593, 0.3333333333333334814, 0.3333333333333332593, 0.3333333333333335369, 0.3333333333333333703, 0.3333333333333333703, 0.3333333333333332038, 0.3333333333333335369, 0.3333333333333333703, 0.3333333333333334259, 0.3333333333333333148, 0.3333333333333334259, 0.3333333333333333148, 0.3333333333333334259, 0.3333333333333333703, 0.3333333333333333703, 0.3333333333333333703, 0.3333333333333334814, 0.3333333333333332038, 0.3333333333333334814, 0.3333333333333333148, 0.3333333333333334259, 0.3333333333333333148, 0.3333333333333333703, 0.3333333333333333703, 0.3333333333333333703, 0.3333333333333332593, 0.3333333333333334814, 0.3333333333333333148, 0.3333333333333333703, 0.3333333333333334259, 0.3333333333333333148, 0.3333333333333334259, 0.3333333333333333703, 0.3333333333333334814, 0.3333333333333333148, 0.3333333333333333703, 0.3333333333333334259, 0.3333333333333333703, 0.3333333333333333148, 0.3333333333333334814, 0.3333333333333333703, 0.3333333333333332593, 0.3333333333333335369, 0.3333333333333332038, 0.3333333333333335369, 0.3333333333333333148, 0.3333333333333334259, 0.3333333333333333703, 0.3333333333333333703, 0.3333333333333334259, 0.3333333333333333703, 0.3333333333333333703, 0.3333333333333333703, 0.3333333333333332593, 0.3333333333333334259, 0.3333333333333334259, 0.3333333333333333148, 0.3333333333333333703, 0.3333333333333333148, 0.3333333333333334259, 0.3333333333333334259, 0.3333333333333333148, 0.3333333333333333703, 0.3333333333333333703, 0.3333333333333333703, 0.3333333333333333703, 0.3333333333333334259, 0.3333333333333334259, 0.3333333333333333703, 0.3333333333333334259, 0.3333333333333333148, 0.3333333333333334814, 0.3333333333333334259, 0.3333333333333333148, 0.3333333333333333703, 0.3333333333333333703, 0.3333333333333334259, 0.3333333333333333703, 0.3333333333333333703, 0.3333333333333333148, 0.3333333333333335924, 0.3333333333333332038, 0.3333333333333335924, 0.3333333333333333148, 0.3333333333333333703, 0.3333333333333333148, 0.3333333333333333148, 0.3333333333333334814, 0.3333333333333332038, 0.3333333333333334814, 0.3333333333333334259, 0.3333333333333333703, 0.3333333333333334259, 0.3333333333333333148, 0.3333333333333333703, 0.3333333333333334259, 0.3333333333333333148, 0.3333333333333333148, 0.3333333333333334259, 0.3333333333333334259, 0.3333333333333333148, 0.3333333333333334814, 0.3333333333333333703, 0.3333333333333334259, 0.3333333333333333703, 0.3333333333333333148, 0.3333333333333333703, 0.3333333333333333703, 0.3333333333333333703, 0.3333333333333333703, 0.3333333333333333703, 0.3333333333333334814, 0.3333333333333333148, 0.3333333333333334259, 0.3333333333333334259, 0.3333333333333333148, 0.3333333333333334259, 0.3333333333333332038, 0.3333333333333335369, 0.3333333333333332593, 0.3333333333333333703, 0.3333333333333333703, 0.3333333333333333148, 0.3333333333333334259, 0.3333333333333333148, 0.3333333333333334259, 0.3333333333333333148, 0.3333333333333333703, 0.3333333333333334259, 0.3333333333333333703, 0.3333333333333333148, 0.3333333333333333703, 0.3333333333333333148, 0.3333333333333334259, 0.3333333333333334259, 0.3333333333333333148, 0.3333333333333333148, 0.3333333333333333703, 0.3333333333333333703, 0.3333333333333333703, 0.3333333333333333703, 0.3333333333333334259, 0.3333333333333333148, 0.3333333333333334814, 0.3333333333333332593, 0.3333333333333334259, 0.3333333333333333703, 0.3333333333333333703, 0.3333333333333333703, 0.3333333333333333148, 0.3333333333333335369, 0.3333333333333333703, 0.3333333333333332593, 0.3333333333333334814, 0.3333333333333333703, 0.3333333333333333703, 0.3333333333333333703, 0.3333333333333333703, 0.3333333333333333703, 0.3333333333333333703, 0.3333333333333333703, 0.3333333333333333703, 0.3333333333333333703, 0.3333333333333334259, 0.3333333333333332593, 0.3333333333333333148, 0.3333333333333334259, 0.3333333333333334259, 0.3333333333333334259),
 ( 0.3333333333333334259, 0.3333333333333334259, 0.3333333333333333703, 0.3333333333333334259, 0.3333333333333333703, 0.3333333333333332593, 0.3333333333333334814, 0.3333333333333333703, 0.3333333333333334814, 0.3333333333333334259, 0.3333333333333333148, 0.3333333333333333148, 0.3333333333333333703, 0.3333333333333334259, 0.3333333333333332593, 0.3333333333333334814, 0.3333333333333331483, 0.3333333333333334814, 0.3333333333333333148, 0.3333333333333333148, 0.3333333333333334259, 0.3333333333333333703, 0.3333333333333333703, 0.3333333333333333148, 0.3333333333333335369, 0.3333333333333332593, 0.3333333333333333703, 0.3333333333333333703, 0.3333333333333334259, 0.3333333333333333148, 0.3333333333333333148, 0.3333333333333333148, 0.3333333333333334259, 0.3333333333333332593, 0.3333333333333334259, 0.3333333333333334259, 0.3333333333333333148, 0.3333333333333332593, 0.3333333333333333703, 0.3333333333333333703, 0.3333333333333332593, 0.3333333333333334814, 0.3333333333333333703, 0.3333333333333333703, 0.3333333333333333148, 0.3333333333333334259, 0.3333333333333333703, 0.3333333333333333703, 0.3333333333333334814, 0.3333333333333332038, 0.3333333333333334259, 0.3333333333333333703, 0.3333333333333333148, 0.3333333333333333148, 0.3333333333333333703, 0.3333333333333333703, 0.3333333333333333148, 0.3333333333333334814, 0.3333333333333333148, 0.3333333333333333703, 0.3333333333333333148, 0.3333333333333333148, 0.3333333333333334259, 0.3333333333333333703, 0.3333333333333333703, 0.3333333333333334259, 0.3333333333333333148, 0.3333333333333333148, 0.3333333333333333703, 0.3333333333333333703, 0.3333333333333332593, 0.3333333333333333703, 0.3333333333333333703, 0.3333333333333333703, 0.3333333333333333148, 0.3333333333333333148, 0.3333333333333334814, 0.3333333333333333703, 0.3333333333333334259, 0.3333333333333334259, 0.3333333333333334814, 0.3333333333333333148, 0.3333333333333333703, 0.3333333333333334259, 0.3333333333333333148, 0.3333333333333333703, 0.3333333333333333703, 0.3333333333333333703, 0.3333333333333333703, 0.3333333333333333703, 0.3333333333333333148, 0.3333333333333334814, 0.3333333333333332593, 0.3333333333333334259, 0.3333333333333333703, 0.3333333333333333703, 0.3333333333333333148, 0.3333333333333333703, 0.3333333333333334259, 0.3333333333333332593, 0.3333333333333334259, 0.3333333333333333703, 0.3333333333333333148, 0.3333333333333333148, 0.3333333333333332593, 0.3333333333333334259, 0.3333333333333333703, 0.3333333333333333703, 0.3333333333333333148, 0.3333333333333334259, 0.3333333333333333148, 0.3333333333333335369, 0.3333333333333333148, 0.3333333333333333703, 0.3333333333333333703, 0.3333333333333333703, 0.3333333333333334259, 0.3333333333333332593, 0.3333333333333333703, 0.3333333333333333703, 0.3333333333333333703, 0.3333333333333333703, 0.3333333333333333148, 0.3333333333333333703, 0.3333333333333333703, 0.3333333333333334259, 0.3333333333333333703, 0.3333333333333333703, 0.3333333333333335369, 0.3333333333333333148, 0.3333333333333333148, 0.3333333333333333703, 0.3333333333333333703, 0.3333333333333333148, 0.3333333333333334259, 0.3333333333333333148, 0.3333333333333333703, 0.3333333333333333148, 0.3333333333333334814, 0.3333333333333334259, 0.3333333333333333703, 0.3333333333333334259, 0.3333333333333334259, 0.3333333333333332593, 0.3333333333333333703, 0.3333333333333334259, 0.3333333333333334259, 0.3333333333333333148, 0.3333333333333334259, 0.3333333333333333148, 0.3333333333333334259, 0.3333333333333333703, 0.3333333333333333148, 0.3333333333333334814, 0.3333333333333332038, 0.3333333333333333703, 0.3333333333333334259, 0.3333333333333333703, 0.3333333333333333703, 0.3333333333333334814, 0.3333333333333332593, 0.3333333333333334814, 0.3333333333333332593, 0.3333333333333334259, 0.3333333333333334259, 0.3333333333333332593, 0.3333333333333334259, 0.3333333333333334259, 0.3333333333333333148, 0.3333333333333332593, 0.3333333333333334259, 0.3333333333333333148, 0.3333333333333334259, 0.3333333333333333703, 0.3333333333333334259, 0.3333333333333332038, 0.3333333333333334814, 0.3333333333333333148, 0.3333333333333333703, 0.3333333333333334259, 0.3333333333333333703, 0.3333333333333333703, 0.3333333333333334259, 0.3333333333333334259, 0.3333333333333333148, 0.3333333333333334259, 0.3333333333333333148, 0.3333333333333333703, 0.3333333333333333703, 0.3333333333333333148, 0.3333333333333335369, 0.3333333333333333148, 0.3333333333333334259, 0.3333333333333333148, 0.3333333333333334259, 0.3333333333333335369, 0.3333333333333332593, 0.3333333333333333703, 0.3333333333333333148, 0.3333333333333334259, 0.3333333333333333148, 0.3333333333333334814, 0.3333333333333332593, 0.3333333333333333703, 0.3333333333333333148, 0.3333333333333334259, 0.3333333333333333703, 0.3333333333333333148, 0.3333333333333333703, 0.3333333333333334814, 0.3333333333333333148, 0.3333333333333333703, 0.3333333333333333148, 0.3333333333333333703, 0.3333333333333333148, 0.3333333333333333703, 0.3333333333333333148, 0.3333333333333332593, 0.3333333333333334814, 0.3333333333333332593, 0.3333333333333335369, 0.3333333333333333703, 0.3333333333333333703, 0.3333333333333332038, 0.3333333333333335369, 0.3333333333333333703, 0.3333333333333334259, 0.3333333333333333148, 0.3333333333333334259, 0.3333333333333333148, 0.3333333333333334259, 0.3333333333333333703, 0.3333333333333333703, 0.3333333333333333703, 0.3333333333333334814, 0.3333333333333332038, 0.3333333333333334814, 0.3333333333333333148, 0.3333333333333334259, 0.3333333333333333148, 0.3333333333333333703, 0.3333333333333333703, 0.3333333333333333703, 0.3333333333333332593, 0.3333333333333334814, 0.3333333333333333148, 0.3333333333333333703, 0.3333333333333334259, 0.3333333333333333148, 0.3333333333333334259, 0.3333333333333333703, 0.3333333333333334814, 0.3333333333333333148, 0.3333333333333333703, 0.3333333333333334259, 0.3333333333333333703, 0.3333333333333333148, 0.3333333333333334814, 0.3333333333333333703, 0.3333333333333332593, 0.3333333333333335369, 0.3333333333333332038, 0.3333333333333335369, 0.3333333333333333148, 0.3333333333333334259, 0.3333333333333333703, 0.3333333333333333703, 0.3333333333333334259, 0.3333333333333333703, 0.3333333333333333703, 0.3333333333333333703, 0.3333333333333332593, 0.3333333333333334259, 0.3333333333333334259, 0.3333333333333333148, 0.3333333333333333703, 0.3333333333333333148, 0.3333333333333334259, 0.3333333333333334259, 0.3333333333333333148, 0.3333333333333333703, 0.3333333333333333703, 0.3333333333333333703, 0.3333333333333333703, 0.3333333333333334259, 0.3333333333333334259, 0.3333333333333333703, 0.3333333333333334259, 0.3333333333333333148, 0.3333333333333334814, 0.3333333333333334259, 0.3333333333333333148, 0.3333333333333333703, 0.3333333333333333703, 0.3333333333333334259, 0.3333333333333333703, 0.3333333333333333703, 0.3333333333333333148, 0.3333333333333335924, 0.3333333333333332038, 0.3333333333333335924, 0.3333333333333333148, 0.3333333333333333703, 0.3333333333333333148, 0.3333333333333333148, 0.3333333333333334814, 0.3333333333333332038, 0.3333333333333334814, 0.3333333333333334259, 0.3333333333333333703, 0.3333333333333334259, 0.3333333333333333148, 0.3333333333333333703, 0.3333333333333334259, 0.3333333333333333148, 0.3333333333333333148, 0.3333333333333334259, 0.3333333333333334259, 0.3333333333333333148, 0.3333333333333334814, 0.3333333333333333703, 0.3333333333333334259, 0.3333333333333333703, 0.3333333333333333148, 0.3333333333333333703, 0.3333333333333333703, 0.3333333333333333703, 0.3333333333333333703, 0.3333333333333333703, 0.3333333333333334814, 0.3333333333333333148, 0.3333333333333334259, 0.3333333333333334259, 0.3333333333333333148, 0.3333333333333334259, 0.3333333333333332038, 0.3333333333333335369, 0.3333333333333332593, 0.3333333333333333703, 0.3333333333333333703, 0.3333333333333333148, 0.3333333333333334259, 0.3333333333333333148, 0.3333333333333334259, 0.3333333333333333148, 0.3333333333333333703, 0.3333333333333334259, 0.3333333333333333703, 0.3333333333333333148, 0.3333333333333333703, 0.3333333333333333148, 0.3333333333333334259, 0.3333333333333334259, 0.3333333333333333148, 0.3333333333333333148, 0.3333333333333333703, 0.3333333333333333703, 0.3333333333333333703, 0.3333333333333333703, 0.3333333333333334259, 0.3333333333333333148, 0.3333333333333334814, 0.3333333333333332593, 0.3333333333333334259, 0.3333333333333333703, 0.3333333333333333703, 0.3333333333333333703, 0.3333333333333333148, 0.3333333333333335369, 0.3333333333333333703, 0.3333333333333332593, 0.3333333333333334814, 0.3333333333333333703, 0.3333333333333333703, 0.3333333333333333703, 0.3333333333333333703, 0.3333333333333333703, 0.3333333333333333703, 0.3333333333333333703, 0.3333333333333333703, 0.3333333333333333703, 0.3333333333333334259, 0.3333333333333332593, 0.3333333333333333148, 0.3333333333333334259, 0.3333333333333334259, 0.3333333333333334259),
 ( 1.000000000000000222, 1.000000000000000222, 1.000000000000000000, 1.000000000000000222, 1.000000000000000000, 0.9999999999999997780, 1.000000000000000222, 1.000000000000000000, 1.000000000000000222, 1.000000000000000222, 1.000000000000000000, 0.9999999999999997780, 1.000000000000000000, 1.000000000000000222, 0.9999999999999997780, 1.000000000000000222, 0.9999999999999994449, 1.000000000000000444, 0.9999999999999996669, 1.000000000000000000, 1.000000000000000222, 1.000000000000000000, 1.000000000000000000, 0.9999999999999997780, 1.000000000000000444, 0.9999999999999996669, 1.000000000000000000, 1.000000000000000222, 0.9999999999999997780, 1.000000000000000000, 0.9999999999999997780, 0.9999999999999997780, 1.000000000000000444, 0.9999999999999994449, 1.000000000000000444, 0.9999999999999997780, 0.9999999999999997780, 0.9999999999999996669, 1.000000000000000222, 1.000000000000000000, 0.9999999999999997780, 1.000000000000000222, 0.9999999999999997780, 1.000000000000000222, 1.000000000000000000, 1.000000000000000222, 1.000000000000000000, 1.000000000000000000, 1.000000000000000444, 0.9999999999999996669, 0.9999999999999997780, 1.000000000000000000, 0.9999999999999997780, 0.9999999999999997780, 1.000000000000000000, 1.000000000000000000, 0.9999999999999997780, 1.000000000000000444, 1.000000000000000000, 0.9999999999999997780, 1.000000000000000222, 0.9999999999999996669, 1.000000000000000222, 1.000000000000000000, 0.9999999999999997780, 1.000000000000000222, 0.9999999999999997780, 1.000000000000000000, 0.9999999999999997780, 1.000000000000000222, 0.9999999999999996669, 1.000000000000000000, 1.000000000000000222, 0.9999999999999997780, 1.000000000000000222, 0.9999999999999996669, 1.000000000000000444, 1.000000000000000000, 1.000000000000000000, 1.000000000000000222, 1.000000000000000222, 1.000000000000000000, 0.9999999999999997780, 1.000000000000000222, 0.9999999999999997780, 1.000000000000000000, 1.000000000000000000, 1.000000000000000000, 0.9999999999999997780, 1.000000000000000000, 0.9999999999999997780, 1.000000000000000222, 0.9999999999999997780, 1.000000000000000000, 1.000000000000000222, 0.9999999999999997780, 1.000000000000000000, 0.9999999999999996669, 1.000000000000000444, 0.9999999999999997780, 1.000000000000000000, 1.000000000000000000, 1.000000000000000000, 0.9999999999999997780, 0.9999999999999997780, 1.000000000000000222, 1.000000000000000222, 0.9999999999999997780, 1.000000000000000000, 1.000000000000000000, 1.000000000000000222, 1.000000000000000222, 1.000000000000000000, 0.9999999999999997780, 1.000000000000000222, 1.000000000000000000, 1.000000000000000000, 0.9999999999999997780, 0.9999999999999997780, 1.000000000000000222, 1.000000000000000000, 1.000000000000000000, 1.000000000000000000, 0.9999999999999997780, 1.000000000000000222, 1.000000000000000000, 1.000000000000000000, 1.000000000000000000, 1.000000000000000444, 0.9999999999999997780, 0.9999999999999997780, 1.000000000000000000, 1.000000000000000000, 0.9999999999999997780, 1.000000000000000222, 0.9999999999999997780, 1.000000000000000222, 1.000000000000000000, 1.000000000000000222, 1.000000000000000222, 1.000000000000000000, 1.000000000000000222, 1.000000000000000000, 0.9999999999999996669, 1.000000000000000222, 0.9999999999999997780, 1.000000000000000444, 0.9999999999999997780, 1.000000000000000000, 0.9999999999999997780, 1.000000000000000222, 1.000000000000000000, 0.9999999999999997780, 1.000000000000000222, 0.9999999999999994449, 1.000000000000000000, 1.000000000000000222, 1.000000000000000222, 0.9999999999999997780, 1.000000000000000444, 0.9999999999999997780, 1.000000000000000222, 0.9999999999999997780, 1.000000000000000222, 0.9999999999999997780, 1.000000000000000000, 1.000000000000000000, 1.000000000000000222, 0.9999999999999997780, 0.9999999999999996669, 1.000000000000000444, 0.9999999999999997780, 1.000000000000000222, 1.000000000000000000, 1.000000000000000222, 0.9999999999999994449, 1.000000000000000444, 0.9999999999999997780, 1.000000000000000000, 1.000000000000000222, 1.000000000000000000, 1.000000000000000000, 0.9999999999999997780, 1.000000000000000444, 0.9999999999999997780, 1.000000000000000444, 0.9999999999999997780, 1.000000000000000000, 1.000000000000000222, 0.9999999999999996669, 1.000000000000000222, 1.000000000000000000, 1.000000000000000000, 0.9999999999999996669, 1.000000000000000222, 1.000000000000000444, 0.9999999999999997780, 1.000000000000000222, 0.9999999999999996669, 1.000000000000000444, 0.9999999999999997780, 1.000000000000000444, 0.9999999999999996669, 0.9999999999999997780, 1.000000000000000000, 0.9999999999999997780, 1.000000000000000000, 1.000000000000000000, 1.000000000000000000, 1.000000000000000000, 0.9999999999999997780, 1.000000000000000000, 0.9999999999999997780, 1.000000000000000000, 1.000000000000000000, 1.000000000000000000, 1.000000000000000000, 0.9999999999999997780, 1.000000000000000222, 0.9999999999999997780, 1.000000000000000222, 0.9999999999999997780, 1.000000000000000222, 0.9999999999999994449, 1.000000000000000444, 1.000000000000000000, 1.000000000000000222, 0.9999999999999997780, 1.000000000000000000, 0.9999999999999997780, 1.000000000000000222, 1.000000000000000000, 1.000000000000000000, 1.000000000000000222, 1.000000000000000222, 0.9999999999999996669, 1.000000000000000444, 0.9999999999999996669, 1.000000000000000444, 0.9999999999999996669, 1.000000000000000000, 1.000000000000000000, 1.000000000000000000, 0.9999999999999997780, 1.000000000000000222, 0.9999999999999997780, 1.000000000000000222, 1.000000000000000000, 0.9999999999999997780, 1.000000000000000000, 1.000000000000000222, 1.000000000000000222, 1.000000000000000000, 1.000000000000000000, 1.000000000000000000, 1.000000000000000000, 0.9999999999999997780, 1.000000000000000444, 1.000000000000000000, 0.9999999999999997780, 1.000000000000000222, 0.9999999999999996669, 1.000000000000000444, 1.000000000000000000, 1.000000000000000222, 1.000000000000000222, 0.9999999999999997780, 1.000000000000000222, 0.9999999999999997780, 1.000000000000000000, 1.000000000000000000, 0.9999999999999997780, 1.000000000000000000, 1.000000000000000000, 0.9999999999999997780, 1.000000000000000222, 1.000000000000000000, 1.000000000000000000, 1.000000000000000222, 1.000000000000000000, 1.000000000000000000, 1.000000000000000000, 1.000000000000000222, 0.9999999999999997780, 1.000000000000000222, 1.000000000000000000, 0.9999999999999997780, 1.000000000000000222, 0.9999999999999997780, 1.000000000000000222, 1.000000000000000222, 1.000000000000000000, 0.9999999999999997780, 1.000000000000000000, 1.000000000000000222, 1.000000000000000000, 1.000000000000000000, 0.9999999999999996669, 1.000000000000000444, 0.9999999999999994449, 1.000000000000000444, 0.9999999999999997780, 1.000000000000000000, 1.000000000000000000, 0.9999999999999997780, 1.000000000000000222, 0.9999999999999997780, 1.000000000000000000, 1.000000000000000444, 0.9999999999999997780, 1.000000000000000000, 0.9999999999999997780, 1.000000000000000000, 1.000000000000000000, 0.9999999999999997780, 0.9999999999999997780, 1.000000000000000000, 1.000000000000000444, 1.000000000000000000, 1.000000000000000444, 1.000000000000000000, 1.000000000000000000, 1.000000000000000000, 0.9999999999999997780, 1.000000000000000000, 1.000000000000000000, 1.000000000000000000, 1.000000000000000000, 0.9999999999999997780, 1.000000000000000222, 1.000000000000000000, 0.9999999999999997780, 1.000000000000000444, 0.9999999999999997780, 1.000000000000000222, 0.9999999999999996669, 1.000000000000000444, 1.000000000000000000, 0.9999999999999997780, 1.000000000000000000, 1.000000000000000000, 1.000000000000000000, 0.9999999999999997780, 1.000000000000000000, 1.000000000000000000, 0.9999999999999997780, 1.000000000000000444, 0.9999999999999997780, 0.9999999999999997780, 1.000000000000000000, 1.000000000000000000, 1.000000000000000222, 1.000000000000000222, 0.9999999999999997780, 1.000000000000000000, 1.000000000000000222, 1.000000000000000000, 0.9999999999999997780, 1.000000000000000222, 1.000000000000000000, 1.000000000000000000, 1.000000000000000000, 0.9999999999999997780, 1.000000000000000000, 1.000000000000000000, 1.000000000000000000, 1.000000000000000000, 0.9999999999999997780, 1.000000000000000666, 0.9999999999999996669, 0.9999999999999996669, 1.000000000000000444, 0.9999999999999996669, 1.000000000000000222, 1.000000000000000000, 1.000000000000000000, 1.000000000000000000, 1.000000000000000000, 1.000000000000000000, 0.9999999999999997780, 1.000000000000000222, 1.000000000000000222, 0.9999999999999996669, 0.9999999999999997780, 1.000000000000000000, 1.000000000000000222, 1.000000000000000222),
 ( 0.3333333333333334259, 0.3333333333333334259, 0.3333333333333333703, 0.3333333333333334259, 0.3333333333333333703, 0.3333333333333332593, 0.3333333333333334814, 0.3333333333333333703, 0.3333333333333334814, 0.3333333333333334259, 0.3333333333333333148, 0.3333333333333333148, 0.3333333333333333703, 0.3333333333333334259, 0.3333333333333332593, 0.3333333333333334814, 0.3333333333333331483, 0.3333333333333334814, 0.3333333333333333148, 0.3333333333333333148, 0.3333333333333334259, 0.3333333333333333703, 0.3333333333333333703, 0.3333333333333333148, 0.3333333333333335369, 0.3333333333333332593, 0.3333333333333333703, 0.3333333333333333703, 0.3333333333333334259, 0.3333333333333333148, 0.3333333333333333148, 0.3333333333333333148, 0.3333333333333334259, 0.3333333333333332593, 0.3333333333333334259, 0.3333333333333334259, 0.3333333333333333148, 0.3333333333333332593, 0.3333333333333333703, 0.3333333333333333703, 0.3333333333333332593, 0.3333333333333334814, 0.3333333333333333703, 0.3333333333333333703, 0.3333333333333333148, 0.3333333333333334259, 0.3333333333333333703, 0.3333333333333333703, 0.3333333333333334814, 0.3333333333333332038, 0.3333333333333334259, 0.3333333333333333703, 0.3333333333333333148, 0.3333333333333333148, 0.3333333333333333703, 0.3333333333333333703, 0.3333333333333333148, 0.3333333333333334814, 0.3333333333333333148, 0.3333333333333333703, 0.3333333333333333148, 0.3333333333333333148, 0.3333333333333334259, 0.3333333333333333703, 0.3333333333333333703, 0.3333333333333334259, 0.3333333333333333148, 0.3333333333333333148, 0.3333333333333333703, 0.3333333333333333703, 0.3333333333333332593, 0.3333333333333333703, 0.3333333333333333703, 0.3333333333333333703, 0.3333333333333333148, 0.3333333333333333148, 0.3333333333333334814, 0.3333333333333333703, 0.3333333333333334259, 0.3333333333333334259, 0.3333333333333334814, 0.3333333333333333148, 0.3333333333333333703, 0.3333333333333334259, 0.3333333333333333148, 0.3333333333333333703, 0.3333333333333333703, 0.3333333333333333703, 0.3333333333333333703, 0.3333333333333333703, 0.3333333333333333148, 0.3333333333333334814, 0.3333333333333332593, 0.3333333333333334259, 0.3333333333333333703, 0.3333333333333333703, 0.3333333333333333148, 0.3333333333333333703, 0.3333333333333334259, 0.3333333333333332593, 0.3333333333333334259, 0.3333333333333333703, 0.3333333333333333148, 0.3333333333333333148, 0.3333333333333332593, 0.3333333333333334259, 0.3333333333333333703, 0.3333333333333333703, 0.3333333333333333148, 0.3333333333333334259, 0.3333333333333333148, 0.3333333333333335369, 0.3333333333333333148, 0.3333333333333333703, 0.3333333333333333703, 0.3333333333333333703, 0.3333333333333334259, 0.3333333333333332593, 0.3333333333333333703, 0.3333333333333333703, 0.3333333333333333703, 0.3333333333333333703, 0.3333333333333333148, 0.3333333333333333703, 0.3333333333333333703, 0.3333333333333334259, 0.3333333333333333703, 0.3333333333333333703, 0.3333333333333335369, 0.3333333333333333148, 0.3333333333333333148, 0.3333333333333333703, 0.3333333333333333703, 0.3333333333333333148, 0.3333333333333334259, 0.3333333333333333148, 0.3333333333333333703, 0.3333333333333333148, 0.3333333333333334814, 0.3333333333333334259, 0.3333333333333333703, 0.3333333333333334259, 0.3333333333333334259, 0.3333333333333332593, 0.3333333333333333703, 0.3333333333333334259, 0.3333333333333334259, 0.3333333333333333148, 0.3333333333333334259, 0.3333333333333333148, 0.3333333333333334259, 0.3333333333333333703, 0.3333333333333333148, 0.3333333333333334814, 0.3333333333333332038, 0.3333333333333333703, 0.3333333333333334259, 0.3333333333333333703, 0.3333333333333333703, 0.3333333333333334814, 0.3333333333333332593, 0.3333333333333334814, 0.3333333333333332593, 0.3333333333333334259, 0.3333333333333334259, 0.3333333333333332593, 0.3333333333333334259, 0.3333333333333334259, 0.3333333333333333148, 0.3333333333333332593, 0.3333333333333334259, 0.3333333333333333148, 0.3333333333333334259, 0.3333333333333333703, 0.3333333333333334259, 0.3333333333333332038, 0.3333333333333334814, 0.3333333333333333148, 0.3333333333333333703, 0.3333333333333334259, 0.3333333333333333703, 0.3333333333333333703, 0.3333333333333334259, 0.3333333333333334259, 0.3333333333333333148, 0.3333333333333334259, 0.3333333333333333148, 0.3333333333333333703, 0.3333333333333333703, 0.3333333333333333148, 0.3333333333333335369, 0.3333333333333333148, 0.3333333333333334259, 0.3333333333333333148, 0.3333333333333334259, 0.3333333333333335369, 0.3333333333333332593, 0.3333333333333333703, 0.3333333333333333148, 0.3333333333333334259, 0.3333333333333333148, 0.3333333333333334814, 0.3333333333333332593, 0.3333333333333333703, 0.3333333333333333148, 0.3333333333333334259, 0.3333333333333333703, 0.3333333333333333148, 0.3333333333333333703, 0.3333333333333334814, 0.3333333333333333148, 0.3333333333333333703, 0.3333333333333333148, 0.3333333333333333703, 0.3333333333333333148, 0.3333333333333333703, 0.3333333333333333148, 0.3333333333333332593, 0.3333333333333334814, 0.3333333333333332593, 0.3333333333333335369, 0.3333333333333333703, 0.3333333333333333703, 0.3333333333333332038, 0.3333333333333335369, 0.3333333333333333703, 0.3333333333333334259, 0.3333333333333333148, 0.3333333333333334259, 0.3333333333333333148, 0.3333333333333334259, 0.3333333333333333703, 0.3333333333333333703, 0.3333333333333333703, 0.3333333333333334814, 0.3333333333333332038, 0.3333333333333334814, 0.3333333333333333148, 0.3333333333333334259, 0.3333333333333333148, 0.3333333333333333703, 0.3333333333333333703, 0.3333333333333333703, 0.3333333333333332593, 0.3333333333333334814, 0.3333333333333333148, 0.3333333333333333703, 0.3333333333333334259, 0.3333333333333333148, 0.3333333333333334259, 0.3333333333333333703, 0.3333333333333334814, 0.3333333333333333148, 0.3333333333333333703, 0.3333333333333334259, 0.3333333333333333703, 0.3333333333333333148, 0.3333333333333334814, 0.3333333333333333703, 0.3333333333333332593, 0.3333333333333335369, 0.3333333333333332038, 0.3333333333333335369, 0.3333333333333333148, 0.3333333333333334259, 0.3333333333333333703, 0.3333333333333333703, 0.3333333333333334259, 0.3333333333333333703, 0.3333333333333333703, 0.3333333333333333703, 0.3333333333333332593, 0.3333333333333334259, 0.3333333333333334259, 0.3333333333333333148, 0.3333333333333333703, 0.3333333333333333148, 0.3333333333333334259, 0.3333333333333334259, 0.3333333333333333148, 0.3333333333333333703, 0.3333333333333333703, 0.3333333333333333703, 0.3333333333333333703, 0.3333333333333334259, 0.3333333333333334259, 0.3333333333333333703, 0.3333333333333334259, 0.3333333333333333148, 0.3333333333333334814, 0.3333333333333334259, 0.3333333333333333148, 0.3333333333333333703, 0.3333333333333333703, 0.3333333333333334259, 0.3333333333333333703, 0.3333333333333333703, 0.3333333333333333148, 0.3333333333333335924, 0.3333333333333332038, 0.3333333333333335924, 0.3333333333333333148, 0.3333333333333333703, 0.3333333333333333148, 0.3333333333333333148, 0.3333333333333334814, 0.3333333333333332038, 0.3333333333333334814, 0.3333333333333334259, 0.3333333333333333703, 0.3333333333333334259, 0.3333333333333333148, 0.3333333333333333703, 0.3333333333333334259, 0.3333333333333333148, 0.3333333333333333148, 0.3333333333333334259, 0.3333333333333334259, 0.3333333333333333148, 0.3333333333333334814, 0.3333333333333333703, 0.3333333333333334259, 0.3333333333333333703, 0.3333333333333333148, 0.3333333333333333703, 0.3333333333333333703, 0.3333333333333333703, 0.3333333333333333703, 0.3333333333333333703, 0.3333333333333334814, 0.3333333333333333148, 0.3333333333333334259, 0.3333333333333334259, 0.3333333333333333148, 0.3333333333333334259, 0.3333333333333332038, 0.3333333333333335369, 0.3333333333333332593, 0.3333333333333333703, 0.3333333333333333703, 0.3333333333333333148, 0.3333333333333334259, 0.3333333333333333148, 0.3333333333333334259, 0.3333333333333333148, 0.3333333333333333703, 0.3333333333333334259, 0.3333333333333333703, 0.3333333333333333148, 0.3333333333333333703, 0.3333333333333333148, 0.3333333333333334259, 0.3333333333333334259, 0.3333333333333333148, 0.3333333333333333148, 0.3333333333333333703, 0.3333333333333333703, 0.3333333333333333703, 0.3333333333333333703, 0.3333333333333334259, 0.3333333333333333148, 0.3333333333333334814, 0.3333333333333332593, 0.3333333333333334259, 0.3333333333333333703, 0.3333333333333333703, 0.3333333333333333703, 0.3333333333333333148, 0.3333333333333335369, 0.3333333333333333703, 0.3333333333333332593, 0.3333333333333334814, 0.3333333333333333703, 0.3333333333333333703, 0.3333333333333333703, 0.3333333333333333703, 0.3333333333333333703, 0.3333333333333333703, 0.3333333333333333703, 0.3333333333333333703, 0.3333333333333333703, 0.3333333333333334259, 0.3333333333333332593, 0.3333333333333333148, 0.3333333333333334259, 0.3333333333333334259, 0.3333333333333334259),
 ( 0.3333333333333334259, 0.3333333333333334259, 0.3333333333333333703, 0.3333333333333334259, 0.3333333333333333703, 0.3333333333333332593, 0.3333333333333334814, 0.3333333333333333703, 0.3333333333333334814, 0.3333333333333334259, 0.3333333333333333148, 0.3333333333333333148, 0.3333333333333333703, 0.3333333333333334259, 0.3333333333333332593, 0.3333333333333334814, 0.3333333333333331483, 0.3333333333333334814, 0.3333333333333333148, 0.3333333333333333148, 0.3333333333333334259, 0.3333333333333333703, 0.3333333333333333703, 0.3333333333333333148, 0.3333333333333335369, 0.3333333333333332593, 0.3333333333333333703, 0.3333333333333333703, 0.3333333333333334259, 0.3333333333333333148, 0.3333333333333333148, 0.3333333333333333148, 0.3333333333333334259, 0.3333333333333332593, 0.3333333333333334259, 0.3333333333333334259, 0.3333333333333333148, 0.3333333333333332593, 0.3333333333333333703, 0.3333333333333333703, 0.3333333333333332593, 0.3333333333333334814, 0.3333333333333333703, 0.3333333333333333703, 0.3333333333333333148, 0.3333333333333334259, 0.3333333333333333703, 0.3333333333333333703, 0.3333333333333334814, 0.3333333333333332038, 0.3333333333333334259, 0.3333333333333333703, 0.3333333333333333148, 0.3333333333333333148, 0.3333333333333333703, 0.3333333333333333703, 0.3333333333333333148, 0.3333333333333334814, 0.3333333333333333148, 0.3333333333333333703, 0.3333333333333333148, 0.3333333333333333148, 0.3333333333333334259, 0.3333333333333333703, 0.3333333333333333703, 0.3333333333333334259, 0.3333333333333333148, 0.3333333333333333148, 0.3333333333333333703, 0.3333333333333333703, 0.3333333333333332593, 0.3333333333333333703, 0.3333333333333333703, 0.3333333333333333703, 0.3333333333333333148, 0.3333333333333333148, 0.3333333333333334814, 0.3333333333333333703, 0.3333333333333334259, 0.3333333333333334259, 0.3333333333333334814, 0.3333333333333333148, 0.3333333333333333703, 0.3333333333333334259, 0.3333333333333333148, 0.3333333333333333703, 0.3333333333333333703, 0.3333333333333333703, 0.3333333333333333703, 0.3333333333333333703, 0.3333333333333333148, 0.3333333333333334814, 0.3333333333333332593, 0.3333333333333334259, 0.3333333333333333703, 0.3333333333333333703, 0.3333333333333333148, 0.3333333333333333703, 0.3333333333333334259, 0.3333333333333332593, 0.3333333333333334259, 0.3333333333333333703, 0.3333333333333333148, 0.3333333333333333148, 0.3333333333333332593, 0.3333333333333334259, 0.3333333333333333703, 0.3333333333333333703, 0.3333333333333333148, 0.3333333333333334259, 0.3333333333333333148, 0.3333333333333335369, 0.3333333333333333148, 0.3333333333333333703, 0.3333333333333333703, 0.3333333333333333703, 0.3333333333333334259, 0.3333333333333332593, 0.3333333333333333703, 0.3333333333333333703, 0.3333333333333333703, 0.3333333333333333703, 0.3333333333333333148, 0.3333333333333333703, 0.3333333333333333703, 0.3333333333333334259, 0.3333333333333333703, 0.3333333333333333703, 0.3333333333333335369, 0.3333333333333333148, 0.3333333333333333148, 0.3333333333333333703, 0.3333333333333333703, 0.3333333333333333148, 0.3333333333333334259, 0.3333333333333333148, 0.3333333333333333703, 0.3333333333333333148, 0.3333333333333334814, 0.3333333333333334259, 0.3333333333333333703, 0.3333333333333334259, 0.3333333333333334259, 0.3333333333333332593, 0.3333333333333333703, 0.3333333333333334259, 0.3333333333333334259, 0.3333333333333333148, 0.3333333333333334259, 0.3333333333333333148, 0.3333333333333334259, 0.3333333333333333703, 0.3333333333333333148, 0.3333333333333334814, 0.3333333333333332038, 0.3333333333333333703, 0.3333333333333334259, 0.3333333333333333703, 0.3333333333333333703, 0.3333333333333334814, 0.3333333333333332593, 0.3333333333333334814, 0.3333333333333332593, 0.3333333333333334259, 0.3333333333333334259, 0.3333333333333332593, 0.3333333333333334259, 0.3333333333333334259, 0.3333333333333333148, 0.3333333333333332593, 0.3333333333333334259, 0.3333333333333333148, 0.3333333333333334259, 0.3333333333333333703, 0.3333333333333334259, 0.3333333333333332038, 0.3333333333333334814, 0.3333333333333333148, 0.3333333333333333703, 0.3333333333333334259, 0.3333333333333333703, 0.3333333333333333703, 0.3333333333333334259, 0.3333333333333334259, 0.3333333333333333148, 0.3333333333333334259, 0.3333333333333333148, 0.3333333333333333703, 0.3333333333333333703, 0.3333333333333333148, 0.3333333333333335369, 0.3333333333333333148, 0.3333333333333334259, 0.3333333333333333148, 0.3333333333333334259, 0.3333333333333335369, 0.3333333333333332593, 0.3333333333333333703, 0.3333333333333333148, 0.3333333333333334259, 0.3333333333333333148, 0.3333333333333334814, 0.3333333333333332593, 0.3333333333333333703, 0.3333333333333333148, 0.3333333333333334259, 0.3333333333333333703, 0.3333333333333333148, 0.3333333333333333703, 0.3333333333333334814, 0.3333333333333333148, 0.3333333333333333703, 0.3333333333333333148, 0.3333333333333333703, 0.3333333333333333148, 0.3333333333333333703, 0.3333333333333333148, 0.3333333333333332593, 0.3333333333333334814, 0.3333333333333332593, 0.3333333333333335369, 0.3333333333333333703, 0.3333333333333333703, 0.3333333333333332038, 0.3333333333333335369, 0.3333333333333333703, 0.3333333333333334259, 0.3333333333333333148, 0.3333333333333334259, 0.3333333333333333148, 0.3333333333333334259, 0.3333333333333333703, 0.3333333333333333703, 0.3333333333333333703, 0.3333333333333334814, 0.3333333333333332038, 0.3333333333333334814, 0.3333333333333333148, 0.3333333333333334259, 0.3333333333333333148, 0.3333333333333333703, 0.3333333333333333703, 0.3333333333333333703, 0.3333333333333332593, 0.3333333333333334814, 0.3333333333333333148, 0.3333333333333333703, 0.3333333333333334259, 0.3333333333333333148, 0.3333333333333334259, 0.3333333333333333703, 0.3333333333333334814, 0.3333333333333333148, 0.3333333333333333703, 0.3333333333333334259, 0.3333333333333333703, 0.3333333333333333148, 0.3333333333333334814, 0.3333333333333333703, 0.3333333333333332593, 0.3333333333333335369, 0.3333333333333332038, 0.3333333333333335369, 0.3333333333333333148, 0.3333333333333334259, 0.3333333333333333703, 0.3333333333333333703, 0.3333333333333334259, 0.3333333333333333703, 0.3333333333333333703, 0.3333333333333333703, 0.3333333333333332593, 0.3333333333333334259, 0.3333333333333334259, 0.3333333333333333148, 0.3333333333333333703, 0.3333333333333333148, 0.3333333333333334259, 0.3333333333333334259, 0.3333333333333333148, 0.3333333333333333703, 0.3333333333333333703, 0.3333333333333333703, 0.3333333333333333703, 0.3333333333333334259, 0.3333333333333334259, 0.3333333333333333703, 0.3333333333333334259, 0.3333333333333333148, 0.3333333333333334814, 0.3333333333333334259, 0.3333333333333333148, 0.3333333333333333703, 0.3333333333333333703, 0.3333333333333334259, 0.3333333333333333703, 0.3333333333333333703, 0.3333333333333333148, 0.3333333333333335924, 0.3333333333333332038, 0.3333333333333335924, 0.3333333333333333148, 0.3333333333333333703, 0.3333333333333333148, 0.3333333333333333148, 0.3333333333333334814, 0.3333333333333332038, 0.3333333333333334814, 0.3333333333333334259, 0.3333333333333333703, 0.3333333333333334259, 0.3333333333333333148, 0.3333333333333333703, 0.3333333333333334259, 0.3333333333333333148, 0.3333333333333333148, 0.3333333333333334259, 0.3333333333333334259, 0.3333333333333333148, 0.3333333333333334814, 0.3333333333333333703, 0.3333333333333334259, 0.3333333333333333703, 0.3333333333333333148, 0.3333333333333333703, 0.3333333333333333703, 0.3333333333333333703, 0.3333333333333333703, 0.3333333333333333703, 0.3333333333333334814, 0.3333333333333333148, 0.3333333333333334259, 0.3333333333333334259, 0.3333333333333333148, 0.3333333333333334259, 0.3333333333333332038, 0.3333333333333335369, 0.3333333333333332593, 0.3333333333333333703, 0.3333333333333333703, 0.3333333333333333148, 0.3333333333333334259, 0.3333333333333333148, 0.3333333333333334259, 0.3333333333333333148, 0.3333333333333333703, 0.3333333333333334259, 0.3333333333333333703, 0.3333333333333333148, 0.3333333333333333703, 0.3333333333333333148, 0.3333333333333334259, 0.3333333333333334259, 0.3333333333333333148, 0.3333333333333333148, 0.3333333333333333703, 0.3333333333333333703, 0.3333333333333333703, 0.3333333333333333703, 0.3333333333333334259, 0.3333333333333333148, 0.3333333333333334814, 0.3333333333333332593, 0.3333333333333334259, 0.3333333333333333703, 0.3333333333333333703, 0.3333333333333333703, 0.3333333333333333148, 0.3333333333333335369, 0.3333333333333333703, 0.3333333333333332593, 0.3333333333333334814, 0.3333333333333333703, 0.3333333333333333703, 0.3333333333333333703, 0.3333333333333333703, 0.3333333333333333703, 0.3333333333333333703, 0.3333333333333333703, 0.3333333333333333703, 0.3333333333333333703, 0.3333333333333334259, 0.3333333333333332593, 0.3333333333333333148, 0.3333333333333334259, 0.3333333333333334259, 0.3333333333333334259),
 ( 1.000000000000000222, 1.000000000000000222, 1.000000000000000000, 1.000000000000000222, 1.000000000000000000, 0.9999999999999997780, 1.000000000000000222, 1.000000000000000000, 1.000000000000000222, 1.000000000000000222, 1.000000000000000000, 0.9999999999999997780, 1.000000000000000000, 1.000000000000000222, 0.9999999999999997780, 1.000000000000000222, 0.9999999999999994449, 1.000000000000000444, 0.9999999999999996669, 1.000000000000000000, 1.000000000000000222, 1.000000000000000000, 1.000000000000000000, 0.9999999999999997780, 1.000000000000000444, 0.9999999999999996669, 1.000000000000000000, 1.000000000000000222, 0.9999999999999997780, 1.000000000000000000, 0.9999999999999997780, 0.9999999999999997780, 1.000000000000000444, 0.9999999999999994449, 1.000000000000000444, 0.9999999999999997780, 0.9999999999999997780, 0.9999999999999996669, 1.000000000000000222, 1.000000000000000000, 0.9999999999999997780, 1.000000000000000222, 0.9999999999999997780, 1.000000000000000222, 1.000000000000000000, 1.000000000000000222, 1.000000000000000000, 1.000000000000000000, 1.000000000000000444, 0.9999999999999996669, 0.9999999999999997780, 1.000000000000000000, 0.9999999999999997780, 0.9999999999999997780, 1.000000000000000000, 1.000000000000000000, 0.9999999999999997780, 1.000000000000000444, 1.000000000000000000, 0.9999999999999997780, 1.000000000000000222, 0.9999999999999996669, 1.000000000000000222, 1.000000000000000000, 0.9999999999999997780, 1.000000000000000222, 0.9999999999999997780, 1.000000000000000000, 0.9999999999999997780, 1.000000000000000222, 0.9999999999999996669, 1.000000000000000000, 1.000000000000000222, 0.9999999999999997780, 1.000000000000000222, 0.9999999999999996669, 1.000000000000000444, 1.000000000000000000, 1.000000000000000000, 1.000000000000000222, 1.000000000000000222, 1.000000000000000000, 0.9999999999999997780, 1.000000000000000222, 0.9999999999999997780, 1.000000000000000000, 1.000000000000000000, 1.000000000000000000, 0.9999999999999997780, 1.000000000000000000, 0.9999999999999997780, 1.000000000000000222, 0.9999999999999997780, 1.000000000000000000, 1.000000000000000222, 0.9999999999999997780, 1.000000000000000000, 0.9999999999999996669, 1.000000000000000444, 0.9999999999999997780, 1.000000000000000000, 1.000000000000000000, 1.000000000000000000, 0.9999999999999997780, 0.9999999999999997780, 1.000000000000000222, 1.000000000000000222, 0.9999999999999997780, 1.000000000000000000, 1.000000000000000000, 1.000000000000000222, 1.000000000000000222, 1.000000000000000000, 0.9999999999999997780, 1.000000000000000222, 1.000000000000000000, 1.000000000000000000, 0.9999999999999997780, 0.9999999999999997780, 1.000000000000000222, 1.000000000000000000, 1.000000000000000000, 1.000000000000000000, 0.9999999999999997780, 1.000000000000000222, 1.000000000000000000, 1.000000000000000000, 1.000000000000000000, 1.000000000000000444, 0.9999999999999997780, 0.9999999999999997780, 1.000000000000000000, 1.000000000000000000, 0.9999999999999997780, 1.000000000000000222, 0.9999999999999997780, 1.000000000000000222, 1.000000000000000000, 1.000000000000000222, 1.000000000000000222, 1.000000000000000000, 1.000000000000000222, 1.000000000000000000, 0.9999999999999996669, 1.000000000000000222, 0.9999999999999997780, 1.000000000000000444, 0.9999999999999997780, 1.000000000000000000, 0.9999999999999997780, 1.000000000000000222, 1.000000000000000000, 0.9999999999999997780, 1.000000000000000222, 0.9999999999999994449, 1.000000000000000000, 1.000000000000000222, 1.000000000000000222, 0.9999999999999997780, 1.000000000000000444, 0.9999999999999997780, 1.000000000000000222, 0.9999999999999997780, 1.000000000000000222, 0.9999999999999997780, 1.000000000000000000, 1.000000000000000000, 1.000000000000000222, 0.9999999999999997780, 0.9999999999999996669, 1.000000000000000444, 0.9999999999999997780, 1.000000000000000222, 1.000000000000000000, 1.000000000000000222, 0.9999999999999994449, 1.000000000000000444, 0.9999999999999997780, 1.000000000000000000, 1.000000000000000222, 1.000000000000000000, 1.000000000000000000, 0.9999999999999997780, 1.000000000000000444, 0.9999999999999997780, 1.000000000000000444, 0.9999999999999997780, 1.000000000000000000, 1.000000000000000222, 0.9999999999999996669, 1.000000000000000222, 1.000000000000000000, 1.000000000000000000, 0.9999999999999996669, 1.000000000000000222, 1.000000000000000444, 0.9999999999999997780, 1.000000000000000222, 0.9999999999999996669, 1.000000000000000444, 0.9999999999999997780, 1.000000000000000444, 0.9999999999999996669, 0.9999999999999997780, 1.000000000000000000, 0.9999999999999997780, 1.000000000000000000, 1.000000000000000000, 1.000000000000000000, 1.000000000000000000, 0.9999999999999997780, 1.000000000000000000, 0.9999999999999997780, 1.000000000000000000, 1.000000000000000000, 1.000000000000000000, 1.000000000000000000, 0.9999999999999997780, 1.000000000000000222, 0.9999999999999997780, 1.000000000000000222, 0.9999999999999997780, 1.000000000000000222, 0.9999999999999994449, 1.000000000000000444, 1.000000000000000000, 1.000000000000000222, 0.9999999999999997780, 1.000000000000000000, 0.9999999999999997780, 1.000000000000000222, 1.000000000000000000, 1.000000000000000000, 1.000000000000000222, 1.000000000000000222, 0.9999999999999996669, 1.000000000000000444, 0.9999999999999996669, 1.000000000000000444, 0.9999999999999996669, 1.000000000000000000, 1.000000000000000000, 1.000000000000000000, 0.9999999999999997780, 1.000000000000000222, 0.9999999999999997780, 1.000000000000000222, 1.000000000000000000, 0.9999999999999997780, 1.000000000000000000, 1.000000000000000222, 1.000000000000000222, 1.000000000000000000, 1.000000000000000000, 1.000000000000000000, 1.000000000000000000, 0.9999999999999997780, 1.000000000000000444, 1.000000000000000000, 0.9999999999999997780, 1.000000000000000222, 0.9999999999999996669, 1.000000000000000444, 1.000000000000000000, 1.000000000000000222, 1.000000000000000222, 0.9999999999999997780, 1.000000000000000222, 0.9999999999999997780, 1.000000000000000000, 1.000000000000000000, 0.9999999999999997780, 1.000000000000000000, 1.000000000000000000, 0.9999999999999997780, 1.000000000000000222, 1.000000000000000000, 1.000000000000000000, 1.000000000000000222, 1.000000000000000000, 1.000000000000000000, 1.000000000000000000, 1.000000000000000222, 0.9999999999999997780, 1.000000000000000222, 1.000000000000000000, 0.9999999999999997780, 1.000000000000000222, 0.9999999999999997780, 1.000000000000000222, 1.000000000000000222, 1.000000000000000000, 0.9999999999999997780, 1.000000000000000000, 1.000000000000000222, 1.000000000000000000, 1.000000000000000000, 0.9999999999999996669, 1.000000000000000444, 0.9999999999999994449, 1.000000000000000444, 0.9999999999999997780, 1.000000000000000000, 1.000000000000000000, 0.9999999999999997780, 1.000000000000000222, 0.9999999999999997780, 1.000000000000000000, 1.000000000000000444, 0.9999999999999997780, 1.000000000000000000, 0.9999999999999997780, 1.000000000000000000, 1.000000000000000000, 0.9999999999999997780, 0.9999999999999997780, 1.000000000000000000, 1.000000000000000444, 1.000000000000000000, 1.000000000000000444, 1.000000000000000000, 1.000000000000000000, 1.000000000000000000, 0.9999999999999997780, 1.000000000000000000, 1.000000000000000000, 1.000000000000000000, 1.000000000000000000, 0.9999999999999997780, 1.000000000000000222, 1.000000000000000000, 0.9999999999999997780, 1.000000000000000444, 0.9999999999999997780, 1.000000000000000222, 0.9999999999999996669, 1.000000000000000444, 1.000000000000000000, 0.9999999999999997780, 1.000000000000000000, 1.000000000000000000, 1.000000000000000000, 0.9999999999999997780, 1.000000000000000000, 1.000000000000000000, 0.9999999999999997780, 1.000000000000000444, 0.9999999999999997780, 0.9999999999999997780, 1.000000000000000000, 1.000000000000000000, 1.000000000000000222, 1.000000000000000222, 0.9999999999999997780, 1.000000000000000000, 1.000000000000000222, 1.000000000000000000, 0.9999999999999997780, 1.000000000000000222, 1.000000000000000000, 1.000000000000000000, 1.000000000000000000, 0.9999999999999997780, 1.000000000000000000, 1.000000000000000000, 1.000000000000000000, 1.000000000000000000, 0.9999999999999997780, 1.000000000000000666, 0.9999999999999996669, 0.9999999999999996669, 1.000000000000000444, 0.9999999999999996669, 1.000000000000000222, 1.000000000000000000, 1.000000000000000000, 1.000000000000000000, 1.000000000000000000, 1.000000000000000000, 0.9999999999999997780, 1.000000000000000222, 1.000000000000000222, 0.9999999999999996669, 0.9999999999999997780, 1.000000000000000000, 1.000000000000000222, 1.000000000000000222) ) ) 
 REPRESENTATION_ITEM ( '' )  SURFACE ( )  );
#164987 = CARTESIAN_POINT ( 'NONE',  ( 4.984931625306495029, 2.076298541577546342, 0.6347802954964998357 ) ) ;
#164988 = CARTESIAN_POINT ( 'NONE',  ( 3.388648328411762556, 6.040841252200647382, 1.199719254218462483 ) ) ;
#164989 = CARTESIAN_POINT ( 'NONE',  ( 5.805875103277515770, -1.124240986939632592, -1.673857227857282082 ) ) ;
#164990 = CARTESIAN_POINT ( 'NONE',  ( 0.7500000000000005551, 4.270513119278528127E-14, 2.052068128417952497 ) ) ;
#164991 = CARTESIAN_POINT ( 'NONE',  ( 0.7499999999999902300, 4.347916667349481123, -1.299038105676658228 ) ) ;
#164992 = CARTESIAN_POINT ( 'NONE',  ( 2.432535651424679646, 1.868085840533942221, 0.4698736581597633966 ) ) ;
#164993 = CARTESIAN_POINT ( 'NONE',  ( -1.500000000000008216, 9.781250000682799595, 3.469446951953614189E-15 ) ) ;
#164994 = CARTESIAN_POINT ( 'NONE',  ( 6.082328216444968128, 1.141246503175277205, 1.905736721132505140 ) ) ;
#164995 = ORIENTED_EDGE ( 'NONE', *, *, #143394, .F. ) ;
#164996 = CARTESIAN_POINT ( 'NONE',  ( 6.983263157960368339, 4.695310640067480001, 2.508805386165738227 ) ) ;
#164997 = CARTESIAN_POINT ( 'NONE',  ( -1.201851678989727383E-14, 1.962500000000020783, 1.732050807568877637 ) ) ;
#164998 = CARTESIAN_POINT ( 'NONE',  ( 6.262976894508937242, 9.394224579314053969, -1.199719254218440723 ) ) ;
#164999 = CARTESIAN_POINT ( 'NONE',  ( 1.647463811467297701, 0.2220449547728920447, 2.210189655316461277 ) ) ;
#165000 = CARTESIAN_POINT ( 'NONE',  ( 6.461383593301071926, 1.630371061775518271, 1.090930979547571456 ) ) ;
#165001 = CARTESIAN_POINT ( 'NONE',  ( 7.782016984564054773, 10.10210578678999482, 1.443375672974076540 ) ) ;
#165002 = CARTESIAN_POINT ( 'NONE',  ( 5.727393547130178675, 5.646656991265468939, 0.000000000000000000 ) ) ;
#165003 = CARTESIAN_POINT ( 'NONE',  ( -3.526529353330355221, 6.168015774643768268, -1.082531754730546636 ) ) ;
#165005 = CARTESIAN_POINT ( 'NONE',  ( 4.299324853187779460, -1.796095115987613955, 1.014086197209535634 ) ) ;
#165004 = DIRECTION ( 'NONE',  ( 2.949029909160572061E-17, 1.000000000000000000, -8.673600428462579015E-15 ) ) ;
#165006 = CARTESIAN_POINT ( 'NONE',  ( -3.242371291962510504, 6.934516940598226320, 1.040834085586084257E-14 ) ) ;
#165007 = CARTESIAN_POINT ( 'NONE',  ( -0.7500000000000215383, 5.222916667349482012, 1.299038105676671107 ) ) ;
#165008 = CARTESIAN_POINT ( 'NONE',  ( -0.6823417656250246877, -0.9489583329919115684, 1.181850606188755259 ) ) ;
#165009 = CARTESIAN_POINT ( 'NONE',  ( 6.116445839754358182, 1.256427234498383561, -1.385894902050835542 ) ) ;
#165010 = CARTESIAN_POINT ( 'NONE',  ( 4.711369565069784215, 1.661324788532690500, 0.4972849887868810437 ) ) ;
#165011 = CARTESIAN_POINT ( 'NONE',  ( 4.950617407298735451, -1.474004690277466834, -0.9251219707713809193 ) ) ;
#165012 = CARTESIAN_POINT ( 'NONE',  ( 2.849184837166184536, 6.475799410002530898, 0.7998128361456362523 ) ) ;
#165013 = CARTESIAN_POINT ( 'NONE',  ( 1.593750267980385882, -0.7671775610453807070, 2.160330554385545110 ) ) ;
#165014 = CARTESIAN_POINT ( 'NONE',  ( -1.364683531249997417, 5.821875000341418804, 1.214306433183764966E-14 ) ) ;
#165015 = CARTESIAN_POINT ( 'NONE',  ( 6.023005994326640078, -1.968326514718239828, 0.7052485104920204195 ) ) ;
#165016 = CARTESIAN_POINT ( 'NONE',  ( 1.183273638618479673, -0.8294958387620559037, 1.643756842616146630 ) ) ;
#165017 = EDGE_CURVE ( 'NONE', #100589, #187284, #128437, .T. ) ;
#165018 = CARTESIAN_POINT ( 'NONE',  ( 10.72180055030867329, 11.40318881831530540, 0.7998128361456341429 ) ) ;
#165019 =( NAMED_UNIT ( * ) SI_UNIT ( $, .STERADIAN. ) SOLID_ANGLE_UNIT ( ) );
#165020 = CARTESIAN_POINT ( 'NONE',  ( 3.182267690267494231, 1.591318367894577701, 1.238320962759748234 ) ) ;
#165021 = CARTESIAN_POINT ( 'NONE',  ( -0.01142137120296871262, -0.4863542539808898280, -2.144715426241408984 ) ) ;
#165022 = CARTESIAN_POINT ( 'NONE',  ( 8.399998182892758791, 14.34039879828830522, -8.119840057749129869 ) ) ;
#165023 = CARTESIAN_POINT ( 'NONE',  ( -7.226659571283968297, 8.389856573708110332, 1.199719254218450271 ) ) ;
#165024 = CARTESIAN_POINT ( 'NONE',  ( 1.293514844328220281, -1.872496763586928514, 0.8835221827151735763 ) ) ;
#165025 = CARTESIAN_POINT ( 'NONE',  ( 4.222474775652216294, 7.013638773981186958, 1.199719254218462483 ) ) ;
#165026 = CARTESIAN_POINT ( 'NONE',  ( -1.360316468750002894, -0.3072916663252554526, 0.7853790794158901356 ) ) ;
#165027 = CARTESIAN_POINT ( 'NONE',  ( 3.580828998445852562, -1.422877522674294903, 1.572404880189558485 ) ) ;
#165028 = AXIS2_PLACEMENT_3D ( 'NONE', #207628, #176220, #175162 ) ;
#165029 = CARTESIAN_POINT ( 'NONE',  ( 0.6823417656249882723, -0.1572916663252488245, 1.181850606188755259 ) ) ;
#165030 = CARTESIAN_POINT ( 'NONE',  ( 5.549374350267230582, -1.441814640532925074, -1.119852386600270533 ) ) ;
#165031 = EDGE_LOOP ( 'NONE', ( #149413, #65798, #178396, #108935 ) ) ;
#165032 = CARTESIAN_POINT ( 'NONE',  ( -5.631432701629818460, 7.663367133358481631, 1.599625672291263179 ) ) ;
#165033 = CARTESIAN_POINT ( 'NONE',  ( 8.452618703115982512, 11.94880668935564216, 1.199719254218450271 ) ) ;
#165034 = CARTESIAN_POINT ( 'NONE',  ( 5.004368096775565711, 8.852530189631227842, -0.7216878364870458196 ) ) ;
#165035 = CARTESIAN_POINT ( 'NONE',  ( -3.474999999999998312, -2.727083332377418845, 2.006292185433951047 ) ) ;
#165036 = CARTESIAN_POINT ( 'NONE',  ( -4.882907879216086933, 8.848476292394087395, -0.7998128361456281477 ) ) ;
#165037 = CARTESIAN_POINT ( 'NONE',  ( 3.603775140268844712, 1.465814181579458753, 1.389848736882649094 ) ) ;
#165038 = CARTESIAN_POINT ( 'NONE',  ( 6.493228066955544442, 1.923254169853494178, -1.081975473724585690 ) ) ;
#165039 = CARTESIAN_POINT ( 'NONE',  ( -7.442499979258930587, 7.647614495415686164, -0.7998128361456362523 ) ) ;
#165040 = CARTESIAN_POINT ( 'NONE',  ( 9.836604141914616406, 11.43479190611061647, 1.199719254218452047 ) ) ;
#165041 = CARTESIAN_POINT ( 'NONE',  ( 5.682414339916787682, 1.109973489246698808, -1.493480506080862469 ) ) ;
#165042 = CARTESIAN_POINT ( 'NONE',  ( 8.372323551638698902, 9.726464550788689323, 1.199719254218462483 ) ) ;
#165043 = EDGE_CURVE ( 'NONE', #6976, #30182, #180298, .T. ) ;
#165044 = CARTESIAN_POINT ( 'NONE',  ( 11.87828357749917529, 13.80310252740378907, -1.708055325888794496 ) ) ;
#165046 = ORIENTED_EDGE ( 'NONE', *, *, #189556, .F. ) ;
#165045 = CARTESIAN_POINT ( 'NONE',  ( -3.602716132929368875, 5.226254793216122074, 1.599625672291267398 ) ) ;
#165047 = CARTESIAN_POINT ( 'NONE',  ( -5.859094939400033120, 9.987361195942037639, -0.7998128361456231517 ) ) ;
#165048 = CARTESIAN_POINT ( 'NONE',  ( 6.420785563114608685, 1.921975812937461781, 0.7442927364858693551 ) ) ;
#165050 = CARTESIAN_POINT ( 'NONE',  ( -4.797329538616279976, 6.965272035667838146, 1.434408638962878957 ) ) ;
#165049 = CARTESIAN_POINT ( 'NONE',  ( -7.435720902452096936, 7.639705572474380091, 0.000000000000000000 ) ) ;
#165051 = CARTESIAN_POINT ( 'NONE',  ( 1.364683531249988757, 0.3843750003414206362, 0.000000000000000000 ) ) ;
#165052 = CARTESIAN_POINT ( 'NONE',  ( 2.090756734626127766, 1.002568922338117563, -1.414341044747928766 ) ) ;
#165053 = CARTESIAN_POINT ( 'NONE',  ( 1.429236002152774576, 0.8600564655791165247, -1.512861638240108997 ) ) ;
#165055 = CARTESIAN_POINT ( 'NONE',  ( 7.632877294813741109, 8.007371053478589573, 1.040834085586084257E-14 ) ) ;
#165054 = CARTESIAN_POINT ( 'NONE',  ( 6.551428954101934821, -1.849038126066489207, -1.380618780084260644 ) ) ;
#165056 = CARTESIAN_POINT ( 'NONE',  ( 6.447401996410142999, 6.870587565654037832, 0.7192207954679635806 ) ) ;
#165057 = CARTESIAN_POINT ( 'NONE',  ( 2.179047869568909945, -0.09785464545388269930, -2.058565441667548068 ) ) ;
#165058 = CARTESIAN_POINT ( 'NONE',  ( 6.356075086708249167, 6.309842444114747373, -0.7998128361456281477 ) ) ;
#165059 = CARTESIAN_POINT ( 'NONE',  ( 0.9134352171796227271, 0.5825640498151598567, 1.930122961472901855 ) ) ;
#165060 = CARTESIAN_POINT ( 'NONE',  ( 9.277806814877628483, 13.85436241318128125, -7.538798676216699413 ) ) ;
#165061 = CARTESIAN_POINT ( 'NONE',  ( -5.448397627845328550, 7.449826213943242514, 1.599625672291263179 ) ) ;
#165062 = CARTESIAN_POINT ( 'NONE',  ( 6.543822781336226413, 0.7137633992815132222, -1.729328153040734506 ) ) ;
#165063 = VECTOR ( 'NONE', #189110, 1000.000000000000000 ) ;
#165066 = EDGE_CURVE ( 'NONE', #137099, #36083, #45319, .T. ) ;
#165065 = CARTESIAN_POINT ( 'NONE',  ( -6.075462232699549325, 9.141770800574526845, 1.082531754730549967 ) ) ;
#165064 = CARTESIAN_POINT ( 'NONE',  ( 4.974826827724895928, -1.381046924789817831, 1.323090558688621909 ) ) ;
#165067 = CARTESIAN_POINT ( 'NONE',  ( 6.410767893487317792, 1.638320036227768783, -1.478771730184471389 ) ) ;
#165068 = CARTESIAN_POINT ( 'NONE',  ( -6.495764994278840021, 8.671754808115688107, 1.443375672974064550 ) ) ;
#165069 = CARTESIAN_POINT ( 'NONE',  ( 5.677832469072920496, 9.846164657218904992, 0.000000000000000000 ) ) ;
#165070 = CARTESIAN_POINT ( 'NONE',  ( -5.935437387732586778, 10.14670372898850381, -0.7998128361456362523 ) ) ;
#165071 = CARTESIAN_POINT ( 'NONE',  ( 0.2760433103432077262, 1.997375541027920587, -0.2984889601853820129 ) ) ;
#165072 = ORIENTED_EDGE ( 'NONE', *, *, #128175, .F. ) ;
#165073 = CARTESIAN_POINT ( 'NONE',  ( -0.7500000000000179856, 12.82291666734946389, 1.299038105676658228 ) ) ;
#165074 = EDGE_CURVE ( 'NONE', #60029, #96467, #52852, .T. ) ;
#165075 = CARTESIAN_POINT ( 'NONE',  ( 5.016800025512162975, 1.595470874386342608, -1.667385368739245255 ) ) ;
#165076 = CARTESIAN_POINT ( 'NONE',  ( 4.879329150013382410, -0.09822140645733207220, 1.959542894978071992 ) ) ;
#165077 = CARTESIAN_POINT ( 'NONE',  ( 2.395295693335119935, -1.754585731169123752, 0.8775363634117984146 ) ) ;
#165078 = CARTESIAN_POINT ( 'NONE',  ( 9.642873567817520808, 12.27310513391906532, 1.599625672291279388 ) ) ;
#165079 = EDGE_LOOP ( 'NONE', ( #101798, #156309 ) ) ;
#165080 = CARTESIAN_POINT ( 'NONE',  ( 0.5150563930837145366, 0.1624822992478615336, 2.111197286521369065 ) ) ;
#165082 = CARTESIAN_POINT ( 'NONE',  ( -7.472515219426274946, 11.86968485597268064, 0.000000000000000000 ) ) ;
#165081 = CARTESIAN_POINT ( 'NONE',  ( -3.438964519360665051, 7.163875705896082913, -0.7998128361456281477 ) ) ;
#165083 = CARTESIAN_POINT ( 'NONE',  ( 0.6207436649305307919, -1.749090901066195691, 0.5750481222980761142 ) ) ;
#165084 = ORIENTED_EDGE ( 'NONE', *, *, #129354, .F. ) ;
#165085 = CARTESIAN_POINT ( 'NONE',  ( 4.364261492936694076, -2.165649721281979190, 0.1538544128360258556 ) ) ;
#165086 = CARTESIAN_POINT ( 'NONE',  ( 9.397879144821104092, 13.53129603721547447, -7.462055881301289162 ) ) ;
#165087 = CARTESIAN_POINT ( 'NONE',  ( 1.547299434221154124, 0.2130619955753136618, 2.109896976817266179 ) ) ;
#165088 = CARTESIAN_POINT ( 'NONE',  ( 1.499999999999989120, 2.535416667349483344, 0.8660254037844524744 ) ) ;
#165089 = CARTESIAN_POINT ( 'NONE',  ( 8.809047120577066181, 11.30030761213851953, 1.599625672291281386 ) ) ;
#165090 = CARTESIAN_POINT ( 'NONE',  ( -1.225000000000038058, 0.4791666666666983265, -0.7072540797573158011 ) ) ;
#165091 = CARTESIAN_POINT ( 'NONE',  ( 6.257994703896152089, 7.000112715747270009, 0.9732540237740094913 ) ) ;
#165092 = CARTESIAN_POINT ( 'NONE',  ( 2.003267984693514858, 1.711604303819891593, 1.147383568780909302 ) ) ;
#165093 = CARTESIAN_POINT ( 'NONE',  ( -7.828943636887387925, 11.22118577875556156, 1.199719254218453823 ) ) ;
#165094 = CARTESIAN_POINT ( 'NONE',  ( -1.201851678989727383E-14, 3.071875000341420137, 1.575800808251672791 ) ) ;
#165095 = CARTESIAN_POINT ( 'NONE',  ( 0.07735805125220260314, 1.351236195817316466, -2.344668200922094492 ) ) ;
#165096 = CARTESIAN_POINT ( 'NONE',  ( -4.905525160107071514, 6.476373528817366498, 2.499999999999998668 ) ) ;
#165097 = CARTESIAN_POINT ( 'NONE',  ( 6.006500814222540008, -1.903516144586704151, -0.1827706444143817055 ) ) ;
#165098 = CIRCLE ( 'NONE', #199709, 0.08000000000000020983 ) ;
#165099 = CARTESIAN_POINT ( 'NONE',  ( 11.89839339040395316, 12.27122531596078403, -1.560885614203536997 ) ) ;
#165100 = CARTESIAN_POINT ( 'NONE',  ( 1.985968398796404299, 1.559226912063184534, 1.639530705753606821 ) ) ;
#165101 = CARTESIAN_POINT ( 'NONE',  ( -3.765413976293358278, 5.416068943807445635, 1.599625672291267398 ) ) ;
#165102 = CARTESIAN_POINT ( 'NONE',  ( 1.564434226245875026, 0.5705330181091838870, 1.719429346978663897 ) ) ;
#165103 = CARTESIAN_POINT ( 'NONE',  ( 1.710024596074321002, 1.099767263899156244, -1.568400350156524459 ) ) ;
#165104 = CARTESIAN_POINT ( 'NONE',  ( 3.525891238081061640, 2.020528833579691597, -0.4508363271973143682 ) ) ;
#165105 = CARTESIAN_POINT ( 'NONE',  ( -1.402160292154681736E-14, 2.009375000341422801, -1.575800808251660134 ) ) ;
#165106 = CARTESIAN_POINT ( 'NONE',  ( 1.991034414115494089, 1.716142376821601534, -0.9701854037313780710 ) ) ;
#165107 = CARTESIAN_POINT ( 'NONE',  ( 5.145112535762402572, -1.651256390841379762, 0.9921342509419928124 ) ) ;
#165109 = CARTESIAN_POINT ( 'NONE',  ( 5.528015674651411970, 7.440572265265038787, -1.248273786418591103 ) ) ;
#165108 = CARTESIAN_POINT ( 'NONE',  ( 1.331197006551400497, 2.225188506942116895, 0.6113326355875832174 ) ) ;
#165110 = CARTESIAN_POINT ( 'NONE',  ( -1.364683531250014514, 1.738541667008085545, -0.7879004041258289570 ) ) ;
#165111 = CARTESIAN_POINT ( 'NONE',  ( 5.652800580869365099, -0.4976084531597444460, -2.001653870753268283 ) ) ;
#165112 = CARTESIAN_POINT ( 'NONE',  ( -6.196239896645333367, 7.187700286629718605, -1.199719254218446718 ) ) ;
#165113 = CARTESIAN_POINT ( 'NONE',  ( 6.317209508963599340, 9.457495962844502557, 1.199719254218462483 ) ) ;
#165114 = FACE_OUTER_BOUND ( 'NONE', #46754, .T. ) ;
#165116 = CARTESIAN_POINT ( 'NONE',  ( -1.500000000000011324, 4.920833333333354709, 0.8660254037844403729 ) ) ;
#165115 = CARTESIAN_POINT ( 'NONE',  ( 6.668975466350578252, -1.923848446808050783, -0.8571054451525415008 ) ) ;
#165117 = CARTESIAN_POINT ( 'NONE',  ( 0.6823417656249882723, 2.488541667008084435, -1.181850606188749264 ) ) ;
#165118 = CARTESIAN_POINT ( 'NONE',  ( 5.307972821619873827, -2.151738229465068653, 0.2060058040841972193 ) ) ;
#165119 = CARTESIAN_POINT ( 'NONE',  ( 5.356120063770971385, 0.8164924478912498618, -1.847455861782754782 ) ) ;
#165120 = DIRECTION ( 'NONE',  ( 0.000000000000000000, 1.000000000000000000, 0.000000000000000000 ) ) ;
#165121 = AXIS2_PLACEMENT_3D ( 'NONE', #31528, #29392, #78125 ) ;
#165122 = CARTESIAN_POINT ( 'NONE',  ( -5.639828713604883248, 6.642516923036197340, 1.082531754730548412 ) ) ;
#165125 = CARTESIAN_POINT ( 'NONE',  ( 5.260200412422194383, 7.159986452624450770, -1.443375672974051449 ) ) ;
#165124 = CARTESIAN_POINT ( 'NONE',  ( 3.285556943749998737, -2.005208332855377140, -1.896917185911906500 ) ) ;
#165123 = CARTESIAN_POINT ( 'NONE',  ( 7.550965208168244125, 7.774157262476569130, -0.7998128361456341429 ) ) ;
#165126 = CARTESIAN_POINT ( 'NONE',  ( -5.330290668828105538, 6.247702530834755130, 1.199719254218452935 ) ) ;
#165127 = CARTESIAN_POINT ( 'NONE',  ( 3.432827581131673522, -1.645759781613131967, 1.164986487700324425 ) ) ;
#165128 = CARTESIAN_POINT ( 'NONE',  ( -9.515124878692420296, 9.995400534762978850, 1.040834085586084257E-14 ) ) ;
#165130 = CARTESIAN_POINT ( 'NONE',  ( -10.99935770452674610, -5.294776013890323263, 0.1368885365587619307 ) ) ;
#165129 = CARTESIAN_POINT ( 'NONE',  ( -9.571693261567968847, 12.19006144329456731, 1.443375672974076540 ) ) ;
#165131 = CARTESIAN_POINT ( 'NONE',  ( 0.6823417656249917140, 5.342708333674749177, 1.181850606188765695 ) ) ;
#165133 = CARTESIAN_POINT ( 'NONE',  ( -11.94105721839855327, 12.57301656658875544, -1.187919402540362768 ) ) ;
#165132 = CARTESIAN_POINT ( 'NONE',  ( 4.557600102482579629, 0.4766696971462945909, -2.108333899287537339 ) ) ;
#165134 = FACE_OUTER_BOUND ( 'NONE', #208726, .T. ) ;
#165135 = CARTESIAN_POINT ( 'NONE',  ( -11.93214369018126142, 7.875338098606396109, -1.299425011414485187 ) ) ;
#165137 = CARTESIAN_POINT ( 'NONE',  ( 5.396111305808362957, -0.9091601233324579923, -1.799916296964368279 ) ) ;
#165136 = CARTESIAN_POINT ( 'NONE',  ( -6.629573926958124197, 9.717958100551031819, 1.082531754730548412 ) ) ;
#165138 = CARTESIAN_POINT ( 'NONE',  ( -1.364683531250014514, -0.4072916663252447167, 0.7879004041258379498 ) ) ;
#165139 = CARTESIAN_POINT ( 'NONE',  ( 1.154464490038846547, -1.361941861570209467, 1.058318063114448648 ) ) ;
#165140 = CARTESIAN_POINT ( 'NONE',  ( 5.574337433874081427, 6.532423756721743580, -1.199719254218452047 ) ) ;
#165142 = CARTESIAN_POINT ( 'NONE',  ( 6.180537922983273091, 8.303989891604203422, -1.599625672291281386 ) ) ;
#165141 = CARTESIAN_POINT ( 'NONE',  ( 6.968527767744088663, 11.07377346243604599, 0.7216878364870438212 ) ) ;
#165143 = CARTESIAN_POINT ( 'NONE',  ( -10.50000000000000000, 0.000000000000000000, 3.599999999999999201 ) ) ;
#165144 = CARTESIAN_POINT ( 'NONE',  ( 0.3503969169679886919, -1.426633182142377443, 1.047046497418676392 ) ) ;
#165145 = CARTESIAN_POINT ( 'NONE',  ( 0.7154901591317133214, 1.647040347281914396, 1.157252022262734714 ) ) ;
#165146 = CARTESIAN_POINT ( 'NONE',  ( 6.539320575229245591, 2.459069921018588900, 2.280790101157427419 ) ) ;
#165147 = CARTESIAN_POINT ( 'NONE',  ( 3.429849674132933846, 5.024577257953626308, -1.443375672974058777 ) ) ;
#165148 = CARTESIAN_POINT ( 'NONE',  ( -6.089020385868862739, 8.197219431637373432, -1.443375672974066548 ) ) ;
#165149 = VERTEX_POINT ( 'NONE', #20763 ) ;
#165150 = CARTESIAN_POINT ( 'NONE',  ( 7.904040366642678173, 12.16520482781775137, 0.7216878364870438212 ) ) ;
#165152 = CARTESIAN_POINT ( 'NONE',  ( 2.302361438560030393, 1.314982760645909465, -1.528754769246756240 ) ) ;
#165151 = CARTESIAN_POINT ( 'NONE',  ( 2.297662419472700002, 1.937625723843895864, -0.8618613456389671024 ) ) ;
#165153 = CARTESIAN_POINT ( 'NONE',  ( 2.197251250676080847, 1.655042475022786785, -0.7371099161151051238 ) ) ;
#165154 = CARTESIAN_POINT ( 'NONE',  ( 8.174640274396848483, 8.501778173076651512, 0.7998128361456291469 ) ) ;
#165155 = CARTESIAN_POINT ( 'NONE',  ( 6.227428301493934448, -2.037140905555033576, 0.7235935974677574212 ) ) ;
#165156 = CARTESIAN_POINT ( 'NONE',  ( 5.286789834324991055, 8.255339675766103724, -1.199719254218452935 ) ) ;
#165158 = CARTESIAN_POINT ( 'NONE',  ( 0.5322733027907312620, 0.5591794568308214863, 1.832249074504808783 ) ) ;
#165157 = CARTESIAN_POINT ( 'NONE',  ( -3.744022975668147790, 7.519777238254810925, -0.7998128361456281477 ) ) ;
#165159 = CARTESIAN_POINT ( 'NONE',  ( -15.75000000000000000, 13.40000000000000036, -1.400000000000001910 ) ) ;
#165160 = CARTESIAN_POINT ( 'NONE',  ( 6.141480396866128899, 6.267408005873028820, -0.7216878364870257245 ) ) ;
#165161 = CARTESIAN_POINT ( 'NONE',  ( -0.6823417656250003738, 0.2802083336747515641, -1.181850606188749264 ) ) ;
#165162 = CARTESIAN_POINT ( 'NONE',  ( -11.01135777277262129, 0.000000000000000000, -1.400000000000001910 ) ) ;
#165163 = CARTESIAN_POINT ( 'NONE',  ( -9.459838494033043332, 12.05956421450382088, 1.599625672291281386 ) ) ;
#165164 = CARTESIAN_POINT ( 'NONE',  ( 4.153314892778156242, -1.795761387672462961, -1.203114871582221079 ) ) ;
#165165 = CARTESIAN_POINT ( 'NONE',  ( -5.316205630334255972, 8.255971431148344308, -1.082531754730549967 ) ) ;
#165166 = CARTESIAN_POINT ( 'NONE',  ( 4.421367491832268293, 7.211993602896056288, 1.082531754730549078 ) ) ;
#165167 = CARTESIAN_POINT ( 'NONE',  ( 2.021885665735908333, -0.4598567139443253682, 2.069992740399699382 ) ) ;
#165168 = CARTESIAN_POINT ( 'NONE',  ( 6.440460073785046369, 1.806197173870389694, 0.2645596887278709453 ) ) ;
#165169 =( BOUNDED_SURFACE ( )  B_SPLINE_SURFACE ( 3, 3, ( 
 ( #185156, #56247, #139654, #3193, #69264, #85537, #37860, #201399, #153748, #71398 ),
 ( #73550, #184099, #54117, #151628, #135380, #40003, #55180, #203526, #53036, #19462 ),
 ( #120251, #121325, #202462, #169982, #152676, #86609, #187301, #168922, #172133, #38927 ),
 ( #20527, #119171, #36780, #171050, #21569, #102865, #138572, #51989, #4259, #7471 ),
 ( #70329, #105010, #101795, #6400, #103940, #22648, #118114, #136446, #88758, #106112 ),
 ( #87676, #5316, #154815, #23728, #204594, #122405, #188363, #89834, #155882, #35719 ),
 ( #8548, #95159, #94100, #193693, #160139, #45337, #208864, #127736, #174283, #190489 ) ),
 .UNSPECIFIED., .T., .F., .T. ) 
 B_SPLINE_SURFACE_WITH_KNOTS ( ( 4, 3, 4 ),
 ( 4, 1, 1, 1, 1, 1, 1, 4 ),
 ( 0.000000000000000000, 0.5000000000000000000, 1.000000000000000000 ),
 ( 0.000000000000000000, 0.09853459476447307130, 0.1926867929487333375, 0.2613852218134048999, 0.3629775382994345767, 0.5216635214973427415, 0.7338723600040717443, 1.000000000000000000 ),
 .UNSPECIFIED. ) 
 GEOMETRIC_REPRESENTATION_ITEM ( )  RATIONAL_B_SPLINE_SURFACE ( (
 ( 1.000000000000000000, 1.000000000000000000, 1.000000000000000222, 1.000000000000000000, 0.9999999999999997780, 1.000000000000000000, 0.9999999999999997780, 0.9999999999999997780, 1.000000000000000000, 1.000000000000000000),
 ( 0.3333333333333333703, 0.3333333333333333703, 0.3333333333333334259, 0.3333333333333333703, 0.3333333333333332593, 0.3333333333333334259, 0.3333333333333333148, 0.3333333333333333148, 0.3333333333333333703, 0.3333333333333333703),
 ( 0.3333333333333333703, 0.3333333333333333703, 0.3333333333333334259, 0.3333333333333333703, 0.3333333333333332593, 0.3333333333333334259, 0.3333333333333333148, 0.3333333333333333148, 0.3333333333333333703, 0.3333333333333333703),
 ( 1.000000000000000000, 1.000000000000000000, 1.000000000000000222, 1.000000000000000000, 0.9999999999999997780, 1.000000000000000000, 0.9999999999999997780, 0.9999999999999997780, 1.000000000000000000, 1.000000000000000000),
 ( 0.3333333333333333703, 0.3333333333333333703, 0.3333333333333334259, 0.3333333333333333703, 0.3333333333333332593, 0.3333333333333334259, 0.3333333333333333148, 0.3333333333333333148, 0.3333333333333333703, 0.3333333333333333703),
 ( 0.3333333333333333703, 0.3333333333333333703, 0.3333333333333334259, 0.3333333333333333703, 0.3333333333333332593, 0.3333333333333334259, 0.3333333333333333148, 0.3333333333333333148, 0.3333333333333333703, 0.3333333333333333703),
 ( 1.000000000000000000, 1.000000000000000000, 1.000000000000000222, 1.000000000000000000, 0.9999999999999997780, 1.000000000000000000, 0.9999999999999997780, 0.9999999999999997780, 1.000000000000000000, 1.000000000000000000) ) ) 
 REPRESENTATION_ITEM ( '' )  SURFACE ( )  );
#165170 = CARTESIAN_POINT ( 'NONE',  ( 3.848864690211077466, -1.613568265775822130, 1.132301161112803545 ) ) ;
#165171 = CARTESIAN_POINT ( 'NONE',  ( 5.748291730981218706, 0.9368611416523886515, -1.667099895225135686 ) ) ;
#165172 = ORIENTED_EDGE ( 'NONE', *, *, #174500, .F. ) ;
#165173 = CARTESIAN_POINT ( 'NONE',  ( 9.484513307599968357, -6.630981389236904278, -0.1588444833727744865 ) ) ;
#165174 = CARTESIAN_POINT ( 'NONE',  ( 6.566861343609567747, 1.460344857008318398, -1.321773145083295464 ) ) ;
#165175 = CARTESIAN_POINT ( 'NONE',  ( 1.939301023820143577, 0.7432367423349227620, -1.794281902191755540 ) ) ;
#165176 = ORIENTED_EDGE ( 'NONE', *, *, #80209, .T. ) ;
#165177 = CARTESIAN_POINT ( 'NONE',  ( -3.851398154733808088, 6.650992392901508232, -1.199719254218450271 ) ) ;
#165179 = CARTESIAN_POINT ( 'NONE',  ( 7.635176783151273128, 8.936736330878529699, 1.199719254218452935 ) ) ;
#165178 = CARTESIAN_POINT ( 'NONE',  ( -7.160114521792834807, 8.486460042580672436, 1.082531754730549078 ) ) ;
#165181 = CARTESIAN_POINT ( 'NONE',  ( 7.579171565239241737, 8.801120566655981747, 1.199719254218462483 ) ) ;
#165180 = CARTESIAN_POINT ( 'NONE',  ( 2.080132315211229876, -2.050506710900898977, -0.4067329413659624970 ) ) ;
#165183 = CARTESIAN_POINT ( 'NONE',  ( 5.695833931072550094, 5.817763472438987726, 0.000000000000000000 ) ) ;
#165182 = CARTESIAN_POINT ( 'NONE',  ( 6.982612806237943559, 8.105135347821125436, -1.199719254218446718 ) ) ;
#165185 = ORIENTED_EDGE ( 'NONE', *, *, #136789, .T. ) ;
#165184 = CARTESIAN_POINT ( 'NONE',  ( 5.777967262743825216, 1.883199444611630691, -0.3313529498064629597 ) ) ;
#165186 = CARTESIAN_POINT ( 'NONE',  ( 4.793709216081707858, 1.633822259641436903, 1.483752339651790653 ) ) ;
#165187 = EDGE_CURVE ( 'NONE', #195087, #157913, #54364, .T. ) ;
#165188 = CARTESIAN_POINT ( 'NONE',  ( 1.483733071427257411, 2.038639745401783721, -0.8453341458589253010 ) ) ;
#165189 = CARTESIAN_POINT ( 'NONE',  ( 0.8031952904608251620, 1.686239601473665140, -0.9019194118903075541 ) ) ;
#165190 = FACE_OUTER_BOUND ( 'NONE', #66367, .T. ) ;
#165191 = CARTESIAN_POINT ( 'NONE',  ( 11.41381676900473430, 13.53041960022391343, -3.704697931490291918 ) ) ;
#165192 = CARTESIAN_POINT ( 'NONE',  ( 3.754400092289136293, -2.067862582909282487, -0.1045053291982081939 ) ) ;
#165193 = CARTESIAN_POINT ( 'NONE',  ( -4.954615070790188369, 7.867802451642154082, -1.199719254218452047 ) ) ;
#165194 = AXIS2_PLACEMENT_3D ( 'NONE', #157494, #58910, #9088 ) ;
#165196 = CARTESIAN_POINT ( 'NONE',  ( 1.850665834824256173, 0.6780317805383448970, 2.052694239800388676 ) ) ;
#165195 = CARTESIAN_POINT ( 'NONE',  ( -4.627410500965859264, 4.293067094081919777, 0.7998128361456341429 ) ) ;
#165197 = CARTESIAN_POINT ( 'NONE',  ( 4.019203527901527018, -2.096847714747759106, 0.6372333828079318474 ) ) ;
#165198 = CARTESIAN_POINT ( 'NONE',  ( -6.158835246850665884E-15, 0.8125000000000031086, 1.224999999999960565 ) ) ;
#165199 = EDGE_CURVE ( 'NONE', #195013, #130986, #57830, .T. ) ;
#165200 = PRESENTATION_STYLE_ASSIGNMENT (( #19996 ) ) ;
#165201 = DIRECTION ( 'NONE',  ( -0.000000000000000000, -0.000000000000000000, 1.000000000000000000 ) ) ;
#165202 = CARTESIAN_POINT ( 'NONE',  ( -0.6823417656250039265, 14.63020833367473195, -1.181850606188755259 ) ) ;
#165203 = CARTESIAN_POINT ( 'NONE',  ( -5.679940009482361774, 5.591294530676332641, 0.7998128361456281477 ) ) ;
#165205 = EDGE_CURVE ( 'NONE', #56213, #91101, #37106, .T. ) ;
#165204 = UNCERTAINTY_MEASURE_WITH_UNIT (LENGTH_MEASURE( 1.000000000000000082E-05 ), #49154, 'distance_accuracy_value', 'NONE');
#165206 = CARTESIAN_POINT ( 'NONE',  ( 6.223290642006293893, 1.716731611696775683, 0.2442158411369663995 ) ) ;
#165207 = CARTESIAN_POINT ( 'NONE',  ( -9.653042183249970876, 11.32459930428888306, -1.082531754730539753 ) ) ;
#165208 = CARTESIAN_POINT ( 'NONE',  ( 4.399325512199628641, -1.803763729973751451, 1.015883459259236954 ) ) ;
#165209 = CARTESIAN_POINT ( 'NONE',  ( 5.782842150838196638, 1.730585719646136056, -1.219460781990765463 ) ) ;
#165210 = CARTESIAN_POINT ( 'NONE',  ( 6.823831386379729302, 6.855558127064808716, -0.7998128361456281477 ) ) ;
#165211 = CARTESIAN_POINT ( 'NONE',  ( -0.6823417656250212460, 5.551041667008087543, 1.181850606188767472 ) ) ;
#165212 = CARTESIAN_POINT ( 'NONE',  ( 3.080859285270169057, 1.852775266960526412, 0.6680929264101590492 ) ) ;
#165213 = CARTESIAN_POINT ( 'NONE',  ( 6.087847202767847854, -2.280615992951875448, -0.2307264670357595804 ) ) ;
#165214 = CARTESIAN_POINT ( 'NONE',  ( 2.596107596775329540, -1.820790993511243849, -0.1344670722737417168 ) ) ;
#165215 = CARTESIAN_POINT ( 'NONE',  ( 2.905190055078214595, 6.611415174225076186, 0.7998128361456271485 ) ) ;
#165216 = CARTESIAN_POINT ( 'NONE',  ( 3.945059511452237100, 6.586024615794168646, -1.082531754730548412 ) ) ;
#165217 = CARTESIAN_POINT ( 'NONE',  ( -7.555971681517696936, 7.709721804725773175, 0.7998128361456462443 ) ) ;
#165218 = CARTESIAN_POINT ( 'NONE',  ( 4.692003678781083487, 7.631698837623355658, -1.199719254218450271 ) ) ;
#165219 = ORIENTED_EDGE ( 'NONE', *, *, #97745, .F. ) ;
#165220 = CARTESIAN_POINT ( 'NONE',  ( 4.131111929362305091, 1.842322257054655354, 0.8120569753113301426 ) ) ;
#165221 = CARTESIAN_POINT ( 'NONE',  ( 4.926587646396720643, -1.284401507782207963, 1.482881906352449874 ) ) ;
#165222 = CARTESIAN_POINT ( 'NONE',  ( -6.368579470117215813, 8.453095353268645695, 1.599625672291283607 ) ) ;
#165223 = CARTESIAN_POINT ( 'NONE',  ( -3.588104209110990706, 7.337872010604796991, 1.040834085586084257E-14 ) ) ;
#165224 = SURFACE_SIDE_STYLE ('',( #111224 ) ) ;
#165226 = CARTESIAN_POINT ( 'NONE',  ( 5.418734442855144273, 1.636401904928608042, 0.6746929113052438920 ) ) ;
#165225 = CARTESIAN_POINT ( 'NONE',  ( 0.02900754732045561154, -1.909850462538491778, 0.8511534736125156986 ) ) ;
#165227 = FACE_OUTER_BOUND ( 'NONE', #131705, .T. ) ;
#165228 = CARTESIAN_POINT ( 'NONE',  ( 1.359612608069911133, 2.158557413232742750, -0.3773744582575569995 ) ) ;
#165229 = CARTESIAN_POINT ( 'NONE',  ( 0.8721245864499425071, -0.04093463707061052725, -1.740139661330299514 ) ) ;
#165230 = CARTESIAN_POINT ( 'NONE',  ( 7.298366762858032430, 7.409182732956175244, 1.040834085586084257E-14 ) ) ;
#165231 = CARTESIAN_POINT ( 'NONE',  ( 0.1333692844072316419, 7.629137130509075604, -2.653547345224521514 ) ) ;
#165232 = CARTESIAN_POINT ( 'NONE',  ( 0.4336905314940731060, 0.8911838752851186651, -1.476660275499335873 ) ) ;
#165233 = CARTESIAN_POINT ( 'NONE',  ( 0.5272844384777974902, 2.272924705895418285, -0.3403917945235325204 ) ) ;
#165234 = CARTESIAN_POINT ( 'NONE',  ( 0.6443834720083198020, 0.6415979653194536780, 2.095529601600601755 ) ) ;
#165235 = CARTESIAN_POINT ( 'NONE',  ( 2.807470779205251343, 1.864772411128329477, 1.179945617918669143 ) ) ;
#165236 = AXIS2_PLACEMENT_3D ( 'NONE', #95862, #178163, #114293 ) ;
#165237 = CARTESIAN_POINT ( 'NONE',  ( 1.446384731406271218, -0.9785283779201507937, 1.938150590114567473 ) ) ;
#165238 = CARTESIAN_POINT ( 'NONE',  ( -1.177073619093339962, 3.006928502340592058, 0.7750000000000152323 ) ) ;
#165239 = CARTESIAN_POINT ( 'NONE',  ( 1.868513053102664356, -2.077584836267523105, -0.4075993926472165074 ) ) ;
#165240 = CARTESIAN_POINT ( 'NONE',  ( 6.827182134110238110, -0.009824402486291110986, 2.288967694407703313 ) ) ;
#165241 = CARTESIAN_POINT ( 'NONE',  ( 5.790048612033079856, -0.8660258810785811390, 1.720834695440204509 ) ) ;
#165242 = ORIENTED_EDGE ( 'NONE', *, *, #48198, .F. ) ;
#165244 = CARTESIAN_POINT ( 'NONE',  ( 1.364683531249986537, 0.2177083336747502595, -0.7879004041258309554 ) ) ;
#165243 = CARTESIAN_POINT ( 'NONE',  ( 2.454944477651953783, -1.996203790030710801, -1.126857184891062236 ) ) ;
#165245 = CARTESIAN_POINT ( 'NONE',  ( 3.147464216666835402, 6.823792019419957278, -0.7998128361456291469 ) ) ;
#165246 = CARTESIAN_POINT ( 'NONE',  ( 6.166260936116925606, 6.088392601758203071, 0.7998128361456341429 ) ) ;
#165247 = STYLED_ITEM ( 'NONE', ( #181144 ), #152261 ) ;
#165248 = CARTESIAN_POINT ( 'NONE',  ( 5.074942145771424329, -1.609735135204511280, 1.530878986171863687 ) ) ;
#165249 = CARTESIAN_POINT ( 'NONE',  ( -8.188761592974051595, 9.616271948966963024, -1.082531754730543971 ) ) ;
#165250 = CARTESIAN_POINT ( 'NONE',  ( 5.495418255317095380, 6.026204583819558813, -0.7979391942483995415 ) ) ;
#165251 = CARTESIAN_POINT ( 'NONE',  ( 5.124618876285529367, 7.962177208099690873, -1.082531754730549078 ) ) ;
#165252 = CARTESIAN_POINT ( 'NONE',  ( -7.171900071504748730, 8.429933507252760805, -1.082531754730549078 ) ) ;
#165253 = CARTESIAN_POINT ( 'NONE',  ( 3.757017964762656703, 7.397288368949487491, -1.734723475976807094E-15 ) ) ;
#165254 = ORIENTED_EDGE ( 'NONE', *, *, #143150, .T. ) ;
#165255 = CARTESIAN_POINT ( 'NONE',  ( 2.690077459517980163, 1.704938782060089864, 1.076316768488336351 ) ) ;
#165257 = CARTESIAN_POINT ( 'NONE',  ( 1.411062195701995980, -1.628543573593312921, 1.265665014175233916 ) ) ;
#165256 = CARTESIAN_POINT ( 'NONE',  ( 5.913327553854682783, 10.05063257947248800, -0.7998128361456291469 ) ) ;
#165258 = DIRECTION ( 'NONE',  ( -0.05872483221476459958, 0.000000000000000000, 0.9982742078614211811 ) ) ;
#165259 = CARTESIAN_POINT ( 'NONE',  ( 5.533136087708556694, 5.627949321847663278, 0.000000000000000000 ) ) ;
#165260 = CARTESIAN_POINT ( 'NONE',  ( -7.214015694910790089, -7.024005795613424752, -7.869907041762409960 ) ) ;
#165261 = CARTESIAN_POINT ( 'NONE',  ( -1.201851678989727383E-14, 4.196875000341417028, -1.575800808251660134 ) ) ;
#165262 = CARTESIAN_POINT ( 'NONE',  ( 3.697391623616069101, -0.6365095100077067247, 2.096977347260075231 ) ) ;
#165263 = CARTESIAN_POINT ( 'NONE',  ( 1.512342498431101134, -1.897697209584522815, 0.6819976561535444626 ) ) ;
#165264 = CARTESIAN_POINT ( 'NONE',  ( 1.223879446662301307, 1.774596971308094018, 0.4907264878865265634 ) ) ;
#165265 = CARTESIAN_POINT ( 'NONE',  ( 4.259580805731934205, 0.8699401392010926992, 1.622648742527862620 ) ) ;
#165266 = EDGE_CURVE ( 'NONE', #109313, #150264, #60158, .T. ) ;
#165267 = CARTESIAN_POINT ( 'NONE',  ( 8.769426429940780920, 9.125419011219408461, 0.7998128361456462443 ) ) ;
#165268 = FILL_AREA_STYLE_COLOUR ( '', #96882 ) ;
#165269 = CARTESIAN_POINT ( 'NONE',  ( 4.717693524642503355, -1.790169364231732674, 0.3569235582787863570 ) ) ;
#165270 = CARTESIAN_POINT ( 'NONE',  ( 5.783827325522512552, 1.646840809264274119, -1.163266671679111353 ) ) ;
#165271 = CARTESIAN_POINT ( 'NONE',  ( -7.557780564614042795, 10.90482886110335414, -1.199719254218446718 ) ) ;
#165273 = CARTESIAN_POINT ( 'NONE',  ( -6.089547271193396227, 7.133501900260939443, -1.199719254218453823 ) ) ;
#165272 = CARTESIAN_POINT ( 'NONE',  ( 4.258826902089789535, -1.679047235397194804, 1.516690725115140692 ) ) ;
#165274 = CARTESIAN_POINT ( 'NONE',  ( 0.4519647057620000408, 0.6586765168765180700, -2.000488393216502292 ) ) ;
#165275 = CARTESIAN_POINT ( 'NONE',  ( -1.499999999999997780, 4.181250000682819490, 1.214306433183764966E-14 ) ) ;
#165276 = CARTESIAN_POINT ( 'NONE',  ( 4.193848433072798088, -1.425472641756184489, -1.501718461524886195 ) ) ;
#165277 = CARTESIAN_POINT ( 'NONE',  ( 10.21336978979620191, 10.81001959771741205, 0.7998128361456462443 ) ) ;
#165278 = CARTESIAN_POINT ( 'NONE',  ( 4.184706906422049677, 7.590773377626947038, -0.8858016570119742195 ) ) ;
#165279 = APPLICATION_PROTOCOL_DEFINITION ( 'draft international standard', 'automotive_design', 1998, #201209 ) ;
#165280 = CARTESIAN_POINT ( 'NONE',  ( -6.855619230004478482, 11.14997286831390788, -0.7998128361456291469 ) ) ;
#165281 = DIRECTION ( 'NONE',  ( 0.7592566023653005702, -0.6507913734559639396, 0.000000000000000000 ) ) ;
#165282 = CARTESIAN_POINT ( 'NONE',  ( 6.013923656113508542, 9.173938811177871244, -1.199719254218452047 ) ) ;
#165283 = CARTESIAN_POINT ( 'NONE',  ( 4.872649465673598357, 6.683545894502381124, -1.250567445346082218 ) ) ;
#165284 = CARTESIAN_POINT ( 'NONE',  ( -3.277320446201389181, 4.846626492033466072, 1.599625672291267398 ) ) ;
#165286 = CARTESIAN_POINT ( 'NONE',  ( 1.564984312397620814, 0.7026195195478746047, 2.107413697313319290 ) ) ;
#165285 = CARTESIAN_POINT ( 'NONE',  ( 0.2113915902133572944, 1.759560880827226947, -1.183302968686468226 ) ) ;
#165287 = CARTESIAN_POINT ( 'NONE',  ( -5.608757509019071996, 5.629766575911039794, 0.4613631940431175416 ) ) ;
#165288 = CARTESIAN_POINT ( 'NONE',  ( -7.774674742793745708, 8.035151719539642912, 0.7998128361456341429 ) ) ;
#165289 = CARTESIAN_POINT ( 'NONE',  ( 6.959412922516382771, 7.013736585890911535, 0.7998128361456341429 ) ) ;
#165290 = CARTESIAN_POINT ( 'NONE',  ( 2.857805160684105950, -0.6180756922911297968, 1.862011555624979886 ) ) ;
#165291 = CARTESIAN_POINT ( 'NONE',  ( 4.286349120214771879, 8.152491073559232859, -0.7998128361456221525 ) ) ;
#165292 = CARTESIAN_POINT ( 'NONE',  ( -4.044208510193211481, 7.583498396275582643, -0.3544512193057146598 ) ) ;
#165293 = CARTESIAN_POINT ( 'NONE',  ( 4.142179624174931796, 4.791296635414242111, 1.199719254218464037 ) ) ;
#165294 = CARTESIAN_POINT ( 'NONE',  ( -5.316205630334255972, 8.255971431148344308, -1.082531754730549967 ) ) ;
#165295 = CARTESIAN_POINT ( 'NONE',  ( -7.293923454472094114, 9.532663335016016148, 1.443375672974090751 ) ) ;
#165296 = CARTESIAN_POINT ( 'NONE',  ( 2.619513681940002670, 1.793805257907291395, 1.130712135851599465 ) ) ;
#165297 = CARTESIAN_POINT ( 'NONE',  ( -7.096767062110449942, 7.244259425409119046, -0.7998128361456362523 ) ) ;
#165298 = CARTESIAN_POINT ( 'NONE',  ( 4.369553226407375313, -0.3375162941181614751, 1.932460123137308861 ) ) ;
#165299 = CARTESIAN_POINT ( 'NONE',  ( 2.764712544972968811, -1.491509591961351910, 1.564943835847030229 ) ) ;
#165300 = CARTESIAN_POINT ( 'NONE',  ( 2.595044651933966495, -0.5755060336137384214, 1.749081985381637061 ) ) ;
#165301 = CARTESIAN_POINT ( 'NONE',  ( -4.218308198147158627, 7.356310275799033960, -0.8477421400144637964 ) ) ;
#165302 = CARTESIAN_POINT ( 'NONE',  ( -1.402160292154681736E-14, -0.7406249996585823059, -1.575800808251665908 ) ) ;
#165303 = CARTESIAN_POINT ( 'NONE',  ( 4.540767487494163035, -1.347652659646558115, -1.101159657664248170 ) ) ;
#165305 = AXIS2_PLACEMENT_3D ( 'NONE', #211439, #194131, #78250 ) ;
#165304 = CARTESIAN_POINT ( 'NONE',  ( -3.796053574490726223, 16.00000000000285993, -12.24940615670100463 ) ) ;
#165306 = CARTESIAN_POINT ( 'NONE',  ( 3.850152436600926542, 7.435668909435648288, -0.7216878364870197293 ) ) ;
#165307 =( NAMED_UNIT ( * ) SI_UNIT ( $, .STERADIAN. ) SOLID_ANGLE_UNIT ( ) );
#165308 = CARTESIAN_POINT ( 'NONE',  ( 2.167066695894452888, -1.976221826324360498, -0.8764929760368763700 ) ) ;
#165309 = CARTESIAN_POINT ( 'NONE',  ( 4.938827285099913311, 1.158512636183751665, 1.649828125244500843 ) ) ;
#165310 = CARTESIAN_POINT ( 'NONE',  ( -7.822691444960696572, 12.07029775252209092, -0.7216878364870267237 ) ) ;
#165311 = CARTESIAN_POINT ( 'NONE',  ( 1.340939272977889951, 0.4221563536682856332, 2.119910705745978508 ) ) ;
#165312 = CARTESIAN_POINT ( 'NONE',  ( 2.975414797803474176, 1.872564425654202225, -0.6168198417838985925 ) ) ;
#165313 = CARTESIAN_POINT ( 'NONE',  ( 3.163306973099208275, 0.2928498925126362673, -1.949387327701812334 ) ) ;
#165314 = CARTESIAN_POINT ( 'NONE',  ( 6.509000000000034980, 7.629137130509102249, 2.699999999999993516 ) ) ;
#165315 = CARTESIAN_POINT ( 'NONE',  ( 2.964326597902953608, -1.795398894311397209, -0.7408281928331180710 ) ) ;
#165319 = ORIENTED_EDGE ( 'NONE', *, *, #187677, .T. ) ;
#165318 = EDGE_CURVE ( 'NONE', #111999, #154266, #204842, .T. ) ;
#165317 = CARTESIAN_POINT ( 'NONE',  ( -4.095971805104331231, 5.871996087412059140, 1.443375672974065660 ) ) ;
#165316 = CARTESIAN_POINT ( 'NONE',  ( -9.612367721964613310, 11.27714576612263997, -1.082531754730537976 ) ) ;
#165320 = CARTESIAN_POINT ( 'NONE',  ( -5.908321080505254841, 10.11506803722328129, 0.7998128361456291469 ) ) ;
#165321 = CARTESIAN_POINT ( 'NONE',  ( 3.074666975249065626, 6.809138247757705820, 0.000000000000000000 ) ) ;
#165322 = CARTESIAN_POINT ( 'NONE',  ( -5.981082042284069367, 7.006959133200059142, 1.199719254218452935 ) ) ;
#165323 = CARTESIAN_POINT ( 'NONE',  ( -8.256552360598034213, 11.61609960646427986, 1.082531754730549967 ) ) ;
#165324 = EDGE_CURVE ( 'NONE', #189127, #133087, #48874, .T. ) ;
#165325 = CARTESIAN_POINT ( 'NONE',  ( 1.079469989902905214, -0.05558308599296066244, -2.206230565744627281 ) ) ;
#165326 = CARTESIAN_POINT ( 'NONE',  ( 3.285556943750000514, -3.463541666188707957, 1.896917185911906500 ) ) ;
#165327 = CARTESIAN_POINT ( 'NONE',  ( 5.260583753728677259, -0.6573284944802314511, -1.848511375219172415 ) ) ;
#165328 = ORIENTED_EDGE ( 'NONE', *, *, #158729, .T. ) ;
#165329 = CARTESIAN_POINT ( 'NONE',  ( 3.450509668567053545, -1.418736885945747428, 1.571922360790501738 ) ) ;
#165330 = CARTESIAN_POINT ( 'NONE',  ( 1.499999999999989120, 3.056250000682818158, 1.214306433183764966E-14 ) ) ;
#165331 = CARTESIAN_POINT ( 'NONE',  ( 0.07479286986305544449, 2.888457405263197941, -2.344396930208477947 ) ) ;
#165332 = CARTESIAN_POINT ( 'NONE',  ( 3.995923475689294513, -0.5793754966058572986, -1.747668199984537152 ) ) ;
#165333 = ORIENTED_EDGE ( 'NONE', *, *, #120212, .T. ) ;
#165334 = UNCERTAINTY_MEASURE_WITH_UNIT (LENGTH_MEASURE( 1.000000000000000082E-05 ), #158740, 'distance_accuracy_value', 'NONE');
#165335 = CARTESIAN_POINT ( 'NONE',  ( -9.158696461231359720, 10.64389961198009615, 1.199719254218462483 ) ) ;
#165336 = CARTESIAN_POINT ( 'NONE',  ( -5.273758566035884776, 5.255065869904374409, 0.000000000000000000 ) ) ;
#165337 = CARTESIAN_POINT ( 'NONE',  ( 5.045234882716379765, 0.1584239314957915090, 2.114765283346302205 ) ) ;
#165338 = CARTESIAN_POINT ( 'NONE',  ( 6.959412922516382771, 7.013736585890911535, 0.7998128361456341429 ) ) ;
#165339 = CARTESIAN_POINT ( 'NONE',  ( 5.782513925583750769, -2.009559558911724775, -0.4558285042701361589 ) ) ;
#165342 = CARTESIAN_POINT ( 'NONE',  ( 2.647807870277216757, 0.6224553824519338807, 1.732961026760751366 ) ) ;
#165341 = CARTESIAN_POINT ( 'NONE',  ( 0.5724163261710726314, 1.287614217418028506, -1.343956351914729952 ) ) ;
#165340 = CARTESIAN_POINT ( 'NONE',  ( -6.966220764712169000, 6.002124920821316323, -2.500000000000000444 ) ) ;
#165343 = CARTESIAN_POINT ( 'NONE',  ( 8.945682426918439845, 9.331051007693339727, 1.040834085586084257E-14 ) ) ;
#165344 = LINE ( 'NONE', #149093, #151994 ) ;
#165345 = CARTESIAN_POINT ( 'NONE',  ( -4.843110422882263677, 5.040344427663700166, -0.8886672019048741378 ) ) ;
#165346 = CARTESIAN_POINT ( 'NONE',  ( 5.085343294144600179, 4.914812813773358435, 0.1758235994440172922 ) ) ;
#165347 = AXIS2_PLACEMENT_3D ( 'NONE', #72761, #138860, #188653 ) ;
#165348 = CARTESIAN_POINT ( 'NONE',  ( 2.772332522587173997, 1.181257105606844160, 1.863944272329665086 ) ) ;
#165349 = CARTESIAN_POINT ( 'NONE',  ( 4.376441990627045087, -1.307286168679543614, 1.846302370218126265 ) ) ;
#165350 = CARTESIAN_POINT ( 'NONE',  ( 3.643767777461913493, 2.000731686840724333, -0.2516315899964287617 ) ) ;
#165351 = CARTESIAN_POINT ( 'NONE',  ( -7.700668062882084719, 8.086460282891644979, -0.7216878364870278340 ) ) ;
#165352 = CARTESIAN_POINT ( 'NONE',  ( 4.939644399817936460, -1.717766137778716118, 0.5755910463909068575 ) ) ;
#165353 = CARTESIAN_POINT ( 'NONE',  ( 5.208173988833650903, 1.135812200204017630, -1.542565181195413526 ) ) ;
#165354 = CARTESIAN_POINT ( 'NONE',  ( 4.979306205331720747, 1.745251617482036943, -0.6738592683939447214 ) ) ;
#165355 = CARTESIAN_POINT ( 'NONE',  ( 5.265987090187672415, -1.852092866064008803, 0.1821183643400964280 ) ) ;
#165356 = CARTESIAN_POINT ( 'NONE',  ( 0.6823417656249899377, 5.676041667008087543, -1.181850606188754593 ) ) ;
#165357 = EDGE_CURVE ( 'NONE', #173308, #193052, #53209, .T. ) ;
#165358 = CARTESIAN_POINT ( 'NONE',  ( 5.981276632755388789, 1.633781900041403334, -0.6810181619275444964 ) ) ;
#165360 = TOROIDAL_SURFACE ( 'NONE', #172176, 0.8299999999999998490, 0.08000000000000000167 ) ;
#165359 = PRESENTATION_LAYER_ASSIGNMENT (  '', '', ( #6243 ) ) ;
#165361 = CARTESIAN_POINT ( 'NONE',  ( 0.09298292169932984019, 1.756857073293972116, 0.9896806593640145033 ) ) ;
#165363 = CARTESIAN_POINT ( 'NONE',  ( 3.264387862500417903, 0.9470664325190655264, 1.881190857022313478 ) ) ;
#165362 = CARTESIAN_POINT ( 'NONE',  ( -2.453662613948990323, 5.806430783008362795, -0.7216878364870257245 ) ) ;
#165364 = CARTESIAN_POINT ( 'NONE',  ( 9.073431116043567002, 11.60875560684942265, -1.599625672291262513 ) ) ;
#165366 = CARTESIAN_POINT ( 'NONE',  ( 0.5101186646354113341, -1.387778780781445676E-14, 1.261047121698059215 ) ) ;
#165365 = CARTESIAN_POINT ( 'NONE',  ( 0.4019237886466814902, 11.85491455036742892, 1.499999999999999334 ) ) ;
#165367 = SURFACE_STYLE_USAGE ( .BOTH. , #112428 ) ;
#165368 = CARTESIAN_POINT ( 'NONE',  ( 1.898700399197379651, -1.981625571768164340, -0.3898374508689693152 ) ) ;
#165369 = CARTESIAN_POINT ( 'NONE',  ( 1.364683531249990311, 2.634375000341422801, 1.214306433183764966E-14 ) ) ;
#165370 = CARTESIAN_POINT ( 'NONE',  ( 4.844340958784499662, 4.546152628203684820, 0.7998128361456341429 ) ) ;
#165371 = EDGE_LOOP ( 'NONE', ( #208996, #117376, #187001, #6783, #24065, #212545 ) ) ;
#165372 = CARTESIAN_POINT ( 'NONE',  ( 2.214359598146302677, -1.016813397907929239, -1.907474440234189217 ) ) ;
#165373 = CARTESIAN_POINT ( 'NONE',  ( 6.609999999999968345, 7.051749200714771959, 2.878153929105996323 ) ) ;
#165376 = LINE ( 'NONE', #15907, #86376 ) ;
#165375 = CARTESIAN_POINT ( 'NONE',  ( -6.471393748265538370, 5.229711127717889596, -2.499999999999995115 ) ) ;
#165374 = CARTESIAN_POINT ( 'NONE',  ( 5.096939404094710468, 4.911127157724081371, 0.000000000000000000 ) ) ;
#165377 = CARTESIAN_POINT ( 'NONE',  ( 8.988692655735958326, 12.47026328412523988, -1.082531754730543083 ) ) ;
#165378 = FACE_OUTER_BOUND ( 'NONE', #61711, .T. ) ;
#165379 = CARTESIAN_POINT ( 'NONE',  ( -8.541273586929371220, 9.067166727613487964, 0.7216878364870438212 ) ) ;
#165380 = CARTESIAN_POINT ( 'NONE',  ( 0.7147126110796617748, 2.027027023440019171, 0.8336157706642086662 ) ) ;
#165381 = CARTESIAN_POINT ( 'NONE',  ( -3.890471347679111513, 5.946836461140907915, 1.325960742581899110 ) ) ;
#165382 = CARTESIAN_POINT ( 'NONE',  ( 1.991474686832030994, 1.968180706754483644, -1.115757519136374221 ) ) ;
#165383 = CARTESIAN_POINT ( 'NONE',  ( -8.681298431451969222, 9.022603012982438386, 1.040834085586084257E-14 ) ) ;
#165384 = CARTESIAN_POINT ( 'NONE',  ( -4.189106276498259618, 6.870745841681152655, 1.082531754730560403 ) ) ;
#165385 = CARTESIAN_POINT ( 'NONE',  ( -0.6823417656250212460, 3.613541667008085767, 1.181850606188767472 ) ) ;
#165386 = CARTESIAN_POINT ( 'NONE',  ( 4.720979226589129496, 8.219560628541461966, -0.6735110442024627719 ) ) ;
#165387 = CARTESIAN_POINT ( 'NONE',  ( -6.009258394948636914E-15, 10.93750000000000355, -1.732050807568875195 ) ) ;
#165388 = CARTESIAN_POINT ( 'NONE',  ( 4.309512724297349884, 6.121127159803966933, 1.599625672291261402 ) ) ;
#165389 = CARTESIAN_POINT ( 'NONE',  ( 3.549836697621409964, 1.769921775324476698, 0.002857994197370468913 ) ) ;
#165390 = CARTESIAN_POINT ( 'NONE',  ( 6.616270032800761314, -1.034323699838369359, -1.949367651511712207 ) ) ;
#165391 = CARTESIAN_POINT ( 'NONE',  ( 1.364683531249996529, 14.52604166700806232, 0.7879004041258405033 ) ) ;
#165392 = ORIENTED_EDGE ( 'NONE', *, *, #44272, .F. ) ;
#165393 = CARTESIAN_POINT ( 'NONE',  ( -4.936050443827081580, 7.916420063510339666, 1.199719254218452935 ) ) ;
#165394 = CARTESIAN_POINT ( 'NONE',  ( 5.044546077387519922, -1.458546410489666600, 1.392558106302365095 ) ) ;
#165396 = ORIENTED_EDGE ( 'NONE', *, *, #43069, .F. ) ;
#165395 = CARTESIAN_POINT ( 'NONE',  ( 4.834136970758627250, -0.9753174380719393799, -1.526440946957215994 ) ) ;
#165397 = COLOUR_RGB ( '', 0.31764706, 0.68627451, 0.89019608) ;
#165398 = CARTESIAN_POINT ( 'NONE',  ( 2.061206331123175861, 0.3224310286589862629, -1.842498087946140561 ) ) ;
#165399 = B_SPLINE_CURVE_WITH_KNOTS ( 'NONE', 3,
 ( #82413, #184177, #183118, #100797, #4336, #201476, #118188, #2202, #197231, #180987 ),
 .UNSPECIFIED., .F., .F.,
 ( 4, 2, 2, 2, 4 ),
 ( 0.001497391484644590995, 0.001840867574616280060, 0.002184343664587968907, 0.002527819754559657971, 0.002871295844531347036 ),
 .UNSPECIFIED. ) ;
#165400 = CARTESIAN_POINT ( 'NONE',  ( 3.766520095694513515, -0.8345382577515869649, -1.894767260282135490 ) ) ;
#165401 = CARTESIAN_POINT ( 'NONE',  ( -7.566859129758459979, 8.000626204239226880, 0.000000000000000000 ) ) ;
#165402 = CARTESIAN_POINT ( 'NONE',  ( 1.757924209179074770, 0.7287868685415777037, -1.768279316124596878 ) ) ;
#165403 = DIRECTION ( 'NONE',  ( 0.000000000000000000, -1.000000000000000000, 0.000000000000000000 ) ) ;
#165404 = CARTESIAN_POINT ( 'NONE',  ( -0.2024025116420367920, -4.140708350189159503, -0.9999999999999991118 ) ) ;
#165405 = CARTESIAN_POINT ( 'NONE',  ( -4.001001215408780176, 7.681935780300273464, 0.003373008766155432755 ) ) ;
#165406 = CARTESIAN_POINT ( 'NONE',  ( -1.364683531250010295, 4.092708333674751842, 0.7879004041258379498 ) ) ;
#165407 = CARTESIAN_POINT ( 'NONE',  ( 0.7910927259777954523, -0.04954035392716604758, -1.911929172785244102 ) ) ;
#165408 = B_SPLINE_CURVE_WITH_KNOTS ( 'NONE', 3,
 ( #179070, #97826, #95702, #79422, #30690, #211537, #162823, #93561, #142325, #63172, #59967 ),
 .UNSPECIFIED., .F., .F.,
 ( 4, 1, 1, 1, 1, 1, 1, 1, 4 ),
 ( 0.000000000000000000, 0.2254704865597413344, 0.3973194950497592193, 0.5246576192285303808, 0.6166070239209043846, 0.6823180413592140336, 0.7309932997181896042, 0.7717238569598857678, 1.000000000000000000 ),
 .UNSPECIFIED. ) ;
#165409 = CARTESIAN_POINT ( 'NONE',  ( 6.726253606155519371, 7.019919760035800316, -0.7216878364870458196 ) ) ;
#165410 = CARTESIAN_POINT ( 'NONE',  ( 2.734756269166933151, -1.876540383875524576, -0.5722209215143353456 ) ) ;
#165411 = CARTESIAN_POINT ( 'NONE',  ( 0.2806244687772480040, -1.977743564115455932, 0.3905345501400147024 ) ) ;
#165412 = CARTESIAN_POINT ( 'NONE',  ( -5.204350862799341115, 7.165104988056252289, -1.599625672291271394 ) ) ;
#165413 = CARTESIAN_POINT ( 'NONE',  ( 5.678019686890188211, 2.088907387943875982, -0.3644037002746222664 ) ) ;
#165415 = CARTESIAN_POINT ( 'NONE',  ( -2.279673327430177476, 5.603443282069742182, 1.040551764627347231E-14 ) ) ;
#165414 = CARTESIAN_POINT ( 'NONE',  ( 8.127223016387999266, 11.56917838817298616, 1.199719254218460707 ) ) ;
#165416 = CARTESIAN_POINT ( 'NONE',  ( 6.432890565879505473, 0.1910017811236862373, 1.962057160394870881 ) ) ;
#165417 = CARTESIAN_POINT ( 'NONE',  ( -0.6823417656250212460, 2.051041667008083991, 1.181850606188767472 ) ) ;
#165418 = CARTESIAN_POINT ( 'NONE',  ( 1.986589674187682064, -1.235133946311824049, 1.589746892572386994 ) ) ;
#165420 = CARTESIAN_POINT ( 'NONE',  ( 1.476322311366547124, -2.107388574805735271, -0.2037450385454323831 ) ) ;
#165419 = CARTESIAN_POINT ( 'NONE',  ( -5.572037945536512105, 9.444535336527177805, 0.000000000000000000 ) ) ;
#165421 = CARTESIAN_POINT ( 'NONE',  ( 9.281915779689660084, 11.43972118546268213, -7.608961053593318979 ) ) ;
#165422 = CARTESIAN_POINT ( 'NONE',  ( 2.770052221688572125, -2.048192801557855436, 0.3012726569043902569 ) ) ;
#165423 = CARTESIAN_POINT ( 'NONE',  ( 4.115782150200256950, 6.959440387612411349, 1.199719254218452047 ) ) ;
#165425 = CARTESIAN_POINT ( 'NONE',  ( 3.005103603723342953, 6.657704637652544832, -0.7998128361456291469 ) ) ;
#165424 = CARTESIAN_POINT ( 'NONE',  ( 6.158164957586691912, -1.479299979846586455, 1.477571280793017694 ) ) ;
#165427 = ORIENTED_EDGE ( 'NONE', *, *, #69515, .F. ) ;
#165426 = CARTESIAN_POINT ( 'NONE',  ( 4.295794115256676982, -0.6985059363485807138, 1.686860163339451990 ) ) ;
#165428 = CARTESIAN_POINT ( 'NONE',  ( 8.432281472695482449, 11.92507992053172572, 1.199719254218450271 ) ) ;
#165429 = CIRCLE ( 'NONE', #134397, 2.600000000000008082 ) ;
#165430 = CARTESIAN_POINT ( 'NONE',  ( 6.890000000000005898, 2.048573291599069091, 2.305811639209849773 ) ) ;
#165431 = CARTESIAN_POINT ( 'NONE',  ( 10.78928497238454476, 8.180547903054934622, -2.738679714801448561 ) ) ;
#165432 = CARTESIAN_POINT ( 'NONE',  ( 5.016741729952475914, 1.524926965779101140, -1.595359541877178877 ) ) ;
#165433 = CARTESIAN_POINT ( 'NONE',  ( 1.364683531249997417, 11.04687500034139802, 2.602085213965210642E-15 ) ) ;
#165434 = ORIENTED_EDGE ( 'NONE', *, *, #74132, .F. ) ;
#165435 = CARTESIAN_POINT ( 'NONE',  ( 4.248624793116656306, 1.876006594227698221, 0.3698101955103145211 ) ) ;
#165436 = CARTESIAN_POINT ( 'NONE',  ( -2.123823618835070537, 5.629544655282869847, 1.040834085586084257E-14 ) ) ;
#165437 = CARTESIAN_POINT ( 'NONE',  ( 6.825640269476072497, 10.05066518344239412, 1.199719254218460707 ) ) ;
#165438 = CARTESIAN_POINT ( 'NONE',  ( 1.360316468749957597, 1.776041667008106506, 0.7853790794158801436 ) ) ;
#165439 = CARTESIAN_POINT ( 'NONE',  ( 3.999292125906894313, 7.609665213625947722, 0.7216878364870317197 ) ) ;
#165440 = CARTESIAN_POINT ( 'NONE',  ( 6.391719935120313778, 6.567462711928209629, -2.438448603877958476 ) ) ;
#165441 = CARTESIAN_POINT ( 'NONE',  ( 7.872831621983168660, 14.31746563593600285, -9.057160014918840929 ) ) ;
#165442 = CARTESIAN_POINT ( 'NONE',  ( 0.01093749962182561340, -1.805946196879630872, 0.3578947576599255109 ) ) ;
#165443 = CIRCLE ( 'NONE', #68640, 1.240450515248286534 ) ;
#165444 = ADVANCED_FACE ( 'NONE', ( #74876 ), #42398, .F. ) ;
#165445 = DIRECTION ( 'NONE',  ( 0.000000000000000000, 0.000000000000000000, -1.000000000000000000 ) ) ;
#165446 = CARTESIAN_POINT ( 'NONE',  ( 4.833189656263336964, -1.710893631887340005, 0.7565425265826586365 ) ) ;
#165447 = CARTESIAN_POINT ( 'NONE',  ( -2.788906526875773208E-15, 10.93750000000000178, -1.499999999999998446 ) ) ;
#165448 = DIRECTION ( 'NONE',  ( -0.6250000000000002220, 1.408756634010579298E-16, -0.7806247497997996776 ) ) ;
#165449 = CARTESIAN_POINT ( 'NONE',  ( -6.060131475628484310, 10.01397778830115470, 0.000000000000000000 ) ) ;
#165450 = CARTESIAN_POINT ( 'NONE',  ( 5.522248639467795428, 5.337044922334209573, -0.7998128361456231517 ) ) ;
#165451 = CARTESIAN_POINT ( 'NONE',  ( 1.516386633922983895, 0.7932475597272764523, 1.802804710252394527 ) ) ;
#165452 = CARTESIAN_POINT ( 'NONE',  ( 1.933220473845993492, -1.621196910160098925, -1.198842755339262212 ) ) ;
#165453 = CARTESIAN_POINT ( 'NONE',  ( -9.182950115157607840, 9.607863310639020327, 0.7998128361456462443 ) ) ;
#165454 = CARTESIAN_POINT ( 'NONE',  ( 4.993145711582793744, 9.047363440147082159, -0.7998128361456481317 ) ) ;
#165455 = SURFACE_STYLE_USAGE ( .BOTH. , #181691 ) ;
#165456 = CARTESIAN_POINT ( 'NONE',  ( 3.011879173929287834, -1.080601074572758558, -1.906429682232862799 ) ) ;
#165457 = CARTESIAN_POINT ( 'NONE',  ( 6.568987803155795113, -1.671525225137669102, -0.7347104647430282576 ) ) ;
#165458 = CARTESIAN_POINT ( 'NONE',  ( -3.164938793786285842, 5.779846795137578930, -1.199719254218452935 ) ) ;
#165459 = CARTESIAN_POINT ( 'NONE',  ( 6.825078400183548055, 2.461594334264828987, 2.239602747093616841 ) ) ;
#165460 = CARTESIAN_POINT ( 'NONE',  ( 10.43434622977930637, 1.529612873802629336, -5.577395135400672110 ) ) ;
#165461 = CARTESIAN_POINT ( 'NONE',  ( 5.560252395380222090, 5.659585014131299552, 0.7216878364870328300 ) ) ;
#165462 = CARTESIAN_POINT ( 'NONE',  ( 8.127223016387999266, 11.56917838817298616, 1.199719254218460707 ) ) ;
#165463 = EDGE_CURVE ( 'NONE', #42674, #199393, #211353, .T. ) ;
#165464 = CARTESIAN_POINT ( 'NONE',  ( -1.387358672533697046, 7.315968950353781253, -4.254625267138305134 ) ) ;
#165465 = CARTESIAN_POINT ( 'NONE',  ( 7.363486825997814123, 7.763358516518489516, 0.000000000000000000 ) ) ;
#165466 = EDGE_LOOP ( 'NONE', ( #128053, #127819, #158267, #101467 ) ) ;
#165468 = CARTESIAN_POINT ( 'NONE',  ( 1.084635982312625924, -1.275300252541565538, 1.557628696486039077 ) ) ;
#165467 = CARTESIAN_POINT ( 'NONE',  ( 4.810013364240863787, 1.265987717737980134, -1.337210144835267345 ) ) ;
#165469 = CARTESIAN_POINT ( 'NONE',  ( 2.970384050378202634, 1.940355284992447027, 1.231690374697077095 ) ) ;
#165471 = CARTESIAN_POINT ( 'NONE',  ( 1.234942694251008000, -0.03850059531256519452, -1.860717468297488297 ) ) ;
#165470 = CARTESIAN_POINT ( 'NONE',  ( 3.226477370372305753, 4.787309570232886280, 1.443375672974062551 ) ) ;
#165473 = CARTESIAN_POINT ( 'NONE',  ( -3.285556943750000070, -3.609374999522043659, 0.000000000000000000 ) ) ;
#165472 =( REPRESENTATION_RELATIONSHIP ('NONE','NONE', #84563, #149737 ) REPRESENTATION_RELATIONSHIP_WITH_TRANSFORMATION ( #93660 )SHAPE_REPRESENTATION_RELATIONSHIP( ) );
#165474 = CARTESIAN_POINT ( 'NONE',  ( -5.278201874421821316, 5.052323696447222900, 0.7998128361456341429 ) ) ;
#165475 = CARTESIAN_POINT ( 'NONE',  ( 4.148624843374196125, 1.876505540506741010, 0.3678670841067502861 ) ) ;
#165476 = CARTESIAN_POINT ( 'NONE',  ( -8.076906825439122528, 10.44614393447756129, -1.599625672291263179 ) ) ;
#165477 = CARTESIAN_POINT ( 'NONE',  ( -6.617788377246196951, 7.853746207276256719, -1.082531754730549967 ) ) ;
#165479 = CARTESIAN_POINT ( 'NONE',  ( 2.817106861211693847, -0.1851908181382568019, 1.861470920997858380 ) ) ;
#165478 = CARTESIAN_POINT ( 'NONE',  ( 4.054300615058183510, -1.547851416709244310, 1.405648825684354897 ) ) ;
#165480 = CARTESIAN_POINT ( 'NONE',  ( 7.537970219518073556, 9.817384560903001045, -1.443375672974057666 ) ) ;
#165481 = CARTESIAN_POINT ( 'NONE',  ( -0.6823417656250212460, 5.613541667008087543, 1.181850606188767472 ) ) ;
#165482 = CARTESIAN_POINT ( 'NONE',  ( 5.935073298327618652, -1.338256116417003927, -1.264887592264056559 ) ) ;
#165483 = CARTESIAN_POINT ( 'NONE',  ( 3.440018289565364817, 5.036440642624797626, 1.599625672291267398 ) ) ;
#165484 = CARTESIAN_POINT ( 'NONE',  ( 5.712296854416149650, 6.230208010187211265, -1.006048757959861151 ) ) ;
#165485 = CARTESIAN_POINT ( 'NONE',  ( 4.512129967005336084, -0.7409026826630369378, -1.557792038885176700 ) ) ;
#165486 = CARTESIAN_POINT ( 'NONE',  ( -7.063961727919978451, 8.200042423116789436, 1.199719254218450271 ) ) ;
#165487 = CARTESIAN_POINT ( 'NONE',  ( 0.2989044949552251418, 1.198067244415670141, -1.254020425504979164 ) ) ;
#165488 = CARTESIAN_POINT ( 'NONE',  ( 0.000000000000000000, 12.21999999999998288, 0.000000000000000000 ) ) ;
#165489 = CARTESIAN_POINT ( 'NONE',  ( 1.403499169902377552, 7.376709478543040710, 4.304123474984470121 ) ) ;
#165490 = AXIS2_PLACEMENT_3D ( 'NONE', #115996, #181984, #99686 ) ;
#165491 = FILL_AREA_STYLE ('',( #99436 ) ) ;
#165492 = CARTESIAN_POINT ( 'NONE',  ( 4.592743594998466072, 2.127975290613278503, 0.4296678846467619772 ) ) ;
#165493 = CARTESIAN_POINT ( 'NONE',  ( 2.965264444195826243, 0.2674972279559268973, -1.805858685475017378 ) ) ;
#165494 = CARTESIAN_POINT ( 'NONE',  ( 0.5671465430379521999, 1.703994235754960451, 0.9719838849941149217 ) ) ;
#165495 = CARTESIAN_POINT ( 'NONE',  ( 5.981681833671104620, -0.7110503908294771858, 1.994531755910114112 ) ) ;
#165496 = B_SPLINE_CURVE_WITH_KNOTS ( 'NONE', 3,
 ( #214276, #213241, #166649, #47590, #197008, #200188, #97402, #15037, #81129, #131016 ),
 .UNSPECIFIED., .F., .F.,
 ( 4, 3, 3, 4 ),
 ( 3.001204002259073297E-18, 8.735586674212287715E-05, 0.0001834092658857657617, 0.0002312911391078497833 ),
 .UNSPECIFIED. ) ;
#165497 = EDGE_LOOP ( 'NONE', ( #93159, #1722, #176263, #9228, #112141 ) ) ;
#165499 = CARTESIAN_POINT ( 'NONE',  ( 1.364683531249988535, 3.717708333674750953, -0.7879004041258239610 ) ) ;
#165498 = CARTESIAN_POINT ( 'NONE',  ( 5.583585467610721054, -1.033564708330332316, 2.046191781174087509 ) ) ;
#165500 = CARTESIAN_POINT ( 'NONE',  ( 8.378048858240820351, 11.86180853700128601, -1.199719254218446718 ) ) ;
#165501 = CARTESIAN_POINT ( 'NONE',  ( 1.752743329737327826, 2.097873456429504735, 0.3079802404963859486 ) ) ;
#165502 = CARTESIAN_POINT ( 'NONE',  ( -4.284013352238255301, 6.981470763377843447, -1.082531754730549967 ) ) ;
#165503 = CYLINDRICAL_SURFACE ( 'NONE', #108410, 0.04999999999999991257 ) ;
#165504 = CARTESIAN_POINT ( 'NONE',  ( -4.324687812634898876, 6.068555086205916105, 1.443375672974064550 ) ) ;
#165505 = AXIS2_PLACEMENT_3D ( 'NONE', #67971, #87473, #204381 ) ;
#165506 = CARTESIAN_POINT ( 'NONE',  ( 6.772352023501587936, -1.015705593385501482, -1.918810339808636023 ) ) ;
#165508 = CARTESIAN_POINT ( 'NONE',  ( 1.499999999999993117, 12.63541666734946389, 0.8660254037844409281 ) ) ;
#165507 = CARTESIAN_POINT ( 'NONE',  ( 6.883263157960330503, 7.629137130509037412, 2.753810918356710769 ) ) ;
#165510 = ORIENTED_EDGE ( 'NONE', *, *, #21017, .T. ) ;
#165509 = CARTESIAN_POINT ( 'NONE',  ( 1.805654246593148660, 1.930672025830199479, -1.098395813934008425 ) ) ;
#165511 = CARTESIAN_POINT ( 'NONE',  ( 6.451795992440088057, -1.844709169062180409, -0.8146298745319994206 ) ) ;
#165513 = CARTESIAN_POINT ( 'NONE',  ( 4.487212223095434105, 0.09620561770018636050, 2.060423205476647812 ) ) ;
#165512 = CARTESIAN_POINT ( 'NONE',  ( 4.009460741339333723, 5.700790169694431420, -1.599625672291256295 ) ) ;
#165515 = CARTESIAN_POINT ( 'NONE',  ( -1.737499999999997824, -3.091666666666666341, 3.009438278150925683 ) ) ;
#165514 = CARTESIAN_POINT ( 'NONE',  ( 6.866278450678116485, 6.975356045404744521, 0.000000000000000000 ) ) ;
#165516 = CARTESIAN_POINT ( 'NONE',  ( 4.389807875774629942, 8.343469298370917997, 0.7998128361456271485 ) ) ;
#165517 = CARTESIAN_POINT ( 'NONE',  ( -3.285556943750000514, -4.076041666188709556, -1.896917185911906500 ) ) ;
#165518 = FILL_AREA_STYLE_COLOUR ( '', #172084 ) ;
#165519 = CARTESIAN_POINT ( 'NONE',  ( 0.2520486530714799445, 0.8021226228236020273, 1.930841216200715360 ) ) ;
#165520 = CARTESIAN_POINT ( 'NONE',  ( 4.089279031174639201, -0.7008038172400687937, 1.702867937621636463 ) ) ;
#165521 = ADVANCED_FACE ( 'NONE', ( #189679 ), #98775, .T. ) ;
#165522 = CARTESIAN_POINT ( 'NONE',  ( 5.250031796989762967, 7.148123067953287446, 1.599625672291267398 ) ) ;
#165523 = SHAPE_REPRESENTATION_RELATIONSHIP ( 'NONE' , 'NONE' ,  #47273, #88981 ) ;
#165524 = CARTESIAN_POINT ( 'NONE',  ( 2.361930338997704659, 0.7344707938763440636, 1.560707491107244715 ) ) ;
#165525 = CARTESIAN_POINT ( 'NONE',  ( 0.5675926644314840397, 1.357872185771633156, 1.490966652548594285 ) ) ;
#165526 = CARTESIAN_POINT ( 'NONE',  ( 1.565480925793379274, -1.225038264044479686, 1.944918359529357543 ) ) ;
#165527 = CARTESIAN_POINT ( 'NONE',  ( -5.819474248763749635, 7.812472595022922128, -1.599625672291256295 ) ) ;
#165528 = CARTESIAN_POINT ( 'NONE',  ( 1.810245590833154283, -2.245401999695510575, 0.2761584955175334644 ) ) ;
#165529 = CARTESIAN_POINT ( 'NONE',  ( 4.424511703531566198, 1.296206220603330461, -1.659847191385990239 ) ) ;
#165530 = CARTESIAN_POINT ( 'NONE',  ( -7.946487431385463651, 8.443525889470736345, 0.7216878364870317197 ) ) ;
#165531 = CARTESIAN_POINT ( 'NONE',  ( 2.565387841970759197, 1.736461783412158955, -0.3405875811831828859 ) ) ;
#165532 = CARTESIAN_POINT ( 'NONE',  ( 5.289652487626049115, 9.323011668872403845, 0.7998128361456462443 ) ) ;
#165533 = CARTESIAN_POINT ( 'NONE',  ( 5.736508391913541338, 6.825586224388162648, -1.082531754730548412 ) ) ;
#165534 = CARTESIAN_POINT ( 'NONE',  ( 6.031250000000003553, -0.7852924748303007352, -1.895863743163946680 ) ) ;
#165535 = CARTESIAN_POINT ( 'NONE',  ( -4.726989112658928072, 8.666571064744069020, 1.040834085586084257E-14 ) ) ;
#165536 = CARTESIAN_POINT ( 'NONE',  ( -1.500000000000013101, 2.379166666666686414, -0.8660254037844313801 ) ) ;
#165537 = CARTESIAN_POINT ( 'NONE',  ( -3.815730167242251003, 6.539103397502874948, -1.199719254218452047 ) ) ;
#165538 = CARTESIAN_POINT ( 'NONE',  ( 5.045291550738682851, 0.1642389012704112972, 2.215424048113129540 ) ) ;
#165539 = CARTESIAN_POINT ( 'NONE',  ( 3.064592470464472029, -2.024993410009158890, -0.8382372354380845936 ) ) ;
#165540 = CARTESIAN_POINT ( 'NONE',  ( -5.925076824372040640, 6.871343368977510302, 1.199719254218450271 ) ) ;
#165541 = CARTESIAN_POINT ( 'NONE',  ( -3.298376509874564988, 7.070132704820777825, 0.000000000000000000 ) ) ;
#165542 = CARTESIAN_POINT ( 'NONE',  ( 5.813165546740090228, 1.733599321496303691, -1.220823391460408303 ) ) ;
#165543 = CARTESIAN_POINT ( 'NONE',  ( -1.201851678989727383E-14, 3.696875000341422801, -1.575800808251660134 ) ) ;
#165544 = CARTESIAN_POINT ( 'NONE',  ( 6.610000000000011866, 2.967812824040619191, 2.453181572820534395 ) ) ;
#165545 = CARTESIAN_POINT ( 'NONE',  ( -5.422898255786203769, 6.389431388914436738, -1.082531754730544860 ) ) ;
#165546 = CARTESIAN_POINT ( 'NONE',  ( 5.291314375706784645, -0.05428322906628547939, -2.120082430678168706 ) ) ;
#165547 = CARTESIAN_POINT ( 'NONE',  ( -7.295696057929500711, 7.684269287105433222, 0.7216878364870317197 ) ) ;
#165548 = EDGE_LOOP ( 'NONE', ( #126866, #152794, #6920, #45877 ) ) ;
#165550 = CARTESIAN_POINT ( 'NONE',  ( 6.631704542599726082, -1.407888343591977121, -1.640466528430361670 ) ) ;
#165549 = CARTESIAN_POINT ( 'NONE',  ( -5.207740401424942434, 6.208690235484773723, 1.082531754730549078 ) ) ;
#165551 = CARTESIAN_POINT ( 'NONE',  ( 4.656335691289526402, 7.519809842224722374, -1.199719254218452047 ) ) ;
#165552 = CARTESIAN_POINT ( 'NONE',  ( 5.741722636381444644, 1.839460222191912742, 0.08393339073512616488 ) ) ;
#165553 = DIRECTION ( 'NONE',  ( 1.000000000000000000, 0.000000000000000000, -3.491481338843133355E-15 ) ) ;
#165554 = CARTESIAN_POINT ( 'NONE',  ( 1.364683531249988535, 2.676041667008082214, 0.7879004041258500513 ) ) ;
#165555 = CARTESIAN_POINT ( 'NONE',  ( 0.9951963871240524506, -1.740626720728695620, -0.001451476259923395245 ) ) ;
#165556 = CARTESIAN_POINT ( 'NONE',  ( 3.440018289565364817, 5.036440642624797626, 1.599625672291267398 ) ) ;
#165557 = CARTESIAN_POINT ( 'NONE',  ( -3.285556943750000070, -0.1531249995220425320, 0.000000000000000000 ) ) ;
#165558 = CARTESIAN_POINT ( 'NONE',  ( -0.6823417656250003738, 0.03020833367475134201, -1.181850606188749264 ) ) ;
#165559 =( NAMED_UNIT ( * ) PLANE_ANGLE_UNIT ( ) SI_UNIT ( $, .RADIAN. ) );
#165560 = CARTESIAN_POINT ( 'NONE',  ( 5.067319851952804655, 0.2155487944876262052, -2.150937003660175595 ) ) ;
#165561 = CARTESIAN_POINT ( 'NONE',  ( -2.272963308585411735, 5.803540959991587478, 0.7998128361456341429 ) ) ;
#165562 = CARTESIAN_POINT ( 'NONE',  ( -5.490689023410187275, 8.389259046411751797, 1.082531754730548412 ) ) ;
#165563 = CARTESIAN_POINT ( 'NONE',  ( 4.961884481312108797, 2.138711985806662330, -0.3135959325617638238 ) ) ;
#165565 = ORIENTED_EDGE ( 'NONE', *, *, #69142, .T. ) ;
#165564 = CARTESIAN_POINT ( 'NONE',  ( -11.04536101718726293, 0.000000000000000000, -1.100000000000002087 ) ) ;
#165566 = CARTESIAN_POINT ( 'NONE',  ( 1.364683531249986537, 2.655208333674754062, -0.7879004041258239610 ) ) ;
#165567 = CARTESIAN_POINT ( 'NONE',  ( 5.466080325957246799, 0.9693943247218398396, 1.716448534147915650 ) ) ;
#165568 = CARTESIAN_POINT ( 'NONE',  ( 5.184772435558752335, -0.9287019638352255191, -1.463892056132688024 ) ) ;
#165570 = CARTESIAN_POINT ( 'NONE',  ( 1.611130907606239004, -0.2639259086049255965, 2.175532687872412829 ) ) ;
#165569 = CARTESIAN_POINT ( 'NONE',  ( -7.561650146977034455E-14, -0.5468749996585524631, 1.570758158831754070 ) ) ;
#165571 = CARTESIAN_POINT ( 'NONE',  ( 1.677271382912606246, -2.191714306423699021, -0.7221938283701042627 ) ) ;
#165572 = CARTESIAN_POINT ( 'NONE',  ( 4.886040457987857799, -0.9749269275126177803, 1.815604017143893634 ) ) ;
#165573 = CARTESIAN_POINT ( 'NONE',  ( 6.567919353034534780, -1.191429365117269157, 1.534444726360333799 ) ) ;
#165575 = ADVANCED_FACE ( 'NONE', ( #159318 ), #193944, .F. ) ;
#165574 = CARTESIAN_POINT ( 'NONE',  ( -7.226132685959434809, 8.493204890783200511, 1.082531754730549967 ) ) ;
#165576 = CARTESIAN_POINT ( 'NONE',  ( -4.411198876399886615, 6.239761003923544713, -1.599625672291271394 ) ) ;
#165577 = CARTESIAN_POINT ( 'NONE',  ( -0.2108831679770960255, -0.001785917861228669690, -1.896958272444612792 ) ) ;
#165578 = CARTESIAN_POINT ( 'NONE',  ( 4.131183091185314460, 1.940096312829143299, 0.8565103500411813675 ) ) ;
#165579 = DIRECTION ( 'NONE',  ( -1.000000000000000000, 0.000000000000000000, 0.000000000000000000 ) ) ;
#165580 = CARTESIAN_POINT ( 'NONE',  ( 1.266250242576156815, 1.862016182229693673, -0.7743172429433076154 ) ) ;
#165581 = CARTESIAN_POINT ( 'NONE',  ( -6.927853306458756855, 9.105581495667113501, 1.443375672974078761 ) ) ;
#165582 = CARTESIAN_POINT ( 'NONE',  ( 4.594872931952145301, -0.4798491958124780910, -2.153818993410236970 ) ) ;
#165583 = CARTESIAN_POINT ( 'NONE',  ( -3.285556943749998737, -2.617708332855374298, 1.896917185911908499 ) ) ;
#165584 = ADVANCED_FACE ( 'NONE', ( #26109 ), #76535, .T. ) ;
#165585 = DIRECTION ( 'NONE',  ( 0.000000000000000000, 1.000000000000000000, 0.000000000000000000 ) ) ;
#165586 = CARTESIAN_POINT ( 'NONE',  ( -1.843739406749240750, 8.920000000000001705, -0.7749999999999996891 ) ) ;
#165587 = CARTESIAN_POINT ( 'NONE',  ( 7.013428937081408243, 5.939655416065873439, -2.436399677959149024 ) ) ;
#165589 = CARTESIAN_POINT ( 'NONE',  ( -0.1290005225502675879, -0.006633637972621592160, -2.173875058097324064 ) ) ;
#165588 = CARTESIAN_POINT ( 'NONE',  ( -4.584908210271880336, 8.498668195373706880, -0.01721603403951645073 ) ) ;
#165590 = FILL_AREA_STYLE_COLOUR ( '', #16336 ) ;
#165591 = ORIENTED_EDGE ( 'NONE', *, *, #46016, .T. ) ;
#165592 = CARTESIAN_POINT ( 'NONE',  ( 3.221608841920938993, -1.986550002599724252, 0.5482939856576442006 ) ) ;
#165593 = CARTESIAN_POINT ( 'NONE',  ( -1.953008978358306879E-14, 1.828125000341410678, -1.570758158831798257 ) ) ;
#165594 = EDGE_CURVE ( 'NONE', #36083, #144861, #38511, .T. ) ;
#165595 = CARTESIAN_POINT ( 'NONE',  ( -6.338600509588822263, 7.353787668397130162, -1.199719254218446718 ) ) ;
#165596 = CARTESIAN_POINT ( 'NONE',  ( 3.000653711923051414, -1.990157830909113024, -0.3430147326864175783 ) ) ;
#165597 = CARTESIAN_POINT ( 'NONE',  ( 1.499999999999987121, -0.9958333333333134751, 0.8660254037844524744 ) ) ;
#165598 = VECTOR ( 'NONE', #187698, 1000.000000000000000 ) ;
#165599 = CARTESIAN_POINT ( 'NONE',  ( 9.951321562750607086, 11.67259191370631477, -1.082531754730537088 ) ) ;
#165600 = CARTESIAN_POINT ( 'NONE',  ( 1.780222679459046997, -1.103320402871512673, 1.740482491890801287 ) ) ;
#165601 =( BOUNDED_SURFACE ( )  B_SPLINE_SURFACE ( 1, 2, ( 
 ( #100358, #87312, #150194, #152314, #165356, #102494, #184789, #71030, #183739, #19093, #35347, #66753, #33225, #686, #133968, #185858, #201031, #52673, #118804, #101425, #36415, #3891, #199975, #168558, #181597, #99309, #20157, #137144, #86244, #136073, #53746, #119880, #34285, #37490, #153381, #132894, #83033, #149107, #50544, #58010, #107905, #188001, #26571, #173931, #24419, #23357, #88386, #40713, #204226, #154456, #91612, #25504, #7101, #120965, #38568, #74273, #191193, #108967, #6034, #90532, #89466, #205311, #207456, #157663, #190138, #106818, #9261, #75332, #174987, #92676, #55878, #141449, #156594, #59075, #170690, #155520, #72103, #124174, #189080, #8188, #140365, #105731, #22277, #171761, #138214, #172848, #42860, #122035, #41792, #186936, #10318, #104643, #139279, #56948, #123120, #206384, #158720, #125235, #76392, #142501, #208507, #39626, #73173, #95877, #210656, #13522, #30867, #128444, #145714, #177103, #60142, #28718, #194410, #161932, #43921, #114305, #112173, #180303, #111097, #96945, #14576, #196550, #78524, #143577, #144641, #46052, #31925, #211712, #79595, #93741, #11380, #162995, #77459, #164061, #127372, #63348, #179243, #94805, #159780, #212780, #80671, #176048, #61215, #146762, #160854, #98004, #126299, #12445, #178177, #48193, #193343, #62284, #15640, #81727, #192258, #29792, #129507, #195488, #47122, #130560, #64415, #113239, #147810, #110036, #27641, #209569, #44988, #149937, #167247, #184538, #67572, #84919, #116417, #213829, #182408, #133716, #35091, #197599, #53488, #51368, #119625, #50299, #36160, #168310, #135819, #17760, #82788, #83848, #199722, #185609, #151007, #18835, #32979, #165110, #102239, #16702, #103312, #66505, #2577, #118556, #34037, #99055, #152067, #19908, #115361, #434, #85993, #100110, #37241, #65447, #166171, #117491, #201843, #132644, #1506, #169374, #131597, #134770, #20958, #198650, #68647, #183482, #101162, #148861, #200778, #3637, #52430, #69716, #87056, #181353, #49242, #140105, #5769, #58827, #206132, #56698, #55624, #120706, #72926, #22020, #186681, #123923, #57762, #39376, #153128, #70775, #106564, #9004, #141192, #38309, #122865, #121781, #23099, #25251, #189891, #7927, #139032, #41533, #107644, #207202, #124981, #88130, #173676, #188826, #91351, #202915, #187748, #104386, #90273, #6848, #40460, #172592, #137957, #54560, #203977, #170433, #205056, #75079, #154201, #74013, #4699, #157413, #190941, #136889, #24170, #156342, #42605, #105473, #89215, #108712, #174740, #71849, #26313, #171506, #155267, #192003, #96699, #92426, #11124, #80412, #60961, #63094, #76142, #13273, #95629, #196299, #94555, #78270, #160594, #43668, #158466, #126040, #193085, #162746, #210397, #177923, #111923, #12200, #194154, #129263, #77202, #144396, #180052, #10066, #195233, #114060, #93486, #46871, #161679, #30610, #14319, #212527, #112985, #146510, #130311, #64168, #62040 ),
 ( #45802, #178995, #128193, #29538, #209314, #142245, #127118, #79347, #145464, #208258, #47945, #211459, #59891, #143320, #109785, #175794, #27386, #110842, #159525, #176848, #44736, #28461, #183233, #199467, #65202, #197349, #2321, #48991, #135568, #98804, #34838, #150759, #66253, #131354, #184289, #134525, #147557, #32722, #68397, #185, #3394, #97751, #82530, #17511, #168058, #164857, #116168, #19660, #31674, #167001, #201592, #16449, #117234, #132401, #148617, #181106, #149680, #52176, #115109, #51109, #200531, #213579, #100913, #151820, #198403, #118302, #1261, #35914, #81480, #50045, #182154, #18592, #99863, #67319, #84670, #33784, #165926, #83598, #133463, #101989, #85735, #69463, #53240, #163810, #119369, #15386, #203724, #55372, #121526, #72676, #41281, #7667, #40197, #88957, #58572, #86806, #187496, #6595, #39126, #138772, #156081, #105209, #56443, #87874, #185357, #153946, #171246, #204790, #169116, #24993, #22842, #91096, #21766, #73752, #139847, #107390, #155010, #54311, #122602, #188565, #157156, #106308, #172331, #4450, #136636, #205876, #202661, #74830, #38062, #23919, #90025, #5515, #70520, #123669, #57511, #152872, #186423, #189632, #71595, #8748, #36979, #137704, #173412, #140929, #104132, #206943, #103062, #20713, #120449, #170178, #109531, #210132, #159265, #43407, #59632, #28205, #145196, #9811, #78015, #95368, #26057, #61774, #111656, #191752, #30348, #177668, #94299, #27126, #92171, #44475, #208008, #158222, #161419, #29277, #10865, #124728, #42346, #144140, #194967, #112722, #75886, #160340, #93232, #209059, #211203, #13002, #193895, #110591, #79078, #62828, #178734, #76939, #141994, #127942, #192817, #11943, #45542, #175536, #174481, #143064, #125790, #176594, #46603, #60695, #128988, #190687, #14057, #108461, #126860, #96433, #162484, #80145, #146248, #212264, #133197, #181890, #151560, #179793, #65990, #99598, #214359, #17252, #34586, #132139, #149415, #180840, #63898, #32466, #198146, #165664, #47680, #118047, #115905, #184033, #114842, #100660, #18327, #200271, #82267, #147297, #148361, #49778, #35648, #997, #83329, #97487, #15129, #166736, #81217, #167798, #131101, #67061, #182971, #98536, #163544, #2057, #84410, #31413, #64950, #150498, #164597, #101727, #130053, #16184, #33527, #51923, #197090, #199199, #19393, #196047, #50848, #85473, #48729, #116974, #68131, #134265, #213327, #113791, #26605, #102801, #170989, #191229, #119108, #154754, #204534, #70265, #126332, #56183, #121264, #120188, #185090, #137448, #86544, #36714, #42892, #122344, #103872, #3128, #135318, #22588, #76421, #208539, #168858, #187237, #186164, #87616, #92706, #109001, #72410, #203464, #175018, #158753, #60175, #192291, #152610, #10347, #38866, #142532, #52971, #37797, #153687, #43951, #110067, #138510, #55118, #176079, #27677, #93772, #69197, #4195, #201332, #104949, #20461, #136380, #169922, #202398, #6338 ) ),
 .UNSPECIFIED., .F., .F., .T. ) 
 B_SPLINE_SURFACE_WITH_KNOTS ( ( 2, 2 ),
 ( 3, 2, 2, 2, 2, 2, 2, 2, 2, 2, 2, 2, 2, 2, 2, 2, 2, 2, 2, 2, 2, 2, 2, 2, 2, 2, 2, 2, 2, 2, 2, 2, 2, 2, 2, 2, 2, 2, 2, 2, 2, 2, 2, 2, 2, 2, 2, 2, 2, 2, 2, 2, 2, 2, 2, 2, 2, 2, 2, 2, 2, 2, 2, 2, 2, 2, 2, 2, 2, 2, 2, 2, 2, 2, 2, 2, 2, 2, 2, 2, 2, 2, 2, 2, 2, 2, 2, 2, 2, 2, 2, 2, 2, 2, 2, 2, 2, 2, 2, 2, 2, 2, 2, 2, 2, 2, 2, 2, 2, 2, 2, 2, 2, 2, 2, 2, 2, 2, 2, 2, 2, 2, 2, 2, 2, 2, 2, 2, 2, 2, 2, 2, 2, 2, 2, 2, 2, 2, 2, 2, 2, 2, 2, 2, 2, 2, 2, 2, 2, 2, 2, 2, 2, 2, 2, 2, 2, 2, 2, 2, 2, 2, 2, 2, 2, 2, 2, 2, 3 ),
 ( 0.000000000000000000, 1.000000000000000000 ),
 ( 0.000000000000000000, 0.005952380952380952051, 0.01190476190476190410, 0.01785714285714285615, 0.02380952380952380820, 0.02976190476190476025, 0.03571428571428571230, 0.04166666666666666435, 0.04761904761904761640, 0.05357142857142856845, 0.05952380952380952051, 0.06547619047619047949, 0.07142857142857142461, 0.07738095238095238360, 0.08333333333333332871, 0.08928571428571428770, 0.09523809523809523281, 0.1011904761904761918, 0.1071428571428571369, 0.1130952380952380959, 0.1190476190476190410, 0.1250000000000000000, 0.1309523809523809590, 0.1369047619047619180, 0.1428571428571428492, 0.1488095238095238082, 0.1547619047619047672, 0.1607142857142857262, 0.1666666666666666574, 0.1726190476190476164, 0.1785714285714285754, 0.1845238095238095344, 0.1904761904761904656, 0.1964285714285714246, 0.2023809523809523836, 0.2083333333333333426, 0.2142857142857142738, 0.2202380952380952328, 0.2261904761904761918, 0.2321428571428571508, 0.2380952380952380820, 0.2440476190476190410, 0.2500000000000000000, 0.2559523809523809312, 0.2619047619047619180, 0.2678571428571428492, 0.2738095238095238360, 0.2797619047619047672, 0.2857142857142856984, 0.2916666666666666852, 0.2976190476190476164, 0.3035714285714285476, 0.3095238095238095344, 0.3154761904761904656, 0.3214285714285714524, 0.3273809523809523836, 0.3333333333333333148, 0.3392857142857143016, 0.3452380952380952328, 0.3511904761904761640, 0.3571428571428571508, 0.3630952380952380820, 0.3690476190476190688, 0.3750000000000000000, 0.3809523809523809312, 0.3869047619047619180, 0.3928571428571428492, 0.3988095238095238360, 0.4047619047619047672, 0.4107142857142856984, 0.4166666666666666852, 0.4226190476190476164, 0.4285714285714285476, 0.4345238095238095344, 0.4404761904761904656, 0.4464285714285714524, 0.4523809523809523836, 0.4583333333333333148, 0.4642857142857143016, 0.4702380952380952328, 0.4761904761904761640, 0.4821428571428571508, 0.4880952380952380820, 0.4940476190476190688, 0.5000000000000000000, 0.5059523809523809312, 0.5119047619047618625, 0.5178571428571429047, 0.5238095238095238360, 0.5297619047619047672, 0.5357142857142856984, 0.5416666666666666297, 0.5476190476190476719, 0.5535714285714286031, 0.5595238095238095344, 0.5654761904761904656, 0.5714285714285713969, 0.5773809523809523281, 0.5833333333333333703, 0.5892857142857143016, 0.5952380952380952328, 0.6011904761904761640, 0.6071428571428570953, 0.6130952380952381375, 0.6190476190476190688, 0.6250000000000000000, 0.6309523809523809312, 0.6369047619047618625, 0.6428571428571429047, 0.6488095238095238360, 0.6547619047619047672, 0.6607142857142856984, 0.6666666666666666297, 0.6726190476190476719, 0.6785714285714286031, 0.6845238095238095344, 0.6904761904761904656, 0.6964285714285713969, 0.7023809523809523281, 0.7083333333333333703, 0.7142857142857143016, 0.7202380952380952328, 0.7261904761904761640, 0.7321428571428570953, 0.7380952380952381375, 0.7440476190476190688, 0.7500000000000000000, 0.7559523809523809312, 0.7619047619047618625, 0.7678571428571429047, 0.7738095238095238360, 0.7797619047619047672, 0.7857142857142856984, 0.7916666666666666297, 0.7976190476190476719, 0.8035714285714286031, 0.8095238095238095344, 0.8154761904761904656, 0.8214285714285713969, 0.8273809523809523281, 0.8333333333333333703, 0.8392857142857143016, 0.8452380952380952328, 0.8511904761904761640, 0.8571428571428570953, 0.8630952380952381375, 0.8690476190476190688, 0.8750000000000000000, 0.8809523809523809312, 0.8869047619047618625, 0.8928571428571429047, 0.8988095238095238360, 0.9047619047619047672, 0.9107142857142856984, 0.9166666666666666297, 0.9226190476190476719, 0.9285714285714286031, 0.9345238095238095344, 0.9404761904761904656, 0.9464285714285713969, 0.9523809523809523281, 0.9583333333333333703, 0.9642857142857143016, 0.9702380952380952328, 0.9761904761904761640, 0.9821428571428570953, 0.9880952380952381375, 0.9940476190476190688, 1.000000000000000000 ),
 .UNSPECIFIED. ) 
 GEOMETRIC_REPRESENTATION_ITEM ( )  RATIONAL_B_SPLINE_SURFACE ( (
 ( 1.000000000000000000, 0.8660254037844387076, 1.000000000000000000, 0.8660254037844387076, 1.000000000000000000, 0.8660254037844387076, 1.000000000000000000, 0.8660254037844387076, 1.000000000000000000, 0.8660254037844387076, 1.000000000000000000, 0.8660254037844387076, 1.000000000000000000, 0.8660254037844387076, 1.000000000000000000, 0.8660254037844387076, 1.000000000000000000, 0.8660254037844387076, 1.000000000000000000, 0.8660254037844387076, 1.000000000000000000, 0.8660254037844387076, 1.000000000000000000, 0.8660254037844387076, 1.000000000000000000, 0.8660254037844387076, 1.000000000000000000, 0.8660254037844387076, 1.000000000000000000, 0.8660254037844387076, 1.000000000000000000, 0.8660254037844387076, 1.000000000000000000, 0.8660254037844387076, 1.000000000000000000, 0.8660254037844387076, 1.000000000000000000, 0.8660254037844387076, 1.000000000000000000, 0.8660254037844387076, 1.000000000000000000, 0.8660254037844387076, 1.000000000000000000, 0.8660254037844387076, 1.000000000000000000, 0.8660254037844387076, 1.000000000000000000, 0.8660254037844387076, 1.000000000000000000, 0.8660254037844387076, 1.000000000000000000, 0.8660254037844387076, 1.000000000000000000, 0.8660254037844387076, 1.000000000000000000, 0.8660254037844387076, 1.000000000000000000, 0.8660254037844387076, 1.000000000000000000, 0.8660254037844387076, 1.000000000000000000, 0.8660254037844387076, 1.000000000000000000, 0.8660254037844387076, 1.000000000000000000, 0.8660254037844387076, 1.000000000000000000, 0.8660254037844387076, 1.000000000000000000, 0.8660254037844387076, 1.000000000000000000, 0.8660254037844387076, 1.000000000000000000, 0.8660254037844387076, 1.000000000000000000, 0.8660254037844387076, 1.000000000000000000, 0.8660254037844387076, 1.000000000000000000, 0.8660254037844387076, 1.000000000000000000, 0.8660254037844387076, 1.000000000000000000, 0.8660254037844387076, 1.000000000000000000, 0.8660254037844387076, 1.000000000000000000, 0.8660254037844387076, 1.000000000000000000, 0.8660254037844387076, 1.000000000000000000, 0.8660254037844387076, 1.000000000000000000, 0.8660254037844387076, 1.000000000000000000, 0.8660254037844387076, 1.000000000000000000, 0.8660254037844387076, 1.000000000000000000, 0.8660254037844387076, 1.000000000000000000, 0.8660254037844387076, 1.000000000000000000, 0.8660254037844387076, 1.000000000000000000, 0.8660254037844387076, 1.000000000000000000, 0.8660254037844387076, 1.000000000000000000, 0.8660254037844387076, 1.000000000000000000, 0.8660254037844387076, 1.000000000000000000, 0.8660254037844387076, 1.000000000000000000, 0.8660254037844387076, 1.000000000000000000, 0.8660254037844387076, 1.000000000000000000, 0.8660254037844387076, 1.000000000000000000, 0.8660254037844387076, 1.000000000000000000, 0.8660254037844387076, 1.000000000000000000, 0.8660254037844387076, 1.000000000000000000, 0.8660254037844387076, 1.000000000000000000, 0.8660254037844387076, 1.000000000000000000, 0.8660254037844387076, 1.000000000000000000, 0.8660254037844387076, 1.000000000000000000, 0.8660254037844387076, 1.000000000000000000, 0.8660254037844387076, 1.000000000000000000, 0.8660254037844387076, 1.000000000000000000, 0.8660254037844387076, 1.000000000000000000, 0.8660254037844387076, 1.000000000000000000, 0.8660254037844387076, 1.000000000000000000, 0.8660254037844387076, 1.000000000000000000, 0.8660254037844387076, 1.000000000000000000, 0.8660254037844387076, 1.000000000000000000, 0.8660254037844387076, 1.000000000000000000, 0.8660254037844387076, 1.000000000000000000, 0.8660254037844387076, 1.000000000000000000, 0.8660254037844387076, 1.000000000000000000, 0.8660254037844387076, 1.000000000000000000, 0.8660254037844387076, 1.000000000000000000, 0.8660254037844387076, 1.000000000000000000, 0.8660254037844387076, 1.000000000000000000, 0.8660254037844387076, 1.000000000000000000, 0.8660254037844387076, 1.000000000000000000, 0.8660254037844387076, 1.000000000000000000, 0.8660254037844387076, 1.000000000000000000, 0.8660254037844387076, 1.000000000000000000, 0.8660254037844387076, 1.000000000000000000, 0.8660254037844387076, 1.000000000000000000, 0.8660254037844387076, 1.000000000000000000, 0.8660254037844387076, 1.000000000000000000, 0.8660254037844387076, 1.000000000000000000, 0.8660254037844387076, 1.000000000000000000, 0.8660254037844387076, 1.000000000000000000, 0.8660254037844387076, 1.000000000000000000, 0.8660254037844387076, 1.000000000000000000, 0.8660254037844387076, 1.000000000000000000, 0.8660254037844387076, 1.000000000000000000, 0.8660254037844387076, 1.000000000000000000, 0.8660254037844387076, 1.000000000000000000, 0.8660254037844387076, 1.000000000000000000, 0.8660254037844387076, 1.000000000000000000, 0.8660254037844387076, 1.000000000000000000, 0.8660254037844387076, 1.000000000000000000, 0.8660254037844387076, 1.000000000000000000, 0.8660254037844387076, 1.000000000000000000, 0.8660254037844387076, 1.000000000000000000, 0.8660254037844387076, 1.000000000000000000, 0.8660254037844387076, 1.000000000000000000, 0.8660254037844387076, 1.000000000000000000, 0.8660254037844387076, 1.000000000000000000, 0.8660254037844387076, 1.000000000000000000, 0.8660254037844387076, 1.000000000000000000, 0.8660254037844387076, 1.000000000000000000, 0.8660254037844387076, 1.000000000000000000, 0.8660254037844387076, 1.000000000000000000, 0.8660254037844387076, 1.000000000000000000, 0.8660254037844387076, 1.000000000000000000, 0.8660254037844387076, 1.000000000000000000, 0.8660254037844387076, 1.000000000000000000, 0.8660254037844387076, 1.000000000000000000, 0.8660254037844387076, 1.000000000000000000, 0.8660254037844387076, 1.000000000000000000, 0.8660254037844387076, 1.000000000000000000, 0.8660254037844387076, 1.000000000000000000, 0.8660254037844387076, 1.000000000000000000, 0.8660254037844387076, 1.000000000000000000, 0.8660254037844387076, 1.000000000000000000, 0.8660254037844387076, 1.000000000000000000, 0.8660254037844387076, 1.000000000000000000, 0.8660254037844387076, 1.000000000000000000, 0.8660254037844387076, 1.000000000000000000, 0.8660254037844387076, 1.000000000000000000, 0.8660254037844387076, 1.000000000000000000, 0.8660254037844387076, 1.000000000000000000, 0.8660254037844387076, 1.000000000000000000, 0.8660254037844387076, 1.000000000000000000, 0.8660254037844387076, 1.000000000000000000, 0.8660254037844387076, 1.000000000000000000, 0.8660254037844387076, 1.000000000000000000, 0.8660254037844387076, 1.000000000000000000, 0.8660254037844387076, 1.000000000000000000, 0.8660254037844387076, 1.000000000000000000, 0.8660254037844387076, 1.000000000000000000, 0.8660254037844387076, 1.000000000000000000, 0.8660254037844387076, 1.000000000000000000, 0.8660254037844387076, 1.000000000000000000, 0.8660254037844387076, 1.000000000000000000, 0.8660254037844387076, 1.000000000000000000, 0.8660254037844387076, 1.000000000000000000, 0.8660254037844387076, 1.000000000000000000, 0.8660254037844387076, 1.000000000000000000, 0.8660254037844387076, 1.000000000000000000, 0.8660254037844387076, 1.000000000000000000, 0.8660254037844387076, 1.000000000000000000, 0.8660254037844387076, 1.000000000000000000, 0.8660254037844387076, 1.000000000000000000, 0.8660254037844387076, 1.000000000000000000, 0.8660254037844387076, 1.000000000000000000, 0.8660254037844387076, 1.000000000000000000, 0.8660254037844387076, 1.000000000000000000, 0.8660254037844387076, 1.000000000000000000, 0.8660254037844387076, 1.000000000000000000, 0.8660254037844387076, 1.000000000000000000, 0.8660254037844387076, 1.000000000000000000, 0.8660254037844387076, 1.000000000000000000),
 ( 1.000000000000000000, 0.8660254037844387076, 1.000000000000000000, 0.8660254037844387076, 1.000000000000000000, 0.8660254037844387076, 1.000000000000000000, 0.8660254037844387076, 1.000000000000000000, 0.8660254037844387076, 1.000000000000000000, 0.8660254037844387076, 1.000000000000000000, 0.8660254037844387076, 1.000000000000000000, 0.8660254037844387076, 1.000000000000000000, 0.8660254037844387076, 1.000000000000000000, 0.8660254037844387076, 1.000000000000000000, 0.8660254037844387076, 1.000000000000000000, 0.8660254037844387076, 1.000000000000000000, 0.8660254037844387076, 1.000000000000000000, 0.8660254037844387076, 1.000000000000000000, 0.8660254037844387076, 1.000000000000000000, 0.8660254037844387076, 1.000000000000000000, 0.8660254037844387076, 1.000000000000000000, 0.8660254037844387076, 1.000000000000000000, 0.8660254037844387076, 1.000000000000000000, 0.8660254037844387076, 1.000000000000000000, 0.8660254037844387076, 1.000000000000000000, 0.8660254037844387076, 1.000000000000000000, 0.8660254037844387076, 1.000000000000000000, 0.8660254037844387076, 1.000000000000000000, 0.8660254037844387076, 1.000000000000000000, 0.8660254037844387076, 1.000000000000000000, 0.8660254037844387076, 1.000000000000000000, 0.8660254037844387076, 1.000000000000000000, 0.8660254037844387076, 1.000000000000000000, 0.8660254037844387076, 1.000000000000000000, 0.8660254037844387076, 1.000000000000000000, 0.8660254037844387076, 1.000000000000000000, 0.8660254037844387076, 1.000000000000000000, 0.8660254037844387076, 1.000000000000000000, 0.8660254037844387076, 1.000000000000000000, 0.8660254037844387076, 1.000000000000000000, 0.8660254037844387076, 1.000000000000000000, 0.8660254037844387076, 1.000000000000000000, 0.8660254037844387076, 1.000000000000000000, 0.8660254037844387076, 1.000000000000000000, 0.8660254037844387076, 1.000000000000000000, 0.8660254037844387076, 1.000000000000000000, 0.8660254037844387076, 1.000000000000000000, 0.8660254037844387076, 1.000000000000000000, 0.8660254037844387076, 1.000000000000000000, 0.8660254037844387076, 1.000000000000000000, 0.8660254037844387076, 1.000000000000000000, 0.8660254037844387076, 1.000000000000000000, 0.8660254037844387076, 1.000000000000000000, 0.8660254037844387076, 1.000000000000000000, 0.8660254037844387076, 1.000000000000000000, 0.8660254037844387076, 1.000000000000000000, 0.8660254037844387076, 1.000000000000000000, 0.8660254037844387076, 1.000000000000000000, 0.8660254037844387076, 1.000000000000000000, 0.8660254037844387076, 1.000000000000000000, 0.8660254037844387076, 1.000000000000000000, 0.8660254037844387076, 1.000000000000000000, 0.8660254037844387076, 1.000000000000000000, 0.8660254037844387076, 1.000000000000000000, 0.8660254037844387076, 1.000000000000000000, 0.8660254037844387076, 1.000000000000000000, 0.8660254037844387076, 1.000000000000000000, 0.8660254037844387076, 1.000000000000000000, 0.8660254037844387076, 1.000000000000000000, 0.8660254037844387076, 1.000000000000000000, 0.8660254037844387076, 1.000000000000000000, 0.8660254037844387076, 1.000000000000000000, 0.8660254037844387076, 1.000000000000000000, 0.8660254037844387076, 1.000000000000000000, 0.8660254037844387076, 1.000000000000000000, 0.8660254037844387076, 1.000000000000000000, 0.8660254037844387076, 1.000000000000000000, 0.8660254037844387076, 1.000000000000000000, 0.8660254037844387076, 1.000000000000000000, 0.8660254037844387076, 1.000000000000000000, 0.8660254037844387076, 1.000000000000000000, 0.8660254037844387076, 1.000000000000000000, 0.8660254037844387076, 1.000000000000000000, 0.8660254037844387076, 1.000000000000000000, 0.8660254037844387076, 1.000000000000000000, 0.8660254037844387076, 1.000000000000000000, 0.8660254037844387076, 1.000000000000000000, 0.8660254037844387076, 1.000000000000000000, 0.8660254037844387076, 1.000000000000000000, 0.8660254037844387076, 1.000000000000000000, 0.8660254037844387076, 1.000000000000000000, 0.8660254037844387076, 1.000000000000000000, 0.8660254037844387076, 1.000000000000000000, 0.8660254037844387076, 1.000000000000000000, 0.8660254037844387076, 1.000000000000000000, 0.8660254037844387076, 1.000000000000000000, 0.8660254037844387076, 1.000000000000000000, 0.8660254037844387076, 1.000000000000000000, 0.8660254037844387076, 1.000000000000000000, 0.8660254037844387076, 1.000000000000000000, 0.8660254037844387076, 1.000000000000000000, 0.8660254037844387076, 1.000000000000000000, 0.8660254037844387076, 1.000000000000000000, 0.8660254037844387076, 1.000000000000000000, 0.8660254037844387076, 1.000000000000000000, 0.8660254037844387076, 1.000000000000000000, 0.8660254037844387076, 1.000000000000000000, 0.8660254037844387076, 1.000000000000000000, 0.8660254037844387076, 1.000000000000000000, 0.8660254037844387076, 1.000000000000000000, 0.8660254037844387076, 1.000000000000000000, 0.8660254037844387076, 1.000000000000000000, 0.8660254037844387076, 1.000000000000000000, 0.8660254037844387076, 1.000000000000000000, 0.8660254037844387076, 1.000000000000000000, 0.8660254037844387076, 1.000000000000000000, 0.8660254037844387076, 1.000000000000000000, 0.8660254037844387076, 1.000000000000000000, 0.8660254037844387076, 1.000000000000000000, 0.8660254037844387076, 1.000000000000000000, 0.8660254037844387076, 1.000000000000000000, 0.8660254037844387076, 1.000000000000000000, 0.8660254037844387076, 1.000000000000000000, 0.8660254037844387076, 1.000000000000000000, 0.8660254037844387076, 1.000000000000000000, 0.8660254037844387076, 1.000000000000000000, 0.8660254037844387076, 1.000000000000000000, 0.8660254037844387076, 1.000000000000000000, 0.8660254037844387076, 1.000000000000000000, 0.8660254037844387076, 1.000000000000000000, 0.8660254037844387076, 1.000000000000000000, 0.8660254037844387076, 1.000000000000000000, 0.8660254037844387076, 1.000000000000000000, 0.8660254037844387076, 1.000000000000000000, 0.8660254037844387076, 1.000000000000000000, 0.8660254037844387076, 1.000000000000000000, 0.8660254037844387076, 1.000000000000000000, 0.8660254037844387076, 1.000000000000000000, 0.8660254037844387076, 1.000000000000000000, 0.8660254037844387076, 1.000000000000000000, 0.8660254037844387076, 1.000000000000000000, 0.8660254037844387076, 1.000000000000000000, 0.8660254037844387076, 1.000000000000000000, 0.8660254037844387076, 1.000000000000000000, 0.8660254037844387076, 1.000000000000000000, 0.8660254037844387076, 1.000000000000000000, 0.8660254037844387076, 1.000000000000000000, 0.8660254037844387076, 1.000000000000000000, 0.8660254037844387076, 1.000000000000000000, 0.8660254037844387076, 1.000000000000000000, 0.8660254037844387076, 1.000000000000000000, 0.8660254037844387076, 1.000000000000000000, 0.8660254037844387076, 1.000000000000000000, 0.8660254037844387076, 1.000000000000000000, 0.8660254037844387076, 1.000000000000000000, 0.8660254037844387076, 1.000000000000000000, 0.8660254037844387076, 1.000000000000000000, 0.8660254037844387076, 1.000000000000000000, 0.8660254037844387076, 1.000000000000000000, 0.8660254037844387076, 1.000000000000000000, 0.8660254037844387076, 1.000000000000000000, 0.8660254037844387076, 1.000000000000000000, 0.8660254037844387076, 1.000000000000000000, 0.8660254037844387076, 1.000000000000000000, 0.8660254037844387076, 1.000000000000000000, 0.8660254037844387076, 1.000000000000000000, 0.8660254037844387076, 1.000000000000000000, 0.8660254037844387076, 1.000000000000000000, 0.8660254037844387076, 1.000000000000000000, 0.8660254037844387076, 1.000000000000000000, 0.8660254037844387076, 1.000000000000000000, 0.8660254037844387076, 1.000000000000000000) ) ) 
 REPRESENTATION_ITEM ( '' )  SURFACE ( )  );
#165602 = CARTESIAN_POINT ( 'NONE',  ( -9.407146676474797076, 14.61749904134098266, -7.348982780145471239 ) ) ;
#165603 = CARTESIAN_POINT ( 'NONE',  ( 6.006425746053997372, 6.966250444273174303, -1.199719254218445830 ) ) ;
#165604 = CARTESIAN_POINT ( 'NONE',  ( -0.2411972340276360705, 6.947779742164541972, -2.495493578726155182 ) ) ;
#165605 = CARTESIAN_POINT ( 'NONE',  ( 1.499689682683522207, -0.6613356838569836027, -1.718437284301529422 ) ) ;
#165606 = CARTESIAN_POINT ( 'NONE',  ( 6.604147088760183415, -2.206502607372296421, 0.04933187264975073122 ) ) ;
#165607 = CARTESIAN_POINT ( 'NONE',  ( 6.723917837734620484, 6.809268663637336516, 0.000000000000000000 ) ) ;
#165608 = CARTESIAN_POINT ( 'NONE',  ( 1.651884467337715989, 0.6291892518628816600, -2.067965918892029631 ) ) ;
#165609 = AXIS2_PLACEMENT_3D ( 'NONE', #11925, #106292, #207987 ) ;
#165610 = CARTESIAN_POINT ( 'NONE',  ( -3.795919822146289313, 5.451659097302528068, -1.443375672974053447 ) ) ;
#165611 = CARTESIAN_POINT ( 'NONE',  ( 1.885954221117658092, -2.015980662343511032, 0.05432778586660082232 ) ) ;
#165612 = CARTESIAN_POINT ( 'NONE',  ( 2.126706441246130286, 0.3935840842550219487, -2.264316624754546314 ) ) ;
#165613 = CARTESIAN_POINT ( 'NONE',  ( 0.07933194018404610137, -7.215568602689907074, -9.499668754396999759 ) ) ;
#165614 = CARTESIAN_POINT ( 'NONE',  ( 0.09234973940512071489, -0.4041859633337717694, -1.833079292876439670 ) ) ;
#165615 = CARTESIAN_POINT ( 'NONE',  ( 11.48767021851167414, 11.33004227463828961, 3.470194894594677226 ) ) ;
#165616 = EDGE_CURVE ( 'NONE', #42462, #103348, #209431, .T. ) ;
#165617 = CARTESIAN_POINT ( 'NONE',  ( 4.733256667524862848, -1.802829663221987788, 0.7981805449851049339 ) ) ;
#165618 = CARTESIAN_POINT ( 'NONE',  ( 3.081267818761534549, 1.592661989535900657, 1.236799713577160231 ) ) ;
#165620 = CARTESIAN_POINT ( 'NONE',  ( 10.19536832735223975, 10.99694392477354477, 0.000000000000000000 ) ) ;
#165619 = CARTESIAN_POINT ( 'NONE',  ( -0.6823417656250003738, 2.467708333674753618, -1.181850606188749264 ) ) ;
#165622 = CARTESIAN_POINT ( 'NONE',  ( 5.707678396406405064, -0.5131847548165735518, 2.042461488563215966 ) ) ;
#165621 = CARTESIAN_POINT ( 'NONE',  ( -7.877450944739929461, 9.149113176073413456, 1.199719254218462483 ) ) ;
#165623 = CARTESIAN_POINT ( 'NONE',  ( 4.861816338261779613, -0.5554421346023461492, 1.994381909410049669 ) ) ;
#165624 = CARTESIAN_POINT ( 'NONE',  ( 8.132193210098487057, 8.381980254736715708, 1.040834085586084257E-14 ) ) ;
#165625 = CARTESIAN_POINT ( 'NONE',  ( -7.386494761346872551, 7.511998731193139989, -0.7998128361456291469 ) ) ;
#165626 = CARTESIAN_POINT ( 'NONE',  ( 6.639320575229291421, 2.053731943030055795, 2.310327526069462234 ) ) ;
#165627 = CARTESIAN_POINT ( 'NONE',  ( 5.467059065379825888, -1.589572006150547168, 1.245957840514285042 ) ) ;
#165628 = CARTESIAN_POINT ( 'NONE',  ( -1.500000000000015099, -0.5895833326505155458, -0.8660254037844383745 ) ) ;
#165629 = CARTESIAN_POINT ( 'NONE',  ( 3.457953323470845941, 0.5611853863643158080, -2.238310864172543546 ) ) ;
#165630 = CARTESIAN_POINT ( 'NONE',  ( 0.6728087625662204641, 1.424998530877854552, -1.491364779339200641 ) ) ;
#165631 = CARTESIAN_POINT ( 'NONE',  ( 8.758204044748005401, 10.28062147603659504, 1.082531754730549967 ) ) ;
#165632 = CARTESIAN_POINT ( 'NONE',  ( 5.505492895601038938, 8.580769590579979678, -1.199719254218452047 ) ) ;
#165633 = CARTESIAN_POINT ( 'NONE',  ( 4.050854035433010480, 7.948023151305657841, 0.000000000000000000 ) ) ;
#165634 = CARTESIAN_POINT ( 'NONE',  ( -0.6823417656250212460, 1.113541667008083325, 1.181850606188755259 ) ) ;
#165635 = CARTESIAN_POINT ( 'NONE',  ( 5.825163275726873202, 6.825053905550038991, 1.199719254218452047 ) ) ;
#165636 = CARTESIAN_POINT ( 'NONE',  ( 5.924549939047454750, 9.855799328956630134, -0.7216878364870267237 ) ) ;
#165638 = DIRECTION ( 'NONE',  ( 0.000000000000000000, 1.000000000000000000, 0.000000000000000000 ) ) ;
#165637 = CARTESIAN_POINT ( 'NONE',  ( 3.209609721163650509, -1.773450621654437009, -1.252290679139915319 ) ) ;
#165639 = CARTESIAN_POINT ( 'NONE',  ( -10.39230484541327826, 4.000000000000003553, -5.999999999999975131 ) ) ;
#165641 = CARTESIAN_POINT ( 'NONE',  ( 2.595044651933966495, -0.5755060336137384214, 1.749081985381637061 ) ) ;
#165640 = CARTESIAN_POINT ( 'NONE',  ( -3.904385051055635270, 6.538571078664754843, 1.082531754730560403 ) ) ;
#165642 = CARTESIAN_POINT ( 'NONE',  ( 1.364683531249990311, 4.384375000341417028, 1.214306433183764966E-14 ) ) ;
#165643 = CARTESIAN_POINT ( 'NONE',  ( 4.107102485094754840, -0.3736803571842538529, 2.159302612355806339 ) ) ;
#165644 = DIRECTION ( 'NONE',  ( 0.000000000000000000, -0.06195440338563660415, 0.9980789807931683688 ) ) ;
#165645 = CARTESIAN_POINT ( 'NONE',  ( 4.803764043965432329, -0.6079002506334645339, 2.179255796609281148 ) ) ;
#165646 = CARTESIAN_POINT ( 'NONE',  ( -5.789674969154799733, 6.218922551941099108, -1.014761583188450000 ) ) ;
#165647 = CARTESIAN_POINT ( 'NONE',  ( 5.631620320865258655, 7.357208097040313532, -1.234165276361798735 ) ) ;
#165648 = CARTESIAN_POINT ( 'NONE',  ( -5.926322542504877333, 7.047036066744706950, -1.082531754730549967 ) ) ;
#165649 = CARTESIAN_POINT ( 'NONE',  ( 4.800995793014950941, 5.734154859006458160, -1.082531754730548412 ) ) ;
#165650 = CARTESIAN_POINT ( 'NONE',  ( 6.309784262603465699, -1.756040378898944043, 0.2188775834443684731 ) ) ;
#165651 =( BOUNDED_CURVE ( )  B_SPLINE_CURVE ( 2, ( #110481, #13952, #80035, #144023, #29162, #176480, #146138 ),
 .UNSPECIFIED., .F., .T. ) 
 B_SPLINE_CURVE_WITH_KNOTS ( ( 3, 2, 2, 3 ),
 ( 0.1750000000000002942, 0.1791666666666668351, 0.1833333333333333759, 0.1874999999999999167 ),
 .UNSPECIFIED. ) 
 CURVE ( )  GEOMETRIC_REPRESENTATION_ITEM ( )  RATIONAL_B_SPLINE_CURVE ( ( 0.9999999999999902300, 0.8660254037844484776, 1.000000000000000000, 0.8660254037844387076, 1.000000000000000000, 0.8660254037844413721, 0.9999999999999973355 ) ) 
 REPRESENTATION_ITEM ( '' )  );
#165653 = CARTESIAN_POINT ( 'NONE',  ( 4.371743676962040581, 0.4387793907001916738, -1.964547544987900851 ) ) ;
#165652 = AXIS2_PLACEMENT_3D ( 'NONE', #169493, #9131, #54676 ) ;
#165654 = CARTESIAN_POINT ( 'NONE',  ( 6.632963465583686435, 8.761543347979550589, -1.599625672291262513 ) ) ;
#165655 = CARTESIAN_POINT ( 'NONE',  ( 2.801903084826493640, -0.6620233120280398786, 1.999254901717039790 ) ) ;
#165656 = CARTESIAN_POINT ( 'NONE',  ( 0.4916157762205043413, -1.906313760269543911, 0.1885876022650559980 ) ) ;
#165657 = CARTESIAN_POINT ( 'NONE',  ( 3.765413976293345844, 5.416068943807445635, 1.599625672291267398 ) ) ;
#165658 = CARTESIAN_POINT ( 'NONE',  ( 1.873436276770530595, -0.2440693053713405281, 1.954313301998261920 ) ) ;
#165659 = CARTESIAN_POINT ( 'NONE',  ( 0.9361565222895779081, 1.842281575443193375, 0.3236747858033904302 ) ) ;
#165660 = CARTESIAN_POINT ( 'NONE',  ( 1.486689167417578394, 1.889818972856545987, 0.5264814339432166701 ) ) ;
#165662 = VERTEX_POINT ( 'NONE', #83380 ) ;
#165661 = CARTESIAN_POINT ( 'NONE',  ( 6.411931881972196610E-05, -0.8997486769052507327, 1.687471195204979457 ) ) ;
#165663 = CARTESIAN_POINT ( 'NONE',  ( 5.829642864196171281, 5.903597551091405826, 0.7216878364870317197 ) ) ;
#165664 = CARTESIAN_POINT ( 'NONE',  ( -1.364683531250014514, 1.051041667008090208, -0.7879004041258289570 ) ) ;
#165665 = CARTESIAN_POINT ( 'NONE',  ( 5.664887262500884368, -1.691755685069219695, -0.7986314380193232365 ) ) ;
#165666 = DIRECTION ( 'NONE',  ( 0.000000000000000000, 1.000000000000000000, 0.000000000000000000 ) ) ;
#165667 = DIRECTION ( 'NONE',  ( -0.7592566023653016805, 0.6507913734559627184, 0.000000000000000000 ) ) ;
#165668 = VECTOR ( 'NONE', #140188, 1000.000000000000000 ) ;
#165669 = SURFACE_SIDE_STYLE ('',( #166740 ) ) ;
#165670 = CARTESIAN_POINT ( 'NONE',  ( 1.346235217667652417, -0.9325981557438846048, 1.848514419461377845 ) ) ;
#165671 = CARTESIAN_POINT ( 'NONE',  ( 0.7499999999999885647, 0.2333333333333562076, 1.299038105676657340 ) ) ;
#165672 = CARTESIAN_POINT ( 'NONE',  ( 7.233438648090761980, 8.397765496649418182, 1.199719254218462483 ) ) ;
#165673 = CARTESIAN_POINT ( 'NONE',  ( -7.018317073368468328, 11.33978701890523233, -0.7998128361456291469 ) ) ;
#165674 = CARTESIAN_POINT ( 'NONE',  ( 5.716698046817569434, 6.698511138489155137, -1.199719254218452047 ) ) ;
#165675 = CARTESIAN_POINT ( 'NONE',  ( 5.004590575528129470, -2.104527602236761386, -0.2589986953433416894 ) ) ;
#165676 = CARTESIAN_POINT ( 'NONE',  ( 4.573896719763862251, 6.429575154514868274, -1.599625672291273171 ) ) ;
#165677 = CARTESIAN_POINT ( 'NONE',  ( 0.6823417656249899377, 1.842708333674752952, 1.181850606188755259 ) ) ;
#165678 = ORIENTED_EDGE ( 'NONE', *, *, #53487, .F. ) ;
#165679 = CARTESIAN_POINT ( 'NONE',  ( 0.7499999999999885647, 2.566666666666689522, -1.299038105676658228 ) ) ;
#165681 = CARTESIAN_POINT ( 'NONE',  ( 4.467575310902914154, 5.170924936596891008, 1.199719254218464037 ) ) ;
#165680 = CARTESIAN_POINT ( 'NONE',  ( 5.934033239752055877, 1.167398200610193282, 1.576599764842034457 ) ) ;
#165682 = CARTESIAN_POINT ( 'NONE',  ( 2.759138561942891421, -2.010518527590241966, -0.1511176148010634768 ) ) ;
#165683 = CARTESIAN_POINT ( 'NONE',  ( 3.415159944131008096, -1.768026670962073110, 0.7381028802780668086 ) ) ;
#165684 = CARTESIAN_POINT ( 'NONE',  ( -1.893304937267614285, 3.295344712542847887, -0.4038802767149019535 ) ) ;
#165685 = CARTESIAN_POINT ( 'NONE',  ( 1.048660896456204528, -1.724490848714568259, 1.352309724062021878 ) ) ;
#165686 = CARTESIAN_POINT ( 'NONE',  ( 0.2335667940002320309, 1.326312899344052276, -2.404742575607053734 ) ) ;
#165687 = CARTESIAN_POINT ( 'NONE',  ( 3.444469828353763141, 0.4513171681363346566, 1.815172769691273835 ) ) ;
#165688 = CARTESIAN_POINT ( 'NONE',  ( 1.499999999999985123, -0.9229166659838452524, -0.8660254037844323793 ) ) ;
#165689 = CARTESIAN_POINT ( 'NONE',  ( -5.994676475536691029, 10.14553965476814845, 0.7998128361456481317 ) ) ;
#165691 = CARTESIAN_POINT ( 'NONE',  ( 5.923477664823041167, -1.533883339688602465, -1.459648931523350068 ) ) ;
#165690 = CARTESIAN_POINT ( 'NONE',  ( -4.121315508874262790, 6.791656612786516334, -1.082531754730549967 ) ) ;
#165692 = DIRECTION ( 'NONE',  ( 0.000000000000000000, 0.000000000000000000, -1.000000000000000000 ) ) ;
#165693 = CARTESIAN_POINT ( 'NONE',  ( -11.41381675112453564, 12.56994333910004791, 3.704697986577180302 ) ) ;
#165695 = CARTESIAN_POINT ( 'NONE',  ( 3.990100951807514562, 7.610040142558228915, -0.03152230841159352204 ) ) ;
#165694 = CARTESIAN_POINT ( 'NONE',  ( 2.859016124132291115, 0.3040538821531354463, -2.068378887337805949 ) ) ;
#165697 = ORIENTED_EDGE ( 'NONE', *, *, #126439, .T. ) ;
#165696 = CARTESIAN_POINT ( 'NONE',  ( 0.7094338256347174632, -1.717145877019264022, 0.1620263704987124354 ) ) ;
#165698 = CARTESIAN_POINT ( 'NONE',  ( 6.100279051144945619, 9.204410428722734849, -1.199719254218440723 ) ) ;
#165699 =( NAMED_UNIT ( * ) PLANE_ANGLE_UNIT ( ) SI_UNIT ( $, .RADIAN. ) );
#165700 = CARTESIAN_POINT ( 'NONE',  ( 7.346809171966453889, -6.836568542494980250, 8.002408263930263388 ) ) ;
#165701 = AXIS2_PLACEMENT_3D ( 'NONE', #111334, #12675, #62506 ) ;
#165702 = FACE_OUTER_BOUND ( 'NONE', #213065, .T. ) ;
#165703 = CARTESIAN_POINT ( 'NONE',  ( 5.436456408955479880, 9.286356877182658565, -0.7216878364870267237 ) ) ;
#165704 = CARTESIAN_POINT ( 'NONE',  ( -0.9399888277780873436, 7.435091042679319528, -4.383624543540896035 ) ) ;
#165706 = CARTESIAN_POINT ( 'NONE',  ( 0.2404698186789978875, 1.732857435387507250, 0.5278947837941138088 ) ) ;
#165705 = CARTESIAN_POINT ( 'NONE',  ( 6.017840079619279692, 8.114175741012878973, -1.599625672291281386 ) ) ;
#165707 = CARTESIAN_POINT ( 'NONE',  ( -5.845536785786364931, 9.971543350059432598, 0.000000000000000000 ) ) ;
#165708 = CARTESIAN_POINT ( 'NONE',  ( 5.529027716274630855, 5.344953845275508542, 1.040834085586084257E-14 ) ) ;
#165709 = CARTESIAN_POINT ( 'NONE',  ( -5.911423380092099222, 7.159701334921778404, 1.127351979631958434 ) ) ;
#165710 = CARTESIAN_POINT ( 'NONE',  ( 6.607619761813720238, 8.802252036906432764, 1.599625672291268286 ) ) ;
#165711 = CARTESIAN_POINT ( 'NONE',  ( 6.539320575229250920, 2.072231551265828475, 2.205269387046896679 ) ) ;
#165712 = PLANE ( 'NONE',  #166518 ) ;
#165713 = CARTESIAN_POINT ( 'NONE',  ( 4.100926828275982317, 7.458749316499424964, -0.6398019981258776800 ) ) ;
#165714 = CARTESIAN_POINT ( 'NONE',  ( 9.463228032658635769, 11.10314946193233965, -1.082531754730543083 ) ) ;
#165715 = EDGE_LOOP ( 'NONE', ( #36568, #28396, #121922, #121748 ) ) ;
#165716 = ADVANCED_FACE ( 'NONE', ( #46652 ), #15178, .F. ) ;
#165717 = CARTESIAN_POINT ( 'NONE',  ( 2.611566863951066519, 0.4996721132001956112, -1.792629727676842144 ) ) ;
#165718 = CIRCLE ( 'NONE', #55023, 6.249999999999995559 ) ;
#165719 = CARTESIAN_POINT ( 'NONE',  ( 0.4213150654816185114, -1.355317750890722595, -1.354022888547769421 ) ) ;
#165720 = CARTESIAN_POINT ( 'NONE',  ( 0.07680821025393690105, 0.005952109439256307241, -1.810863387344714193 ) ) ;
#165721 = DIRECTION ( 'NONE',  ( -1.000000000000000000, 0.000000000000000000, 0.000000000000000000 ) ) ;
#165722 = CARTESIAN_POINT ( 'NONE',  ( 2.273349394227877074, 5.683342515206170731, 0.4597581080974435519 ) ) ;
#165723 = CARTESIAN_POINT ( 'NONE',  ( -1.527330013470517001, 8.693738994866430758, -2.519751708053318495 ) ) ;
#165724 = CARTESIAN_POINT ( 'NONE',  ( -4.338245966692955591, 5.124003718305597310, 1.082531754730560403 ) ) ;
#165725 = CARTESIAN_POINT ( 'NONE',  ( 9.246297574839983824, 9.889694713509232571, 0.7216878364870438212 ) ) ;
#165726 = CARTESIAN_POINT ( 'NONE',  ( 4.961744348476156752, -0.5292939252423340957, 1.896881419486784681 ) ) ;
#165727 = CARTESIAN_POINT ( 'NONE',  ( 1.243013918421622233, 2.044566944090483229, 0.5621290157047582614 ) ) ;
#165728 = CARTESIAN_POINT ( 'NONE',  ( -4.394814349124112951, 8.279033840620114049, -0.7998128361456281477 ) ) ;
#165729 = CARTESIAN_POINT ( 'NONE',  ( -8.673617379884035472E-15, 3.507114751586604129, -11.99288524841337455 ) ) ;
#165730 = DIRECTION ( 'NONE',  ( -5.578564026256490882E-16, -1.000000000000000000, -9.066213480720158442E-32 ) ) ;
#165731 = CARTESIAN_POINT ( 'NONE',  ( 5.841772037242090931, 2.188765561305112683, 0.1107676204459909497 ) ) ;
#165732 = CARTESIAN_POINT ( 'NONE',  ( -1.115562610750309283E-14, 10.09375000068279782, 1.500000000000001554 ) ) ;
#165733 = CARTESIAN_POINT ( 'NONE',  ( 4.348602224742101008, 0.5129591300635885087, 1.856786894687269207 ) ) ;
#165734 = CARTESIAN_POINT ( 'NONE',  ( -7.691553217654356622, 7.867900263551875994, -0.7998128361456291469 ) ) ;
#165735 = CARTESIAN_POINT ( 'NONE',  ( -1.225000000000010747, 2.312500000682803147, -2.081668171172168513E-14 ) ) ;
#165736 = CARTESIAN_POINT ( 'NONE',  ( 1.313402753022639091, 1.947697196196996217, 1.037691534346518729 ) ) ;
#165737 = CARTESIAN_POINT ( 'NONE',  ( 0.000000000000000000, 13.49999999999999822, 0.000000000000000000 ) ) ;
#165738 = EDGE_LOOP ( 'NONE', ( #149144, #21847, #74086, #61031 ) ) ;
#165739 = CARTESIAN_POINT ( 'NONE',  ( 0.7500000000000006661, 10.61458333401613174, 1.299038105676657340 ) ) ;
#165740 = ORIENTED_EDGE ( 'NONE', *, *, #4542, .T. ) ;
#165741 = CARTESIAN_POINT ( 'NONE',  ( 5.805506361076694155, -1.550124894993635261, -1.214668715896784379 ) ) ;
#165743 = B_SPLINE_CURVE_WITH_KNOTS ( 'NONE', 3,
 ( #142601, #110139, #143685, #11490, #209677, #61321, #155258 ),
 .UNSPECIFIED., .F., .F.,
 ( 4, 3, 4 ),
 ( 0.0001135037245265561694, 0.001517139415464327252, 0.002007692284160942763 ),
 .UNSPECIFIED. ) ;
#165742 = CARTESIAN_POINT ( 'NONE',  ( 1.997508135846944421, -1.941589802808607157, 0.04981292379131925518 ) ) ;
#165744 = CARTESIAN_POINT ( 'NONE',  ( 6.098996632684510644, 1.141130774408656068, -1.995064312872560697 ) ) ;
#165746 = CARTESIAN_POINT ( 'NONE',  ( 4.557361202124784683, 1.492679318236398878, 1.111055945242465093 ) ) ;
#165745 = CARTESIAN_POINT ( 'NONE',  ( -5.582925393777276035, 9.735439736040634173, 0.7998128361456291469 ) ) ;
#165747 = CARTESIAN_POINT ( 'NONE',  ( 7.201315867513990554, 8.430565262634994284, -1.199719254218452047 ) ) ;
#165748 =( LENGTH_UNIT ( ) NAMED_UNIT ( * ) SI_UNIT ( .MILLI., .METRE. ) );
#165749 = CARTESIAN_POINT ( 'NONE',  ( 1.500000000000035971, 6.999999999999999112, 9.886859966642587594 ) ) ;
#165750 = CARTESIAN_POINT ( 'NONE',  ( -4.882907879216086933, 8.848476292394087395, -0.7998128361456281477 ) ) ;
#165751 = CARTESIAN_POINT ( 'NONE',  ( -3.634994582239682526, 6.294558541704648569, 1.082531754730549967 ) ) ;
#165752 = CARTESIAN_POINT ( 'NONE',  ( -0.05867695357848409787, -1.698172713885632401, -1.384993232510664640 ) ) ;
#165753 = CARTESIAN_POINT ( 'NONE',  ( 4.148431816101584957, 6.823292304551739740, -1.082531754730548412 ) ) ;
#165754 = ORIENTED_EDGE ( 'NONE', *, *, #62818, .T. ) ;
#165755 = AXIS2_PLACEMENT_3D ( 'NONE', #25742, #9505, #43104 ) ;
#165756 = DIRECTION ( 'NONE',  ( 1.276756478318932585E-15, -1.000000000000000000, 1.665334536937738262E-16 ) ) ;
#165757 = FACE_OUTER_BOUND ( 'NONE', #170346, .T. ) ;
#165758 = CARTESIAN_POINT ( 'NONE',  ( 2.051128252772801641, -1.465761996925791122, -1.088229512710245261 ) ) ;
#165759 = CARTESIAN_POINT ( 'NONE',  ( -5.122283107864663343, 4.870418468797203637, 0.000000000000000000 ) ) ;
#165760 = CARTESIAN_POINT ( 'NONE',  ( 4.166485388134741008, 1.137239580169274067, 1.309253364134143505 ) ) ;
#165761 = CARTESIAN_POINT ( 'NONE',  ( -6.529347706211431124, 6.814240946220119000, -0.5220719126654594922 ) ) ;
#165762 = CARTESIAN_POINT ( 'NONE',  ( -9.367496996949647325, 15.51845925588232333, 7.500000000809289524 ) ) ;
#165763 = CARTESIAN_POINT ( 'NONE',  ( 0.1331565106231571705, 4.092041177288479048, -2.500854978060399691 ) ) ;
#165764 = CARTESIAN_POINT ( 'NONE',  ( 6.252569598636129378, 0.5776572744066664766, 1.731972519516040032 ) ) ;
#165765 = CARTESIAN_POINT ( 'NONE',  ( 4.188298518248590341, 1.053080760608171129, -1.654974388233184657 ) ) ;
#165766 = TOROIDAL_SURFACE ( 'NONE', #207194, 2.600000000000000089, 0.1000000000000000056 ) ;
#165767 = CARTESIAN_POINT ( 'NONE',  ( -8.701635661872465732, 9.046329781806354831, 1.040834085586084257E-14 ) ) ;
#165768 = CARTESIAN_POINT ( 'NONE',  ( 6.205881626753210867, 8.263281202677319470, 1.599625672291281386 ) ) ;
#165769 = CIRCLE ( 'NONE', #152017, 0.2000000000000005107 ) ;
#165770 = CARTESIAN_POINT ( 'NONE',  ( 5.356147330077114077, 0.8591290142025626020, -1.938821108677920346 ) ) ;
#165771 = CARTESIAN_POINT ( 'NONE',  ( 6.343235766347262938, 8.493804042195527870, -1.599625672291281386 ) ) ;
#165772 = CARTESIAN_POINT ( 'NONE',  ( -9.332089804907933939, 9.781859615347734405, 1.040834085586084257E-14 ) ) ;
#165773 = CARTESIAN_POINT ( 'NONE',  ( 5.172599298813543633, 5.993452922492633839, -1.199719254218452047 ) ) ;
#165774 = CARTESIAN_POINT ( 'NONE',  ( 3.028250241984064228, 1.103615759228196325, 1.751372171329562688 ) ) ;
#165776 = CARTESIAN_POINT ( 'NONE',  ( -0.6823417656250246877, 0.1135416670080893753, 1.181850606188755259 ) ) ;
#165775 = FACE_OUTER_BOUND ( 'NONE', #45479, .T. ) ;
#165777 = ORIENTED_EDGE ( 'NONE', *, *, #37327, .F. ) ;
#165778 = CARTESIAN_POINT ( 'NONE',  ( 2.883697495508124042, -0.6696099726914479522, -2.198986239785024388 ) ) ;
#165779 = CARTESIAN_POINT ( 'NONE',  ( 8.514157279702022407, 10.95626946445095307, -1.443375672974063439 ) ) ;
#165781 = CARTESIAN_POINT ( 'NONE',  ( -3.285556943750000070, -3.259374999522044014, 0.000000000000000000 ) ) ;
#165780 = CARTESIAN_POINT ( 'NONE',  ( 5.885648082108188461, 8.920320958217979879, 1.082531754730549967 ) ) ;
#165782 = CARTESIAN_POINT ( 'NONE',  ( -10.38614328979761403, 3.507114751586604129, 5.996442624206741456 ) ) ;
#165783 = PRESENTATION_STYLE_ASSIGNMENT (( #132249 ) ) ;
#165784 = ORIENTED_EDGE ( 'NONE', *, *, #100023, .F. ) ;
#165785 = CARTESIAN_POINT ( 'NONE',  ( 0.000000000000000000, -7.246166700194011767, 9.579665964935665912 ) ) ;
#165786 = CARTESIAN_POINT ( 'NONE',  ( 4.043146078444789460, 0.09904687726844901841, 1.909973672635330910 ) ) ;
#165787 = CARTESIAN_POINT ( 'NONE',  ( 10.62873463776380056, 13.79999999999998295, 3.199999999999997957 ) ) ;
#165788 = CARTESIAN_POINT ( 'NONE',  ( 5.455954713372185516, 1.722626330383254745, -0.08824682005538657392 ) ) ;
#165789 = CARTESIAN_POINT ( 'NONE',  ( 3.942592416894859841, -1.490970858180176162, 1.357867534901323614 ) ) ;
#165790 = CARTESIAN_POINT ( 'NONE',  ( 5.590575961319281362, -0.5612465257360791382, 2.229044676911738687 ) ) ;
#165791 = CARTESIAN_POINT ( 'NONE',  ( -11.41381675112459781, 12.69999999999998863, -3.704697986577260682 ) ) ;
#165792 = CARTESIAN_POINT ( 'NONE',  ( 0.6103625832605160673, -2.195865045534075133, 0.2202409711149767024 ) ) ;
#165793 = CARTESIAN_POINT ( 'NONE',  ( -3.960390268967665328, 6.674186842887300131, 1.082531754730549967 ) ) ;
#165794 = CARTESIAN_POINT ( 'NONE',  ( 5.606658687911298955, 1.339352548545174937, -1.156898068784556255 ) ) ;
#165796 = CARTESIAN_POINT ( 'NONE',  ( 1.781587602986109742, 1.582980622272272653, 1.658122128702421261 ) ) ;
#165795 = CARTESIAN_POINT ( 'NONE',  ( 4.850785098639300408, 8.881276058379668825, -0.7998128361456481317 ) ) ;
#165797 = CARTESIAN_POINT ( 'NONE',  ( 0.2162406733101406298, -0.09061050886127393345, 1.738091409524551878 ) ) ;
#165798 = CARTESIAN_POINT ( 'NONE',  ( -5.772739544368596043, 9.956889578397179363, -0.7998128361456362523 ) ) ;
#165799 = CARTESIAN_POINT ( 'NONE',  ( -3.006876207180748217, 6.730049018344652190, -0.7998128361456481317 ) ) ;
#165800 = CARTESIAN_POINT ( 'NONE',  ( -0.6801582343750403048, -0.5364583329919083710, 1.178068619123807004 ) ) ;
#165801 = CARTESIAN_POINT ( 'NONE',  ( -8.158817897275659092, 15.51988520119759762, 8.845126866080887496 ) ) ;
#165802 = CARTESIAN_POINT ( 'NONE',  ( 0.1687529456618936941, -0.9278834597439933329, -1.960587321289827267 ) ) ;
#165803 = CARTESIAN_POINT ( 'NONE',  ( 2.589077643123653072, 1.706113014995232380, 1.074661422923957055 ) ) ;
#165804 = AXIS2_PLACEMENT_3D ( 'NONE', #167915, #151677, #68252 ) ;
#165805 = CARTESIAN_POINT ( 'NONE',  ( 1.499999999999989120, -0.1937499993171845625, 0.000000000000000000 ) ) ;
#165806 = CARTESIAN_POINT ( 'NONE',  ( 5.514262516685338511, -0.8683059565382322820, -1.719797162412556535 ) ) ;
#165807 = CARTESIAN_POINT ( 'NONE',  ( -0.6823417656250003738, 12.15104166700806054, 1.181850606188754593 ) ) ;
#165808 = CARTESIAN_POINT ( 'NONE',  ( 2.443850186789862100, -2.070980460497043651, 0.8039724962528942420 ) ) ;
#165809 = ORIENTED_EDGE ( 'NONE', *, *, #165616, .T. ) ;
#165810 = DIRECTION ( 'NONE',  ( -1.561251128379126077E-17, -1.301042606982605475E-17, -1.000000000000000000 ) ) ;
#165811 = FACE_BOUND ( 'NONE', #207427, .T. ) ;
#165812 = CARTESIAN_POINT ( 'NONE',  ( 7.730120138085914583, 12.17022392774227768, 0.7998128361456462443 ) ) ;
#165813 = FACE_OUTER_BOUND ( 'NONE', #176113, .T. ) ;
#165814 = CARTESIAN_POINT ( 'NONE',  ( 0.000000000000000000, 8.999999999999998224, 0.000000000000000000 ) ) ;
#165815 = CARTESIAN_POINT ( 'NONE',  ( 4.563825558218141509, -1.132311722701891510, 1.321849635945840706 ) ) ;
#165816 = CARTESIAN_POINT ( 'NONE',  ( 3.930091730393743710, 1.087902980620155891, 1.632394305395828304 ) ) ;
#165818 = CARTESIAN_POINT ( 'NONE',  ( -8.188761592974058701, 8.655902734665618325, -0.7216878364870278340 ) ) ;
#165817 = CARTESIAN_POINT ( 'NONE',  ( 5.359550796103802028, 5.147230771742885125, -0.7998128361456231517 ) ) ;
#165819 = CARTESIAN_POINT ( 'NONE',  ( -5.867692518273577740, 6.026634161543212187, 0.3546184694816056360 ) ) ;
#165820 = CARTESIAN_POINT ( 'NONE',  ( 8.367353357928214663, 12.91366268422496688, 1.040834085586084257E-14 ) ) ;
#165821 = CARTESIAN_POINT ( 'NONE',  ( 0.5903720789649337108, 1.061967407477812264, -1.768178413720230990 ) ) ;
#165822 = CARTESIAN_POINT ( 'NONE',  ( -7.426115451983156923, 9.686887332112256388, -1.599625672291263179 ) ) ;
#165823 = CARTESIAN_POINT ( 'NONE',  ( -2.887523529586332405, 5.352232636950553513, 1.082531754730560403 ) ) ;
#165824 = CARTESIAN_POINT ( 'NONE',  ( 1.762946358529001056, -1.599227303849257043, 1.600698272852623338 ) ) ;
#165825 = EDGE_LOOP ( 'NONE', ( #152915, #213645, #88764, #105170 ) ) ;
#165826 = CARTESIAN_POINT ( 'NONE',  ( 1.499999999999987566, -0.4437499993171847845, 0.000000000000000000 ) ) ;
#165827 = CARTESIAN_POINT ( 'NONE',  ( 3.004993591039197831, 1.578202713744047303, 1.003818400984110681 ) ) ;
#165828 = CARTESIAN_POINT ( 'NONE',  ( 1.898628203569406203, -0.8177110325628260679, -1.529257715385720307 ) ) ;
#165829 = CARTESIAN_POINT ( 'NONE',  ( 5.460537066722415567, -1.980877156148381335, -0.9378266216248376530 ) ) ;
#165830 = CARTESIAN_POINT ( 'NONE',  ( 0.1478802723770406002, -1.707511933842900564, -1.397569297917726550 ) ) ;
#165831 = CARTESIAN_POINT ( 'NONE',  ( 1.024374290915401442, 1.228313541842564138, -1.654675390109799693 ) ) ;
#165832 = CARTESIAN_POINT ( 'NONE',  ( 3.802622829840444751, 1.666041102563616816, 0.9975114776080131751 ) ) ;
#165833 = CARTESIAN_POINT ( 'NONE',  ( -4.161989969270909917, 5.878740935614591656, 1.443375672974064550 ) ) ;
#165834 = CARTESIAN_POINT ( 'NONE',  ( 5.378141472655761923, -1.040010688794581029, 1.554561134376866383 ) ) ;
#165835 = CARTESIAN_POINT ( 'NONE',  ( 0.5937500000000017764, -1.895863743164141191, -0.7852924748299565660 ) ) ;
#165836 = CARTESIAN_POINT ( 'NONE',  ( 1.404687167041647866, 13.32212500979552594, 0.2168455861850217548 ) ) ;
#165837 = CARTESIAN_POINT ( 'NONE',  ( 6.802112138117927920, -1.802125342305498146, 0.9040232568291312054 ) ) ;
#165838 = CARTESIAN_POINT ( 'NONE',  ( -0.6801582343750125492, 1.098958333674737720, -1.178068619123855409 ) ) ;
#165839 = CARTESIAN_POINT ( 'NONE',  ( 4.817029820108094995, 1.034167108704350024, -1.730865207599366240 ) ) ;
#165840 = CARTESIAN_POINT ( 'NONE',  ( -4.080641047588914994, 5.783833860318930320, -1.443375672974051449 ) ) ;
#165841 = CARTESIAN_POINT ( 'NONE',  ( 9.772729797352075920, 10.29593960653257234, -0.7998128361456281477 ) ) ;
#165842 = CARTESIAN_POINT ( 'NONE',  ( 4.634908411025333130, 6.500755460986618495, 1.599625672291268286 ) ) ;
#165844 = DIRECTION ( 'NONE',  ( 1.276756478318932585E-15, -1.000000000000000000, 1.665334536937738262E-16 ) ) ;
#165843 = CARTESIAN_POINT ( 'NONE',  ( 2.402731849113007190, 1.466575434288765800, -1.087121784572639527 ) ) ;
#165845 = CARTESIAN_POINT ( 'NONE',  ( 6.824425546749162130, -8.104785249476798015, -6.609253696060804373 ) ) ;
#165846 = CARTESIAN_POINT ( 'NONE',  ( -10.44369227015510404, 5.112964020592959180, 5.232143560358712087 ) ) ;
#165847 = ORIENTED_EDGE ( 'NONE', *, *, #103675, .F. ) ;
#165848 = CARTESIAN_POINT ( 'NONE',  ( -4.773879485343255347, 8.583626809626847987, 0.000000000000000000 ) ) ;
#165849 = EDGE_CURVE ( 'NONE', #126795, #190246, #197469, .T. ) ;
#165850 = CARTESIAN_POINT ( 'NONE',  ( -0.4350687514514777199, -7.666862915010147717, 10.91132967064556603 ) ) ;
#165851 = CARTESIAN_POINT ( 'NONE',  ( -9.820183334999905256, 10.35130206712171130, 1.040834085586084257E-14 ) ) ;
#165852 = CARTESIAN_POINT ( 'NONE',  ( 6.633471379370169174, -0.1512203817595116073, 1.986116118494333227 ) ) ;
#165853 = CARTESIAN_POINT ( 'NONE',  ( 0.5223349339509277822, -2.109880975928311031, 0.2119513895993754005 ) ) ;
#165854 = ORIENTED_EDGE ( 'NONE', *, *, #187238, .F. ) ;
#165855 = CARTESIAN_POINT ( 'NONE',  ( -6.129167961829681488, 9.308390501180058507, -1.199719254218452047 ) ) ;
#165856 = CARTESIAN_POINT ( 'NONE',  ( 4.143988507271280319, 7.986403691791820414, -0.7998128361456221525 ) ) ;
#165857 = COLOUR_RGB ( '', 0.66274510, 0.83137255, 0.94901961) ;
#165858 = CARTESIAN_POINT ( 'NONE',  ( 6.543830163797104582, 0.7912256320986108538, -1.903158165889913045 ) ) ;
#165859 = CARTESIAN_POINT ( 'NONE',  ( 5.098279808040273586, -0.2930726886911337870, 1.994869512123042199 ) ) ;
#165860 = ORIENTED_EDGE ( 'NONE', *, *, #113967, .F. ) ;
#165861 = CARTESIAN_POINT ( 'NONE',  ( 2.884486378366592607, 6.439576038332424979, 0.3703176727237925681 ) ) ;
#165862 = CARTESIAN_POINT ( 'NONE',  ( -0.2108831679770959699, 2.036692374882024037, -2.313561348563981657 ) ) ;
#165865 = ORIENTED_EDGE ( 'NONE', *, *, #129225, .T. ) ;
#165864 = CARTESIAN_POINT ( 'NONE',  ( -1.123270288250318494, 3.235197346350006331, -0.7749999999993560929 ) ) ;
#165863 = CARTESIAN_POINT ( 'NONE',  ( -7.130662446144611977, 7.283804040115648526, 0.000000000000000000 ) ) ;
#165866 = CARTESIAN_POINT ( 'NONE',  ( 4.623177087595867540, 8.455029494522658950, -0.3425024339245314464 ) ) ;
#165867 = CARTESIAN_POINT ( 'NONE',  ( 5.026720154644213068, 1.994564127574052215, -0.2930270067487000252 ) ) ;
#165868 = CARTESIAN_POINT ( 'NONE',  ( 4.769393013670423009, 1.062472638025207416, 1.503447196605799174 ) ) ;
#165869 = CARTESIAN_POINT ( 'NONE',  ( -0.02338929933904005179, 0.7691289590099622542, -1.796825425911799723 ) ) ;
#165870 = CARTESIAN_POINT ( 'NONE',  ( 3.457953323470845941, 0.5611853863643158080, -2.238310864172543546 ) ) ;
#165871 = CARTESIAN_POINT ( 'NONE',  ( 8.005163354226054295, 8.304055099544019214, 0.000000000000000000 ) ) ;
#165872 = CARTESIAN_POINT ( 'NONE',  ( 4.991577004318280331, 1.598001195387260154, 1.455802845438579407 ) ) ;
#165873 = CARTESIAN_POINT ( 'NONE',  ( 6.421758314367153275, 10.64380180007036891, -0.7998128361456291469 ) ) ;
#165874 = CARTESIAN_POINT ( 'NONE',  ( 0.5912263705248020917, -0.6977439394254668636, 1.812568619595144925 ) ) ;
#165875 = CARTESIAN_POINT ( 'NONE',  ( -3.924195396151603177, 6.665646164563756138, 1.199719254218464037 ) ) ;
#165876 = CIRCLE ( 'NONE', #127944, 0.08000000000000020983 ) ;
#165877 = CARTESIAN_POINT ( 'NONE',  ( 0.9486429539266807431, 2.917910930033675854, -1.028101543437250465 ) ) ;
#165878 = CARTESIAN_POINT ( 'NONE',  ( -5.492988512192097161, 6.437516681426083132, 1.199719254218452935 ) ) ;
#165879 = CARTESIAN_POINT ( 'NONE',  ( 3.889402362484274622, 1.354500474538382626, 1.290456140434749654 ) ) ;
#165880 = EDGE_CURVE ( 'NONE', #39666, #143793, #113844, .T. ) ;
#165883 = CARTESIAN_POINT ( 'NONE',  ( -6.261886844665283114, 8.398896966899865646, 1.599625672291269396 ) ) ;
#165882 = CARTESIAN_POINT ( 'NONE',  ( -1.500000000000015099, -0.7979166659838445863, 0.8660254037844403729 ) ) ;
#165881 = CARTESIAN_POINT ( 'NONE',  ( 1.617294888471169312, 1.591762500684265946, 1.059657513450793953 ) ) ;
#165884 = CARTESIAN_POINT ( 'NONE',  ( 2.438337523484556790, 1.039148161723329578, -1.946916322307743474 ) ) ;
#165885 = B_SPLINE_CURVE_WITH_KNOTS ( 'NONE', 3,
 ( #33676, #186317, #167948, #136531, #18482, #153840 ),
 .UNSPECIFIED., .F., .F.,
 ( 4, 2, 4 ),
 ( 0.000000000000000000, 0.001225895755212353007, 0.002451791510424706014 ),
 .UNSPECIFIED. ) ;
#165886 = CARTESIAN_POINT ( 'NONE',  ( -5.786256696412555911, 6.075953140482280190, 0.5845640519336701146 ) ) ;
#165887 = CARTESIAN_POINT ( 'NONE',  ( 3.842846474469570062, 6.570739089268092137, -1.199719254218452047 ) ) ;
#165888 = CARTESIAN_POINT ( 'NONE',  ( 7.973603738168424826, 8.475161580717541554, 0.000000000000000000 ) ) ;
#165889 = CARTESIAN_POINT ( 'NONE',  ( -3.490334480514268645, 6.159475096320226939, -1.199719254218452935 ) ) ;
#165890 = CARTESIAN_POINT ( 'NONE',  ( -7.390603132780795725, 8.755363422066633206, -1.082531754730549967 ) ) ;
#165891 = CARTESIAN_POINT ( 'NONE',  ( 0.4386656386161046917, 0.3326637607320662160, 1.942932543480476726 ) ) ;
#165892 = CARTESIAN_POINT ( 'NONE',  ( 0.3238087740765641653, -0.1086241252120211664, 2.305164108462977701 ) ) ;
#165893 = CARTESIAN_POINT ( 'NONE',  ( 1.398799877119625501, 0.3793605821263335565, 1.924665094374561791 ) ) ;
#165894 = CARTESIAN_POINT ( 'NONE',  ( 4.575086232891404592, 1.883663672660494504, 0.8406736911329756312 ) ) ;
#165895 = CARTESIAN_POINT ( 'NONE',  ( 4.961921032921539521, 7.772363057508363759, -1.082531754730549078 ) ) ;
#165896 = CARTESIAN_POINT ( 'NONE',  ( 4.694866332082116678, 8.699370830729650450, 0.7998128361456341429 ) ) ;
#165897 = ORIENTED_EDGE ( 'NONE', *, *, #178287, .F. ) ;
#165898 = CARTESIAN_POINT ( 'NONE',  ( 6.412643469139427843, 10.42524178073059993, -0.7216878364870267237 ) ) ;
#165899 = CARTESIAN_POINT ( 'NONE',  ( -1.364683531249997417, 4.571875000341417028, 1.214306433183764966E-14 ) ) ;
#165900 = LINE ( 'NONE', #136610, #159531 ) ;
#165901 = CARTESIAN_POINT ( 'NONE',  ( 3.456965981360264895, 6.016582164020185530, -1.082531754730543971 ) ) ;
#165902 = CARTESIAN_POINT ( 'NONE',  ( 0.9015274132509668581, -1.862984440646279438, 1.114554472006025865 ) ) ;
#165904 = CARTESIAN_POINT ( 'NONE',  ( 5.935073298327618652, -1.338256116417003927, -1.264887592264056559 ) ) ;
#165903 = CARTESIAN_POINT ( 'NONE',  ( 0.000000000000000000, -3.499999999999999556, 3.017800438942086050 ) ) ;
#165905 = CARTESIAN_POINT ( 'NONE',  ( -2.269535221383012225, 3.870433085555832431, 11.40607948006776873 ) ) ;
#165906 = LINE ( 'NONE', #200510, #73856 ) ;
#165907 = CARTESIAN_POINT ( 'NONE',  ( 1.721729502718066795, -1.034818790731323990, -1.558030248997283040 ) ) ;
#165908 = CARTESIAN_POINT ( 'NONE',  ( 5.184929619776310616, -0.2588774643964042999, -2.145956309214678726 ) ) ;
#165909 = CARTESIAN_POINT ( 'NONE',  ( -6.016097364521681534, 6.072308155256833651, 0.6301904134648171896 ) ) ;
#165910 = CARTESIAN_POINT ( 'NONE',  ( 5.796475149741596056, 7.337953333587568849, -1.293683646293428913 ) ) ;
#165911 = CARTESIAN_POINT ( 'NONE',  ( -1.364683531250012516, 5.051041667008085767, -0.7879004041258300672 ) ) ;
#165912 = CARTESIAN_POINT ( 'NONE',  ( 0.7856316122640573107, 1.842795011522216697, -0.5104879603500325214 ) ) ;
#165913 = CARTESIAN_POINT ( 'NONE',  ( 2.992752380588555638, 1.518849080061919654, -0.9082622674112093009 ) ) ;
#165914 = CARTESIAN_POINT ( 'NONE',  ( 0.7856316122640573107, 1.842795011522216697, -0.5104879603500325214 ) ) ;
#165916 = CARTESIAN_POINT ( 'NONE',  ( 3.972214814312221343, -1.895280843596976350, -0.2773303961090283765 ) ) ;
#165915 = CARTESIAN_POINT ( 'NONE',  ( 6.493979435825333546, -7.868711954889218596, -6.493979435825359303 ) ) ;
#165917 = CARTESIAN_POINT ( 'NONE',  ( 5.160591359625510854, -0.6618325696593707619, -1.855173450206740071 ) ) ;
#165918 = CARTESIAN_POINT ( 'NONE',  ( 1.371502371489873751, -1.821557607348308405, -1.085495857948336251 ) ) ;
#165919 = LINE ( 'NONE', #17504, #79169 ) ;
#165920 = CARTESIAN_POINT ( 'NONE',  ( 3.766346201128992988, -1.256895078192099335, 1.385637336983977397 ) ) ;
#165922 = EDGE_LOOP ( 'NONE', ( #81477, #91015, #172915, #154897 ) ) ;
#165921 = CARTESIAN_POINT ( 'NONE',  ( 0.3459771380207553593, 1.820543102168985961, 0.1377627428671979182 ) ) ;
#165924 = CARTESIAN_POINT ( 'NONE',  ( -5.492461626867567226, 6.540864998501174199, 1.082531754730549078 ) ) ;
#165923 = CARTESIAN_POINT ( 'NONE',  ( 2.930518499080053907, 1.225513248159842083, -1.835134156090315605 ) ) ;
#165925 = AXIS2_PLACEMENT_3D ( 'NONE', #101226, #34098, #166234 ) ;
#165926 = CARTESIAN_POINT ( 'NONE',  ( 0.6823417656249899377, 4.238541667008085767, -1.181850606188754593 ) ) ;
#165927 = CARTESIAN_POINT ( 'NONE',  ( 1.416547059616825699, 0.8341270235591256021, 1.886661834507087798 ) ) ;
#165928 = CARTESIAN_POINT ( 'NONE',  ( 5.612185521052973414, 8.634967976948757951, -1.199719254218440723 ) ) ;
#165929 = CARTESIAN_POINT ( 'NONE',  ( -8.533967624797991647, 12.04371376465130439, -1.199719254218446718 ) ) ;
#165930 = CARTESIAN_POINT ( 'NONE',  ( -9.132253115921022513, 1.016282880930314603, -8.222717639126782885 ) ) ;
#165931 = CARTESIAN_POINT ( 'NONE',  ( 0.000000000000000000, 18.91999999999999815, 0.000000000000000000 ) ) ;
#165932 = CARTESIAN_POINT ( 'NONE',  ( 6.416268857797894576, -1.911816439625917852, 0.05404522429636184067 ) ) ;
#165933 = VERTEX_POINT ( 'NONE', #114891 ) ;
#165934 = CARTESIAN_POINT ( 'NONE',  ( 4.527825515032589898, 2.008996319933327612, -0.4998958796476050681 ) ) ;
#165935 = CARTESIAN_POINT ( 'NONE',  ( -1.402160292154681736E-14, -0.8656249996585829720, 1.575800808251672791 ) ) ;
#165936 = CARTESIAN_POINT ( 'NONE',  ( 1.880366631079612771, -1.158069840294423392, 1.825029014904603342 ) ) ;
#165937 = CARTESIAN_POINT ( 'NONE',  ( -5.432786300537782331, 7.535064667520821047, -1.248352293942560642 ) ) ;
#165938 = CARTESIAN_POINT ( 'NONE',  ( 2.350265711909118593, 0.9499565981557709371, -1.782299418695271198 ) ) ;
#165939 = PLANE ( 'NONE',  #28663 ) ;
#165940 = ORIENTED_EDGE ( 'NONE', *, *, #94477, .T. ) ;
#165942 = CARTESIAN_POINT ( 'NONE',  ( 8.432808358020016826, 10.86136238915529084, 1.443375672974076540 ) ) ;
#165941 = CARTESIAN_POINT ( 'NONE',  ( -1.737500000000000266, -3.208333333333333925, -3.009438278150923907 ) ) ;
#165943 = CYLINDRICAL_SURFACE ( 'NONE', #78619, 0.09999999999999982514 ) ;
#165944 = CARTESIAN_POINT ( 'NONE',  ( 0.3566581422463632189, -1.900417414521380133, -0.6748426577906708745 ) ) ;
#165945 = CARTESIAN_POINT ( 'NONE',  ( 6.639320575229255894, 7.629137130509070275, 2.703262396134015866 ) ) ;
#165946 = CARTESIAN_POINT ( 'NONE',  ( 5.249643141573060667, 2.189086832579402842, -0.1069518675670885766 ) ) ;
#165947 = CARTESIAN_POINT ( 'NONE',  ( -1.499999999999997780, 3.681250000682819046, 1.214306433183764966E-14 ) ) ;
#165948 = CARTESIAN_POINT ( 'NONE',  ( 3.744317949583543470, 1.018843395500759197, -1.618198357137661469 ) ) ;
#165949 = CARTESIAN_POINT ( 'NONE',  ( -5.742041750587549842, 6.657802449562273850, 1.199719254218450271 ) ) ;
#165950 = CARTESIAN_POINT ( 'NONE',  ( 3.592547517496925913, 5.214391408544949869, -1.443375672974058777 ) ) ;
#165952 = CARTESIAN_POINT ( 'NONE',  ( 2.618767733003044551, 0.2496279305150179983, 2.000855661889962445 ) ) ;
#165951 = CARTESIAN_POINT ( 'NONE',  ( 5.630352418794719149, 6.139657267270441920, -0.8181431533968346326 ) ) ;
#165953 = CARTESIAN_POINT ( 'NONE',  ( -1.402160292154681736E-14, 11.98437500034140335, 1.575800808251682339 ) ) ;
#165955 = CARTESIAN_POINT ( 'NONE',  ( -5.438755897737433287, 6.374245297895642537, -1.199719254218453823 ) ) ;
#165954 = CARTESIAN_POINT ( 'NONE',  ( 0.4336627441306003528, -1.626622142924066594, -1.615526755278140492 ) ) ;
#165956 = CARTESIAN_POINT ( 'NONE',  ( 4.190264469598516506, -1.706116514292443931, -0.2520994348873573654 ) ) ;
#165957 = FACE_OUTER_BOUND ( 'NONE', #177739, .T. ) ;
#165958 = CARTESIAN_POINT ( 'NONE',  ( 2.822068529938852155, 6.444163718237301275, -0.7998128361456291469 ) ) ;
#165959 = CARTESIAN_POINT ( 'NONE',  ( -4.905110356762790502, 4.827649200395154772, -0.06592220986076716138 ) ) ;
#165960 = CARTESIAN_POINT ( 'NONE',  ( 0.9593383959572501229, 1.601786533887459507, 1.132500672181527168 ) ) ;
#165961 = DIRECTION ( 'NONE',  ( 0.000000000000000000, 8.546850786086437571E-32, 1.000000000000000000 ) ) ;
#165962 = CARTESIAN_POINT ( 'NONE',  ( 5.355634372598031767, 6.206993841907870291, -1.199719254218445830 ) ) ;
#165963 = CARTESIAN_POINT ( 'NONE',  ( 0.1753634416057497925, 7.629137130509101361, -2.744001747789548418 ) ) ;
#165964 = COLOUR_RGB ( '', 0.31764706, 0.68627451, 0.89019608) ;
#165965 = ORIENTED_EDGE ( 'NONE', *, *, #63237, .F. ) ;
#165966 = CARTESIAN_POINT ( 'NONE',  ( 5.408800935855493819, -0.4461688933581753336, -1.755527745762341718 ) ) ;
#165967 = EDGE_LOOP ( 'NONE', ( #129393, #42897, #43579, #35578, #176539, #115836, #48581, #180958, #34256, #6518, #119384, #69752, #158121 ) ) ;
#165968 = CARTESIAN_POINT ( 'NONE',  ( 7.178115983792402233, 7.339166500704784823, 0.7998128361456281477 ) ) ;
#165969 = CARTESIAN_POINT ( 'NONE',  ( 6.890000000000050306, -0.002781820520068867264, 1.999840353888074240 ) ) ;
#165970 = CARTESIAN_POINT ( 'NONE',  ( 4.793523346383269157, 1.688353701584244915, -0.6568948891843768845 ) ) ;
#165971 = CARTESIAN_POINT ( 'NONE',  ( 7.499068361690118145, 7.921536974826172361, -0.7216878364870317197 ) ) ;
#165972 = CARTESIAN_POINT ( 'NONE',  ( 2.277354866853175341, 5.622569341069810989, -0.5665490036073304037 ) ) ;
#165973 = CARTESIAN_POINT ( 'NONE',  ( 5.688518940989607309, 6.102662425301288884, -0.7322136710279708582 ) ) ;
#165974 = ORIENTED_EDGE ( 'NONE', *, *, #76499, .F. ) ;
#165975 = EDGE_CURVE ( 'NONE', #78562, #112702, #1045, .T. ) ;
#165977 = CARTESIAN_POINT ( 'NONE',  ( -0.6823417656250003738, 15.15104166700806410, 1.181850606188754593 ) ) ;
#165976 = CARTESIAN_POINT ( 'NONE',  ( 6.338329682780378782, -0.9945775373912761896, 1.572806762946916903 ) ) ;
#165978 = CARTESIAN_POINT ( 'NONE',  ( 3.567908551050925858, -0.9411222629213971125, 1.668380548182837542 ) ) ;
#165979 = CARTESIAN_POINT ( 'NONE',  ( -6.710064404886794343, -7.791858861492868549, -6.725651841507029438 ) ) ;
#165980 = SURFACE_SIDE_STYLE ('',( #65256 ) ) ;
#165981 = DIRECTION ( 'NONE',  ( 0.000000000000000000, 0.000000000000000000, -1.000000000000000000 ) ) ;
#165982 = CARTESIAN_POINT ( 'NONE',  ( 5.314433026876846711, 9.143996264757578984, -0.7216878364870267237 ) ) ;
#165984 = CARTESIAN_POINT ( 'NONE',  ( 5.401600794869550803, -2.065136407520694828, 0.4665587172485561318 ) ) ;
#165983 = CARTESIAN_POINT ( 'NONE',  ( -10.15469386695561482, 10.94949038764413096, 1.040834085586084257E-14 ) ) ;
#165985 = CARTESIAN_POINT ( 'NONE',  ( 0.6730137850648570952, -2.035850703004048246, -0.7271551459356735414 ) ) ;
#165986 = CARTESIAN_POINT ( 'NONE',  ( -5.041653019435350380, 6.975290837464928728, -1.599625672291271394 ) ) ;
#165987 = EDGE_CURVE ( 'NONE', #42674, #112218, #16233, .T. ) ;
#165988 = CARTESIAN_POINT ( 'NONE',  ( 5.903649544107831382, 5.852288987739402870, -0.7998128361456481317 ) ) ;
#165989 = CARTESIAN_POINT ( 'NONE',  ( 0.8502975112493587062, 0.5252643332615304361, 1.748389446526978031 ) ) ;
#165990 = CARTESIAN_POINT ( 'NONE',  ( -4.603156847039612920, 5.329103395422994716, 1.199719254218462483 ) ) ;
#165991 = CARTESIAN_POINT ( 'NONE',  ( 4.049673113991675955, 0.6152068410551281286, -1.718917501701062056 ) ) ;
#165992 = CARTESIAN_POINT ( 'NONE',  ( 11.99987416209243385, 8.248970243831804439, 3.607522456176011971 ) ) ;
#165993 = CARTESIAN_POINT ( 'NONE',  ( 2.425908952446104827, -1.891012092455180760, 0.2844710172774585488 ) ) ;
#165994 = ORIENTED_EDGE ( 'NONE', *, *, #184771, .F. ) ;
#165995 = CARTESIAN_POINT ( 'NONE',  ( 2.857809274136946520, -0.6206004443085939570, 1.869272957157315007 ) ) ;
#165996 = CARTESIAN_POINT ( 'NONE',  ( 5.337426827915986216, 0.7834791095375337466, -1.777179163755914448 ) ) ;
#165997 = CARTESIAN_POINT ( 'NONE',  ( -2.830620210203090181, 6.524417021870718258, 0.000000000000000000 ) ) ;
#165999 = CARTESIAN_POINT ( 'NONE',  ( 5.642871316567687145, 2.044259226470702462, 0.5637153772257290640 ) ) ;
#165998 = CARTESIAN_POINT ( 'NONE',  ( 7.180978637093494044, 8.406838493811077839, -1.199719254218452047 ) ) ;
#166000 = CARTESIAN_POINT ( 'NONE',  ( -3.276785236921248415E-13, -7.217880409008451181, 9.581975256308824740 ) ) ;
#166001 = CARTESIAN_POINT ( 'NONE',  ( 3.088426618631805454, -1.137173348016347063, 1.537276688398482083 ) ) ;
#166002 = CARTESIAN_POINT ( 'NONE',  ( 5.882017484636844706, 6.163768100491378910, 0.8443116549854499109 ) ) ;
#166003 = DIRECTION ( 'NONE',  ( 2.345077562848782505E-16, 0.000000000000000000, 1.000000000000000000 ) ) ;
#166004 = VERTEX_POINT ( 'NONE', #199249 ) ;
#166005 = CARTESIAN_POINT ( 'NONE',  ( -9.367496997601305608, 14.48154074412967596, 7.499999999995371702 ) ) ;
#166006 = CARTESIAN_POINT ( 'NONE',  ( 3.542423274920540432, 7.354853930707762721, -1.734723475976807094E-15 ) ) ;
#166007 = VECTOR ( 'NONE', #198633, 1000.000000000000000 ) ;
#166008 = LINE ( 'NONE', #21850, #199965 ) ;
#166009 = CARTESIAN_POINT ( 'NONE',  ( 5.461492464141177727, 0.3521552718798379722, -1.791230276788812414 ) ) ;
#166010 = CARTESIAN_POINT ( 'NONE',  ( 10.99947830037066510, -9.912501460265211506, -0.1071380031274375144 ) ) ;
#166011 = CARTESIAN_POINT ( 'NONE',  ( -7.836249599018719536, 12.08611559892311504, 0.7216878364870478180 ) ) ;
#166012 = CARTESIAN_POINT ( 'NONE',  ( -6.365373075063135211, 6.924066019909299818, 0.8511317711424144505 ) ) ;
#166013 = CARTESIAN_POINT ( 'NONE',  ( -0.3544712801349413911, 3.975028838742715287, -0.9637995819944503717 ) ) ;
#166014 = CARTESIAN_POINT ( 'NONE',  ( 5.946149726614579301, 1.868617323842229894, 0.09011704611043556967 ) ) ;
#166015 = CARTESIAN_POINT ( 'NONE',  ( 7.832860060393120882, 10.16142270859057462, 1.599625672291281386 ) ) ;
#166016 = EDGE_CURVE ( 'NONE', #74942, #82527, #69711, .T. ) ;
#166017 = CARTESIAN_POINT ( 'NONE',  ( -3.761497552787613330, 6.475832013972435242, 1.199719254218464037 ) ) ;
#166018 = CARTESIAN_POINT ( 'NONE',  ( 2.855963913973019963, 6.483708332943829866, 0.000000000000000000 ) ) ;
#166019 = CARTESIAN_POINT ( 'NONE',  ( -8.012344526598182026E-15, 10.35937500034139624, -1.575800808251669460 ) ) ;
#166020 = CARTESIAN_POINT ( 'NONE',  ( -5.949330478298285207, 5.835307067636438028, 0.7998128361456341429 ) ) ;
#166021 = CIRCLE ( 'NONE', #214360, 0.07999999999999983513 ) ;
#166022 = CARTESIAN_POINT ( 'NONE',  ( -3.594320120954326292, 6.247105003538398371, 1.082531754730549967 ) ) ;
#166023 = CARTESIAN_POINT ( 'NONE',  ( -4.771579997005698459, 7.654261532226910525, -1.199719254218452047 ) ) ;
#166024 = CARTESIAN_POINT ( 'NONE',  ( 0.6024989291013755910, 2.064475859885641640, 0.1558578049991043990 ) ) ;
#166025 = CARTESIAN_POINT ( 'NONE',  ( 1.406030203601447592, -1.179493747730875342, -1.758069577626440116 ) ) ;
#166026 = CARTESIAN_POINT ( 'NONE',  ( 7.228468454380276853, 11.58496363008569574, 1.040834085586084257E-14 ) ) ;
#166027 = ADVANCED_FACE ( 'NONE', ( #99645 ), #165712, .F. ) ;
#166028 = CARTESIAN_POINT ( 'NONE',  ( 6.649288540346695697, 1.804226486660088558, -1.015068834323729297 ) ) ;
#166030 = CARTESIAN_POINT ( 'NONE',  ( 4.433499500630886381, 7.080826916883525612, -1.109343814354251112 ) ) ;
#166029 = CARTESIAN_POINT ( 'NONE',  ( 2.067674361007607597, -1.131582805410412673, 1.452419944642673100 ) ) ;
#166031 = CARTESIAN_POINT ( 'NONE',  ( 5.829642864196162400, 7.824335979694092558, 1.443375672974062551 ) ) ;
#166033 = FACE_OUTER_BOUND ( 'NONE', #132713, .T. ) ;
#166032 = FACE_OUTER_BOUND ( 'NONE', #75710, .T. ) ;
#166034 = CARTESIAN_POINT ( 'NONE',  ( 1.869451396563295065, 2.192715141705191773, -0.6681815460085840375 ) ) ;
#166036 = CARTESIAN_POINT ( 'NONE',  ( 0.2333690889706959148, 4.088440985731725874, -2.608190362703251441 ) ) ;
#166035 = CARTESIAN_POINT ( 'NONE',  ( -4.492294583947431086, 8.028511867738693297, 2.499999999999999556 ) ) ;
#166037 = CARTESIAN_POINT ( 'NONE',  ( 2.742330423940505302, 1.058908597569432120, -1.592262909973440888 ) ) ;
#166038 = EDGE_CURVE ( 'NONE', #179210, #101997, #14084, .T. ) ;
#166039 = ORIENTED_EDGE ( 'NONE', *, *, #145044, .T. ) ;
#166040 = CARTESIAN_POINT ( 'NONE',  ( 7.931156673870037643, 8.355363662377600420, -0.7216878364870267237 ) ) ;
#166041 = CARTESIAN_POINT ( 'NONE',  ( 1.142838885277572825, 1.941394601512283602, 0.5327644489504842484 ) ) ;
#166042 = CARTESIAN_POINT ( 'NONE',  ( 1.217545072937670225, 0.3881152535412414339, -1.922811240370206232 ) ) ;
#166044 = CARTESIAN_POINT ( 'NONE',  ( -9.348561386899501002, 3.999985931113709814, -7.001914024221969512 ) ) ;
#166043 = CARTESIAN_POINT ( 'NONE',  ( -6.991200766141138168, 11.30815132714001159, 0.7998128361456481317 ) ) ;
#166045 = CARTESIAN_POINT ( 'NONE',  ( -9.915825940873133959, 4.173851563286998356, 6.175246223022227809 ) ) ;
#166047 = CARTESIAN_POINT ( 'NONE',  ( 1.955557038561178240, 1.765385265556310701, -0.1263916157485909797 ) ) ;
#166046 = CARTESIAN_POINT ( 'NONE',  ( 3.468770583794348550, 0.05092928562340763576, -2.090184462658881248 ) ) ;
#166048 = CARTESIAN_POINT ( 'NONE',  ( 1.499999999999993117, 12.10416666666666607, 0.8660254037844408170 ) ) ;
#166050 = CARTESIAN_POINT ( 'NONE',  ( 4.980587577705724911, -0.2770739538935252932, -2.275404589957805701 ) ) ;
#166049 = DIRECTION ( 'NONE',  ( -0.6507913734559640506, -0.7592566023653004592, 0.000000000000000000 ) ) ;
#166051 = CARTESIAN_POINT ( 'NONE',  ( 2.870765623479579531, 1.652405209062355773, -0.5463526510798635272 ) ) ;
#166052 = CARTESIAN_POINT ( 'NONE',  ( 10.38962578677386084, 11.01565159419135043, 0.000000000000000000 ) ) ;
#166053 = CARTESIAN_POINT ( 'NONE',  ( 4.037295881819344956, 7.932205305423044805, -0.7998128361456361413 ) ) ;
#166054 = CARTESIAN_POINT ( 'NONE',  ( 3.637800481086241433, 0.04416708034036923719, -1.733463101117929339 ) ) ;
#166055 = CARTESIAN_POINT ( 'NONE',  ( 3.227178390111482553, -2.005013095889785824, -0.8334813368568798619 ) ) ;
#166056 = CARTESIAN_POINT ( 'NONE',  ( 5.345992642490140057, 5.131412925860272090, 1.040834085586084257E-14 ) ) ;
#166057 = CARTESIAN_POINT ( 'NONE',  ( 5.911342272548038679, -1.897112096406332382, 0.6839327336411115121 ) ) ;
#166058 = CARTESIAN_POINT ( 'NONE',  ( 0.9687500000000008882, 0.7852924748299362490, -1.895863743164110327 ) ) ;
#166059 = CARTESIAN_POINT ( 'NONE',  ( 1.499999999999990896, 4.806250000682819490, 1.214306433183764966E-14 ) ) ;
#166060 = CARTESIAN_POINT ( 'NONE',  ( 2.450113916266524416, 1.925923877722035105, 0.04935297016485720029 ) ) ;
#166062 = B_SPLINE_CURVE_WITH_KNOTS ( 'NONE', 3,
 ( #4146, #89726, #70217, #155774, #104901, #153636, #102752, #57204, #107081, #173102, #88647, #6288, #72362, #55070, #138463, #24683, #37748, #121219, #8435, #168808, #90788, #20413, #56135, #136328, #202347, #169869, #71284, #181340, #74524, #92929, #209829, #190386, #206638, #147796, #111354, #143833, #192516, #165097, #42043, #76643, #110289, #207711, #126555, #59333, #157922, #25754, #32967, #141699, #77712, #193597, #109230, #108156, #15626, #177359, #174182, #75589, #45238, #28973, #191450, #125488, #91866, #158974, #61465, #127631, #95058, #10569, #44169, #161107, #43115, #99043, #81715, #115349, #197586, #175240, #140626, #26825, #176298, #213814, #9516, #142759, #58271, #65433, #208765, #131584, #60391, #27901, #93996, #160037, #11641, #49229, #124428, #69703, #117478, #16689, #148847, #184525, #3625, #53474, #38295, #51355, #166158, #101147, #34024, #135805, #182394, #201829, #134758, #183470, #82773, #119611, #202901, #20946, #200766, #102228, #36146, #18822, #118542, #185596, #149925, #84907, #104373, #66491, #1494, #50286, #150995, #153114, #132632, #85979, #420, #120692, #198638, #35077, #152054, #116405, #100097, #87043, #37225, #103299, #52416, #17745, #83833, #67559, #4687, #133703, #68634, #199708, #167235, #70762, #169360, #2560, #136875, #168298, #19894, #54545, #186668, #126027, #59876, #155253, #190928, #140092, #205040, #139018, #40447, #24157, #142232, #107630, #76128, #42592, #123907, #206118, #8991, #55611, #208244, #10052, #56685, #172576, #75066, #122851, #157398, #73999, #108698, #188813, #121766, #173663, #90260, #57749, #189876, #6834, #5755, #72913, #203964, #156328, #92413, #71833, #25236, #170418, #191989, #22006, #106548, #91339, #137943, #41518, #7910, #141178, #187733, #88117, #207188, #58813, #171494, #174726, #89200, #124967, #26299, #39363, #43655, #158452, #23085, #154187, #105459, #161663, #29521, #13258, #163794, #160578, #146493, #93473, #80398, #27373, #78257, #194139, #177908, #81466, #46855, #15372, #130295, #63079, #193068, #60947, #213564, #176834, #112969, #79330, #111906, #95614, #212512, #145447, #147543, #96682, #12185, #159512, #28448, #94538, #30595, #45788, #178981, #162731, #64153, #211445, #129246, #14303, #144381, #210380, #62022, #128177, #195219, #11111, #196284, #127104, #47931, #114044, #180037, #31659, #97737, #65186, #131340, #197334, #109772, #175779, #77185, #143308, #44720, #110827, #209299, #48976, #171, #148602, #53224, #151806, #119355, #50029, #17497, #116153, #51095, #133447, #19645, #182140, #117221, #136621, #115093, #3379, #70505, #183218, #185342, #164844, #118288, #181090, #152858, #32708, #67306, #184274, #16436, #98789, #36965, #85718, #35898, #166987, #82515, #66238, #34823, #84655, #199453, #100898, #33770, #132387, #103046, #201578, #99849, #69446, #83584, #18577, #150744, #135554, #4436, #198387, #165912, #169101, #2306, #149666, #68382, #1245, #20698, #86789, #200516, #134512, #52161, #101975, #168043, #153932, #92154, #55357, #205862, #107373, #22827, #21752, #140914, #91080, #104115, #203710, #173394, #157140, #105195, #121509, #123655, #72660, #57495, #189617, #8732, #138756, #172315, #41264, #187482, #9796, #24977, #26041, #108445, #39111, #158207, #88942, #40181, #74813, #137689, #154995, #204775, #206927, #171232, #58557, #6581 ),
 .UNSPECIFIED., .F., .F.,
 ( 4, 1, 1, 1, 1, 1, 1, 1, 1, 1, 1, 1, 1, 1, 1, 1, 1, 1, 1, 1, 1, 1, 1, 1, 1, 1, 1, 1, 1, 1, 1, 1, 1, 1, 1, 1, 1, 1, 1, 1, 1, 1, 1, 1, 1, 1, 1, 1, 1, 1, 1, 1, 1, 1, 1, 1, 1, 1, 1, 1, 1, 1, 1, 1, 1, 1, 1, 1, 1, 1, 1, 1, 1, 1, 1, 1, 1, 1, 1, 1, 1, 1, 1, 1, 1, 1, 1, 1, 1, 1, 1, 1, 1, 1, 1, 1, 1, 1, 1, 1, 1, 1, 1, 1, 1, 1, 1, 1, 1, 1, 1, 1, 1, 1, 1, 1, 1, 1, 1, 1, 1, 1, 1, 1, 1, 1, 1, 1, 1, 1, 1, 1, 1, 1, 1, 1, 1, 1, 1, 1, 1, 1, 1, 1, 1, 1, 1, 1, 1, 1, 1, 1, 1, 1, 1, 1, 1, 1, 1, 1, 1, 1, 1, 1, 1, 1, 1, 1, 1, 1, 1, 1, 1, 1, 1, 1, 1, 1, 1, 1, 1, 1, 1, 1, 1, 1, 1, 1, 1, 1, 1, 1, 1, 1, 1, 1, 1, 1, 1, 1, 1, 1, 1, 1, 1, 1, 1, 1, 1, 1, 1, 1, 1, 1, 1, 1, 1, 1, 1, 1, 1, 1, 1, 1, 1, 1, 1, 1, 1, 1, 1, 1, 1, 1, 1, 1, 1, 1, 1, 1, 1, 1, 1, 1, 1, 1, 1, 1, 1, 1, 1, 1, 1, 1, 1, 1, 1, 1, 1, 1, 1, 1, 1, 1, 1, 1, 1, 1, 1, 1, 1, 1, 1, 1, 1, 1, 1, 1, 1, 1, 1, 1, 1, 1, 1, 1, 1, 1, 1, 1, 1, 1, 1, 1, 1, 1, 1, 1, 1, 1, 1, 1, 1, 1, 1, 1, 1, 1, 1, 1, 1, 1, 1, 1, 1, 1, 1, 1, 1, 1, 1, 1, 1, 1, 1, 1, 1, 1, 1, 1, 1, 1, 1, 1, 1, 1, 1, 1, 1, 1, 1, 1, 1, 1, 1, 1, 1, 1, 1, 1, 1, 1, 1, 1, 1, 1, 1, 1, 1, 1, 1, 1, 1, 1, 1, 1, 1, 1, 1, 1, 1, 1, 1, 1, 1, 1, 1, 1, 1, 1, 1, 1, 1, 1, 4 ),
 ( 0.000000000000000000, 0.002600137934918278840, 0.005208846947063642402, 0.007813284371963545236, 0.01041597565644012714, 0.01302123463190214131, 0.01562472912267370319, 0.01822934229245065652, 0.02083335053635077330, 0.02343730581734793095, 0.02604195799539401474, 0.02864545692284610826, 0.03125045498156164142, 0.03385385361191795006, 0.03645873261014952182, 0.03906243010681619693, 0.04166674480109257978, 0.04427107247243720900, 0.04687475664952634596, 0.04947964045798968619, 0.05208303702386667122, 0.05468803228817373241, 0.05729153353077973132, 0.05989618223844375006, 0.06250015876865079589, 0.06510412050499821135, 0.06770877833268285073, 0.07031227041168378045, 0.07291726700687002627, 0.07552066596874357218, 0.07812554330212571896, 0.08072923942118487295, 0.08333355289058355653, 0.08593787945419822938, 0.08854156225015286097, 0.09114644488045960113, 0.09374984019314609729, 0.09635483420994474246, 0.09895833431534489799, 0.1015629817166532611, 0.1041669571688737805, 0.1067709175595765864, 0.1093755742645453749, 0.1119790650618166516, 0.1145840604711090005, 0.1171874582687142119, 0.1197923343547293018, 0.1223960294069747767, 0.1250003415701952669, 0.1276046670722256471, 0.1302083485727723866, 0.1328132300777099817, 0.1354166241949035232, 0.1380216170238739992, 0.1406251160503516617, 0.1432297622036773077, 0.1458337366370238142, 0.1484376957407889386, 0.1510423513813509144, 0.1536458409560605698, 0.1562508352375901466, 0.1588542319300798034, 0.1614591068269417562, 0.1640628008713490293, 0.1666671117869774343, 0.1692714362859856492, 0.1718751165501164191, 0.1744799969878772505, 0.1770833899687347668, 0.1796883816679979429, 0.1822918796746371972, 0.1848965246383280081, 0.1875004981115827030, 0.1901044559872153150, 0.1927091106216977379, 0.1953125990329364348, 0.1979175922448092595, 0.2005209878913200294, 0.2031258616572126918, 0.2057295547527302204, 0.2083338644793258920, 0.2109381880338489224, 0.2135418671205281671, 0.2161467465492790951, 0.2187501384529311477, 0.2213551290805818306, 0.2239586261264417955, 0.2265632699588193688, 0.2291672425307399730, 0.2317711992370185270, 0.2343758529237242316, 0.2369793402305566954, 0.2395843324308542799, 0.2421877270904984059, 0.2447925997835804779, 0.2473962919891333490, 0.2500006005852301039, 0.2526049232537817546, 0.2552086012219486610, 0.2578134796998332035, 0.2604168705853860954, 0.2630218601994954719, 0.2656253563436123954, 0.2682299991029740149, 0.2708339708322964334, 0.2734379264279751531, 0.2760425792251849364, 0.2786460654866522724, 0.2812510567334335909, 0.2838544504653006673, 0.2864593221437078951, 0.2890630135181997962, 0.2916673210423081364, 0.2942716428833813125, 0.2968753197919519748, 0.2994801973770923054, 0.3020835873036303854, 0.3046885759622478540, 0.3072920712636373342, 0.3098967130082584398, 0.3125006839536987324, 0.3151046384975096371, 0.3177092904634842285, 0.3203127757386058927, 0.3229177660899096303, 0.3255211589530693228, 0.3281260296749167193, 0.3307297202772326306, 0.3333340267878420748, 0.3359383478599109463, 0.3385420237677806976, 0.3411469005182800607, 0.3437502895448679152, 0.3463552773060237788, 0.3489587718236830116, 0.3515634126118191150, 0.3541673828320756612, 0.3567713363827305639, 0.3593759875757128741, 0.3619794719234893932, 0.3645844614373360826, 0.3671878534908398217, 0.3697927233142242476, 0.3723964132032320795, 0.3750007187588132451, 0.3776050391203355505, 0.3802087140863810166, 0.3828135900603256703, 0.3854169782460106219, 0.3880219651677176973, 0.3906254589606275029, 0.3932300988505167960, 0.3958340684042725433, 0.3984380210204655492, 0.4010426714986830565, 0.4036461549780977487, 0.4062511437124918245, 0.4088545350153757196, 0.4114594039983773821, 0.4140630932329303349, 0.4166673978919369636, 0.4192717176013560643, 0.4218753916844373286, 0.4244802669398990425, 0.4270836543437129262, 0.4296886404839689866, 0.4322921336110964741, 0.4348967726609613837, 0.4375007416068860122, 0.4401046933472957945, 0.4427093431689624881, 0.4453128258389836835, 0.4479178138519160357, 0.4505212044632024293, 0.4531260726638874359, 0.4557297613028266636, 0.4583340651236982866, 0.4609383842394453867, 0.4635420574984087105, 0.4661469320934465421, 0.4687503187744080368, 0.4713553041911981989, 0.4739587967114984313, 0.4765634349795482838, 0.4791674033763006491, 0.4817713542995921694, 0.4843760035229108252, 0.4869794854424946973, 0.4895844727919445583, 0.4921878627706443576, 0.4947927302470669919, 0.4973964183492232127, 0.5000007213903868708, 0.5026050399708832384, 0.5052087124645624483, 0.5078135864572254077, 0.5104169724743423675, 0.5130219572256408123, 0.5156254491980594157, 0.5182300867424926016, 0.5208340546487225664, 0.5234380048135498509, 0.5260426534967141965, 0.5286461347248060383, 0.5312511214687432037, 0.5338545108738584899, 0.5364593776840630435, 0.5390630653082590928, 0.5416673676281316130, 0.5442716857317909662, 0.5468753575190105076, 0.5494802309673390006, 0.5520836163796108975, 0.5546886005233833128, 0.5572920920068584749, 0.5598967288858642810, 0.5625006963602153798, 0.5651046458252231286, 0.5677092940264200083, 0.5703127746219572858, 0.5729177608183441128, 0.5755211497088699169, 0.5781260159108934094, 0.5807297031159460721, 0.5833340047729366207, 0.5859383224581667937, 0.5885419935977430628, 0.5911468665597719996, 0.5937502514261915332, 0.5963552350203973340, 0.5989587260738620245, 0.6015633623456233536, 0.6041673294467342359, 0.6067712782705607655, 0.6093759260479724160, 0.6119794060698863225, 0.6145843917766802278, 0.6171877802116071399, 0.6197926458634805957, 0.6223963327082033814, 0.6250006337607152407, 0.6276049510859208480, 0.6302086216366651339, 0.6328134941704254279, 0.6354168785499811900, 0.6380218616525755726, 0.6406253523349600965, 0.6432299880576550777, 0.6458339548441623945, 0.6484379030854412473, 0.6510425504972472410, 0.6536460300044655281, 0.6562510152796211527, 0.6588544033179367654, 0.6614592684776883225, 0.6640629550208935195, 0.6666672555273263079, 0.6692715725509107427, 0.6718752425716313370, 0.6744801147351520143, 0.6770834986868305982, 0.6796884813557668714, 0.6822919717260003125, 0.6848966069578048543, 0.6875005734883452568, 0.6901045212057073108, 0.6927091683100871089, 0.6953126473615357517, 0.6979176322630067375, 0.7005210199636988655, 0.7031258846893556624, 0.7057295709898557812, 0.7083338710086078960, 0.7109381877889758838, 0.7135418573384794128, 0.7161467291897904985, 0.7187501127725786088, 0.7213550950658099703, 0.7239585851828231888, 0.7265632199819130888, 0.7291671863151253374, 0.7317711335672014705, 0.7343757804223364216, 0.7369792590769420615, 0.7395842436626837157, 0.7421876310847422831, 0.7447924954343322357, 0.7473961815509432283, 0.7500004811404139549, 0.7526047977359727748, 0.7552084668730677519, 0.7578133384702019359, 0.7604167217430886083, 0.7630217037185706985, 0.7656251936412983294, 0.7682298280658512724, 0.7708337942603785686, 0.7734377411058018792, 0.7760423877698768846, 0.7786458660865690495, 0.7812508504145402322, 0.7838542376169586046, 0.7864591016485131814, 0.7890627876400562180, 0.7916670868586475063, 0.7942714033278103214, 0.7968750721113085911, 0.7994799435123028930, 0.8020833265342820484, 0.8046883082499752815, 0.8072917980373575109, 0.8098964321455554005, 0.8125003982600473851, 0.8151043447574546352, 0.8177089912886614798, 0.8203124693263749156, 0.8229174534545398156, 0.8255208404963184643, 0.8281257042678743518, 0.8307293901931780411, 0.8333336890992975032, 0.8359380055004849153, 0.8385416739892034288, 0.8411465452521027508, 0.8437499280821748604, 0.8463549095960458679, 0.8489583993070312085, 0.8515630331570626099, 0.8541669992501779163, 0.8567709454582125295, 0.8593755919147509914, 0.8619790697324273276, 0.8645840537187589048, 0.8671874406589066275, 0.8697923042285079509, 0.8723959901464106714, 0.8750002887984731359, 0.8776046051901155165, 0.8802082734428797739, 0.8828131446257380111, 0.8854165273229123168, 0.8880215086929368340, 0.8906249983864840125, 0.8932296320365455955, 0.8958335981669537373, 0.8984375441442679078, 0.9010421905843485346, 0.9036456682409392815, 0.9062506521434200435, 0.9088540390409564074, 0.9114589024666573946, 0.9140625884360091824, 0.9166668868924389146, 0.9192712033329777377, 0.9218748714086243412, 0.9244797425695093773, 0.9270831251927963423, 0.9296881064769593195, 0.9322915962120889022, 0.9348962297203436966, 0.9375001959466012780, 0.9401041417521586174, 0.9427087882339971747, 0.9453122657876905643, 0.9479172496658602176, 0.9505206365780075606, 0.9531254999124115779, 0.9557291860198475764, 0.9583334843266348990, 0.9609378007344983041, 0.9635414689593263526, 0.9661463405142474148, 0.9687497214891268582, 0.9713547029754164841, 0.9739581985331400293, 0.9765628250748574768, 0.9791667834374845336, 0.9817707607320566021, 0.9843753697534296521, 0.9869788348889786400, 0.9895840831931937975, 0.9921867700316038263, 0.9947911815772807476, 0.9973998924267860611, 1.000000000000000000 ),
 .UNSPECIFIED. ) ;
#166061 = CARTESIAN_POINT ( 'NONE',  ( 0.7500000000000006661, 9.197916667349467446, -1.299038105676657340 ) ) ;
#166063 = CARTESIAN_POINT ( 'NONE',  ( 5.431947826915617838, -2.167270271666811077, 0.4867340719418070671 ) ) ;
#166064 = ORIENTED_EDGE ( 'NONE', *, *, #207763, .F. ) ;
#166065 = CARTESIAN_POINT ( 'NONE',  ( -0.2108831679771167866, 1.375689764684871808, -2.152500126786048185 ) ) ;
#166066 = CARTESIAN_POINT ( 'NONE',  ( 1.499999999999987121, 2.295833333333350268, -0.8660254037844262731 ) ) ;
#166067 = CARTESIAN_POINT ( 'NONE',  ( 7.610204295972345712, 7.772993188256215547, 0.7998128361456341429 ) ) ;
#166068 = CARTESIAN_POINT ( 'NONE',  ( 4.812781342726858647, 6.637997537979888563, 1.443375672974062551 ) ) ;
#166069 = CARTESIAN_POINT ( 'NONE',  ( 3.285556943750000514, -1.013541666188710888, 1.896917185911906722 ) ) ;
#166070 = CARTESIAN_POINT ( 'NONE',  ( 10.42871741020797494, 1.405922845961228962, -5.936700867306154983 ) ) ;
#166071 = CARTESIAN_POINT ( 'NONE',  ( 7.456621297836061757, 11.64321591421002644, 0.7216878364870438212 ) ) ;
#166072 = CARTESIAN_POINT ( 'NONE',  ( 0.2923161531638042709, 3.292654673391459674, 2.051239600996176637 ) ) ;
#166073 = CARTESIAN_POINT ( 'NONE',  ( 4.878955176071345434, 6.785476686873604280, -1.599625672291269396 ) ) ;
#166074 = CARTESIAN_POINT ( 'NONE',  ( -4.095971805104331231, 5.871996087412059140, 1.443375672974065660 ) ) ;
#166075 = CARTESIAN_POINT ( 'NONE',  ( 4.879373355499653897, -0.1046096447297485965, 2.060157192773376611 ) ) ;
#166076 = CARTESIAN_POINT ( 'NONE',  ( -4.042302355168801320, 7.867769847672247074, 0.7998128361456341429 ) ) ;
#166077 = CARTESIAN_POINT ( 'NONE',  ( 1.499999999999990896, 3.306250000682818602, 1.214306433183764966E-14 ) ) ;
#166078 = CARTESIAN_POINT ( 'NONE',  ( 0.6823417656249882723, -0.07395833299191079124, -1.181850606188749264 ) ) ;
#166079 = CARTESIAN_POINT ( 'NONE',  ( 5.747288119592351308, -1.474170506619469023, -1.151262835514428540 ) ) ;
#166080 = CARTESIAN_POINT ( 'NONE',  ( 4.887242738553729815, -0.5912784195612891258, -1.630374673469140223 ) ) ;
#166081 = CARTESIAN_POINT ( 'NONE',  ( 4.405614404729386813, -0.7493292006620960732, -1.571029527175720863 ) ) ;
#166082 = CARTESIAN_POINT ( 'NONE',  ( 5.332434488876471868, 5.115595079977664383, 0.7998128361456341429 ) ) ;
#166083 = CARTESIAN_POINT ( 'NONE',  ( 1.734309787148346382, 2.268178062924830041, 0.3313793973579847729 ) ) ;
#166084 = CARTESIAN_POINT ( 'NONE',  ( -1.364683531250012516, 5.051041667008085767, -0.7879004041258300672 ) ) ;
#166085 = CARTESIAN_POINT ( 'NONE',  ( 5.179275120254928311, 1.405169897584326089, 1.548284651509527210 ) ) ;
#166086 = CARTESIAN_POINT ( 'NONE',  ( 6.298774621056003831, 1.615917059943820622, 1.076740554856120413 ) ) ;
#166087 = DIRECTION ( 'NONE',  ( -3.330669073875479482E-16, 3.330669073875479482E-16, 1.000000000000000000 ) ) ;
#166088 = CARTESIAN_POINT ( 'NONE',  ( 1.108046318188542489, -0.04667474159409169127, 2.016033875899234662 ) ) ;
#166089 = CARTESIAN_POINT ( 'NONE',  ( 0.2522424171345696298, 0.8426718423822797677, 2.023156535103701970 ) ) ;
#166090 = CARTESIAN_POINT ( 'NONE',  ( 9.167121402339585501, 14.44227982134217569, -8.755495446810726889 ) ) ;
#166091 = CARTESIAN_POINT ( 'NONE',  ( -7.874588291438845644, 8.081441182967111558, -0.7998128361456291469 ) ) ;
#166092 = CARTESIAN_POINT ( 'NONE',  ( 4.656335691289526402, 7.519809842224722374, -1.199719254218452047 ) ) ;
#166093 = CARTESIAN_POINT ( 'NONE',  ( -1.360316468750004448, 1.640625000341400241, -2.602085213965210642E-14 ) ) ;
#166094 = CARTESIAN_POINT ( 'NONE',  ( 3.615986862044855421, -0.6139777315949942471, 2.029667854546577388 ) ) ;
#166095 = CARTESIAN_POINT ( 'NONE',  ( -1.402160292154681736E-14, -0.4281249996585808071, 1.575800808251672791 ) ) ;
#166096 = CARTESIAN_POINT ( 'NONE',  ( 5.848246728868278232, 1.823843535133644389, 0.08496628090458313576 ) ) ;
#166097 = ORIENTED_EDGE ( 'NONE', *, *, #181792, .F. ) ;
#166098 = CARTESIAN_POINT ( 'NONE',  ( -6.577640801285370209, 7.702944352034914566, -1.199719254218452047 ) ) ;
#166099 = ADVANCED_FACE ( 'NONE', ( #88738 ), #21548, .T. ) ;
#166100 = DIRECTION ( 'NONE',  ( 0.000000000000000000, 0.000000000000000000, 1.000000000000000000 ) ) ;
#166101 = CARTESIAN_POINT ( 'NONE',  ( 6.278834536460164983, 9.379038488295265097, -1.082531754730548412 ) ) ;
#166102 = CARTESIAN_POINT ( 'NONE',  ( 3.475000000000000533, -2.552083332377419023, -2.006292185433951047 ) ) ;
#166103 = CARTESIAN_POINT ( 'NONE',  ( -5.208303565944065738, 9.228104593576741621, -0.7998128361456231517 ) ) ;
#166104 = CARTESIAN_POINT ( 'NONE',  ( 3.094014924146833323, 1.284692261361711774, 1.558518293110554565 ) ) ;
#166105 = CARTESIAN_POINT ( 'NONE',  ( 6.739307351729481255, -1.974284904759715298, 0.9861035376414882814 ) ) ;
#166106 = CARTESIAN_POINT ( 'NONE',  ( 8.757677159423465696, 12.30470822171437284, 1.199719254218450271 ) ) ;
#166107 = CARTESIAN_POINT ( 'NONE',  ( 3.678407310798579299, 1.183884816018574426, -1.435758196845798418 ) ) ;
#166108 = CARTESIAN_POINT ( 'NONE',  ( 7.892817981449907982, 12.36003807833360391, 0.7998128361456462443 ) ) ;
#166109 = CARTESIAN_POINT ( 'NONE',  ( -6.102578539482539810, 6.292298848917299736, 0.000000000000000000 ) ) ;
#166110 = CARTESIAN_POINT ( 'NONE',  ( -2.442440228756222353, 6.001264033524212671, -0.7998128361456281477 ) ) ;
#166111 = CIRCLE ( 'NONE', #38104, 12.00000000000000355 ) ;
#166112 = CARTESIAN_POINT ( 'NONE',  ( -8.681298431451969222, 9.022603012982438386, 1.040834085586084257E-14 ) ) ;
#166113 = CARTESIAN_POINT ( 'NONE',  ( 0.07536363704235826688, -0.001874865094115066300, -2.144269471569634877 ) ) ;
#166115 = CARTESIAN_POINT ( 'NONE',  ( -4.902910567894817717, 6.875085367926331514, 1.448488056007392721 ) ) ;
#166114 = CARTESIAN_POINT ( 'NONE',  ( -6.749980374757255319, 8.968339418673846097, 1.599625672291269396 ) ) ;
#166116 = CARTESIAN_POINT ( 'NONE',  ( -1.402160292154681736E-14, -0.4281249996585808071, 1.575800808251672791 ) ) ;
#166117 = CARTESIAN_POINT ( 'NONE',  ( 1.229404279783296694, -1.564619330878062931, -0.7474530596254543857 ) ) ;
#166118 = CARTESIAN_POINT ( 'NONE',  ( 0.8315134001313486678, 1.713846476070936653, 0.3014184826048373900 ) ) ;
#166120 = CARTESIAN_POINT ( 'NONE',  ( 6.643132081016105417, 10.69414516125339887, 0.7216878364870438212 ) ) ;
#166119 = CARTESIAN_POINT ( 'NONE',  ( 6.322925365441865786, 2.150718969097795696, 0.8370602354567517889 ) ) ;
#166121 = FACE_OUTER_BOUND ( 'NONE', #97676, .T. ) ;
#166122 = CARTESIAN_POINT ( 'NONE',  ( 1.897801681018367548, -0.6972820500400818133, 1.939346266731331259 ) ) ;
#166123 = CARTESIAN_POINT ( 'NONE',  ( 6.003563092752934871, 5.898578451166879510, 0.7998128361456341429 ) ) ;
#166124 = CARTESIAN_POINT ( 'NONE',  ( 6.380222486609858912, -0.2913964880489598452, 2.279815279960105467 ) ) ;
#166125 = CARTESIAN_POINT ( 'NONE',  ( -5.152980901645737077, 8.169505597632108262, -1.199719254218453823 ) ) ;
#166126 = CARTESIAN_POINT ( 'NONE',  ( 6.332864056472936376, 0.1854757364097951722, 1.861418627818342664 ) ) ;
#166128 = CARTESIAN_POINT ( 'NONE',  ( -6.373741612200205076, 8.529394195690610303, 1.443375672974064550 ) ) ;
#166127 = CARTESIAN_POINT ( 'NONE',  ( 5.185773951807310489, 1.841398108398510480, -0.5159224025059682139 ) ) ;
#166129 = CARTESIAN_POINT ( 'NONE',  ( 6.358075476802443227, 2.201304964888863402, -0.1578768562689457922 ) ) ;
#166130 = CARTESIAN_POINT ( 'NONE',  ( 8.025500584646550806, 8.327781868367935658, 0.000000000000000000 ) ) ;
#166131 = CARTESIAN_POINT ( 'NONE',  ( -3.757017964318317471, 6.436919154129725484, 1.082531754730549967 ) ) ;
#166132 = CARTESIAN_POINT ( 'NONE',  ( 6.633471380297788045, -0.1541069161683609745, 2.086224335282916620 ) ) ;
#166133 = EDGE_LOOP ( 'NONE', ( #160184, #140753, #58473, #181568 ) ) ;
#166134 = CARTESIAN_POINT ( 'NONE',  ( 2.960362034815271048, 2.296572897674476810, -0.2250602657276803420 ) ) ;
#166135 = CARTESIAN_POINT ( 'NONE',  ( 4.633228507203630997, 0.002057781214020309134, -1.962046631861932067 ) ) ;
#166136 = CARTESIAN_POINT ( 'NONE',  ( 2.237090426018002454, -0.09115598566783281176, -1.959741687340323946 ) ) ;
#166137 = CARTESIAN_POINT ( 'NONE',  ( 9.317477881089539338, 11.89347683273640932, 1.599625672291279388 ) ) ;
#166138 = DIRECTION ( 'NONE',  ( 0.000000000000000000, -1.000000000000000000, 0.000000000000000000 ) ) ;
#166139 = ORIENTED_EDGE ( 'NONE', *, *, #117783, .F. ) ;
#166140 = CARTESIAN_POINT ( 'NONE',  ( -0.1880716927101276914, -1.308626981353334662, -1.665352682907685233 ) ) ;
#166142 = CARTESIAN_POINT ( 'NONE',  ( -8.453672473320708036, 9.821371626084353323, -1.199719254218446718 ) ) ;
#166141 = CARTESIAN_POINT ( 'NONE',  ( -4.629219384062206011, 7.488174150459498968, -1.199719254218452047 ) ) ;
#166143 = CARTESIAN_POINT ( 'NONE',  ( 0.04061758243546764735, -1.421021341975825969, -1.170429047309962112 ) ) ;
#166144 = CARTESIAN_POINT ( 'NONE',  ( 3.995131740874768411, 0.3131294011963717816, 2.148239739743092347 ) ) ;
#166145 = CARTESIAN_POINT ( 'NONE',  ( -0.4135631787092041711, 3.000773892238208784, 2.020199156340489743 ) ) ;
#166146 = CARTESIAN_POINT ( 'NONE',  ( 2.267978396857213585, 0.5610993688725562922, -2.044979925899123252 ) ) ;
#166147 = CARTESIAN_POINT ( 'NONE',  ( -1.499999999999997780, 2.431250000682817713, 1.214306433183764966E-14 ) ) ;
#166148 = CARTESIAN_POINT ( 'NONE',  ( 8.055515824813896941, 12.54985222892493368, 0.7998128361456462443 ) ) ;
#166149 = CARTESIAN_POINT ( 'NONE',  ( 11.94980361058168938, 13.40000000000000036, -1.100000000000000311 ) ) ;
#166150 = CARTESIAN_POINT ( 'NONE',  ( 6.505076094845553492, 6.832456077006010098, -0.5564590407885674495 ) ) ;
#166151 = CARTESIAN_POINT ( 'NONE',  ( 2.038423305949757847, 2.037923218716758633, 0.3053300769366319445 ) ) ;
#166153 = CARTESIAN_POINT ( 'NONE',  ( 6.142902043169038429, 7.013529245237516641, 0.9864344219776898237 ) ) ;
#166152 = CARTESIAN_POINT ( 'NONE',  ( -8.317037166979361018, 11.79062823052953668, 1.199719254218453823 ) ) ;
#166154 = CARTESIAN_POINT ( 'NONE',  ( -1.364683531250012516, 2.488541667008088876, -0.7879004041258289570 ) ) ;
#166155 = CARTESIAN_POINT ( 'NONE',  ( 0.07775346131141079586, 1.298946786380944074, -2.537735853881052162 ) ) ;
#166156 = CARTESIAN_POINT ( 'NONE',  ( -3.707465945607718805, 7.355851012256872323, 0.5743249234583160945 ) ) ;
#166157 = ORIENTED_EDGE ( 'NONE', *, *, #172733, .F. ) ;
#166158 = CARTESIAN_POINT ( 'NONE',  ( 4.899028947338643469, -0.2378672112019978024, -1.897373119303269018 ) ) ;
#166159 = CARTESIAN_POINT ( 'NONE',  ( -1.115562610750309283E-14, 9.343750000682801371, 1.500000000000001554 ) ) ;
#166160 = CARTESIAN_POINT ( 'NONE',  ( 1.159873712335700802, 0.4409813497070895760, -2.218855480106549649 ) ) ;
#166161 = CARTESIAN_POINT ( 'NONE',  ( -8.500599126088349777, 12.86119004717103209, 1.040834085586084257E-14 ) ) ;
#166162 = CARTESIAN_POINT ( 'NONE',  ( 0.8085208021518180965, -0.4412475195509023562, -1.756857618417038358 ) ) ;
#166163 = CARTESIAN_POINT ( 'NONE',  ( 1.833070758936614864, -1.541008679516321589, -1.137915016233618015 ) ) ;
#166164 = CARTESIAN_POINT ( 'NONE',  ( 2.822784111170244525, -1.429543836668966561, 1.497820115680066344 ) ) ;
#166165 = CARTESIAN_POINT ( 'NONE',  ( -1.201851678989727383E-14, 1.384375000341419693, 1.575800808251672791 ) ) ;
#166166 = CARTESIAN_POINT ( 'NONE',  ( 0.5671783758751040017, 0.1957704533250003986, -1.961731083161978306 ) ) ;
#166167 = CARTESIAN_POINT ( 'NONE',  ( 5.004483369110711344, -0.6506757832731756563, -1.813419023564779353 ) ) ;
#166168 = ADVANCED_FACE ( 'NONE', ( #22628 ), #24731, .T. ) ;
#166170 = CARTESIAN_POINT ( 'NONE',  ( 5.788239156490550208, 7.236076679697275083, -1.185412701995581797 ) ) ;
#166169 = CARTESIAN_POINT ( 'NONE',  ( 6.516270054225981490, -1.036149114087565382, -1.948532232987249424 ) ) ;
#166171 = CARTESIAN_POINT ( 'NONE',  ( 1.364683531249988757, 1.384375000341421469, 0.000000000000000000 ) ) ;
#166172 = CARTESIAN_POINT ( 'NONE',  ( 5.160619382589332282, -0.6916465251813638249, -1.943403241031741002 ) ) ;
#166173 = CARTESIAN_POINT ( 'NONE',  ( -7.400052914960538963, 7.527816577075747695, 1.040834085586084257E-14 ) ) ;
#166174 = CARTESIAN_POINT ( 'NONE',  ( 8.535021395002688749, 9.916278701380017324, 1.199719254218462483 ) ) ;
#166175 = CARTESIAN_POINT ( 'NONE',  ( 4.650610384687404952, 5.384465856012134566, 1.199719254218462483 ) ) ;
#166176 =( BOUNDED_SURFACE ( )  B_SPLINE_SURFACE ( 3, 3, ( 
 ( #62607, #127718, #129840, #96212, #162263, #29060, #112501, #163328, #63684, #95143 ),
 ( #11723, #47461, #146033, #81002, #44256, #93015, #147090, #110377, #60479, #64745 ),
 ( #192603, #191537, #194745, #79926, #12781, #178511, #94084, #159058, #10654, #78854 ),
 ( #27988, #143918, #144975, #134849, #5854, #104467, #103390, #187826, #22096, #169451 ),
 ( #71926, #86070, #39452, #151090, #204049, #89291, #105547, #2654, #180632, #38385 ),
 ( #152146, #88209, #171582, #53570, #32254, #170514, #154280, #3713, #69790, #68728 ),
 ( #138036, #6924, #52502, #55699, #121855, #135898, #185686, #36237, #201916, #37315 ) ),
 .UNSPECIFIED., .T., .F., .T. ) 
 B_SPLINE_SURFACE_WITH_KNOTS ( ( 4, 3, 4 ),
 ( 4, 1, 1, 1, 1, 1, 1, 4 ),
 ( 0.000000000000000000, 0.5000000000000000000, 1.000000000000000000 ),
 ( 0.000000000000000000, 0.09884949474608377418, 0.1930937302289311708, 0.2616037862002966730, 0.3630310524065313849, 0.5216543902990324888, 0.7338513509102306820, 0.9999999999999998890 ),
 .UNSPECIFIED. ) 
 GEOMETRIC_REPRESENTATION_ITEM ( )  RATIONAL_B_SPLINE_SURFACE ( (
 ( 1.000000000000000222, 1.000000000000000222, 1.000000000000000000, 1.000000000000000222, 1.000000000000000444, 1.000000000000000222, 1.000000000000000222, 1.000000000000000222, 1.000000000000000222, 1.000000000000000222),
 ( 0.3333333333333334259, 0.3333333333333334259, 0.3333333333333334814, 0.3333333333333333703, 0.3333333333333334814, 0.3333333333333333703, 0.3333333333333334814, 0.3333333333333333703, 0.3333333333333334259, 0.3333333333333334259),
 ( 0.3333333333333334259, 0.3333333333333334259, 0.3333333333333334814, 0.3333333333333333703, 0.3333333333333334814, 0.3333333333333333703, 0.3333333333333334814, 0.3333333333333333703, 0.3333333333333334259, 0.3333333333333334259),
 ( 1.000000000000000222, 1.000000000000000222, 1.000000000000000000, 1.000000000000000222, 1.000000000000000444, 1.000000000000000222, 1.000000000000000222, 1.000000000000000222, 1.000000000000000222, 1.000000000000000222),
 ( 0.3333333333333334259, 0.3333333333333334259, 0.3333333333333334814, 0.3333333333333333703, 0.3333333333333334814, 0.3333333333333333703, 0.3333333333333334814, 0.3333333333333333703, 0.3333333333333334259, 0.3333333333333334259),
 ( 0.3333333333333334259, 0.3333333333333334259, 0.3333333333333334814, 0.3333333333333333703, 0.3333333333333334814, 0.3333333333333333703, 0.3333333333333334814, 0.3333333333333333703, 0.3333333333333334259, 0.3333333333333334259),
 ( 1.000000000000000222, 1.000000000000000222, 1.000000000000000000, 1.000000000000000222, 1.000000000000000444, 1.000000000000000222, 1.000000000000000222, 1.000000000000000222, 1.000000000000000222, 1.000000000000000222) ) ) 
 REPRESENTATION_ITEM ( '' )  SURFACE ( )  );
#166178 = CARTESIAN_POINT ( 'NONE',  ( -1.201851678989727383E-14, 3.462500000000019895, 1.732050807568877637 ) ) ;
#166177 = CARTESIAN_POINT ( 'NONE',  ( 4.823321527849568469, -0.1059641466341002675, 2.103426968240690087 ) ) ;
#166179 = CARTESIAN_POINT ( 'NONE',  ( 1.328853926488116510, -1.377647258212051362, 1.678094904287985800 ) ) ;
#166180 = CARTESIAN_POINT ( 'NONE',  ( -1.364683531249997417, 2.571875000341422357, 1.214306433183764966E-14 ) ) ;
#166181 = CARTESIAN_POINT ( 'NONE',  ( 5.184929619776310616, -0.2588774643964043554, -2.145956309214678726 ) ) ;
#166182 = CARTESIAN_POINT ( 'NONE',  ( 5.338538087541965460, 1.201400599988803108, -1.623342581396812090 ) ) ;
#166183 = CARTESIAN_POINT ( 'NONE',  ( -0.1399997263889820043, 5.722209607272843002, -2.594334538518060729 ) ) ;
#166186 = CARTESIAN_POINT ( 'NONE',  ( 4.365362273920230685, 8.036747052974847705, 0.7216878364870298324 ) ) ;
#166185 = CARTESIAN_POINT ( 'NONE',  ( -1.642778471875000035, -2.617708332855375186, -2.845375778867859751 ) ) ;
#166184 = CARTESIAN_POINT ( 'NONE',  ( 8.011942431032855083, 8.311964022485323511, 0.7998128361456291469 ) ) ;
#166187 = CARTESIAN_POINT ( 'NONE',  ( -7.130662446144611977, 7.283804040115648526, 0.000000000000000000 ) ) ;
#166188 = CARTESIAN_POINT ( 'NONE',  ( 3.678922940808615483, 1.700962499606586853, -1.082838980105811366 ) ) ;
#166189 = CARTESIAN_POINT ( 'NONE',  ( -9.189729191964438826, 9.615772233580322848, 1.040834085586084257E-14 ) ) ;
#166190 = CARTESIAN_POINT ( 'NONE',  ( -4.600294193738529103, 4.261431402316699035, -0.7998128361456221525 ) ) ;
#166191 = CARTESIAN_POINT ( 'NONE',  ( 0.6823417656249899377, 4.176041667008085767, -1.181850606188754593 ) ) ;
#166193 = CARTESIAN_POINT ( 'NONE',  ( 0.4019237886466816012, 12.67633545031536713, -1.499999999999998668 ) ) ;
#166192 = CARTESIAN_POINT ( 'NONE',  ( 4.803692121107413726, -0.5798474923815257753, 2.082409481564663434 ) ) ;
#166194 = CARTESIAN_POINT ( 'NONE',  ( -10.91033749632886973, 4.885617943545218722, -4.996452313011734425 ) ) ;
#166196 = CARTESIAN_POINT ( 'NONE',  ( 5.905875104417894761, -1.122515283938491537, -1.674877678029200068 ) ) ;
#166195 = CARTESIAN_POINT ( 'NONE',  ( -7.822691444960713447, 9.189190109618056823, -1.082531754730543083 ) ) ;
#166197 = CARTESIAN_POINT ( 'NONE',  ( -1.001543065824772872E-14, 5.462500000000020783, 1.732050807568877637 ) ) ;
#166198 = ADVANCED_FACE ( 'NONE', ( #154795 ), #97511, .T. ) ;
#166199 = CARTESIAN_POINT ( 'NONE',  ( 0.8028309281867166414, 1.407482529003287075, 0.9968052580264019635 ) ) ;
#166200 = CARTESIAN_POINT ( 'NONE',  ( 5.585032934186686226, 5.480569609498057382, 0.000000000000000000 ) ) ;
#166202 = CARTESIAN_POINT ( 'NONE',  ( 5.671053392266061977, 9.838255734277600695, 0.7998128361456331437 ) ) ;
#166201 = CARTESIAN_POINT ( 'NONE',  ( 8.920901888112002354, 9.510066412326583674, 0.7216878364870438212 ) ) ;
#166203 = CIRCLE ( 'NONE', #72805, 10.99999999999999112 ) ;
#166204 = DIRECTION ( 'NONE',  ( 0.000000000000000000, -1.000000000000000000, 0.000000000000000000 ) ) ;
#166205 = CARTESIAN_POINT ( 'NONE',  ( 6.151601556293980977, 0.5431611868166182910, -1.789914130245950696 ) ) ;
#166206 = CARTESIAN_POINT ( 'NONE',  ( 5.888937080504050847, -1.913070152547487579, -0.6273127349021755395 ) ) ;
#166207 = DIRECTION ( 'NONE',  ( 0.000000000000000000, 0.000000000000000000, 1.000000000000000000 ) ) ;
#166208 = CARTESIAN_POINT ( 'NONE',  ( 3.836594282542920009, 4.538743420130594508, 1.082531754730560403 ) ) ;
#166209 = CARTESIAN_POINT ( 'NONE',  ( -6.468648687051513413, 7.679749902049126220, 1.082531754730549078 ) ) ;
#166210 = ORIENTED_EDGE ( 'NONE', *, *, #186483, .T. ) ;
#166212 = CARTESIAN_POINT ( 'NONE',  ( 1.669546221992053603, 1.392560760841387246, 1.458543886677300394 ) ) ;
#166211 = CARTESIAN_POINT ( 'NONE',  ( 1.893382502257603850, -0.1070854039621378373, -2.117916637519041689 ) ) ;
#166213 = CARTESIAN_POINT ( 'NONE',  ( 2.619172825086816037, 1.532478635541080214, 0.9657477217557136617 ) ) ;
#166214 = EDGE_CURVE ( 'NONE', #74967, #71109, #8720, .T. ) ;
#166215 = CARTESIAN_POINT ( 'NONE',  ( 5.826972158823246595, 10.02016096192762085, -0.7998128361456481317 ) ) ;
#166216 = CARTESIAN_POINT ( 'NONE',  ( 6.069229152942409833, 0.1638285306290177823, -2.155560115052157055 ) ) ;
#166217 = ORIENTED_EDGE ( 'NONE', *, *, #213665, .F. ) ;
#166218 = AXIS2_PLACEMENT_3D ( 'NONE', #167633, #22424, #138350 ) ;
#166219 = CARTESIAN_POINT ( 'NONE',  ( 6.531277313481192337, 8.642909503859968368, 1.599625672291281386 ) ) ;
#166221 = CARTESIAN_POINT ( 'NONE',  ( 0.1103573706816539240, 1.834011727325855379, 0.5536052920952787559 ) ) ;
#166220 = CARTESIAN_POINT ( 'NONE',  ( -4.055860508782465068, 7.883587693554856557, 1.040834085586084257E-14 ) ) ;
#166222 = PRESENTATION_STYLE_ASSIGNMENT (( #202967 ) ) ;
#166223 = SURFACE_SIDE_STYLE ('',( #149987 ) ) ;
#166224 = B_SPLINE_CURVE_WITH_KNOTS ( 'NONE', 3,
 ( #110815, #46843, #144369, #178968, #96665, #160566, #164832, #176820 ),
 .UNSPECIFIED., .F., .F.,
 ( 4, 2, 2, 4 ),
 ( 0.000000000000000000, 0.0001985720215089308081, 0.0003971440430178616162, 0.0007942880860357254009 ),
 .UNSPECIFIED. ) ;
#166225 = CARTESIAN_POINT ( 'NONE',  ( 4.921246571636183731, 7.724909519342112674, -1.082531754730549078 ) ) ;
#166226 = CARTESIAN_POINT ( 'NONE',  ( -1.364683531250000748, 0.8218750003414210248, 0.000000000000000000 ) ) ;
#166227 = CARTESIAN_POINT ( 'NONE',  ( 3.145128448690309053, 4.692402494937224056, -1.443375672974057666 ) ) ;
#166228 = CARTESIAN_POINT ( 'NONE',  ( -8.448702279610222021, 13.00856975952063088, 1.040834085586084257E-14 ) ) ;
#166229 = CARTESIAN_POINT ( 'NONE',  ( 4.170900312159072421, -2.016029151617684256, -0.7805680927704603533 ) ) ;
#166230 = CARTESIAN_POINT ( 'NONE',  ( -6.183927461608886844, 7.347575139032721303, 1.082531754730548412 ) ) ;
#166231 = ADVANCED_FACE ( 'NONE', ( #102844 ), #168901, .F. ) ;
#166232 = CARTESIAN_POINT ( 'NONE',  ( 4.421367491832258523, 8.172362817197399210, 0.7216878364870257245 ) ) ;
#166233 = CARTESIAN_POINT ( 'NONE',  ( 1.969135536805465492, -1.636093909763213228, 1.349083368969570262 ) ) ;
#166234 = DIRECTION ( 'NONE',  ( 2.168404344971003188E-14, 0.000000000000000000, -1.000000000000000000 ) ) ;
#166235 = CARTESIAN_POINT ( 'NONE',  ( 3.708241208800214572, -0.7959428688352770953, -1.803694655455597262 ) ) ;
#166236 = CARTESIAN_POINT ( 'NONE',  ( 5.449440537890920311, -1.726199344983204265, 0.8234401749890255529 ) ) ;
#166237 = VERTEX_POINT ( 'NONE', #23708 ) ;
#166238 = CARTESIAN_POINT ( 'NONE',  ( 9.488025208946959665, -6.683951901172175525, -0.1062647697984070022 ) ) ;
#166239 = CARTESIAN_POINT ( 'NONE',  ( 6.004353349036935406, 1.967244357045078607, 0.09818725807526038074 ) ) ;
#166240 = CARTESIAN_POINT ( 'NONE',  ( 1.042798325077255450, -1.530655164913260702, -1.195007349728629764 ) ) ;
#166241 = EDGE_LOOP ( 'NONE', ( #65134, #9300, #92116 ) ) ;
#166242 = CARTESIAN_POINT ( 'NONE',  ( -3.311934663488232733, 7.085950550703385531, -0.7998128361456481317 ) ) ;
#166244 = CARTESIAN_POINT ( 'NONE',  ( 7.862802741282558294, 8.137967717776607657, 0.000000000000000000 ) ) ;
#166243 = CARTESIAN_POINT ( 'NONE',  ( -5.153507786970262572, 9.026526494858359229, -0.7216878364870338292 ) ) ;
#166245 = CARTESIAN_POINT ( 'NONE',  ( 7.657657833620182153, 7.828355648845348291, -0.7998128361456281477 ) ) ;
#166247 = CARTESIAN_POINT ( 'NONE',  ( 4.950135482320912494, 6.868520377498098739, -1.443375672974068769 ) ) ;
#166246 = CARTESIAN_POINT ( 'NONE',  ( 7.806797523370503811, 8.002351953554066810, 1.040834085586084257E-14 ) ) ;
#166249 = VERTEX_POINT ( 'NONE', #121305 ) ;
#166248 = CARTESIAN_POINT ( 'NONE',  ( 5.971340724440283410, -1.642497693792897451, -0.9790476769208908969 ) ) ;
#166250 = CARTESIAN_POINT ( 'NONE',  ( 2.772332522587173997, 1.181257105606844160, 1.863944272329665086 ) ) ;
#166251 = CARTESIAN_POINT ( 'NONE',  ( 2.169229845753062325, -2.017539712319418310, -0.8944986170207609444 ) ) ;
#166252 = CARTESIAN_POINT ( 'NONE',  ( -5.658207315435856088, 5.763393968100056775, -0.1070472433331712409 ) ) ;
#166253 = CARTESIAN_POINT ( 'NONE',  ( 0.6625817696367036769, 0.5554855734208345996, 1.829800363923417716 ) ) ;
#166254 =( BOUNDED_SURFACE ( )  B_SPLINE_SURFACE ( 3, 2, ( 
 ( #103303, #19899, #85983 ),
 ( #172581, #7918, #72918 ),
 ( #169365, #104378, #87047 ),
 ( #55616, #139023, #24162 ) ),
 .UNSPECIFIED., .F., .F., .T. ) 
 B_SPLINE_SURFACE_WITH_KNOTS ( ( 4, 4 ),
 ( 3, 3 ),
 ( 0.000000000000000000, 0.002003486994853853880 ),
 ( 0.000000000000000000, 1.000000000000000000 ),
 .UNSPECIFIED. ) 
 GEOMETRIC_REPRESENTATION_ITEM ( )  RATIONAL_B_SPLINE_SURFACE ( (
 ( 1.000000000000000000, 0.7779734834199515392, 1.000000000000000000),
 ( 1.000000000000000000, 0.7856061901475724918, 1.000000000000000000),
 ( 1.000000000000000000, 0.7951961705782247813, 1.000000000000000000),
 ( 1.000000000000000000, 0.8104931255419010050, 1.000000000000000000) ) ) 
 REPRESENTATION_ITEM ( '' )  SURFACE ( )  );
#166255 = CARTESIAN_POINT ( 'NONE',  ( -0.08053691275167716712, 15.51846456562902965, 11.99972973886013961 ) ) ;
#166256 = CARTESIAN_POINT ( 'NONE',  ( 11.48243876534946217, 13.88000000000000078, -3.200000000000001510 ) ) ;
#166257 = CARTESIAN_POINT ( 'NONE',  ( 2.787621587699981696, -1.932700977737045633, 0.7428295258242523236 ) ) ;
#166258 = CARTESIAN_POINT ( 'NONE',  ( -6.274726165026268454, 6.214935368819085149, 0.7998128361456341429 ) ) ;
#166260 = CARTESIAN_POINT ( 'NONE',  ( 2.184651956524386041, -2.119909832212972578, -0.4221607449544013679 ) ) ;
#166259 = CARTESIAN_POINT ( 'NONE',  ( -3.684065054611367351, 5.321161868511784299, -1.599625672291256295 ) ) ;
#166261 = CARTESIAN_POINT ( 'NONE',  ( 3.667680160636753506, 1.218766932906123479, 1.821211977396507198 ) ) ;
#166262 = CARTESIAN_POINT ( 'NONE',  ( -3.719872605471121751, 6.605953636083950364, 2.420000000000000373 ) ) ;
#166263 = CARTESIAN_POINT ( 'NONE',  ( 4.909461021924256485, 4.900328411765999981, 0.7216878364870338292 ) ) ;
#166264 = FACE_OUTER_BOUND ( 'NONE', #52314, .T. ) ;
#166265 = CARTESIAN_POINT ( 'NONE',  ( -1.364683531250014514, 13.90104166700806765, -0.7879004041258335089 ) ) ;
#166266 = CARTESIAN_POINT ( 'NONE',  ( -3.955946960137363799, 7.837298230127379917, 0.7998128361456352531 ) ) ;
#166267 = CARTESIAN_POINT ( 'NONE',  ( 6.170542255345159433, 1.203217383492904746, 1.249094692781686611 ) ) ;
#166268 = CARTESIAN_POINT ( 'NONE',  ( -10.00555417720528872, 10.77549408293541866, 0.7216878364870438212 ) ) ;
#166269 = CARTESIAN_POINT ( 'NONE',  ( 3.010663864534826928, 0.6931938328994196041, 1.950912564768356727 ) ) ;
#166270 = CARTESIAN_POINT ( 'NONE',  ( 5.150072296613558365, 1.044590698784592542, 1.841551053096659230 ) ) ;
#166271 = CARTESIAN_POINT ( 'NONE',  ( 7.298366762858032430, 7.409182732956175244, 1.040834085586084257E-14 ) ) ;
#166273 = EDGE_CURVE ( 'NONE', #186548, #73830, #142450, .T. ) ;
#166272 = CARTESIAN_POINT ( 'NONE',  ( 1.364683531249988535, 5.155208333674750953, -0.7879004041258300672 ) ) ;
#166274 = CARTESIAN_POINT ( 'NONE',  ( 2.905082208348725548, -1.640047651136176565, 1.090064613274278837 ) ) ;
#166275 = CARTESIAN_POINT ( 'NONE',  ( 1.388764059443419407, -1.816923020173771830, -0.5969786173363604842 ) ) ;
#166276 = CARTESIAN_POINT ( 'NONE',  ( 5.402359069383361856, 1.738778441700383315, -1.493778605308769603 ) ) ;
#166277 = CARTESIAN_POINT ( 'NONE',  ( 2.877373901574116211, 1.733520850877915187, -0.5729475677913041798 ) ) ;
#166278 = B_SPLINE_CURVE_WITH_KNOTS ( 'NONE', 3,
 ( #195457, #96910, #61180, #65415, #211678, #164030, #30834, #63314 ),
 .UNSPECIFIED., .F., .F.,
 ( 4, 2, 2, 4 ),
 ( 0.000000000000000000, 0.0001671579969091590092, 0.0003343159938183180185, 0.0006686319876366360370 ),
 .UNSPECIFIED. ) ;
#166279 = EDGE_CURVE ( 'NONE', #128654, #130349, #39400, .T. ) ;
#166280 = CARTESIAN_POINT ( 'NONE',  ( 3.390420931869152721, 6.113185632892752075, -1.199719254218452047 ) ) ;
#166281 = CARTESIAN_POINT ( 'NONE',  ( 4.894130264408854458, 6.732904613275549899, -1.443375672974051449 ) ) ;
#166282 = CARTESIAN_POINT ( 'NONE',  ( -8.030507057996002729, 8.263346410617135263, 1.040834085586084257E-14 ) ) ;
#166283 = VERTEX_POINT ( 'NONE', #191531 ) ;
#166284 = ORIENTED_EDGE ( 'NONE', *, *, #49580, .T. ) ;
#166285 = CARTESIAN_POINT ( 'NONE',  ( 3.586193004068451540, 1.121915001286919233, 1.671427700405977212 ) ) ;
#166286 = CARTESIAN_POINT ( 'NONE',  ( 3.854310441289869882, -1.959320932037407426, -0.1006921081871253454 ) ) ;
#166287 = CARTESIAN_POINT ( 'NONE',  ( -6.561256274009600986, 9.742217188731485678, -1.199719254218440723 ) ) ;
#166288 = CARTESIAN_POINT ( 'NONE',  ( -3.978428010606240850, 6.728917548094202949, -1.199719254218452047 ) ) ;
#166289 = CARTESIAN_POINT ( 'NONE',  ( 0.1755611466353291517, 7.629137130509040077, -2.844001552353003781 ) ) ;
#166291 = CARTESIAN_POINT ( 'NONE',  ( 5.278098682986631651, -0.9809853834585824384, 1.472868624863521880 ) ) ;
#166290 = CARTESIAN_POINT ( 'NONE',  ( -0.09403702165171158589, -0.8981432076055823055, -1.886421477387869361 ) ) ;
#166292 = CARTESIAN_POINT ( 'NONE',  ( 11.00038526257060667, -5.601932402265105360, -0.008494835128417067838 ) ) ;
#166293 = CARTESIAN_POINT ( 'NONE',  ( 1.728746526384251858, 0.2170652002222578369, 2.180672313318913869 ) ) ;
#166294 = CARTESIAN_POINT ( 'NONE',  ( 6.667905886031927132, -1.063982290101581185, 1.377602455597818132 ) ) ;
#166295 = CARTESIAN_POINT ( 'NONE',  ( 6.103141704446003679, 10.27208242182903142, 0.7998128361456462443 ) ) ;
#166296 = CARTESIAN_POINT ( 'NONE',  ( 0.6270765232691848379, -1.639361371195736439, 0.5365680580288884061 ) ) ;
#166297 = CARTESIAN_POINT ( 'NONE',  ( 1.036931080102401426, 2.214701571188535834, -0.6144361423649072895 ) ) ;
#166298 = CARTESIAN_POINT ( 'NONE',  ( 1.048660896456204528, -1.724490848714568259, 1.352309724062021878 ) ) ;
#166299 = CARTESIAN_POINT ( 'NONE',  ( 6.643864291637132879, -0.08952462543848457854, -1.731637005886511593 ) ) ;
#166300 = CARTESIAN_POINT ( 'NONE',  ( 3.088704478669739295, -2.174299887604825177, -0.3769171259565203269 ) ) ;
#166301 = ADVANCED_FACE ( 'NONE', ( #9595 ), #138870, .T. ) ;
#166302 = CARTESIAN_POINT ( 'NONE',  ( 6.830535128024421532, -1.341686296255087063, 1.707861204732928018 ) ) ;
#166303 = DIRECTION ( 'NONE',  ( 0.6691306063588511321, 0.000000000000000000, -0.7431448254774005724 ) ) ;
#166304 = CARTESIAN_POINT ( 'NONE',  ( 1.763061546204633290, -0.1096309319212440264, -2.114649557665876145 ) ) ;
#166305 = CARTESIAN_POINT ( 'NONE',  ( 6.725445687907758874, -7.162053774861991684, -6.710127771514625472 ) ) ;
#166306 = CARTESIAN_POINT ( 'NONE',  ( 5.456054696845579421, 1.924170334762603574, -0.09472988109167354565 ) ) ;
#166307 = EDGE_LOOP ( 'NONE', ( #212350, #163587, #184065, #6073, #76864, #169847, #2218, #103636 ) ) ;
#166309 = CARTESIAN_POINT ( 'NONE',  ( -1.500000000000011324, 5.170833333333356485, 0.8660254037844403729 ) ) ;
#166308 = CARTESIAN_POINT ( 'NONE',  ( 2.525266882823226311, -2.137704731703232053, 0.8281840208047249741 ) ) ;
#166310 = CARTESIAN_POINT ( 'NONE',  ( 4.695201269034174452, 4.372156323494968966, 1.214306433183764966E-14 ) ) ;
#166311 = CARTESIAN_POINT ( 'NONE',  ( 3.669453130792974971, 7.432779085900453886, 1.040834085586084257E-14 ) ) ;
#166312 = CARTESIAN_POINT ( 'NONE',  ( 4.899211331842913353, -0.2710981195956448375, -2.204650271698949116 ) ) ;
#166313 = CARTESIAN_POINT ( 'NONE',  ( -6.209271165378811297, 10.18797409300986878, 0.7216878364870458196 ) ) ;
#166314 = CARTESIAN_POINT ( 'NONE',  ( -0.3000000000000103140, 3.322650755865456773, 0.5865692111442551981 ) ) ;
#166315 = CARTESIAN_POINT ( 'NONE',  ( 6.480434237652132445, 7.623223367758051872, 1.082531754730558626 ) ) ;
#166316 = CARTESIAN_POINT ( 'NONE',  ( -9.124274191872645545, 9.747334100047323702, -0.7216878364870267237 ) ) ;
#166317 = AXIS2_PLACEMENT_3D ( 'NONE', #113927, #179923, #60834 ) ;
#166318 = CARTESIAN_POINT ( 'NONE',  ( 4.909461021924231616, 8.741805268971372556, 0.7216878364870317197 ) ) ;
#166319 = VERTEX_POINT ( 'NONE', #7451 ) ;
#166320 = CARTESIAN_POINT ( 'NONE',  ( 2.531875153343257523, -1.674887184936912909, 1.122499117612890673 ) ) ;
#166322 = CARTESIAN_POINT ( 'NONE',  ( 1.305618366820593179, -1.623578218988607658, -1.271935013979957452 ) ) ;
#166321 = CARTESIAN_POINT ( 'NONE',  ( 7.949158136313996259, 8.168439335321471262, 1.040834085586084257E-14 ) ) ;
#166323 = CARTESIAN_POINT ( 'NONE',  ( 4.516274566683592617, 8.283087737857252719, -0.7216878364870357165 ) ) ;
#166324 = SURFACE_STYLE_USAGE ( .BOTH. , #36309 ) ;
#166325 = CARTESIAN_POINT ( 'NONE',  ( -1.201851678989727383E-14, 3.196875000341420137, -1.575800808251660134 ) ) ;
#166326 = CARTESIAN_POINT ( 'NONE',  ( 3.609492757825348175, -2.159078094573213757, 0.3743817768235499499 ) ) ;
#166327 = CARTESIAN_POINT ( 'NONE',  ( 1.529922885524274134, -1.701946718671920600, 1.081067414773040802 ) ) ;
#166328 = CARTESIAN_POINT ( 'NONE',  ( 0.9602180038516641147, -1.664555262390180257, -0.7873027242753791732 ) ) ;
#166329 = CARTESIAN_POINT ( 'NONE',  ( 5.073898020828643496, -1.275178753180395530, 1.904781575909524349 ) ) ;
#166330 = CARTESIAN_POINT ( 'NONE',  ( 4.558453444723221892, -1.645810703501834560, -0.8254300276653583346 ) ) ;
#166331 = CARTESIAN_POINT ( 'NONE',  ( 6.934105498385400246, 10.17720795050327354, -1.199719254218441611 ) ) ;
#166332 = CARTESIAN_POINT ( 'NONE',  ( 4.119992258926360229, -0.9384382104282267267, -1.565754920925747973 ) ) ;
#166333 = CARTESIAN_POINT ( 'NONE',  ( 4.430314669760617718, -1.560499787156752971, -1.277043788614096176 ) ) ;
#166334 = CARTESIAN_POINT ( 'NONE',  ( -7.934546212495630968, 10.28005655271014795, -1.599625672291263179 ) ) ;
#166336 = CARTESIAN_POINT ( 'NONE',  ( -6.583366107887490770, 9.838288338247510367, 1.199719254218452935 ) ) ;
#166335 = CARTESIAN_POINT ( 'NONE',  ( 4.575235619729528302, 0.004297453766812646056, -2.262689076577176106 ) ) ;
#166337 = CARTESIAN_POINT ( 'NONE',  ( 6.545935606868724221, 0.8096169477174266493, -1.944322875993751421 ) ) ;
#166338 = CARTESIAN_POINT ( 'NONE',  ( -6.064239847062411926, 10.29697326487330500, 0.000000000000000000 ) ) ;
#166339 = CARTESIAN_POINT ( 'NONE',  ( 4.756339170418532269, -2.069830778647030023, -0.05414847147890837487 ) ) ;
#166340 = CARTESIAN_POINT ( 'NONE',  ( 8.809047120577066181, 11.30030761213851953, 1.599625672291281386 ) ) ;
#166341 = CARTESIAN_POINT ( 'NONE',  ( 4.666094584615946061, 4.902326079784082857, -0.7990728202500730903 ) ) ;
#166342 = PRODUCT_CONTEXT ( 'NONE', #130779, 'mechanical' ) ;
#166344 = CARTESIAN_POINT ( 'NONE',  ( 2.350114058346234547, 1.926077408352431464, 0.04734757869597795016 ) ) ;
#166343 = CARTESIAN_POINT ( 'NONE',  ( -8.422639742587602285, 10.84949900448412841, -1.599625672291263179 ) ) ;
#166345 = UNCERTAINTY_MEASURE_WITH_UNIT (LENGTH_MEASURE( 1.000000000000000082E-05 ), #173248, 'distance_accuracy_value', 'NONE');
#166346 = CARTESIAN_POINT ( 'NONE',  ( 0.2034765232073352526, -1.520001300341488948, -1.252246736068510335 ) ) ;
#166347 = CARTESIAN_POINT ( 'NONE',  ( 5.691390622686558487, 9.861982503101517139, 0.7998128361456341429 ) ) ;
#166348 = CARTESIAN_POINT ( 'NONE',  ( 5.575284262857175044, 6.175169341367511500, -0.8878447928483481633 ) ) ;
#166349 = CARTESIAN_POINT ( 'NONE',  ( -9.490344339885973923, 12.09515436799890331, -1.443375672974059665 ) ) ;
#166351 = CARTESIAN_POINT ( 'NONE',  ( 1.160717840558170622, 2.219164385786871030, 0.1022553982447590853 ) ) ;
#166350 = CARTESIAN_POINT ( 'NONE',  ( 1.178162429063234207, 2.088287186665960693, -0.3679680078583212333 ) ) ;
#166352 = CARTESIAN_POINT ( 'NONE',  ( 3.417109911095609132, 1.903178947333901583, 0.9019662245143298396 ) ) ;
#166354 = CARTESIAN_POINT ( 'NONE',  ( -5.725286006720766707, 9.901527117808042178, 0.7998128361456291469 ) ) ;
#166353 = CIRCLE ( 'NONE', #194023, 2.000000000000006661 ) ;
#166355 = CARTESIAN_POINT ( 'NONE',  ( 7.124973419181436007, 8.271222729588529887, -1.199719254218446718 ) ) ;
#166356 = CARTESIAN_POINT ( 'NONE',  ( 3.437899435096212208, 1.242623406730450908, 1.518177208742684803 ) ) ;
#166357 = CARTESIAN_POINT ( 'NONE',  ( 5.937581207780954884, 9.014596278131406848, -1.199719254218440723 ) ) ;
#166358 = CARTESIAN_POINT ( 'NONE',  ( -4.159863475130535448, 7.428450666093093346, 0.7365534166655554049 ) ) ;
#166359 = CARTESIAN_POINT ( 'NONE',  ( 3.876741858503734761, 6.610283703974623393, 1.199719254218462483 ) ) ;
#166360 = CARTESIAN_POINT ( 'NONE',  ( -4.651856103264620401, 8.441266197201775512, 0.000000000000000000 ) ) ;
#166361 = CARTESIAN_POINT ( 'NONE',  ( -6.236387472606141458, 10.21960978477508952, -0.7216878364870278340 ) ) ;
#166362 = CARTESIAN_POINT ( 'NONE',  ( 1.371502371489873751, -1.821557607348308405, -1.085495857948336251 ) ) ;
#166363 = CARTESIAN_POINT ( 'NONE',  ( -6.099189001301292379, 8.209082816308541197, 1.599625672291263179 ) ) ;
#166365 = CARTESIAN_POINT ( 'NONE',  ( 4.967221142815226642, 1.706001049663580460, 0.9686458024478412643 ) ) ;
#166364 = CARTESIAN_POINT ( 'NONE',  ( 1.224999999999984990, 1.104166666666725138, 0.7072540797572737237 ) ) ;
#166366 = CARTESIAN_POINT ( 'NONE',  ( 3.678741886385179072, -2.082744454470350615, -0.5786317199799119182 ) ) ;
#166367 = CARTESIAN_POINT ( 'NONE',  ( 2.067674361007607597, -1.131582805410412673, 1.452419944642673100 ) ) ;
#166368 = CARTESIAN_POINT ( 'NONE',  ( -4.055583655087145800, 7.567422049930973671, -0.4132208808486706464 ) ) ;
#166369 = FACE_OUTER_BOUND ( 'NONE', #208395, .T. ) ;
#166370 = CARTESIAN_POINT ( 'NONE',  ( 4.874825007975835511, 1.622202256106145102, -0.6307315249329782381 ) ) ;
#166371 = CARTESIAN_POINT ( 'NONE',  ( 4.020151095146772491, 7.782762254604477015, 0.3270025911792567297 ) ) ;
#166372 = CARTESIAN_POINT ( 'NONE',  ( 6.331294547901813452, 6.488857848747989543, 1.040834085586084257E-14 ) ) ;
#166373 = CARTESIAN_POINT ( 'NONE',  ( -10.93392920578941485, 5.995216197940580471, 6.296921006145307587 ) ) ;
#166374 = AXIS2_PLACEMENT_3D ( 'NONE', #201884, #71892, #105513 ) ;
#166375 = CARTESIAN_POINT ( 'NONE',  ( 1.674925575805393585, -2.052671086741376882, -0.6780288057936025847 ) ) ;
#166376 = CARTESIAN_POINT ( 'NONE',  ( 4.745470142856022200, -1.954873481938533608, -0.4925652823710227612 ) ) ;
#166377 = CARTESIAN_POINT ( 'NONE',  ( -10.60211293576223213, 11.47147930125185589, 1.040834085586084257E-14 ) ) ;
#166378 = CARTESIAN_POINT ( 'NONE',  ( 1.446389902895691693, 2.159248346720197276, 0.1057134262518744372 ) ) ;
#166379 = CARTESIAN_POINT ( 'NONE',  ( 3.924654207020538355, 1.871676352785199393, 0.6194476946735865130 ) ) ;
#166380 = CARTESIAN_POINT ( 'NONE',  ( -3.475000000000000533, -2.756249999044086074, 0.000000000000000000 ) ) ;
#166381 = CARTESIAN_POINT ( 'NONE',  ( 3.245582950214185303, 1.942234966672530261, -0.002794291004394599230 ) ) ;
#166384 = ORIENTED_EDGE ( 'NONE', *, *, #107473, .T. ) ;
#166383 = CARTESIAN_POINT ( 'NONE',  ( -4.394251184604987870, 5.259619482528146150, 1.082531754730549078 ) ) ;
#166382 = CARTESIAN_POINT ( 'NONE',  ( -10.42585693878457853, 11.26584730477792284, -0.7216878364870267237 ) ) ;
#166385 = CARTESIAN_POINT ( 'NONE',  ( -2.997761361953021009, 6.511488999004883205, -0.7216878364870458196 ) ) ;
#166386 = FACE_OUTER_BOUND ( 'NONE', #153767, .T. ) ;
#166387 = CARTESIAN_POINT ( 'NONE',  ( -3.467853430045390706, 7.267855778353407459, 0.7998128361456352531 ) ) ;
#166389 = VERTEX_POINT ( 'NONE', #192595 ) ;
#166388 = CARTESIAN_POINT ( 'NONE',  ( -5.956828388357799042, 8.042995434541133193, 1.599625672291263179 ) ) ;
#166390 = CARTESIAN_POINT ( 'NONE',  ( -7.822691444960696572, 12.07029775252209092, -0.7216878364870267237 ) ) ;
#166391 = CARTESIAN_POINT ( 'NONE',  ( 6.335062919620514599, 0.2175189359726207861, 2.297324976709664845 ) ) ;
#166392 = CARTESIAN_POINT ( 'NONE',  ( -1.642778471874998480, -3.901041666188709289, 2.845375778867863303 ) ) ;
#166393 = CARTESIAN_POINT ( 'NONE',  ( 5.752778578519474273, -0.4731148833870613690, -1.903749215227706015 ) ) ;
#166394 = CARTESIAN_POINT ( 'NONE',  ( 1.406875202279284753, -1.122500148236497575, -1.674886495921081853 ) ) ;
#166395 = ORIENTED_EDGE ( 'NONE', *, *, #141897, .T. ) ;
#166396 = CARTESIAN_POINT ( 'NONE',  ( 3.995394017595743641, -0.3581701549109669869, 2.086669383214428297 ) ) ;
#166397 = CARTESIAN_POINT ( 'NONE',  ( -1.500000000000013101, 3.410416667349487785, -0.8660254037844313801 ) ) ;
#166399 = CARTESIAN_POINT ( 'NONE',  ( -6.715366157470410435, 6.729015360003925750, -0.7998128361456291469 ) ) ;
#166398 = CARTESIAN_POINT ( 'NONE',  ( 9.500331257164623011, -7.246166700193447774, 1.020301583428166389E-12 ) ) ;
#166400 = CARTESIAN_POINT ( 'NONE',  ( 4.031074566243696644, -1.271087849624694233, -1.332192834049110486 ) ) ;
#166401 = VERTEX_POINT ( 'NONE', #8526 ) ;
#166402 = CARTESIAN_POINT ( 'NONE',  ( -6.984421689334302741, 11.30024240419870374, 0.000000000000000000 ) ) ;
#166403 = CARTESIAN_POINT ( 'NONE',  ( 4.711248855110969913, 1.761570823303935551, -1.180294879073326308 ) ) ;
#166404 = CARTESIAN_POINT ( 'NONE',  ( 0.000000000000000000, 3.400000000000000355, 0.000000000000000000 ) ) ;
#166405 = CARTESIAN_POINT ( 'NONE',  ( 5.636439174979242850, 7.598931675607687453, -1.599625672291262513 ) ) ;
#166406 = CARTESIAN_POINT ( 'NONE',  ( 5.659468487958158711, 0.4062720387869744876, -2.020156115232510707 ) ) ;
#166408 = CARTESIAN_POINT ( 'NONE',  ( 2.770863647982471534, 1.747605724785822767, -0.5798694457997202178 ) ) ;
#166407 = CARTESIAN_POINT ( 'NONE',  ( 1.152544200391303786, -0.4473333697519957242, -1.806370492606963474 ) ) ;
#166409 = CARTESIAN_POINT ( 'NONE',  ( 7.964525173024008531, 11.37936423758166526, 1.199719254218460707 ) ) ;
#166410 = CARTESIAN_POINT ( 'NONE',  ( 0.5101186646354113341, -1.387778780781445676E-14, 1.261047121698059215 ) ) ;
#166411 = CARTESIAN_POINT ( 'NONE',  ( 3.015880874418576330, 1.852360388558017545, -0.1794404841957262797 ) ) ;
#166412 = DIRECTION ( 'NONE',  ( 0.000000000000000000, 1.000000000000000000, 0.000000000000000000 ) ) ;
#166413 = DIRECTION ( 'NONE',  ( 0.6507913734559640506, -0.7592566023653004592, 0.000000000000000000 ) ) ;
#166414 = CIRCLE ( 'NONE', #73008, 0.07999999999999971023 ) ;
#166415 = CARTESIAN_POINT ( 'NONE',  ( 1.998912159191484905, -0.5904864226158462737, -2.126349760018491963 ) ) ;
#166416 = CARTESIAN_POINT ( 'NONE',  ( 4.956464464747484477, 0.8595337117903809609, 2.092967149517725112 ) ) ;
#166417 = CARTESIAN_POINT ( 'NONE',  ( 3.591030000661588062, 1.731995077137841843, 1.032480907900306111 ) ) ;
#166418 = AXIS2_PLACEMENT_3D ( 'NONE', #108335, #6472, #25934 ) ;
#166419 = CARTESIAN_POINT ( 'NONE',  ( -7.212574532790100079, 9.437756259720353924, -1.443375672974059665 ) ) ;
#166420 = CARTESIAN_POINT ( 'NONE',  ( 4.341949102618557710, -1.119799544600053265, -1.423922225892548354 ) ) ;
#166421 = CARTESIAN_POINT ( 'NONE',  ( 5.665228803577522676, 1.767359255132592066, -0.7397141715129780248 ) ) ;
#166422 = ADVANCED_FACE ( 'NONE', ( #95137 ), #119683, .T. ) ;
#166423 = CARTESIAN_POINT ( 'NONE',  ( 1.364683531249990311, 5.676041667008088432, 0.7879004041258500513 ) ) ;
#166424 = CARTESIAN_POINT ( 'NONE',  ( 3.766447953776773883, -1.324889289065459774, 1.460063511008972137 ) ) ;
#166425 = CARTESIAN_POINT ( 'NONE',  ( 4.504681594071535677, 1.446009304718363087, -1.186774495104812699 ) ) ;
#166426 = EDGE_CURVE ( 'NONE', #154544, #63320, #208177, .T. ) ;
#166427 = CARTESIAN_POINT ( 'NONE',  ( 5.090230039108806892, 0.9569469540476289726, -1.596034515973473455 ) ) ;
#166428 = CARTESIAN_POINT ( 'NONE',  ( 2.725000000000005862, 0.000000000000000000, 0.000000000000000000 ) ) ;
#166429 = CARTESIAN_POINT ( 'NONE',  ( 4.768267862989370443, -1.154894395163852616, 1.341171105668465646 ) ) ;
#166430 = CARTESIAN_POINT ( 'NONE',  ( 0.5148617154710420918, 0.1531739628206352510, 2.010800830040265996 ) ) ;
#166432 = CARTESIAN_POINT ( 'NONE',  ( 1.910898437428062646, 1.559696066972179107, -1.415416642437119954 ) ) ;
#166431 = CARTESIAN_POINT ( 'NONE',  ( -2.440104460335327463, 5.790612937125752424, 1.040834085586084257E-14 ) ) ;
#166433 = CARTESIAN_POINT ( 'NONE',  ( 9.585778300061798873, 11.14216175728232550, -1.199719254218440723 ) ) ;
#166435 = CARTESIAN_POINT ( 'NONE',  ( -1.154085075685135742, 2.812889018129764107, -0.7749999999999970246 ) ) ;
#166434 = CARTESIAN_POINT ( 'NONE',  ( 0.000000000000000000, 0.5000000000000000000, 10.75000000000000000 ) ) ;
#166436 = CARTESIAN_POINT ( 'NONE',  ( 3.287459871768631636, 0.04819156399121089784, -2.120204644799832394 ) ) ;
#166437 = CARTESIAN_POINT ( 'NONE',  ( -7.777967379493323286, -9.999999999999994671, -7.664830294503433450 ) ) ;
#166438 = CARTESIAN_POINT ( 'NONE',  ( 2.390883991616198578, -1.934022345091526818, -0.5824046739145176677 ) ) ;
#166439 = CARTESIAN_POINT ( 'NONE',  ( -1.201851678989727383E-14, 2.696875000341417916, -1.575800808251660134 ) ) ;
#166440 = CARTESIAN_POINT ( 'NONE',  ( 6.933263157960367629, 7.629137130509066722, 2.653810918356712900 ) ) ;
#166441 = CARTESIAN_POINT ( 'NONE',  ( 4.253507506385319381, 5.985511395581417204, 1.599625672291267398 ) ) ;
#166442 = EDGE_LOOP ( 'NONE', ( #36905, #114274, #147507 ) ) ;
#166443 = CARTESIAN_POINT ( 'NONE',  ( 2.249508738127777630, -1.734628566516350778, -1.289557925820798090 ) ) ;
#166444 = CARTESIAN_POINT ( 'NONE',  ( 6.890000000000009450, 0.5473178204696281801, 2.329866691457019190 ) ) ;
#166447 = CARTESIAN_POINT ( 'NONE',  ( 2.412988153552339643, 5.758977245878946327, 0.7216878364870438212 ) ) ;
#166446 = CARTESIAN_POINT ( 'NONE',  ( 0.4019237886466847653, 13.10491455036743247, 1.499999999999997113 ) ) ;
#166445 = CARTESIAN_POINT ( 'NONE',  ( 4.115782150200256950, 6.959440387612411349, 1.199719254218452047 ) ) ;
#166448 =( BOUNDED_SURFACE ( )  B_SPLINE_SURFACE ( 1, 2, ( 
 ( #187603, #135677, #34946, #167109, #202770, #68504, #171359, #21875, #20819, #3497, #22953, #89067, #18696, #186539, #136743, #84778, #134632, #155125, #6707, #118413, #154056, #101018, #200636, #56556, #39230, #122716, #4558, #38168, #104241, #2427, #150865, #121634, #184398, #52284, #69567, #70632, #36018, #204902, #170287, #169227, #120561, #86915, #152983, #54420, #85847, #105322, #201702, #53345, #87982, #102097, #168167, #37087, #5623, #19765, #72784, #137816, #151924, #203835, #119479, #185467, #103166, #55481, #138884, #209173, #44586, #73866, #208115, #192930, #110699, #139961, #190797, #189737, #172442, #156199, #106419, #42457, #7775, #25101, #205984, #158330, #176699, #59744, #28312, #144252, #142102, #12054, #93342, #207051, #126972, #58683, #94408, #27234, #160447, #125903, #173528, #75997, #191861, #124830, #43522, #74934, #24029, #57620, #174593, #109645, #40312, #78122, #108565, #77051, #91203, #26167, #90132, #8855, #60811, #123777, #92285, #210245, #188678, #41389, #107500, #159378, #9923, #175648, #10977, #143181, #157264, #61881, #141044, #178848, #114952, #177774, #82381, #47793, #213432, #194001, #146359, #32575, #116018, #40, #31525, #112832, #180952, #30459, #211314, #161531, #64013, #128046, #79194, #13116, #132246, #145309, #17363, #16296, #182004, #96544, #130161, #212372, #163658, #164708, #81327, #129107, #45650, #62939, #111767, #195081, #14165, #162591, #80260, #196153, #29389, #46719, #113907, #1113, #179902, #97599, #147406, #15240, #65055, #66104, #33635, #95483, #131211, #197199, #48838, #98651, #148472, #198254, #49894, #99708, #165780, #83447, #149527, #151671, #5364, #67174, #135420, #3242, #68244, #150607, #153794, #105063, #19505, #184140, #119217, #87721, #21613, #167907, #187348, #69308, #2167, #170027, #154864, #200382, #71446, #35764, #201441, #121373, #137558, #171101, #202510, #38977, #133309, #54160, #101839, #186272, #53082, #199314, #22692, #34695, #70373, #50960, #134378, #120299, #203576, #185200, #86652, #36825, #102906, #88805, #100764, #37908, #166846 ),
 ( #117084, #183083, #103984, #18442, #55227, #84519, #52030, #118156, #85581, #168965, #20569, #152720, #4302, #136488, #10722, #76791, #106159, #8594, #7517, #204643, #188413, #138620, #74676, #40050, #57359, #172185, #190540, #142913, #25907, #208913, #176444, #174331, #44320, #125640, #24843, #159121, #90942, #60547, #59483, #126705, #92017, #205724, #108311, #158075, #157008, #9663, #107241, #56294, #23775, #206794, #75739, #72524, #192666, #140779, #109381, #123522, #58426, #122454, #41129, #26974, #89880, #124579, #28056, #6446, #189486, #43263, #110442, #42196, #173262, #155932, #94149, #73599, #139701, #141852, #207857, #191601, #175388, #93079, #77863, #113640, #193743, #82122, #147154, #146098, #128830, #148215, #214217, #143986, #97339, #47527, #209977, #45389, #65846, #131995, #29123, #64808, #11789, #111505, #181746, #98388, #33376, #129905, #163397, #14971, #127788, #61618, #32320, #95210, #177511, #194812, #195889, #161259, #115755, #81068, #79994, #31265, #212109, #63746, #179645, #211045, #16039, #46448, #112569, #213179, #12846, #78920, #145042, #62671, #178580, #30188, #96278, #162328, #13912, #130955, #196945, #48585, #160188, #114701, #180695, #164452, #198004, #49630, #186016, #87478, #165514, #135176, #168715, #17106, #167651, #4052, #20319, #103730, #52830, #187091, #19252, #85332, #183894, #37652, #99457, #151415, #35506, #100514, #182825, #169781, #137307, #51784, #1920, #2989, #120042, #53907, #200131, #5113, #101583, #34441, #202256, #83184, #18178, #21370, #67979, #69056, #153544, #71190, #203324, #86405, #54975, #149267, #152472, #134122, #70122, #201191, #846, #121127, #66911, #102658, #133051, #166589, #136233, #199053, #118967, #184945, #36572, #50699, #116823, #84265, #150350, #117901, #158875, #58172, #6192, #155678, #154613, #122198, #157823, #8345, #74430, #206542, #124330, #72261, #208666, #59227, #89626, #25657, #88552, #207608, #173006, #190290, #104806, #57106, #9419, #26729, #125385, #156756, #23520, #91767, #7260, #188160, #138369, #189237, #38725, #204386, #56042 ) ),
 .UNSPECIFIED., .F., .F., .T. ) 
 B_SPLINE_SURFACE_WITH_KNOTS ( ( 2, 2 ),
 ( 3, 2, 2, 2, 2, 2, 2, 2, 2, 2, 2, 2, 2, 2, 2, 2, 2, 2, 2, 2, 2, 2, 2, 2, 2, 2, 2, 2, 2, 2, 2, 2, 2, 2, 2, 2, 2, 2, 2, 2, 2, 2, 2, 2, 2, 2, 2, 2, 2, 2, 2, 2, 2, 2, 2, 2, 2, 2, 2, 2, 2, 2, 2, 2, 2, 2, 2, 2, 2, 2, 2, 2, 2, 2, 2, 2, 2, 2, 2, 2, 2, 2, 2, 2, 2, 2, 2, 2, 2, 2, 2, 2, 2, 2, 2, 2, 2, 2, 2, 2, 2, 2, 2, 2, 2, 2, 2, 2, 2, 2, 2, 2, 2, 2, 2, 2, 2, 2, 2, 2, 3 ),
 ( 0.000000000000000000, 1.000000000000000000 ),
 ( 0.000000000000000000, 0.008333333333333333218, 0.01666666666666666644, 0.02500000000000000139, 0.03333333333333333287, 0.04166666666666666435, 0.05000000000000000278, 0.05833333333333333426, 0.06666666666666666574, 0.07499999999999999722, 0.08333333333333332871, 0.09166666666666666019, 0.1000000000000000056, 0.1083333333333333370, 0.1166666666666666685, 0.1250000000000000000, 0.1333333333333333315, 0.1416666666666666630, 0.1499999999999999944, 0.1583333333333333259, 0.1666666666666666574, 0.1749999999999999889, 0.1833333333333333204, 0.1916666666666666796, 0.2000000000000000111, 0.2083333333333333426, 0.2166666666666666741, 0.2250000000000000056, 0.2333333333333333370, 0.2416666666666666685, 0.2500000000000000000, 0.2583333333333333592, 0.2666666666666666630, 0.2750000000000000222, 0.2833333333333333259, 0.2916666666666666852, 0.2999999999999999889, 0.3083333333333333481, 0.3166666666666666519, 0.3250000000000000111, 0.3333333333333333148, 0.3416666666666666741, 0.3499999999999999778, 0.3583333333333333370, 0.3666666666666666408, 0.3750000000000000000, 0.3833333333333333592, 0.3916666666666666630, 0.4000000000000000222, 0.4083333333333333259, 0.4166666666666666852, 0.4249999999999999889, 0.4333333333333333481, 0.4416666666666666519, 0.4500000000000000111, 0.4583333333333333148, 0.4666666666666666741, 0.4749999999999999778, 0.4833333333333333370, 0.4916666666666666408, 0.5000000000000000000, 0.5083333333333333037, 0.5166666666666667185, 0.5250000000000000222, 0.5333333333333333259, 0.5416666666666666297, 0.5500000000000000444, 0.5583333333333333481, 0.5666666666666666519, 0.5749999999999999556, 0.5833333333333333703, 0.5916666666666666741, 0.5999999999999999778, 0.6083333333333332815, 0.6166666666666666963, 0.6250000000000000000, 0.6333333333333333037, 0.6416666666666667185, 0.6500000000000000222, 0.6583333333333333259, 0.6666666666666666297, 0.6750000000000000444, 0.6833333333333333481, 0.6916666666666666519, 0.6999999999999999556, 0.7083333333333333703, 0.7166666666666666741, 0.7249999999999999778, 0.7333333333333332815, 0.7416666666666666963, 0.7500000000000000000, 0.7583333333333333037, 0.7666666666666667185, 0.7750000000000000222, 0.7833333333333333259, 0.7916666666666666297, 0.8000000000000000444, 0.8083333333333333481, 0.8166666666666666519, 0.8249999999999999556, 0.8333333333333333703, 0.8416666666666666741, 0.8499999999999999778, 0.8583333333333332815, 0.8666666666666666963, 0.8750000000000000000, 0.8833333333333333037, 0.8916666666666667185, 0.9000000000000000222, 0.9083333333333333259, 0.9166666666666666297, 0.9250000000000000444, 0.9333333333333333481, 0.9416666666666666519, 0.9499999999999999556, 0.9583333333333333703, 0.9666666666666666741, 0.9749999999999999778, 0.9833333333333332815, 0.9916666666666666963, 1.000000000000000000 ),
 .UNSPECIFIED. ) 
 GEOMETRIC_REPRESENTATION_ITEM ( )  RATIONAL_B_SPLINE_SURFACE ( (
 ( 1.000000000000000000, 0.8660254037844387076, 1.000000000000000000, 0.8660254037844387076, 1.000000000000000000, 0.8660254037844387076, 1.000000000000000000, 0.8660254037844387076, 1.000000000000000000, 0.8660254037844387076, 1.000000000000000000, 0.8660254037844387076, 1.000000000000000000, 0.8660254037844387076, 1.000000000000000000, 0.8660254037844387076, 1.000000000000000000, 0.8660254037844387076, 1.000000000000000000, 0.8660254037844387076, 1.000000000000000000, 0.8660254037844387076, 1.000000000000000000, 0.8660254037844387076, 1.000000000000000000, 0.8660254037844387076, 1.000000000000000000, 0.8660254037844387076, 1.000000000000000000, 0.8660254037844387076, 1.000000000000000000, 0.8660254037844387076, 1.000000000000000000, 0.8660254037844387076, 1.000000000000000000, 0.8660254037844387076, 1.000000000000000000, 0.8660254037844387076, 1.000000000000000000, 0.8660254037844387076, 1.000000000000000000, 0.8660254037844387076, 1.000000000000000000, 0.8660254037844387076, 1.000000000000000000, 0.8660254037844387076, 1.000000000000000000, 0.8660254037844387076, 1.000000000000000000, 0.8660254037844387076, 1.000000000000000000, 0.8660254037844387076, 1.000000000000000000, 0.8660254037844387076, 1.000000000000000000, 0.8660254037844387076, 1.000000000000000000, 0.8660254037844387076, 1.000000000000000000, 0.8660254037844387076, 1.000000000000000000, 0.8660254037844387076, 1.000000000000000000, 0.8660254037844387076, 1.000000000000000000, 0.8660254037844387076, 1.000000000000000000, 0.8660254037844387076, 1.000000000000000000, 0.8660254037844387076, 1.000000000000000000, 0.8660254037844387076, 1.000000000000000000, 0.8660254037844387076, 1.000000000000000000, 0.8660254037844387076, 1.000000000000000000, 0.8660254037844387076, 1.000000000000000000, 0.8660254037844387076, 1.000000000000000000, 0.8660254037844387076, 1.000000000000000000, 0.8660254037844387076, 1.000000000000000000, 0.8660254037844387076, 1.000000000000000000, 0.8660254037844387076, 1.000000000000000000, 0.8660254037844387076, 1.000000000000000000, 0.8660254037844387076, 1.000000000000000000, 0.8660254037844387076, 1.000000000000000000, 0.8660254037844387076, 1.000000000000000000, 0.8660254037844387076, 1.000000000000000000, 0.8660254037844387076, 1.000000000000000000, 0.8660254037844387076, 1.000000000000000000, 0.8660254037844387076, 1.000000000000000000, 0.8660254037844387076, 1.000000000000000000, 0.8660254037844387076, 1.000000000000000000, 0.8660254037844387076, 1.000000000000000000, 0.8660254037844387076, 1.000000000000000000, 0.8660254037844387076, 1.000000000000000000, 0.8660254037844387076, 1.000000000000000000, 0.8660254037844387076, 1.000000000000000000, 0.8660254037844387076, 1.000000000000000000, 0.8660254037844387076, 1.000000000000000000, 0.8660254037844387076, 1.000000000000000000, 0.8660254037844387076, 1.000000000000000000, 0.8660254037844387076, 1.000000000000000000, 0.8660254037844387076, 1.000000000000000000, 0.8660254037844387076, 1.000000000000000000, 0.8660254037844387076, 1.000000000000000000, 0.8660254037844387076, 1.000000000000000000, 0.8660254037844387076, 1.000000000000000000, 0.8660254037844387076, 1.000000000000000000, 0.8660254037844387076, 1.000000000000000000, 0.8660254037844387076, 1.000000000000000000, 0.8660254037844387076, 1.000000000000000000, 0.8660254037844387076, 1.000000000000000000, 0.8660254037844387076, 1.000000000000000000, 0.8660254037844387076, 1.000000000000000000, 0.8660254037844387076, 1.000000000000000000, 0.8660254037844387076, 1.000000000000000000, 0.8660254037844387076, 1.000000000000000000, 0.8660254037844387076, 1.000000000000000000, 0.8660254037844387076, 1.000000000000000000, 0.8660254037844387076, 1.000000000000000000, 0.8660254037844387076, 1.000000000000000000, 0.8660254037844387076, 1.000000000000000000, 0.8660254037844387076, 1.000000000000000000, 0.8660254037844387076, 1.000000000000000000, 0.8660254037844387076, 1.000000000000000000, 0.8660254037844387076, 1.000000000000000000, 0.8660254037844387076, 1.000000000000000000, 0.8660254037844387076, 1.000000000000000000, 0.8660254037844387076, 1.000000000000000000, 0.8660254037844387076, 1.000000000000000000, 0.8660254037844387076, 1.000000000000000000, 0.8660254037844387076, 1.000000000000000000, 0.8660254037844387076, 1.000000000000000000, 0.8660254037844387076, 1.000000000000000000, 0.8660254037844387076, 1.000000000000000000, 0.8660254037844387076, 1.000000000000000000, 0.8660254037844387076, 1.000000000000000000, 0.8660254037844387076, 1.000000000000000000, 0.8660254037844387076, 1.000000000000000000, 0.8660254037844387076, 1.000000000000000000, 0.8660254037844387076, 1.000000000000000000, 0.8660254037844387076, 1.000000000000000000, 0.8660254037844387076, 1.000000000000000000, 0.8660254037844387076, 1.000000000000000000, 0.8660254037844387076, 1.000000000000000000, 0.8660254037844387076, 1.000000000000000000, 0.8660254037844387076, 1.000000000000000000, 0.8660254037844387076, 1.000000000000000000, 0.8660254037844387076, 1.000000000000000000, 0.8660254037844387076, 1.000000000000000000, 0.8660254037844387076, 1.000000000000000000, 0.8660254037844387076, 1.000000000000000000, 0.8660254037844387076, 1.000000000000000000, 0.8660254037844387076, 1.000000000000000000, 0.8660254037844387076, 1.000000000000000000, 0.8660254037844387076, 1.000000000000000000, 0.8660254037844387076, 1.000000000000000000, 0.8660254037844387076, 1.000000000000000000),
 ( 1.000000000000000000, 0.8660254037844387076, 1.000000000000000000, 0.8660254037844387076, 1.000000000000000000, 0.8660254037844387076, 1.000000000000000000, 0.8660254037844387076, 1.000000000000000000, 0.8660254037844387076, 1.000000000000000000, 0.8660254037844387076, 1.000000000000000000, 0.8660254037844387076, 1.000000000000000000, 0.8660254037844387076, 1.000000000000000000, 0.8660254037844387076, 1.000000000000000000, 0.8660254037844387076, 1.000000000000000000, 0.8660254037844387076, 1.000000000000000000, 0.8660254037844387076, 1.000000000000000000, 0.8660254037844387076, 1.000000000000000000, 0.8660254037844387076, 1.000000000000000000, 0.8660254037844387076, 1.000000000000000000, 0.8660254037844387076, 1.000000000000000000, 0.8660254037844387076, 1.000000000000000000, 0.8660254037844387076, 1.000000000000000000, 0.8660254037844387076, 1.000000000000000000, 0.8660254037844387076, 1.000000000000000000, 0.8660254037844387076, 1.000000000000000000, 0.8660254037844387076, 1.000000000000000000, 0.8660254037844387076, 1.000000000000000000, 0.8660254037844387076, 1.000000000000000000, 0.8660254037844387076, 1.000000000000000000, 0.8660254037844387076, 1.000000000000000000, 0.8660254037844387076, 1.000000000000000000, 0.8660254037844387076, 1.000000000000000000, 0.8660254037844387076, 1.000000000000000000, 0.8660254037844387076, 1.000000000000000000, 0.8660254037844387076, 1.000000000000000000, 0.8660254037844387076, 1.000000000000000000, 0.8660254037844387076, 1.000000000000000000, 0.8660254037844387076, 1.000000000000000000, 0.8660254037844387076, 1.000000000000000000, 0.8660254037844387076, 1.000000000000000000, 0.8660254037844387076, 1.000000000000000000, 0.8660254037844387076, 1.000000000000000000, 0.8660254037844387076, 1.000000000000000000, 0.8660254037844387076, 1.000000000000000000, 0.8660254037844387076, 1.000000000000000000, 0.8660254037844387076, 1.000000000000000000, 0.8660254037844387076, 1.000000000000000000, 0.8660254037844387076, 1.000000000000000000, 0.8660254037844387076, 1.000000000000000000, 0.8660254037844387076, 1.000000000000000000, 0.8660254037844387076, 1.000000000000000000, 0.8660254037844387076, 1.000000000000000000, 0.8660254037844387076, 1.000000000000000000, 0.8660254037844387076, 1.000000000000000000, 0.8660254037844387076, 1.000000000000000000, 0.8660254037844387076, 1.000000000000000000, 0.8660254037844387076, 1.000000000000000000, 0.8660254037844387076, 1.000000000000000000, 0.8660254037844387076, 1.000000000000000000, 0.8660254037844387076, 1.000000000000000000, 0.8660254037844387076, 1.000000000000000000, 0.8660254037844387076, 1.000000000000000000, 0.8660254037844387076, 1.000000000000000000, 0.8660254037844387076, 1.000000000000000000, 0.8660254037844387076, 1.000000000000000000, 0.8660254037844387076, 1.000000000000000000, 0.8660254037844387076, 1.000000000000000000, 0.8660254037844387076, 1.000000000000000000, 0.8660254037844387076, 1.000000000000000000, 0.8660254037844387076, 1.000000000000000000, 0.8660254037844387076, 1.000000000000000000, 0.8660254037844387076, 1.000000000000000000, 0.8660254037844387076, 1.000000000000000000, 0.8660254037844387076, 1.000000000000000000, 0.8660254037844387076, 1.000000000000000000, 0.8660254037844387076, 1.000000000000000000, 0.8660254037844387076, 1.000000000000000000, 0.8660254037844387076, 1.000000000000000000, 0.8660254037844387076, 1.000000000000000000, 0.8660254037844387076, 1.000000000000000000, 0.8660254037844387076, 1.000000000000000000, 0.8660254037844387076, 1.000000000000000000, 0.8660254037844387076, 1.000000000000000000, 0.8660254037844387076, 1.000000000000000000, 0.8660254037844387076, 1.000000000000000000, 0.8660254037844387076, 1.000000000000000000, 0.8660254037844387076, 1.000000000000000000, 0.8660254037844387076, 1.000000000000000000, 0.8660254037844387076, 1.000000000000000000, 0.8660254037844387076, 1.000000000000000000, 0.8660254037844387076, 1.000000000000000000, 0.8660254037844387076, 1.000000000000000000, 0.8660254037844387076, 1.000000000000000000, 0.8660254037844387076, 1.000000000000000000, 0.8660254037844387076, 1.000000000000000000, 0.8660254037844387076, 1.000000000000000000, 0.8660254037844387076, 1.000000000000000000, 0.8660254037844387076, 1.000000000000000000, 0.8660254037844387076, 1.000000000000000000, 0.8660254037844387076, 1.000000000000000000, 0.8660254037844387076, 1.000000000000000000, 0.8660254037844387076, 1.000000000000000000, 0.8660254037844387076, 1.000000000000000000, 0.8660254037844387076, 1.000000000000000000, 0.8660254037844387076, 1.000000000000000000, 0.8660254037844387076, 1.000000000000000000, 0.8660254037844387076, 1.000000000000000000, 0.8660254037844387076, 1.000000000000000000, 0.8660254037844387076, 1.000000000000000000, 0.8660254037844387076, 1.000000000000000000, 0.8660254037844387076, 1.000000000000000000, 0.8660254037844387076, 1.000000000000000000, 0.8660254037844387076, 1.000000000000000000, 0.8660254037844387076, 1.000000000000000000, 0.8660254037844387076, 1.000000000000000000, 0.8660254037844387076, 1.000000000000000000, 0.8660254037844387076, 1.000000000000000000, 0.8660254037844387076, 1.000000000000000000, 0.8660254037844387076, 1.000000000000000000, 0.8660254037844387076, 1.000000000000000000, 0.8660254037844387076, 1.000000000000000000, 0.8660254037844387076, 1.000000000000000000, 0.8660254037844387076, 1.000000000000000000, 0.8660254037844387076, 1.000000000000000000) ) ) 
 REPRESENTATION_ITEM ( '' )  SURFACE ( )  );
#166449 = CARTESIAN_POINT ( 'NONE',  ( 8.039621902779343188, 12.32338328664385507, -0.7216878364870328300 ) ) ;
#166450 = DIRECTION ( 'NONE',  ( -5.551115123125764829E-17, 0.000000000000000000, 1.000000000000000000 ) ) ;
#166451 = CARTESIAN_POINT ( 'NONE',  ( -6.507550544879489252, 9.575597488125954015, 1.082531754730548412 ) ) ;
#166452 = ADVANCED_BREP_SHAPE_REPRESENTATION ( '', ( #18139, #200407 ), #138598 ) ;
#166453 = CARTESIAN_POINT ( 'NONE',  ( 0.4686481397476391364, -2.065551408369214137, -0.7328327568804984260 ) ) ;
#166454 = CARTESIAN_POINT ( 'NONE',  ( 0.2837385194700463575, 8.150966340525164000, 2.020310785919128715 ) ) ;
#166455 = CARTESIAN_POINT ( 'NONE',  ( 1.429016818436980474, 2.180957219565873295, 0.6017249355739097139 ) ) ;
#166456 = CARTESIAN_POINT ( 'NONE',  ( -8.355902744723985975, 8.642974711799791265, 1.040834085586084257E-14 ) ) ;
#166457 = CARTESIAN_POINT ( 'NONE',  ( -4.406036734316898240, 6.163462161501577441, -1.443375672974051449 ) ) ;
#166458 = CARTESIAN_POINT ( 'NONE',  ( -1.201851678989727383E-14, 2.384375000341416584, 1.575800808251672791 ) ) ;
#166459 = CARTESIAN_POINT ( 'NONE',  ( -10.91033920341459051, 4.885615726745599297, 4.996448585388897357 ) ) ;
#166460 = CARTESIAN_POINT ( 'NONE',  ( 1.499999999999993117, 10.85416666666666785, 0.8660254037844409281 ) ) ;
#166461 = CARTESIAN_POINT ( 'NONE',  ( 5.885648082108177803, 9.880690172519326353, 0.7216878364870317197 ) ) ;
#166462 = CARTESIAN_POINT ( 'NONE',  ( 3.602599932655100812, 1.396742099285839256, -1.086680525292152977 ) ) ;
#166463 = CARTESIAN_POINT ( 'NONE',  ( 6.668967514498191029, -2.014860697535350020, -0.9005387006749266954 ) ) ;
#166464 = ORIENTED_EDGE ( 'NONE', *, *, #19949, .T. ) ;
#166465 = CARTESIAN_POINT ( 'NONE',  ( -6.445975688654487001, 6.485002823043819475, -0.7998128361456362523 ) ) ;
#166466 = CARTESIAN_POINT ( 'NONE',  ( 4.886342304379578394, -0.6820123065829877262, -1.897693145932321634 ) ) ;
#166467 = ORIENTED_EDGE ( 'NONE', *, *, #209086, .F. ) ;
#166468 = CARTESIAN_POINT ( 'NONE',  ( 2.026040307571222332, 1.079255042350239391, -1.527726335390042545 ) ) ;
#166469 = CARTESIAN_POINT ( 'NONE',  ( 2.500909639826456754, 0.4493149015136475022, 2.020762751476639529 ) ) ;
#166470 = TOROIDAL_SURFACE ( 'NONE', #7360, 7.750000000000000888, 0.7500000000000000000 ) ;
#166471 = CARTESIAN_POINT ( 'NONE',  ( -7.282137903871469753, 8.628820655005750240, 1.082531754730549078 ) ) ;
#166472 = CARTESIAN_POINT ( 'NONE',  ( 2.091926199050548441, 1.179367891222588005, 1.505316542580182659 ) ) ;
#166473 = CARTESIAN_POINT ( 'NONE',  ( 0.4019237886466778820, 9.573664549684629321, 1.500000000000001554 ) ) ;
#166474 = CARTESIAN_POINT ( 'NONE',  ( -10.14898710519052649, 3.000029897349846930, -7.601419320309957151 ) ) ;
#166475 = CARTESIAN_POINT ( 'NONE',  ( 5.411112705185558092, 6.445957923205511086, -1.082531754730548412 ) ) ;
#166476 = B_SPLINE_CURVE_WITH_KNOTS ( 'NONE', 3,
 ( #137255, #53856, #203274, #85277, #52776, #184895, #69005, #182768, #132997, #198998, #165457, #84210, #151363, #149211, #87425, #34385, #201138, #134070, #50644, #86350, #100457, #168661, #119989, #115701, #183841, #71137, #135122, #167600, #118914, #2933, #117849, #166532, #181693, #18122, #150298, #66853, #19199, #1864, #21318, #200079, #116771, #786, #36520, #185966, #37598, #67925, #33323, #102607, #20266, #17052, #152421, #4000, #136182, #202200, #169729, #153492, #5062, #121072, #90643, #188108, #175093, #140480, #73283, #72208, #25608, #39738, #206492, #174036, #24535, #91720, #88499, #6138, #41898, #204330, #138315, #55989, #122140, #189186, #157771, #191301, #74378, #172956, #155625, #26681, #139387, #105843, #9370, #142607, #171870, #59181, #23466, #92783, #89576, #123222, #40823, #7210, #156703, #58122, #205420, #76496, #57057, #10424, #42969, #125338, #106932, #8294, #124281, #75441, #158828, #54921, #190240, #109077, #108009, #187040, #141553, #38672, #104751, #207560, #170800, #22389, #154561, #14683, #78628, #12553, #112275, #176156, #80780, #15747, #94914, #144752, #180406, #28826, #128548, #44025, #163103, #194514, #79700, #60249, #210764, #113348, #196655, #62384, #47231, #178290, #97050, #110143, #208616, #160963, #32025, #179353, #30975, #46162, #63457, #130666, #146868, #29898, #212889, #95984, #64520, #48295, #114407, #27756, #164162, #61326, #126406, #127486, #98110, #192366, #93851, #159889, #81832, #162036, #13627, #193457, #11496, #45101, #111210, #77568, #145813, #211820, #143690, #209682, #177213, #129611, #195596, #152170, #3739, #116520, #147915, #86094, #83951, #135920, #150042, #1613, #181456, #134874, #65553, #37342, #103416, #69814, #201939, #131698, #53595, #52526, #151114, #49346, #67672, #167353, #133816, #51471, #99161, #18940, #119729, #2680, #148965, #213931, #185708, #199830, #168413, #17868, #166277, #200881, #35194, #102341, #117595, #183586, #197704, #169476, #82889, #36263, #115465, #101269, #21061, #33086, #182511, #184644, #165214, #85025, #68752, #118660, #20010, #16804, #537, #66604, #132750, #198753, #50400, #34141, #100210, #56798, #38412, #9114, #186786, #153229, #54661, #40564, #41643, #39477, #5877, #70879, #57864, #87158, #154303, #191050, #136992, #4799, #120809, #108823, #25358, #174848, #122967, #24273, #156448, #106671, #71951, #104494, #170537, #203019, #55726, #188926, #22122, #207311, #88234, #91458, #75190, #125092, #157519, #204074, #140218, #141302, #138061, #155364, #42715, #172695, #6949, #90379, #8032, #189992, #205155, #58934, #121880, #187851, #74122, #206237, #124026, #107757, #105576, #171608, #173783, #23202, #89317, #73029, #139128, #160707, #129366, #162852, #45912, #110953, #62144, #192116, #12301, #109893, #195344, #114166, #159641, #30720, #11238, #146618, #27497, #94664, #78381, #175906, #128304, #112030, #176960, #48053, #28576, #113092, #194266, #43780, #96803, #144502, #178032, #46976, #64276, #130421, #44847, #14430, #79453, #80520, #13378, #212635, #26425, #210509, #29650, #10176, #196408, #92537, #95735, #161787, #158577, #208369, #179098, #76250, #127230, #145569, #142359, #61071, #211568, #60000, #126153, #63202, #93597, #77317, #143430, #209426, #193199, #101020, #116277, #82640, #102099, #81584, #180159, #132511, #3500, #84781, #18699 ),
 .UNSPECIFIED., .F., .F.,
 ( 4, 1, 1, 1, 1, 1, 1, 1, 1, 1, 1, 1, 1, 1, 1, 1, 1, 1, 1, 1, 1, 1, 1, 1, 1, 1, 1, 1, 1, 1, 1, 1, 1, 1, 1, 1, 1, 1, 1, 1, 1, 1, 1, 1, 1, 1, 1, 1, 1, 1, 1, 1, 1, 1, 1, 1, 1, 1, 1, 1, 1, 1, 1, 1, 1, 1, 1, 1, 1, 1, 1, 1, 1, 1, 1, 1, 1, 1, 1, 1, 1, 1, 1, 1, 1, 1, 1, 1, 1, 1, 1, 1, 1, 1, 1, 1, 1, 1, 1, 1, 1, 1, 1, 1, 1, 1, 1, 1, 1, 1, 1, 1, 1, 1, 1, 1, 1, 1, 1, 1, 1, 1, 1, 1, 1, 1, 1, 1, 1, 1, 1, 1, 1, 1, 1, 1, 1, 1, 1, 1, 1, 1, 1, 1, 1, 1, 1, 1, 1, 1, 1, 1, 1, 1, 1, 1, 1, 1, 1, 1, 1, 1, 1, 1, 1, 1, 1, 1, 1, 1, 1, 1, 1, 1, 1, 1, 1, 1, 1, 1, 1, 1, 1, 1, 1, 1, 1, 1, 1, 1, 1, 1, 1, 1, 1, 1, 1, 1, 1, 1, 1, 1, 1, 1, 1, 1, 1, 1, 1, 1, 1, 1, 1, 1, 1, 1, 1, 1, 1, 1, 1, 1, 1, 1, 1, 1, 1, 1, 1, 1, 1, 1, 1, 1, 1, 1, 1, 1, 1, 1, 1, 1, 1, 1, 1, 1, 1, 1, 1, 1, 1, 1, 1, 1, 1, 1, 1, 1, 1, 1, 1, 1, 1, 1, 1, 1, 1, 1, 1, 1, 1, 1, 1, 1, 1, 1, 1, 1, 1, 1, 1, 1, 1, 1, 1, 1, 1, 1, 1, 1, 1, 1, 1, 1, 1, 1, 1, 1, 1, 1, 1, 1, 1, 1, 1, 1, 1, 1, 1, 1, 1, 1, 1, 1, 1, 1, 1, 1, 1, 1, 1, 1, 1, 1, 1, 1, 1, 1, 1, 1, 1, 1, 1, 1, 1, 1, 1, 1, 1, 1, 1, 1, 1, 1, 1, 1, 1, 1, 1, 1, 1, 1, 1, 1, 1, 1, 1, 1, 1, 1, 1, 1, 1, 1, 1, 1, 1, 1, 1, 1, 1, 1, 1, 1, 1, 1, 1, 1, 1, 1, 1, 1, 1, 1, 4 ),
 ( 0.000000000000000000, 0.002600214693118923798, 0.005208871813129847643, 0.007813341859462101871, 0.01041561011214237054, 0.01302159838915000617, 0.01562452542669844589, 0.01822945805747129902, 0.02083332260852943998, 0.02343713088342555886, 0.02604210653276634729, 0.02864513693292065552, 0.03125071383394792401, 0.03385356881896259273, 0.03645895053148855841, 0.03906228851054763251, 0.04166670673482164577, 0.04427111720854654681, 0.04687446234244373178, 0.04947983976256019323, 0.05208269766733494843, 0.05468827385445936690, 0.05729129101459448647, 0.05989628262864687969, 0.06250008845252298662, 0.06510390268380349121, 0.06770888856031336001, 0.07031191025079500112, 0.07291748459129859805, 0.07552033970978830335, 0.07812571920045624507, 0.08072905536012038585, 0.08333347174482363950, 0.08593788071299547637, 0.08854122383090638759, 0.09114659965375219997, 0.09374945576594469199, 0.09635503022752239799, 0.09895804583665256116, 0.1015630356028039000, 0.1041668400134527495, 0.1067706523020897913, 0.1093756367037285043, 0.1119786565701353653, 0.1145842293264338063, 0.1171870828570002881, 0.1197924606432616973, 0.1223957954228293843, 0.1250002099740243899, 0.1276046175975352470, 0.1302079588893767237, 0.1328133332639841735, 0.1354161877457908392, 0.1380217606440506395, 0.1406247748629219918, 0.1432297629411592166, 0.1458335661004374617, 0.1484373766077259071, 0.1510423596945167368, 0.1536453778991425101, 0.1562509492307036785, 0.1588538013357113088, 0.1614591775772540871, 0.1640625111385781432, 0.1666669240170048083, 0.1692713304565471311, 0.1718746700842041231, 0.1744800431702197008, 0.1770828961840006377, 0.1796884676783837009, 0.1822914806691622869, 0.1848964672195632097, 0.1875002692887918765, 0.1901040781760970355, 0.1927090601080766463, 0.1953120768130981733, 0.1979176468793322763, 0.2005204977210985895, 0.2031258725775486607, 0.2057292050824250096, 0.2083336164487647746, 0.2109380218649763994, 0.2135413599902747928, 0.2161467319472901716, 0.2187495836553486062, 0.2213551539052408534, 0.2239581658300387468, 0.2265631510126252801, 0.2291669521530730058, 0.2317707595817034838, 0.2343757405188569010, 0.2369787558863956922, 0.2395843248466610342, 0.2421871745874512594, 0.2447925482183819501, 0.2473958798285567084, 0.2500002898434375842, 0.2526046943969075254, 0.2552080311816201097, 0.2578134021691782518, 0.2604162527337665622, 0.2630218218985046486, 0.2656248329193858781, 0.2682298168941298910, 0.2708336172670197106, 0.2734374233982336255, 0.2760424035005001331, 0.2786454176926287940, 0.2812509857062375773, 0.2838538345082703418, 0.2864592070732082663, 0.2890625379503836689, 0.2916669467743862043, 0.2942713506256608436, 0.2968746862315132518, 0.2994800564091141259, 0.3020829059924399762, 0.3046884742313171190, 0.3072914845103039694, 0.3098964674371332273, 0.3125002672036480411, 0.3151040721986592130, 0.3177090516259382103, 0.3203120648046862140, 0.3229176320309106729, 0.3255204800563645251, 0.3281258517147956355, 0.3307291820206363919, 0.3333335898142997245, 0.3359379931238887229, 0.3385413277125659537, 0.3411466972396727249, 0.3437495460039050044, 0.3463551134761772565, 0.3489581231752558743, 0.3515631052140602009, 0.3541669045353489920, 0.3567707085553323276, 0.3593756874674896018, 0.3619786997948497009, 0.3645842663929277916, 0.3671871138039469185, 0.3697924847153226668, 0.3723958146114617063, 0.3750002215352895019, 0.3776046244636719340, 0.3802079581968237365, 0.3828133272328684833, 0.3854161753401436075, 0.3880217422050354359, 0.3906247514861621029, 0.3932297327967993472, 0.3958335318339832876, 0.3984373350400814418, 0.4010423135969549691, 0.4036453252348887744, 0.4062508913640303643, 0.4088537383227308641, 0.4114591086464738368, 0.4140624382945181647, 0.4166668445089845574, 0.4192712472166146842, 0.4218745802558619973, 0.4244799489602520959, 0.4270827965726798348, 0.4296883629893904488, 0.4322913720144979099, 0.4348963527567997200, 0.4375001516709778882, 0.4401039542243071478, 0.4427089325857130886, 0.4453119436961573974, 0.4479175095155500941, 0.4505203561840259718, 0.4531257260795358843, 0.4557290556410732441, 0.4583334613066292196, 0.4609378639539425948, 0.4635411964608836533, 0.4661465649930071620, 0.4687494122726767465, 0.4713549784003855381, 0.4739579873313886638, 0.4765629676651664814, 0.4791667666174222462, 0.4817705686790782482, 0.4843755470048167200, 0.4869785577496898998, 0.4895841234185048796, 0.4921869699588339309, 0.4947923395854939010, 0.4973956692220981579, 0.5000000744991768276, 0.5026044772465965149, 0.5052078093828125116, 0.5078131779020444991, 0.5104160250110306718, 0.5130215910089035436, 0.5156246000077054914, 0.5182295800927568807, 0.5208333792441637300, 0.5234371809752277338, 0.5260421594250891397, 0.5286451699662961801, 0.5312507356436946271, 0.5338535822179446555, 0.5364589517351265879, 0.5390622816083643354, 0.5416666866573878192, 0.5442710896653298880, 0.5468744215923915242, 0.5494797902580997873, 0.5520826373584690749, 0.5546882033856646022, 0.5572912126141627009, 0.5598961926102767883, 0.5624999921219043797, 0.5651037936834493181, 0.5677087724172201755, 0.5703117829166597375, 0.5729173487617980065, 0.5755201955320329299, 0.5781255650991041772, 0.5807288953705399548, 0.5833333003519244331, 0.5859377037808047861, 0.5885410356602774895, 0.5911464046318289922, 0.5937492518856454238, 0.5963548181013198501, 0.5989578277214122615, 0.6015628077883760083, 0.6041666078212959423, 0.6067704093743923055, 0.6093753885518610192, 0.6119783991714310423, 0.6145839653434672645, 0.6171868124717531101, 0.6197921822480817466, 0.6223955130792849788, 0.6249999181534476866, 0.6276043221636865566, 0.6302076541571374202, 0.6328130235939036785, 0.6354158711632348355, 0.6380214377265494008, 0.6406244479001403924, 0.6432294281977445349, 0.6458332289130368498, 0.6484370306187589028, 0.6510420103997216490, 0.6536450213013255128, 0.6562505879594253688, 0.6588534356078361576, 0.6614588057527972520, 0.6640621373053481324, 0.6666665426327121891, 0.6692709473847417989, 0.6718742796537453543, 0.6744796497151083203, 0.6770824977620315543, 0.6796880648321572682, 0.6822910757211636534, 0.6848960564092084757, 0.6874998579679674204, 0.6901036599873985322, 0.6927086405316660311, 0.6953116518772185506, 0.6979172191805607106, 0.7005200675111846742, 0.7031254381841663958, 0.7057287706196612165, 0.7083331763606625087, 0.7109375820149322900, 0.7135409147210758363, 0.7161462855664346705, 0.7187491342530435423, 0.7213547019891674017, 0.7239577137555243125, 0.7265626949938263079, 0.7291664975571658935, 0.7317703000514055311, 0.7343752815188082650, 0.7369782934702413524, 0.7395838615780243597, 0.7421867107529701579, 0.7447920821133793279, 0.7473954155934371402, 0.7499998219085300954, 0.7526042286255122393, 0.7552075619304030596, 0.7578129337191791270, 0.7604157832075884027, 0.7630213517689198310, 0.7656243645745874904, 0.7682293465229839136, 0.7708331502520449074, 0.7734369533822141873, 0.7760419359326080624, 0.7786449486518774998, 0.7812505177233250997, 0.7838533679047272607, 0.7864587401119955690, 0.7890620747982641792, 0.7916664818479275390, 0.7942708897881238794, 0.7968742238533942368, 0.7994795967450375462, 0.8020824471973901915, 0.8046880167431663677, 0.8072910307501349747, 0.8098960135684915018, 0.8124998186244467568, 0.8151036225516941069, 0.8177086063449673370, 0.8203116199940584385, 0.8229171901884252405, 0.8255200415384508217, 0.8281254147520410447, 0.8307287508062024539, 0.8333331587509454907, 0.8359375680748931670, 0.8385409030622068549, 0.8411462772162020540, 0.8437491287946751184, 0.8463546994841673055, 0.8489577148544642515, 0.8515626987026798655, 0.8541665052467400931, 0.8567703101322480252, 0.8593752953283267937, 0.8619783100692604005, 0.8645838815458386506, 0.8671867342266933454, 0.8697921086061042306, 0.8723954461898817403, 0.8749998551902504751, 0.8776042660585271493, 0.8802076021295854868, 0.8828129777054576355, 0.8854158305722678035, 0.8880214025647872322, 0.8906244194604823194, 0.8932294044984951942, 0.8958332126919159588, 0.8984370186969063976, 0.9010420054557602976, 0.9036450214505988843, 0.9062505943687239052, 0.9088534485426573717, 0.9114588242474312985, 0.9140621635225948394, 0.9166665737391771485, 0.9192709863124074454, 0.9218743236289563825, 0.9244797007862803895, 0.9270825551036790957, 0.9296881285585824051, 0.9322911471418501295, 0.9348961335295734587, 0.9374999435335269471, 0.9401037508197458425, 0.9427087393012421046, 0.9453117567106092967, 0.9479173312323898593, 0.9505201870615167525, 0.9531255642405720430, 0.9557289053967781278, 0.9583333169903581750, 0.9609377312744702415, 0.9635410702737328137, 0.9661464495301401723, 0.9687493035862174695, 0.9713548794777306927, 0.9739579066090123804, 0.9765628826531806972, 0.9791666865793459129, 0.9817705523293528413, 0.9843754818126480011, 0.9869784094881522973, 0.9895843956701340094, 0.9921866610829068733, 0.9947911313000845634, 0.9973997837621362272, 1.000000000000000000 ),
 .UNSPECIFIED. ) ;
#166477 = CARTESIAN_POINT ( 'NONE',  ( 1.364683531249990311, 4.946875000341417916, 1.214306433183764966E-14 ) ) ;
#166478 = CARTESIAN_POINT ( 'NONE',  ( 0.4746845637013074604, -1.383529810647101455, 1.320479256824915071 ) ) ;
#166479 = CARTESIAN_POINT ( 'NONE',  ( 4.556949027968946631, 8.330541276023501140, -0.7216878364870357165 ) ) ;
#166480 = CARTESIAN_POINT ( 'NONE',  ( 1.363640982571033611, -0.4799814350611387725, 1.902108589862220311 ) ) ;
#166481 = FACE_OUTER_BOUND ( 'NONE', #208545, .T. ) ;
#166482 = EDGE_CURVE ( 'NONE', #14542, #188147, #17117, .T. ) ;
#166483 = CARTESIAN_POINT ( 'NONE',  ( -5.123001941117347080, 7.070197912760590064, 1.599625672291263179 ) ) ;
#166484 = CARTESIAN_POINT ( 'NONE',  ( 5.133110336712339183, 1.960249873928998410, 0.8093987030339530042 ) ) ;
#166486 = FILL_AREA_STYLE_COLOUR ( '', #25955 ) ;
#166485 = CARTESIAN_POINT ( 'NONE',  ( 8.289920859751990889, 11.75899253876431416, 1.199719254218450271 ) ) ;
#166487 = CARTESIAN_POINT ( 'NONE',  ( 6.626250064558294461, 1.136881752820615432, -1.610320780329032253 ) ) ;
#166488 = CARTESIAN_POINT ( 'NONE',  ( 1.364683531249988535, 1.863541667008086211, 0.7879004041258500513 ) ) ;
#166489 = CARTESIAN_POINT ( 'NONE',  ( 2.285404485177256362, 0.09469097253389560653, -2.011075120970148511 ) ) ;
#166491 = CARTESIAN_POINT ( 'NONE',  ( 1.159931391799984279, 1.264437666799199889, 1.698043086552150749 ) ) ;
#166490 = CARTESIAN_POINT ( 'NONE',  ( -6.019457014787517046, 9.006155036351978893, 1.082531754730548412 ) ) ;
#166492 = CARTESIAN_POINT ( 'NONE',  ( 11.96807573623599552, 6.670661610224271953, 1.000409426482763875 ) ) ;
#166493 = CARTESIAN_POINT ( 'NONE',  ( 2.154816067267216084, -0.5500195584662926906, -1.995915215819036748 ) ) ;
#166494 = CARTESIAN_POINT ( 'NONE',  ( 5.727393547130178675, 5.646656991265468939, 0.000000000000000000 ) ) ;
#166495 = CARTESIAN_POINT ( 'NONE',  ( 4.441177836928239309, 7.339068688795062911, 1.199719254218452047 ) ) ;
#166496 = VERTEX_POINT ( 'NONE', #6121 ) ;
#166498 = CARTESIAN_POINT ( 'NONE',  ( 3.344057444064992168, 7.053150784717805877, 1.040834085586084257E-14 ) ) ;
#166497 = CARTESIAN_POINT ( 'NONE',  ( 5.437476023981094642, 0.8479630442611612029, -1.911130889300112878 ) ) ;
#166501 = EDGE_LOOP ( 'NONE', ( #6833, #179317, #111766, #30788 ) ) ;
#166500 = CARTESIAN_POINT ( 'NONE',  ( 2.877393275988342047, 0.2635569349610377143, -1.792047384982973890 ) ) ;
#166499 = CARTESIAN_POINT ( 'NONE',  ( 3.996943106591983597, 1.542326501817241180, -0.9764022233923685956 ) ) ;
#166502 = CARTESIAN_POINT ( 'NONE',  ( 9.915090410295563927, 10.46202698829998567, -0.7998128361456281477 ) ) ;
#166503 = CARTESIAN_POINT ( 'NONE',  ( 9.553970131394970977, 11.68474399595152136, -6.135158682309066691 ) ) ;
#166504 = AXIS2_PLACEMENT_3D ( 'NONE', #150167, #1735, #68872 ) ;
#166505 = CARTESIAN_POINT ( 'NONE',  ( 5.526482418920476647, 1.318621124876094397, -1.769340128416618363 ) ) ;
#166506 = CARTESIAN_POINT ( 'NONE',  ( 0.6823417656249969321, 9.088541667008065872, -1.181850606188757036 ) ) ;
#166507 = EDGE_CURVE ( 'NONE', #58157, #119756, #104733, .T. ) ;
#166508 = ORIENTED_EDGE ( 'NONE', *, *, #4338, .F. ) ;
#166509 = CARTESIAN_POINT ( 'NONE',  ( 4.406835678522929456, -0.4222698756407486931, -1.864907683101609370 ) ) ;
#166510 = CARTESIAN_POINT ( 'NONE',  ( -3.948449050077848632, 5.629609863222681199, 1.599625672291267398 ) ) ;
#166511 = CARTESIAN_POINT ( 'NONE',  ( 6.259060471003163428, 10.45398764947904624, -0.7998128361456291469 ) ) ;
#166512 = CARTESIAN_POINT ( 'NONE',  ( 0.6801582343750056658, 0.5885416670080856338, -1.178068619123862515 ) ) ;
#166513 = CARTESIAN_POINT ( 'NONE',  ( 5.314433026432511475, 5.302519407033794430, 1.040834085586084257E-14 ) ) ;
#166514 = CARTESIAN_POINT ( 'NONE',  ( 1.814759087649938429, 3.975067388631681187, 0.4606438099578180068 ) ) ;
#166515 = CARTESIAN_POINT ( 'NONE',  ( 8.810048391696781778, 13.28851571758703720, -8.147727092588498365 ) ) ;
#166516 = CARTESIAN_POINT ( 'NONE',  ( 0.02850758872123548837, -1.683968158181762043, 0.7450552726024004535 ) ) ;
#166517 = ORIENTED_EDGE ( 'NONE', *, *, #1511, .T. ) ;
#166518 = AXIS2_PLACEMENT_3D ( 'NONE', #17301, #183018, #67108 ) ;
#166519 = CARTESIAN_POINT ( 'NONE',  ( -1.737499999999997824, -2.041666666666667407, 3.009438278150925683 ) ) ;
#166520 = CARTESIAN_POINT ( 'NONE',  ( 3.620239363633662055, 1.188986022374241225, -1.444006105232334969 ) ) ;
#166521 = CARTESIAN_POINT ( 'NONE',  ( 6.912678218121202534, 9.158153569265168770, 1.599625672291268286 ) ) ;
#166522 = CARTESIAN_POINT ( 'NONE',  ( -1.499999999999995559, 8.673756432004008587, -2.614717076620594050 ) ) ;
#166523 = CARTESIAN_POINT ( 'NONE',  ( -6.073689629242151611, 10.02979563418376685, -0.7216878364870278340 ) ) ;
#166524 = CARTESIAN_POINT ( 'NONE',  ( 4.527533231959700366, 7.369540306339926516, 1.199719254218462483 ) ) ;
#166525 = CARTESIAN_POINT ( 'NONE',  ( 0.6726246190636753219, 1.362232206854155914, -1.422558973980556418 ) ) ;
#166526 = CARTESIAN_POINT ( 'NONE',  ( 1.757435634535610136, 1.928746520693159550, -0.5880414618760835266 ) ) ;
#166527 = CARTESIAN_POINT ( 'NONE',  ( -7.971304249830880373, 11.38727316052296601, 1.199719254218453823 ) ) ;
#166528 = CARTESIAN_POINT ( 'NONE',  ( 6.866278450678116485, 6.975356045404744521, 0.000000000000000000 ) ) ;
#166530 = EDGE_CURVE ( 'NONE', #172216, #105059, #197068, .T. ) ;
#166529 = CARTESIAN_POINT ( 'NONE',  ( -15.75000000000000000, 12.30000000000000071, 0.6999999999999992895 ) ) ;
#166531 = CARTESIAN_POINT ( 'NONE',  ( 2.906388222866810978, 1.586772471669075424, -1.511725739355776366 ) ) ;
#166532 = CARTESIAN_POINT ( 'NONE',  ( 6.199803715563785289, -0.6102442156579388488, 1.720816905678754560 ) ) ;
#166533 = CARTESIAN_POINT ( 'NONE',  ( -4.973143418114339021, 4.696422164088486895, 0.7998128361456341429 ) ) ;
#166534 = LINE ( 'NONE', #66856, #202309 ) ;
#166535 = EDGE_CURVE ( 'NONE', #21552, #104455, #24046, .T. ) ;
#166536 = CARTESIAN_POINT ( 'NONE',  ( 3.580761967785000888, 7.191656372475549119, -0.7216878364870338292 ) ) ;
#166537 = CARTESIAN_POINT ( 'NONE',  ( 8.666686507633574621, 11.13422023037111330, 1.599625672291281386 ) ) ;
#166538 = CARTESIAN_POINT ( 'NONE',  ( 2.517010073631369860, 6.088262185878572375, -0.7998128361456281477 ) ) ;
#166539 = CARTESIAN_POINT ( 'NONE',  ( 6.861835142292147083, 7.178098218861903135, 0.7216878364870328300 ) ) ;
#166540 = VERTEX_POINT ( 'NONE', #176135 ) ;
#166542 = CARTESIAN_POINT ( 'NONE',  ( 0.4869769290230832048, -1.896302947978160791, -0.6760925243112311245 ) ) ;
#166541 = CARTESIAN_POINT ( 'NONE',  ( 4.177188522404684079, 1.205947341878073287, 1.391433828303423326 ) ) ;
#166543 = CARTESIAN_POINT ( 'NONE',  ( 3.515276618313140311, 2.298542322452525877, 0.003563541299675049897 ) ) ;
#166545 = CARTESIAN_POINT ( 'NONE',  ( 0.7251815698985024650, 0.1899481183357653036, -1.851258252060000498 ) ) ;
#166544 = LINE ( 'NONE', #179602, #171609 ) ;
#166546 = CARTESIAN_POINT ( 'NONE',  ( -1.737500000000000266, -0.4083333333333334370, -3.009438278150923907 ) ) ;
#166547 = CARTESIAN_POINT ( 'NONE',  ( -4.874319919312905647, 5.645460313075203018, -1.199719254218446718 ) ) ;
#166548 = CARTESIAN_POINT ( 'NONE',  ( -9.585712968046856020, 14.76505204444259256, -7.219336745274212319 ) ) ;
#166549 = CARTESIAN_POINT ( 'NONE',  ( 4.816621285000030284, -0.6497861859515661198, -1.798733151862880186 ) ) ;
#166550 = B_SPLINE_CURVE_WITH_KNOTS ( 'NONE', 3,
 ( #157360, #189837, #21969, #8952, #105420, #54510, #42557, #207153, #203929, #57713, #186633, #23047 ),
 .UNSPECIFIED., .F., .F.,
 ( 4, 2, 2, 2, 2, 4 ),
 ( 0.001599105520544900991, 0.002495321489371081849, 0.002943429473784172495, 0.003391537458197263141, 0.004287753427023444433, 0.005183969395849624857 ),
 .UNSPECIFIED. ) ;
#166551 = CARTESIAN_POINT ( 'NONE',  ( -9.020252271793614440, 9.418049160047695878, 0.7998128361456462443 ) ) ;
#166552 = CARTESIAN_POINT ( 'NONE',  ( 6.053075614097062740, 7.042710966267798689, -1.019147762646470001 ) ) ;
#166553 = CARTESIAN_POINT ( 'NONE',  ( -5.641601317062233001, 9.595968946632336127, -0.7216878364870338292 ) ) ;
#166555 = CARTESIAN_POINT ( 'NONE',  ( 2.008475284031425723, 1.387998011844304491, -1.254312187223500796 ) ) ;
#166554 = CARTESIAN_POINT ( 'NONE',  ( 3.509396081178951743, -2.059435208860632915, 0.3595599189689518416 ) ) ;
#166556 = CARTESIAN_POINT ( 'NONE',  ( 7.673551755654734130, 9.015193805427763607, -1.082531754730537976 ) ) ;
#166557 = CARTESIAN_POINT ( 'NONE',  ( 0.6823417656249899377, 5.738541667008087543, -1.181850606188754593 ) ) ;
#166558 = CARTESIAN_POINT ( 'NONE',  ( 5.442854017605395889, -1.455216020186438364, -1.127989967910733915 ) ) ;
#166559 = CARTESIAN_POINT ( 'NONE',  ( 4.207107738942202246, 3.802713871720993399, 1.214306433183764966E-14 ) ) ;
#166561 = CARTESIAN_POINT ( 'NONE',  ( 4.168242161197552420, 6.950367390450747251, -1.199719254218452047 ) ) ;
#166560 = CARTESIAN_POINT ( 'NONE',  ( 1.224999999999995204, 1.145833333333333259, -0.7072540797572898219 ) ) ;
#166562 = CARTESIAN_POINT ( 'NONE',  ( 3.510098308409233869, -0.7004517935718050925, -1.576443202522736842 ) ) ;
#166563 = CARTESIAN_POINT ( 'NONE',  ( -8.037286134802835491, 8.271255333558444889, -0.7998128361456291469 ) ) ;
#166564 = CARTESIAN_POINT ( 'NONE',  ( 6.270183524512255246, 1.130759168108757873, 1.895055401287759178 ) ) ;
#166565 = CARTESIAN_POINT ( 'NONE',  ( 6.983263157960366563, 7.629137130509066722, 2.653810918356712900 ) ) ;
#166566 = CIRCLE ( 'NONE', #145894, 2.025000000000006573 ) ;
#166567 = CARTESIAN_POINT ( 'NONE',  ( 3.486133158594716510E-16, 0.8750000006828204668, 1.224999999999968336 ) ) ;
#166568 = CARTESIAN_POINT ( 'NONE',  ( 5.295835511405859286, -1.530271966869084954, -1.540324818649402072 ) ) ;
#166569 = CARTESIAN_POINT ( 'NONE',  ( 2.859763506297557711, 1.816872213737670938, -0.1792109616642542924 ) ) ;
#166570 = CARTESIAN_POINT ( 'NONE',  ( 0.5319879461419263489, 1.124744735265088780, 1.607134405190835391 ) ) ;
#166571 = CARTESIAN_POINT ( 'NONE',  ( 5.190659055775300956, 1.601436234092843414, -1.385157061098884146 ) ) ;
#166572 = VECTOR ( 'NONE', #38117, 1000.000000000000000 ) ;
#166573 = EDGE_LOOP ( 'NONE', ( #111869, #41762, #7072, #8277, #65151, #5918, #172962, #22961, #151055, #26866, #153988, #19409, #74707, #186304, #28832, #153096, #1617, #114436, #138635, #44807 ) ) ;
#166575 = CARTESIAN_POINT ( 'NONE',  ( 0.6823417656249899377, 2.405208333674753618, 1.181850606188767472 ) ) ;
#166574 = CARTESIAN_POINT ( 'NONE',  ( 6.321853416579415352, 1.323700039822506280, -1.871417125626378075 ) ) ;
#166576 = CARTESIAN_POINT ( 'NONE',  ( 8.540746701604824409, 12.05162268759261224, -1.199719254218446718 ) ) ;
#166577 = CARTESIAN_POINT ( 'NONE',  ( 1.629697543846151619, -0.2563088357964183883, 2.104862515383609800 ) ) ;
#166578 = CARTESIAN_POINT ( 'NONE',  ( -3.470524135418294520, 6.992769224722559684, -0.7216878364870267237 ) ) ;
#166579 = CARTESIAN_POINT ( 'NONE',  ( -7.334597915313094241, 9.580116872663850813, 1.040834085586084257E-14 ) ) ;
#166580 = CARTESIAN_POINT ( 'NONE',  ( -4.514501963226242864, 7.250374142863800664, 1.082531754730560403 ) ) ;
#166581 = CARTESIAN_POINT ( 'NONE',  ( 6.666846200133992539, 1.614693783697606522, -1.451540455714307010 ) ) ;
#166583 = CARTESIAN_POINT ( 'NONE',  ( -6.009258394948636914E-15, 12.96875000068280137, -1.732050807568875195 ) ) ;
#166582 = CARTESIAN_POINT ( 'NONE',  ( 0.09999999999999592548, -9.999999999999994671, 10.91954211494236660 ) ) ;
#166585 = ORIENTED_EDGE ( 'NONE', *, *, #1086, .T. ) ;
#166584 = CARTESIAN_POINT ( 'NONE',  ( 1.700152687198818402, 1.534743396142525640, 1.606060300191413548 ) ) ;
#166586 = CARTESIAN_POINT ( 'NONE',  ( 0.05395445667428447334, -1.494411465983748855, 1.746745294031383455 ) ) ;
#166588 = CARTESIAN_POINT ( 'NONE',  ( 4.680570805348211572, 1.272886101012826288, -1.622837931747274975 ) ) ;
#166587 = CARTESIAN_POINT ( 'NONE',  ( 5.034155109375821446, 4.767602470560229122, -0.7998128361456221525 ) ) ;
#166590 = CARTESIAN_POINT ( 'NONE',  ( -5.275531169048909952, 7.248148678680751189, -1.443375672974066770 ) ) ;
#166589 = CARTESIAN_POINT ( 'NONE',  ( 6.505933609711257226, 8.683618192786854095, -1.599625672291281386 ) ) ;
#166591 = CARTESIAN_POINT ( 'NONE',  ( 5.515134625708930649, 9.656350506627580543, 0.000000000000000000 ) ) ;
#166592 = CARTESIAN_POINT ( 'NONE',  ( -3.285556943750000070, -4.046874999522040106, 0.000000000000000000 ) ) ;
#166593 = CARTESIAN_POINT ( 'NONE',  ( 0.6170404364503319083, 3.500000000000003109, -1.902435570468858250 ) ) ;
#166594 = CARTESIAN_POINT ( 'NONE',  ( 0.9727375897880451427, -0.05299885879509737968, -2.090136731789421276 ) ) ;
#166595 = CARTESIAN_POINT ( 'NONE',  ( 4.149064681782777875, 0.9530105817698063531, 1.777011888912001014 ) ) ;
#166596 = CARTESIAN_POINT ( 'NONE',  ( 4.616662711240536510, -0.08544939198026380023, 1.839383977539174264 ) ) ;
#166597 = CARTESIAN_POINT ( 'NONE',  ( 5.542585869888291938, 5.360771691158120689, -0.7998128361456211532 ) ) ;
#166598 =( NAMED_UNIT ( * ) PLANE_ANGLE_UNIT ( ) SI_UNIT ( $, .RADIAN. ) );
#166599 = CARTESIAN_POINT ( 'NONE',  ( 2.063112832053456636, 0.2986308487272717471, -1.698545238003341673 ) ) ;
#166600 = CARTESIAN_POINT ( 'NONE',  ( 3.449547071718272573, -1.000000000000000888, -2.024999999999992806 ) ) ;
#166601 = CARTESIAN_POINT ( 'NONE',  ( 0.7920821852162404086, 1.736045259359697335, -1.506783991232300446 ) ) ;
#166602 = CARTESIAN_POINT ( 'NONE',  ( -4.900382456335551140, 7.804531068111707270, 1.199719254218464037 ) ) ;
#166603 = CARTESIAN_POINT ( 'NONE',  ( 1.001694622806301060, 1.849986872810194694, 1.302049432249830607 ) ) ;
#166604 = CARTESIAN_POINT ( 'NONE',  ( 2.508543264270487683, -0.8067718606631252287, -1.945620686511064790 ) ) ;
#166605 = CARTESIAN_POINT ( 'NONE',  ( -3.786470039966538970, 7.639575156594750283, 0.000000000000000000 ) ) ;
#166606 = CARTESIAN_POINT ( 'NONE',  ( 5.449487677688982679, 8.445153826357429949, -1.199719254218446718 ) ) ;
#166608 = EDGE_CURVE ( 'NONE', #55444, #77820, #121775, .T. ) ;
#166607 = CARTESIAN_POINT ( 'NONE',  ( 4.706088717274895750, 6.583799151611112954, 1.443375672974065660 ) ) ;
#166609 = CARTESIAN_POINT ( 'NONE',  ( 6.343749999995762501, 1.895863743059895246, 0.7852924748296488122 ) ) ;
#166610 = CARTESIAN_POINT ( 'NONE',  ( -5.575427483717760424, 7.527751369135936343, 1.599625672291269396 ) ) ;
#166611 = CARTESIAN_POINT ( 'NONE',  ( 1.499999999999987121, 1.545833333333354487, -0.8660254037844253849 ) ) ;
#166612 = CARTESIAN_POINT ( 'NONE',  ( -2.774614992291035698, 6.388801257648172971, 1.040834085586084257E-14 ) ) ;
#166613 = CARTESIAN_POINT ( 'NONE',  ( 4.799211390369230834, -0.2731021391014861188, -2.204526388291703221 ) ) ;
#166614 = CARTESIAN_POINT ( 'NONE',  ( 3.961010909407123304, 0.2689195440248594027, -2.174814543647784593 ) ) ;
#166615 = CARTESIAN_POINT ( 'NONE',  ( -5.412729640353771465, 7.337937218544611895, 1.599625672291269396 ) ) ;
#166616 = CARTESIAN_POINT ( 'NONE',  ( -0.6823417656249969321, 3.717708333674754506, -1.181850606188749264 ) ) ;
#166617 = EDGE_CURVE ( 'NONE', #196589, #141559, #204714, .T. ) ;
#166618 = CARTESIAN_POINT ( 'NONE',  ( -5.260200412422213923, 6.199617238323108737, -1.082531754730544860 ) ) ;
#166619 = CARTESIAN_POINT ( 'NONE',  ( 6.152600690169603759, 2.097733681304454034, 0.3095894981632040244 ) ) ;
#166620 = CARTESIAN_POINT ( 'NONE',  ( -5.777182853198894463, 9.754147405458438058, 0.7216878364870267237 ) ) ;
#166621 = ORIENTED_EDGE ( 'NONE', *, *, #147028, .T. ) ;
#166623 = CARTESIAN_POINT ( 'NONE',  ( 6.455963997168007396, 2.156291961557708525, -0.1537611777119098910 ) ) ;
#166622 = CARTESIAN_POINT ( 'NONE',  ( -5.099275172515603138, 8.002885897026576600, 1.082531754730549967 ) ) ;
#166624 = CARTESIAN_POINT ( 'NONE',  ( 6.505214776458575265, 6.483838748823460563, 1.040834085586084257E-14 ) ) ;
#166625 = CARTESIAN_POINT ( 'NONE',  ( 6.269096963164666469, 1.759884223096353173, -0.5412972069449849544 ) ) ;
#166626 = CARTESIAN_POINT ( 'NONE',  ( 0.6823417656249899377, 2.405208333674753618, 1.181850606188767472 ) ) ;
#166627 = CARTESIAN_POINT ( 'NONE',  ( 1.364397727108757730, 0.1285707514647760064, -1.735724436397204196 ) ) ;
#166628 = CARTESIAN_POINT ( 'NONE',  ( 3.277320446201373638, 4.846626492033466072, 1.599625672291267398 ) ) ;
#166629 = DIRECTION ( 'NONE',  ( 0.000000000000000000, 1.000000000000000000, 0.000000000000000000 ) ) ;
#166630 = CARTESIAN_POINT ( 'NONE',  ( -1.364683531250014514, -0.1989583329919157317, -0.7879004041258359514 ) ) ;
#166631 = LINE ( 'NONE', #187139, #125738 ) ;
#166632 = CARTESIAN_POINT ( 'NONE',  ( 5.682550338946039226, -2.108058120380253087, -0.4779004524640489970 ) ) ;
#166633 = CARTESIAN_POINT ( 'NONE',  ( -3.755772246185468788, 4.340488027759846545, -1.199719254218452047 ) ) ;
#166634 = AXIS2_PLACEMENT_3D ( 'NONE', #7940, #203988, #56711 ) ;
#166635 = CARTESIAN_POINT ( 'NONE',  ( -6.195713011320790109, 9.211787032307496403, -1.082531754730537976 ) ) ;
#166636 = B_SPLINE_CURVE_WITH_KNOTS ( 'NONE', 3,
 ( #74810, #144120, #160321, #110572, #189614, #43389 ),
 .UNSPECIFIED., .F., .F.,
 ( 4, 2, 4 ),
 ( 0.000000000000000000, 0.0003845013059668469482, 0.0007690026119336938965 ),
 .UNSPECIFIED. ) ;
#166637 = CARTESIAN_POINT ( 'NONE',  ( 4.997027575558514734, 1.799266821141291661, -1.197868618907194316 ) ) ;
#166638 = CARTESIAN_POINT ( 'NONE',  ( -0.6823417656250212460, 3.051041667008084879, 1.181850606188767472 ) ) ;
#166640 = CARTESIAN_POINT ( 'NONE',  ( 6.169206948603202179, 0.1476589778573663692, -1.965905794126821426 ) ) ;
#166639 = B_SPLINE_CURVE_WITH_KNOTS ( 'NONE', 3,
 ( #49977, #135504, #16385, #36912, #2255, #169052, #185289, #200467, #102995, #118241 ),
 .UNSPECIFIED., .F., .F.,
 ( 4, 3, 3, 4 ),
 ( 4.670885906470136028E-18, 3.125212466446787460E-05, 6.250460353101360055E-05, 0.0001200463674512635038 ),
 .UNSPECIFIED. ) ;
#166641 = CARTESIAN_POINT ( 'NONE',  ( 4.815645707022956579, -1.391897370064384631, 1.033600972745553070 ) ) ;
#166643 = CARTESIAN_POINT ( 'NONE',  ( 1.962683346935737205, -2.005255389829229351, -0.8846387633431598285 ) ) ;
#166642 = CARTESIAN_POINT ( 'NONE',  ( -10.59752019245792987, 11.30000000000000071, -3.303678142506601745 ) ) ;
#166644 = CARTESIAN_POINT ( 'NONE',  ( 1.765117381242779615, -1.630797578202509701, 1.632866094832433834 ) ) ;
#166645 = CARTESIAN_POINT ( 'NONE',  ( 4.710263567924342532, -0.8773996900517248010, -1.864791387430650094 ) ) ;
#166646 = CARTESIAN_POINT ( 'NONE',  ( 0.3923911919363164413, 1.615042221312415371, -1.078049841609552306 ) ) ;
#166647 = CARTESIAN_POINT ( 'NONE',  ( -6.846504384776758378, 9.010674420371453053, -1.443375672974058777 ) ) ;
#166648 = CARTESIAN_POINT ( 'NONE',  ( -4.625266680917477835, 5.425174544939014964, -1.199719254218453823 ) ) ;
#166649 = CARTESIAN_POINT ( 'NONE',  ( -5.605292224350291619, 5.702808290780939871, -0.2219334806705375862 ) ) ;
#166650 = CARTESIAN_POINT ( 'NONE',  ( 3.340189922722580196, -1.266226476691566738, -1.700888996046201029 ) ) ;
#166651 = CARTESIAN_POINT ( 'NONE',  ( 5.014534001275664288, 7.922250005646839455, -1.103081721458569309 ) ) ;
#166652 = CARTESIAN_POINT ( 'NONE',  ( 1.318982659667154334, 0.9913977828604101372, -1.755770081111128977 ) ) ;
#166653 = CARTESIAN_POINT ( 'NONE',  ( -7.226132685959434809, 8.493204890783200511, 1.082531754730549967 ) ) ;
#166654 = EDGE_CURVE ( 'NONE', #12149, #55162, #125181, .T. ) ;
#166655 = CARTESIAN_POINT ( 'NONE',  ( 4.190592561755676293, -2.182319254149690302, -0.3268587364041104504 ) ) ;
#166656 = CARTESIAN_POINT ( 'NONE',  ( 1.642778471875001811, -1.830208332855375097, 2.845375778867859751 ) ) ;
#166657 = CARTESIAN_POINT ( 'NONE',  ( 1.428301029171385794, -1.185968821734217027, 1.434052760600286858 ) ) ;
#166658 = CARTESIAN_POINT ( 'NONE',  ( -0.1288028175206907822, 7.629137130509059617, -2.873994896247424435 ) ) ;
#166659 = LINE ( 'NONE', #1986, #173559 ) ;
#166660 = CARTESIAN_POINT ( 'NONE',  ( 3.591464764177854541, 3.560402065510233083, -2.500000000000000444 ) ) ;
#166662 = CYLINDRICAL_SURFACE ( 'NONE', #192911, 1.224999999999996980 ) ;
#166661 = CARTESIAN_POINT ( 'NONE',  ( -4.585403371929053229, 8.498043419817562949, 0.04945426522169442396 ) ) ;
#166663 = CARTESIAN_POINT ( 'NONE',  ( 0.6124999999999914957, 2.083333333333339699, 1.060881119635884051 ) ) ;
#166664 = ORIENTED_EDGE ( 'NONE', *, *, #29015, .T. ) ;
#166665 = CARTESIAN_POINT ( 'NONE',  ( 3.784101207196560068, -1.017168810052709205, 1.792309825713923166 ) ) ;
#166666 = CARTESIAN_POINT ( 'NONE',  ( 1.360316468749963592, 1.244791667008120051, 0.7853790794158760358 ) ) ;
#166667 = CARTESIAN_POINT ( 'NONE',  ( -6.555530967407501741, 7.606873202518897870, 1.199719254218450271 ) ) ;
#166668 = CARTESIAN_POINT ( 'NONE',  ( 1.840495965525708932, 1.161060486998789942, -1.652382956570614736 ) ) ;
#166669 = CARTESIAN_POINT ( 'NONE',  ( -1.402160292154681736E-14, -0.1624999999999815481, -1.732050807568870754 ) ) ;
#166670 = CARTESIAN_POINT ( 'NONE',  ( 2.496672843210871129, 6.064535417054653266, -0.7998128361456291469 ) ) ;
#166671 = AXIS2_PLACEMENT_3D ( 'NONE', #98251, #117754, #81980 ) ;
#166672 = CARTESIAN_POINT ( 'NONE',  ( 1.551711473626409266, 0.5993144932881481202, -1.971807626030545268 ) ) ;
#166674 = CARTESIAN_POINT ( 'NONE',  ( -8.012344526598182026E-15, 13.54687500034139269, -1.575800808251669460 ) ) ;
#166673 = CARTESIAN_POINT ( 'NONE',  ( -9.367496997601184816, 15.42330868760440410, -7.413898975931886959 ) ) ;
#166675 = CARTESIAN_POINT ( 'NONE',  ( 6.114890974963323345, 7.092793211334054604, 1.199719254218462483 ) ) ;
#166676 = CARTESIAN_POINT ( 'NONE',  ( -0.2408018239684278916, 6.947782644136219155, -2.695524888730389090 ) ) ;
#166677 = CARTESIAN_POINT ( 'NONE',  ( 1.042614295247261680, -1.450156864641814369, -1.134287774663629733 ) ) ;
#166678 = CARTESIAN_POINT ( 'NONE',  ( 5.707716145626243964, -0.5396369327701348029, 2.139774205771049154 ) ) ;
#166679 = CARTESIAN_POINT ( 'NONE',  ( 6.333594036239346359, 7.418223126147930557, 1.199719254218453823 ) ) ;
#166680 = CARTESIAN_POINT ( 'NONE',  ( 1.300320450452172594, -2.161773191439372965, -0.001381507821696103871 ) ) ;
#166681 = CARTESIAN_POINT ( 'NONE',  ( -4.121315508874262790, 6.791656612786516334, -1.082531754730549967 ) ) ;
#166682 = CARTESIAN_POINT ( 'NONE',  ( 2.026577684455236561, 0.4465047249504557891, 1.966304233017155845 ) ) ;
#166683 = EDGE_CURVE ( 'NONE', #106354, #15498, #190783, .T. ) ;
#166684 = CARTESIAN_POINT ( 'NONE',  ( 0.6373110600932235803, -1.319858442276698129, -1.325903642019378381 ) ) ;
#166685 =( NAMED_UNIT ( * ) SI_UNIT ( $, .STERADIAN. ) SOLID_ANGLE_UNIT ( ) );
#166686 = CARTESIAN_POINT ( 'NONE',  ( 4.223478185285460818, -1.886956702611849002, 0.5710618836329334203 ) ) ;
#166687 = CARTESIAN_POINT ( 'NONE',  ( 3.327361509216096191, -1.530157842762596143, -1.313544516083162028 ) ) ;
#166689 = CARTESIAN_POINT ( 'NONE',  ( 8.717529583462638954, 12.15390636647303069, 1.082531754730546636 ) ) ;
#166688 = CARTESIAN_POINT ( 'NONE',  ( -0.6823417656250003738, 1.717708333674752730, -1.181850606188749264 ) ) ;
#166691 = CARTESIAN_POINT ( 'NONE',  ( 6.322895070704796616, 1.964426112044151518, 0.7597984924697271936 ) ) ;
#166690 = CARTESIAN_POINT ( 'NONE',  ( -6.367525699912501835, 10.58053041653993098, -0.7998128361456291469 ) ) ;
#166692 = CARTESIAN_POINT ( 'NONE',  ( 5.600075274486990828, 0.8424382930321882013, -1.891409743246947217 ) ) ;
#166693 = CARTESIAN_POINT ( 'NONE',  ( 5.621827251160867789, 9.710548892996357040, 1.040834085586084257E-14 ) ) ;
#166694 = CARTESIAN_POINT ( 'NONE',  ( -8.389798128758148010, 8.682519326506312751, 0.7998128361456462443 ) ) ;
#166695 = CARTESIAN_POINT ( 'NONE',  ( -1.467638673046511189, 8.739153922842808342, 2.544768421592544794 ) ) ;
#166696 = CARTESIAN_POINT ( 'NONE',  ( 4.693620712453854260, 1.883065523094022753, -0.7309246526977104530 ) ) ;
#166697 = CARTESIAN_POINT ( 'NONE',  ( 0.7499999999999885647, -0.9854166659838472508, 1.299038105676657340 ) ) ;
#166698 = CARTESIAN_POINT ( 'NONE',  ( 1.358340336993546726, -2.062741126468564890, -0.004002619933256982773 ) ) ;
#166699 = CARTESIAN_POINT ( 'NONE',  ( 7.727784370109387346, 10.99920361756089093, -1.082531754730543083 ) ) ;
#166700 = ADVANCED_FACE ( 'NONE', ( #125320 ), #114792, .T. ) ;
#166701 = CARTESIAN_POINT ( 'NONE',  ( 6.475954649182838807, 7.584310507915338562, 1.199719254218452047 ) ) ;
#166702 = CARTESIAN_POINT ( 'NONE',  ( 5.387385936583818591, 7.378645907471495846, -1.599625672291283607 ) ) ;
#166703 = CARTESIAN_POINT ( 'NONE',  ( 0.6823417656249899377, 1.155208333674752286, 1.181850606188755259 ) ) ;
#166705 =( NAMED_UNIT ( * ) PLANE_ANGLE_UNIT ( ) SI_UNIT ( $, .RADIAN. ) );
#166704 = CARTESIAN_POINT ( 'NONE',  ( 6.229045230835819069, 6.231917288922055320, -0.7998128361456481317 ) ) ;
#166706 = CARTESIAN_POINT ( 'NONE',  ( 6.277061933002777927, 8.346324893301817482, 1.443375672974076540 ) ) ;
#166708 = DIRECTION ( 'NONE',  ( 0.2079116908177593703, 0.000000000000000000, -0.9781476007338056888 ) ) ;
#166707 = CARTESIAN_POINT ( 'NONE',  ( 2.647136220323087485, -0.3691774202370365354, -2.139407045683580755 ) ) ;
#166709 = CARTESIAN_POINT ( 'NONE',  ( 6.608665842073913055, 1.606649649811153768, -1.446306907624186344 ) ) ;
#166711 = CARTESIAN_POINT ( 'NONE',  ( 2.876309626556411203, -0.1380247437976732383, -1.836149222064882514 ) ) ;
#166710 = CARTESIAN_POINT ( 'NONE',  ( -4.772106882330241717, 5.630174786549132726, -1.082531754730544860 ) ) ;
#166712 = CARTESIAN_POINT ( 'NONE',  ( -0.6823417656249969321, 4.717708333674755394, -1.181850606188749264 ) ) ;
#166713 = CARTESIAN_POINT ( 'NONE',  ( 4.476244563333130699, -2.125884358948509689, -0.5320566845071761364 ) ) ;
#166714 = CARTESIAN_POINT ( 'NONE',  ( 8.627766630430368622, 13.75162864925633244, 8.275246034657209648 ) ) ;
#166715 = CARTESIAN_POINT ( 'NONE',  ( 4.733442339874294191, -2.070396585149585356, 0.9127746130930917134 ) ) ;
#166716 = CARTESIAN_POINT ( 'NONE',  ( -5.525111292768871252, 6.404716915440499037, -1.199719254218446718 ) ) ;
#166717 = CARTESIAN_POINT ( 'NONE',  ( -4.851289806644571989, 6.918820993438449030, -1.443092038473028582 ) ) ;
#166718 = CARTESIAN_POINT ( 'NONE',  ( 4.754190777897029818, 8.299541367957775861, -0.7767638722561143183 ) ) ;
#166719 = CARTESIAN_POINT ( 'NONE',  ( -5.519577934094894722, 7.532869904567736974, 1.443375672974058777 ) ) ;
#166720 = CARTESIAN_POINT ( 'NONE',  ( 4.828112100242277549, 6.726159765073026264, -1.443375672974068769 ) ) ;
#166721 = CARTESIAN_POINT ( 'NONE',  ( 0.1625042017948316320, -1.577765994087614310, -0.8020051908347087810 ) ) ;
#166722 = CIRCLE ( 'NONE', #201320, 0.08000000000000020983 ) ;
#166723 = CARTESIAN_POINT ( 'NONE',  ( 4.582685675920167512, -1.313125608480088635, 1.525959163679012187 ) ) ;
#166724 = CARTESIAN_POINT ( 'NONE',  ( 8.145751363712157911, 8.397798100619326078, -0.7998128361456281477 ) ) ;
#166725 = CARTESIAN_POINT ( 'NONE',  ( 2.837057662192625340, 0.2562861413469962879, 2.090225181913709207 ) ) ;
#166726 = CARTESIAN_POINT ( 'NONE',  ( 1.493601000189462624, -1.900943851588072997, 0.2360903481228252554 ) ) ;
#166727 = CIRCLE ( 'NONE', #24934, 11.09999999999999964 ) ;
#166729 = CARTESIAN_POINT ( 'NONE',  ( -1.500000000000013101, 2.129166666666693519, -0.8660254037844313801 ) ) ;
#166728 = CARTESIAN_POINT ( 'NONE',  ( -1.364683531250010295, 11.38020833367473728, 0.7879004041258445001 ) ) ;
#166730 = CARTESIAN_POINT ( 'NONE',  ( 2.154690271565715687, -0.5224902820043091367, -1.898924457017936662 ) ) ;
#166731 = CARTESIAN_POINT ( 'NONE',  ( 0.1275333129481092398, -1.147091320445620566, -1.478225367208672703 ) ) ;
#166732 = CARTESIAN_POINT ( 'NONE',  ( 0.8714495147512549833, -0.2914478312704605889, 1.939986204769503786 ) ) ;
#166734 = ORIENTED_EDGE ( 'NONE', *, *, #77763, .T. ) ;
#166733 = CARTESIAN_POINT ( 'NONE',  ( -0.03509584499547176162, -1.534781374734139670, 1.140672443274578729 ) ) ;
#166735 = CARTESIAN_POINT ( 'NONE',  ( 5.721177635286841756, 6.737423998331861341, -1.082531754730543083 ) ) ;
#166736 = CARTESIAN_POINT ( 'NONE',  ( 1.364683531249986537, 0.6760416670080884316, 0.7879004041258500513 ) ) ;
#166737 = CARTESIAN_POINT ( 'NONE',  ( 6.157094445334826638, -1.605393284960114242, -0.9600186418455139981 ) ) ;
#166738 = CARTESIAN_POINT ( 'NONE',  ( 0.9486429539237110076, 2.850839070649072049, 1.028101543438982413 ) ) ;
#166739 = CARTESIAN_POINT ( 'NONE',  ( 5.875854205266582753, -2.021069926245163906, 0.4479438709683660202 ) ) ;
#166740 = SURFACE_STYLE_FILL_AREA ( #99602 ) ;
#166741 = CARTESIAN_POINT ( 'NONE',  ( -4.706088717274938382, 6.583799151611112954, 1.443375672974058777 ) ) ;
#166742 = CARTESIAN_POINT ( 'NONE',  ( -0.02319159430949970652, 0.003959926571647092407, -1.810968101872318714 ) ) ;
#166743 = CARTESIAN_POINT ( 'NONE',  ( -1.402160292154681736E-14, 0.5875000000000220046, -1.732050807568863648 ) ) ;
#166744 = CARTESIAN_POINT ( 'NONE',  ( 7.461064606222022277, 7.598996883547496139, 1.040834085586084257E-14 ) ) ;
#166745 = CARTESIAN_POINT ( 'NONE',  ( -6.906989191158078079, 10.14557225873805812, -1.199719254218440723 ) ) ;
#166746 = CARTESIAN_POINT ( 'NONE',  ( 5.855142236255289845, 7.924361590421551860, -1.599625672291281386 ) ) ;
#166747 = CARTESIAN_POINT ( 'NONE',  ( 1.364683531249988535, 1.613541667008084879, 0.7879004041258500513 ) ) ;
#166748 = CARTESIAN_POINT ( 'NONE',  ( 1.499999999999987121, 3.045833333333353377, -0.8660254037844262731 ) ) ;
#166750 = CARTESIAN_POINT ( 'NONE',  ( 3.551346171775753735, 6.230655402791975384, 1.199719254218462483 ) ) ;
#166749 = CARTESIAN_POINT ( 'NONE',  ( 5.687936657224680559, -1.243353266631580523, -1.517579924814119074 ) ) ;
#166751 = CARTESIAN_POINT ( 'NONE',  ( 3.286482353612128371, -1.943773746517188039, 0.5350062169211176055 ) ) ;
#166752 = EDGE_CURVE ( 'NONE', #12663, #209328, #116949, .T. ) ;
#166753 = CARTESIAN_POINT ( 'NONE',  ( 3.045994482203842502, 0.8657459236516149570, 1.709044100283881429 ) ) ;
#166754 = CARTESIAN_POINT ( 'NONE',  ( 11.78331023100045627, 9.799999999999998934, -1.800000000000001155 ) ) ;
#166755 = CARTESIAN_POINT ( 'NONE',  ( 2.050558489324630251, -1.691691439650149897, 1.393213601605561180 ) ) ;
#166756 = CARTESIAN_POINT ( 'NONE',  ( 0.1331715793776913348, 0.7364730991098663582, -2.038600455735229300 ) ) ;
#166757 = CARTESIAN_POINT ( 'NONE',  ( 2.899504437521780442, -0.5904213222340527478, 1.774967144274109287 ) ) ;
#166758 = CARTESIAN_POINT ( 'NONE',  ( 0.7499999999999885647, -1.235416665983847473, 1.299038105676657340 ) ) ;
#166759 =( REPRESENTATION_RELATIONSHIP ('NONE','NONE', #84563, #188305 ) REPRESENTATION_RELATIONSHIP_WITH_TRANSFORMATION ( #43842 )SHAPE_REPRESENTATION_RELATIONSHIP( ) );
#166760 = CARTESIAN_POINT ( 'NONE',  ( -8.355902744723985975, 8.642974711799791265, 1.040834085586084257E-14 ) ) ;
#166762 = CARTESIAN_POINT ( 'NONE',  ( 3.954788147838703249, -1.976257328041197470, -0.7601183944087180899 ) ) ;
#166761 = CARTESIAN_POINT ( 'NONE',  ( -5.151735183512911043, 6.073074471262228435, 1.082531754730548412 ) ) ;
#166763 = CARTESIAN_POINT ( 'NONE',  ( -4.101444922696786399, 3.685019076479660427, -2.500000000000000444 ) ) ;
#166764 = CARTESIAN_POINT ( 'NONE',  ( 5.775854211382815073, -2.020734006234246927, 0.4499205674863211990 ) ) ;
#166766 = CARTESIAN_POINT ( 'NONE',  ( 6.620655732516649294, 0.5674144795907026806, 2.226195167976598110 ) ) ;
#166765 = CARTESIAN_POINT ( 'NONE',  ( 2.718400508848108466, 1.969533948853121386, 0.7019594197221010745 ) ) ;
#166768 = EDGE_LOOP ( 'NONE', ( #64208, #202329, #206169, #65656 ) ) ;
#166767 = CARTESIAN_POINT ( 'NONE',  ( 1.254464346661397833, -1.363098773983735024, 1.056675342818178542 ) ) ;
#166769 = CARTESIAN_POINT ( 'NONE',  ( 6.317209508963599340, 9.457495962844502557, 1.199719254218462483 ) ) ;
#166770 = DIRECTION ( 'NONE',  ( -0.8164965809277262565, 8.702247276351162783E-15, 0.5773502691896256200 ) ) ;
#166771 = CARTESIAN_POINT ( 'NONE',  ( -11.00592740523952351, 13.61020242468316432, 1.444008943503716225 ) ) ;
#166772 = CARTESIAN_POINT ( 'NONE',  ( -9.644676237148278375, 5.067654118421841325, 6.575762993896887565 ) ) ;
#166773 = CARTESIAN_POINT ( 'NONE',  ( 5.788968402910795064, 9.697620870130524651, 0.7216878364870438212 ) ) ;
#166774 = CARTESIAN_POINT ( 'NONE',  ( 0.000000000000000000, 1.000000000000000888, -9.999999999999998224 ) ) ;
#166776 = CARTESIAN_POINT ( 'NONE',  ( 0.1350377444619410283, -0.09094779274463302143, 1.809295058508665566 ) ) ;
#166775 = CARTESIAN_POINT ( 'NONE',  ( 5.722423353419669567, 8.833855124701747386, 1.199719254218451159 ) ) ;
#166777 = CARTESIAN_POINT ( 'NONE',  ( -7.100719765255177229, 9.307259030929609267, -1.599625672291263179 ) ) ;
#166778 = CARTESIAN_POINT ( 'NONE',  ( 5.352771719296971042, 5.139321848801576387, 0.7998128361456341429 ) ) ;
#166779 = CARTESIAN_POINT ( 'NONE',  ( -6.401963353335964335, 6.822014978843597532, 0.5293317295896986518 ) ) ;
#166780 = CARTESIAN_POINT ( 'NONE',  ( 6.688968683495743583, 8.897159112202094988, -1.599625672291283607 ) ) ;
#166781 = CARTESIAN_POINT ( 'NONE',  ( -6.778728372092626131, -7.783114986501003862, 6.734029298721179835 ) ) ;
#166783 = B_SPLINE_CURVE_WITH_KNOTS ( 'NONE', 3,
 ( #6388, #56232, #188350, #39990 ),
 .UNSPECIFIED., .F., .F.,
 ( 4, 4 ),
 ( 0.000000000000000000, 1.930757672285080358E-06 ),
 .UNSPECIFIED. ) ;
#166782 = CARTESIAN_POINT ( 'NONE',  ( -11.33772465723237666, 11.00868300734826910, 3.600000000000073364 ) ) ;
#166784 = CARTESIAN_POINT ( 'NONE',  ( 9.625925876022625616, 11.29296361252366765, -1.082531754730537088 ) ) ;
#166785 = ORIENTED_EDGE ( 'NONE', *, *, #124624, .T. ) ;
#166786 = CARTESIAN_POINT ( 'NONE',  ( 0.8256309606260933132, 0.7751641160983432366, -1.751937020314651150 ) ) ;
#166787 = CARTESIAN_POINT ( 'NONE',  ( 0.2762449081346768920, 2.096790360132039233, -0.3154013857558089495 ) ) ;
#166788 = CARTESIAN_POINT ( 'NONE',  ( -1.909527279894951413, 8.998253746724575564, 0.7750000000000013545 ) ) ;
#166789 = VECTOR ( 'NONE', #204742, 1000.000000000000000 ) ;
#166790 = CARTESIAN_POINT ( 'NONE',  ( -0.1399997263889611598, 6.947783040739049731, -2.595329734540325006 ) ) ;
#166791 = CARTESIAN_POINT ( 'NONE',  ( -1.571977147778457651, 8.681624870483057421, -2.500282472944432399 ) ) ;
#166792 = CARTESIAN_POINT ( 'NONE',  ( -4.826339496784927796, 5.693446170079573321, 1.082531754730560403 ) ) ;
#166793 = CARTESIAN_POINT ( 'NONE',  ( 9.300530189294644146, 10.91333531134101165, -1.082531754730543083 ) ) ;
#166794 = CARTESIAN_POINT ( 'NONE',  ( 4.610180678033913182, 1.969109005737102347, -0.04407691609572064739 ) ) ;
#166795 = CARTESIAN_POINT ( 'NONE',  ( 1.875790325896836919, 0.3594715711359475208, -2.089634487563592824 ) ) ;
#166796 = CARTESIAN_POINT ( 'NONE',  ( -5.422371370461663176, 8.413518134592214537, -1.199719254218446718 ) ) ;
#166797 = FACE_OUTER_BOUND ( 'NONE', #48743, .T. ) ;
#166799 = EDGE_CURVE ( 'NONE', #142721, #189233, #59377, .T. ) ;
#166798 = DIRECTION ( 'NONE',  ( -0.5000000000000003331, 0.000000000000000000, -0.8660254037844383745 ) ) ;
#166800 = CARTESIAN_POINT ( 'NONE',  ( 2.483611571103708116, -0.6279893487078171965, 1.916353726171161620 ) ) ;
#166801 = CARTESIAN_POINT ( 'NONE',  ( 5.753911783233988331, 0.8852683131516884130, 2.004867968450708915 ) ) ;
#166802 = DIRECTION ( 'NONE',  ( 5.551115123125764829E-17, 0.000000000000000000, -1.000000000000000000 ) ) ;
#166803 = CARTESIAN_POINT ( 'NONE',  ( 3.786086853528514151, -0.9505683805260138897, 1.675471031514904396 ) ) ;
#166804 = CARTESIAN_POINT ( 'NONE',  ( -7.212047647465563038, 10.50147379109678880, -1.199719254218446718 ) ) ;
#166805 = CARTESIAN_POINT ( 'NONE',  ( 0.1119280604304096899, -0.7754228321929098611, -1.651232954423286436 ) ) ;
#166806 = CARTESIAN_POINT ( 'NONE',  ( 1.190363680384380229, -0.9894552095768920363, 1.972713631218452557 ) ) ;
#166807 = CARTESIAN_POINT ( 'NONE',  ( 5.431895982697334091, 6.433277491268158954, -1.247050338538328029 ) ) ;
#166808 = VERTEX_POINT ( 'NONE', #123205 ) ;
#166809 = DIRECTION ( 'NONE',  ( 0.000000000000000000, -1.000000000000000000, 0.000000000000000000 ) ) ;
#166810 = CARTESIAN_POINT ( 'NONE',  ( 6.315293006042116630, -1.687366247620238457, -1.015419155273014740 ) ) ;
#166811 = CARTESIAN_POINT ( 'NONE',  ( 0.6966983018150345597, 1.588492033560371830, 1.117026046969020303 ) ) ;
#166812 = CARTESIAN_POINT ( 'NONE',  ( 6.433027599926354867, 1.173280253959343211, 1.976260322036479167 ) ) ;
#166814 = CARTESIAN_POINT ( 'NONE',  ( 4.522197165953073750, 0.8743044213657903407, 1.642730557785059053 ) ) ;
#166813 = CARTESIAN_POINT ( 'NONE',  ( -7.618755976236585958, 7.853246491889623648, 0.000000000000000000 ) ) ;
#166815 = CARTESIAN_POINT ( 'NONE',  ( 5.691390622686558487, 9.861982503101517139, 0.7998128361456341429 ) ) ;
#166817 = EDGE_CURVE ( 'NONE', #173465, #87461, #42111, .T. ) ;
#166816 = FACE_OUTER_BOUND ( 'NONE', #208551, .T. ) ;
#166819 = B_SPLINE_CURVE_WITH_KNOTS ( 'NONE', 3,
 ( #90118, #170274, #4541, #22938, #102083, #54407, #187590, #136730, #85831, #69551, #21859, #203820, #19751, #105306, #204888, #186525, #87966, #104227, #151910, #70616, #56539, #122701, #154041, #171343, #3484, #120546, #155110, #156184, #188664, #5606, #20804, #89053, #7762, #6695, #71688, #72770, #138869, #40293, #106404, #73851, #53330, #139946, #201685, #205972, #123763, #37071, #36002, #103152, #189725, #158317, #12039, #79180, #208102, #9908, #74920, #62925, #145296, #91188, #41378, #142088, #13100, #160433, #27222, #26157, #207038, #211301, #78110, #177759, #144237, #29375, #192916, #111754, #59731, #108549, #173513, #210231, #125889, #107488, #95470, #60798, #174581, #8842, #25087, #128034, #157249, #159364, #126957, #44572, #141031, #58669, #61869, #124818, #190782, #75984, #10963, #42446, #93328, #92271, #191847, #161518, #109631, #143165, #43510, #175636, #77038, #209160, #193988, #110688, #176686, #28298, #94395, #45636, #117070, #64000, #80248, #181991, #114940, #32560, #178833, #15227, #34682, #149514, #199301, #14154, #148457, #133295, #50946, #83432, #116005, #98637, #16282, #183068, #131199, #65043, #162580, #132233, #130151, #100751, #196141, #198242, #146347, #49880, #27, #47781, #96531, #150592, #197187, #66091, #48824, #164696, #81317, #163647, #33624, #31513, #166833, #99695, #212359, #97588, #30447, #113895, #165765, #195065, #82368, #1099, #180940, #17350, #67159, #18429, #84502, #179889, #147393, #2154, #213420, #129094, #46705, #112820, #171082, #134362, #101823, #89865, #6432, #70359, #155915, #119200, #136473, #21600, #202494, #54146, #154848, #56279, #200366, #103970, #105046, #167890, #3225, #69293, #137542, #72506, #87706, #68230, #120282, #36809, #102892, #55212, #52015, #184126, #186257, #170012, #38962, #71430, #151655, #135404, #204628, #106144, #153778, #201427, #19491, #37892, #88790, #138605, #85566, #122438, #188396, #22678, #121358, #5348, #203559, #40032, #187333, #4287, #53067, #172168, #185186, #23760, #168951, #118141, #20553, #35749, #86638, #152705, #60527, #29107, #9645, #26956, #158059, #125625, #108294, #42179, #142896, #124563, #127770, #93063, #189471, #190522, #123506, #90926, #126688, #191583, #41113, #94132, #95190, #59466, #75721, #73584, #174315, #28037, #107222, #25889, #177494, #7500, #91999, #44303, #111486, #141835, #207840, #173246, #139687, #205708, #24824, #57343, #43245, #110425, #192650, #109364, #58409, #156992, #8579, #176428, #209961, #160171, #61600, #10704, #11771, #76773, #77844, #193726, #74659, #175373, #143967, #45370, #140763, #159102, #208896, #206775, #66892, #180677, #128812, #63727, #62653, #30168, #65826, #130934, #194793, #33358, #182805, #47509, #116805, #181727, #212091, #148197, #211028, #179624, #34422, #161241, #129886, #197984, #50680, #31244, #195870, #46430, #12827, #78902, #112548, #145024, #113621, #199032, #64790, #178558, #96256, #162309, #13894, #49612, #149249, #115737, #822, #164432, #83166, #97321, #79975, #146079, #131974, #163377, #14952, #133032, #32302, #81049, #147134, #213160, #196927, #48564, #114684, #98369, #16018, #82104, #214197, #99439, #165494, #17088, #166570, #136216, #137289, #200112, #35488, #101566, #169763, #104787, #53888, #188143, #168696, #20301, #184929, #87459, #100495, #1899, #102640, #202236, #71171 ),
 .UNSPECIFIED., .F., .F.,
 ( 4, 1, 1, 1, 1, 1, 1, 1, 1, 1, 1, 1, 1, 1, 1, 1, 1, 1, 1, 1, 1, 1, 1, 1, 1, 1, 1, 1, 1, 1, 1, 1, 1, 1, 1, 1, 1, 1, 1, 1, 1, 1, 1, 1, 1, 1, 1, 1, 1, 1, 1, 1, 1, 1, 1, 1, 1, 1, 1, 1, 1, 1, 1, 1, 1, 1, 1, 1, 1, 1, 1, 1, 1, 1, 1, 1, 1, 1, 1, 1, 1, 1, 1, 1, 1, 1, 1, 1, 1, 1, 1, 1, 1, 1, 1, 1, 1, 1, 1, 1, 1, 1, 1, 1, 1, 1, 1, 1, 1, 1, 1, 1, 1, 1, 1, 1, 1, 1, 1, 1, 1, 1, 1, 1, 1, 1, 1, 1, 1, 1, 1, 1, 1, 1, 1, 1, 1, 1, 1, 1, 1, 1, 1, 1, 1, 1, 1, 1, 1, 1, 1, 1, 1, 1, 1, 1, 1, 1, 1, 1, 1, 1, 1, 1, 1, 1, 1, 1, 1, 1, 1, 1, 1, 1, 1, 1, 1, 1, 1, 1, 1, 1, 1, 1, 1, 1, 1, 1, 1, 1, 1, 1, 1, 1, 1, 1, 1, 1, 1, 1, 1, 1, 1, 1, 1, 1, 1, 1, 1, 1, 1, 1, 1, 1, 1, 1, 1, 1, 1, 1, 1, 1, 1, 1, 1, 1, 1, 1, 1, 1, 1, 1, 1, 1, 1, 1, 1, 1, 1, 1, 1, 1, 1, 1, 1, 1, 1, 1, 1, 1, 1, 1, 1, 1, 1, 1, 1, 1, 1, 1, 1, 1, 1, 1, 1, 1, 1, 1, 1, 1, 1, 1, 1, 1, 1, 1, 1, 1, 1, 1, 1, 1, 1, 1, 1, 1, 1, 1, 1, 1, 1, 1, 1, 1, 1, 1, 1, 1, 1, 1, 1, 1, 1, 1, 1, 1, 1, 1, 1, 1, 1, 1, 1, 1, 1, 1, 1, 1, 1, 1, 1, 1, 1, 1, 1, 1, 1, 1, 1, 1, 1, 1, 1, 1, 1, 1, 1, 1, 1, 1, 1, 1, 1, 1, 1, 1, 1, 1, 1, 1, 1, 1, 1, 1, 1, 1, 1, 1, 1, 1, 1, 1, 1, 1, 1, 1, 1, 1, 1, 1, 1, 1, 1, 1, 1, 1, 1, 1, 1, 1, 1, 1, 1, 1, 4 ),
 ( 0.000000000000000000, 0.002600063085273907840, 0.005208809393482579861, 0.007813201938950280895, 0.01041611862257568050, 0.01302098276518856741, 0.01562474632808895890, 0.01822919105953027183, 0.02083324087635668453, 0.02343728507989274734, 0.02604173773626635227, 0.02864548761524753420, 0.03125016255115702773, 0.03385383280295282959, 0.03645844125268089125, 0.03906229690237970897, 0.04166656525949016115, 0.04427081591349327910, 0.04687468903198145631, 0.04947928942627017462, 0.05208296534865054783, 0.05468764290212216328, 0.05729137561078536528, 0.05989584521530456201, 0.06249987723257615507, 0.06510392926424246607, 0.06770838613806146045, 0.07031213076997053224, 0.07291680575263978503, 0.07552047744215656389, 0.07812508546332513903, 0.08072894086165181837, 0.08333320924388483431, 0.08593745993457323207, 0.08854133291633270453, 0.09114593330519306369, 0.09374960916840779923, 0.09635428668231969807, 0.09895801939011879267, 0.1015624889210437753, 0.1041665209728785957, 0.1067705729027476208, 0.1093750297965602747, 0.1119787743537518920, 0.1145834493281674554, 0.1171871210017138010, 0.1197917289818775377, 0.1223955844170728779, 0.1249998527215379351, 0.1276041034591044177, 0.1302079763611066199, 0.1328125767709825433, 0.1354162526020633861, 0.1380209301064295735, 0.1406246628425296130, 0.1432291323291436380, 0.1458331644451768827, 0.1484372163025670099, 0.1510416732455448496, 0.1536454177576472568, 0.1562500927529001105, 0.1588537644400710158, 0.1614583724083656635, 0.1640622279099430147, 0.1666664961659596600, 0.1692707469797122277, 0.1718746198314790308, 0.1744792202914958457, 0.1770828961200470730, 0.1796875736439581817, 0.1822913064379278192, 0.1848957759094348730, 0.1874998081190861754, 0.1901038599334289314, 0.1927083169547665342, 0.1953120614513534081, 0.1979167364965291054, 0.2005204082269216870, 0.2031250162124720871, 0.2057288718099357372, 0.2083331400468157457, 0.2109373909660553770, 0.2135412637971000893, 0.2161458643363758370, 0.2187495401919937743, 0.2213542177645327069, 0.2239579506459335456, 0.2265624201315297737, 0.2291664524642116896, 0.2317705042649303715, 0.2343749613938155840, 0.2369787059044528299, 0.2395833810286300269, 0.2421870528318344207, 0.2447916608637582536, 0.2473955165866061623, 0.2499997848336539263, 0.2526040358876752157, 0.2552079087275039293, 0.2578125093751503782, 0.2604161852874245509, 0.2630208629376679097, 0.2656245959360551967, 0.2682290654649299166, 0.2708330979500496172, 0.2734371497665608608, 0.2760416070321756732, 0.2786453515864226738, 0.2812500268186742258, 0.2838536987242743503, 0.2864583068316831627, 0.2890621627094078216, 0.2916664309959213219, 0.2942706822140139789, 0.2968745550921262355, 0.2994791558772498252, 0.3020828318757637354, 0.3046875096327826826, 0.3072912427777066413, 0.3098957123790437307, 0.3124997450460035853, 0.3151037969077182255, 0.3177082543392401592, 0.3203119989666507461, 0.3229166743360447622, 0.3255203463736199843, 0.3281249545856204097, 0.3307288106477103140, 0.3333330790029824242, 0.3359373304144318562, 0.3385412033603223403, 0.3411458043120255135, 0.3437494804263583337, 0.3463541583192197293, 0.3489578916402267250, 0.3515623613432052874, 0.3541663942214042238, 0.3567704461577280162, 0.3593749037843310123, 0.3619786485144548260, 0.3645833240500557237, 0.3671869962491814965, 0.3697916045948764219, 0.3723954608708167080, 0.3749997293241361662, 0.3776039809582251716, 0.3802078540013843488, 0.3828124551487663840, 0.3854161314084936785, 0.3880208094662612184, 0.3906245429928945634, 0.3932290128266905938, 0.3958330459455252637, 0.3984370979858605777, 0.4010415558367163569, 0.4036453006990994852, 0.4062499764299690730, 0.4088536488202184072, 0.4114582573287078326, 0.4140621138479816388, 0.4166663824286341855, 0.4192706343146435644, 0.4218745074845589027, 0.4244791088567174686, 0.4270827852914125256, 0.4296874635431477407, 0.4322911973049493040, 0.4348956672987361882, 0.4374997006876018557, 0.4401037528613486738, 0.4427082109656274023, 0.4453119559898139901, 0.4479166319450127998, 0.4505203045559570407, 0.4531249132563394122, 0.4557287700484292658, 0.4583330387856985322, 0.4609372909529084184, 0.4635411642790657205, 0.4661457659050973201, 0.4687494425443319290, 0.4713541210190953512, 0.4739578550456061690, 0.4765623252285562383, 0.4791663589168480009, 0.4817704112534048067, 0.4843748696402766507, 0.4869786148558097882, 0.4895832910643978519, 0.4921869639256079565, 0.4947915728469811647, 0.4973954299413693159, 0.4999996988645384333, 0.5026039513422294602, 0.5052078248541136407, 0.5078124267631153321, 0.5104161036364611714, 0.5130207823633133879, 0.5156245166840751626, 0.5182289870853604707, 0.5208330211024742029, 0.5234370736312391470, 0.5260415323298749390, 0.5286452777662975500, 0.5312499542573357880, 0.5338536273983837122, 0.5364582365698458144, 0.5390620939960163449, 0.5416663631343685559, 0.5442706159518226894, 0.5468744896789192733, 0.5494790918999890028, 0.5520827690370186946, 0.5546874480450217915, 0.5572911826895774468, 0.5598956533383712131, 0.5624996877137050655, 0.5651037404640770756, 0.5677081995036498130, 0.5703119451905063197, 0.5729166219930570403, 0.5755202954435161278, 0.5781249048941674573, 0.5807287626816063364, 0.5833330320644263267, 0.5859372852509285856, 0.5885411592227242084, 0.5911457617849628088, 0.5937494392152512512, 0.5963541185334689798, 0.5989578535313645480, 0.6015623244568418793, 0.6041663592197970001, 0.6067704122211770024, 0.6093748716308627911, 0.6119786175976995590, 0.6145832947408284008, 0.6171869685302752151, 0.6197915782892181591, 0.6223954364674153528, 0.6249997061239902507, 0.6276039597088286515, 0.6302078339548128350, 0.6328124368873246919, 0.6354161146404495586, 0.6380207942979494451, 0.6406245296787346222, 0.6432290009100736228, 0.6458330360900554901, 0.6484370893718474083, 0.6510415491808263511, 0.6536452954571934093, 0.6562499729699700080, 0.6588536471279848872, 0.6614582572243260516, 0.6640621158227759668, 0.6666663857823964534, 0.6692706397948642305, 0.6718745143445301604, 0.6744791176764239893, 0.6770827957819672838, 0.6796874758078212952, 0.6822912116010506622, 0.6848956831674339885, 0.6874997187938534093, 0.6901037723854651640, 0.6927082326229228038, 0.6953119792383747333, 0.6979166571498732763, 0.7005203317060422208, 0.7031249421688929857, 0.7057288012170955804, 0.7083330715090569996, 0.7109373259784533827, 0.7135412008612989077, 0.7161458046216893081, 0.7187494831092385850, 0.7213541635325240176, 0.7239578997677582617, 0.7265623716983737879, 0.7291664078006476757, 0.7317704617314926274, 0.7343749224266207243, 0.7369786694107173242, 0.7395833477500189934, 0.7421870227339337767, 0.7447916335924112952, 0.7473954931198736329, 0.7499997637734774347, 0.7526040187291080930, 0.7552078939746372788, 0.7578124981926457338, 0.7604161770917949870, 0.7630208579415957981, 0.7656245946484027121, 0.7682290669724446408, 0.7708331035799980135, 0.7734371578794957403, 0.7760416190614934928, 0.7786453664438016675, 0.7812500452399944173, 0.7838537206812543623, 0.7864583319644831150, 0.7890621920007202528, 0.7916664630452742157, 0.7942707185164536998, 0.7968745941541772737, 0.7994791988589329268, 0.8020828781992835887, 0.8046875595046918406, 0.8072912967126475436, 0.8098957694593176271, 0.8124998066015838294, 0.8151038612991610144, 0.8177083229972362810, 0.8203120708073305956, 0.8229167500895105958, 0.8255204260177235742, 0.8281250377548363684, 0.8307288983293719120, 0.8333331697941922522, 0.8359374258102438837, 0.8385413018696807885, 0.8411459070903221091, 0.8437495869014844940, 0.8463542686916004643, 0.8489580064302900686, 0.8515624796287988296, 0.8541665173352209761, 0.8567705724603134065, 0.8593750347036837045, 0.8619787829711476057, 0.8645834627684209073, 0.8671871392132045608, 0.8697917514333429745, 0.8723956125757112989, 0.8749998844901232253, 0.8776041410803804288, 0.8802080175910590443, 0.8828126233567346048, 0.8854163036683286858, 0.8880209859722626442, 0.8906247242712825862, 0.8932291979508502067, 0.8958332362508822921, 0.8984372918329353030, 0.9010417546508288078, 0.9036455034052560675, 0.9062501837467389354, 0.9088538607377212308, 0.9114584734700372781, 0.9140623352097841936, 0.9166666076031229071, 0.9192708647969299873, 0.9218747417883903505, 0.9244793481282622682, 0.9270830289699085736, 0.9296877118167798937, 0.9322914507057830091, 0.9348959248956096868, 0.9374999638185942397, 0.9401040198872741005, 0.9427084833090058069, 0.9453122325795346725, 0.9479169134952544207, 0.9505205910598265584, 0.9531252043308329203, 0.9557290667238423909, 0.9583333396063040688, 0.9609375973010293448, 0.9635414750455153499, 0.9661460823481272664, 0.9687497623469286667, 0.9713544456720903941, 0.9739581901020435417, 0.9765626606554614897, 0.9791666924408860551, 0.9817707657828746992, 0.9843752055175947202, 0.9869789906880002128, 0.9895838567146432174, 0.9921867690109741345, 0.9947911791560083428, 0.9973999138825643263, 0.9999999999999998890 ),
 .UNSPECIFIED. ) ;
#166818 = CARTESIAN_POINT ( 'NONE',  ( -4.543954038874438162, 8.453030145328826350, 1.040834085586084257E-14 ) ) ;
#166820 = CARTESIAN_POINT ( 'NONE',  ( -3.381773599491823656, -0.9528023431436689616, 0.2057550699296430974 ) ) ;
#166821 = CARTESIAN_POINT ( 'NONE',  ( -0.1114211809780316365, -0.4883405756051837354, -2.144353428667714390 ) ) ;
#166822 = CARTESIAN_POINT ( 'NONE',  ( 5.178851490740205676, 6.104710163027444736, 1.082531754730558626 ) ) ;
#166823 = AXIS2_PLACEMENT_3D ( 'NONE', #105095, #102944, #106195 ) ;
#166824 = CARTESIAN_POINT ( 'NONE',  ( 10.98997987423603995, -6.700000000000007283, -0.4694063952341755996 ) ) ;
#166825 = CARTESIAN_POINT ( 'NONE',  ( -0.4373349612950744869, -5.212340523078053955, -10.97895254167817569 ) ) ;
#166826 = CARTESIAN_POINT ( 'NONE',  ( 0.3283667639546791195, 1.746078182827022429, 0.5332771064449209897 ) ) ;
#166827 = CARTESIAN_POINT ( 'NONE',  ( -4.192495815123836955, 5.914331089109674089, -1.599625672291256295 ) ) ;
#166828 = CARTESIAN_POINT ( 'NONE',  ( 3.832397100292153524, 0.5799717274662331556, -1.634443932507266384 ) ) ;
#166829 = CARTESIAN_POINT ( 'NONE',  ( 3.469446951953614189E-15, -16.99999999999999645, 6.938893903907228378E-15 ) ) ;
#166830 = CARTESIAN_POINT ( 'NONE',  ( -0.6125000000000262457, 2.791666666666692276, 1.060881119635882497 ) ) ;
#166831 = CARTESIAN_POINT ( 'NONE',  ( -0.3282377607281317666, 0.3013354503153871100, 1.224999999999968114 ) ) ;
#166832 = CARTESIAN_POINT ( 'NONE',  ( 0.3461526914491962481, 1.921225470409862357, 0.1432632881103387268 ) ) ;
#166833 = CARTESIAN_POINT ( 'NONE',  ( 4.293769791895286403, -1.349757117914761384, -1.423854091114319598 ) ) ;
#166834 = CARTESIAN_POINT ( 'NONE',  ( -9.515124878692420296, 9.995400534762978850, 1.040834085586084257E-14 ) ) ;
#166835 = CARTESIAN_POINT ( 'NONE',  ( 5.425234023762710578, 9.481190127698507553, -0.7998128361456291469 ) ) ;
#166836 = CARTESIAN_POINT ( 'NONE',  ( 5.145234815219777325, 0.1564148900096741512, 2.114790009947895122 ) ) ;
#166837 = CARTESIAN_POINT ( 'NONE',  ( 5.508355548902068577, 9.648441583686274470, 0.7998128361456331437 ) ) ;
#166838 = CARTESIAN_POINT ( 'NONE',  ( -8.350932551013499960, 11.83017284523606172, -1.199719254218446718 ) ) ;
#166839 = DIRECTION ( 'NONE',  ( -0.000000000000000000, -1.000000000000000000, 0.000000000000000000 ) ) ;
#166840 = CARTESIAN_POINT ( 'NONE',  ( 2.676698048161993082, 1.355622082481915847, -1.564734663558226879 ) ) ;
#166842 = CARTESIAN_POINT ( 'NONE',  ( -1.402160292154681736E-14, -0.1156249996585793222, 1.575800808251672791 ) ) ;
#166841 = LINE ( 'NONE', #131206, #144695 ) ;
#166843 = ORIENTED_EDGE ( 'NONE', *, *, #32207, .T. ) ;
#166844 = CARTESIAN_POINT ( 'NONE',  ( 3.358291665479910648, 0.05479990919179249936, -2.298175070600398939 ) ) ;
#166845 = CARTESIAN_POINT ( 'NONE',  ( 8.649738815838679429, 10.15407870897571563, -1.082531754730543083 ) ) ;
#166847 = CARTESIAN_POINT ( 'NONE',  ( 3.285556943750000514, -1.713541666188707735, 1.896917185911906500 ) ) ;
#166846 = CARTESIAN_POINT ( 'NONE',  ( 8.014278199453778839, 8.522615118883788199, 0.000000000000000000 ) ) ;
#166848 = FACE_OUTER_BOUND ( 'NONE', #128967, .T. ) ;
#166849 = DIRECTION ( 'NONE',  ( 0.000000000000000000, 0.000000000000000000, 1.000000000000000000 ) ) ;
#166850 = EDGE_LOOP ( 'NONE', ( #23173, #4386, #25388, #118226 ) ) ;
#166851 = CARTESIAN_POINT ( 'NONE',  ( 0.000000000000000000, 7.999999999999992895, 0.000000000000000000 ) ) ;
#166852 = CARTESIAN_POINT ( 'NONE',  ( 4.060738401289211374, 0.5150538496448524572, 1.841637258418599155 ) ) ;
#166853 = CARTESIAN_POINT ( 'NONE',  ( -0.1021852871539802865, 7.053056311352817076, -4.037408415137027085 ) ) ;
#166854 = CARTESIAN_POINT ( 'NONE',  ( 4.752814332062330394, -1.383916046847250669, 1.029161146002472549 ) ) ;
#166855 = CARTESIAN_POINT ( 'NONE',  ( 3.714077560468319827, 1.074663192196689376, -1.706111893292367343 ) ) ;
#166856 = CARTESIAN_POINT ( 'NONE',  ( 5.010469735608720221, -2.183386834666663390, 0.7190086036765501731 ) ) ;
#166857 = CARTESIAN_POINT ( 'NONE',  ( 4.296393142825894351, -2.000000000000001776, -4.470011852588160473 ) ) ;
#166858 = CARTESIAN_POINT ( 'NONE',  ( 0.7685542157043163680, 1.090964843879228097, 1.918292034055509632 ) ) ;
#166859 = CARTESIAN_POINT ( 'NONE',  ( -6.292392690518214593, 7.474117906093608710, -1.082531754730549967 ) ) ;
#166860 = EDGE_LOOP ( 'NONE', ( #31155, #87389, #133472, #1575 ) ) ;
#166861 = CARTESIAN_POINT ( 'NONE',  ( 5.325387591137793919, -1.680293062798293713, 0.5557786991975487423 ) ) ;
#166863 = CARTESIAN_POINT ( 'NONE',  ( 2.045279198001882737, -1.842668879747776156, -1.363283251902024817 ) ) ;
#166862 = CARTESIAN_POINT ( 'NONE',  ( 6.038177310039780643, 8.137902509836795417, -1.599625672291283607 ) ) ;
#166864 = CARTESIAN_POINT ( 'NONE',  ( 6.632757984263843554, -1.642112545546599023, 0.8327811610863435909 ) ) ;
#166865 = FACE_OUTER_BOUND ( 'NONE', #61286, .T. ) ;
#166866 = CARTESIAN_POINT ( 'NONE',  ( 11.86239285000045918, 11.30000000000000249, -1.812080536912752837 ) ) ;
#166867 = CARTESIAN_POINT ( 'NONE',  ( -3.817502770699643388, 6.611447778194983194, 1.199719254218452935 ) ) ;
#166868 = CARTESIAN_POINT ( 'NONE',  ( 1.360316468749955598, -0.7239583329918893861, 0.7853790794158480582 ) ) ;
#166869 = CARTESIAN_POINT ( 'NONE',  ( 3.933798568561588826, 7.324796930770500758, -0.8815854234727003025 ) ) ;
#166870 =( BOUNDED_CURVE ( )  B_SPLINE_CURVE ( 2, ( #121170, #5160, #200173, #38768, #70169, #135224, #34486, #170895, #154655 ),
 .UNSPECIFIED., .F., .T. ) 
 B_SPLINE_CURVE_WITH_KNOTS ( ( 3, 2, 2, 2, 3 ),
 ( 0.2968749999999998335, 0.3020833333333333148, 0.3125000000000000000, 0.3229166666666666852, 0.3281250000000001665 ),
 .UNSPECIFIED. ) 
 CURVE ( )  GEOMETRIC_REPRESENTATION_ITEM ( )  RATIONAL_B_SPLINE_CURVE ( ( 0.9330127018922194093, 0.9330127018922171889, 1.000000000000000000, 0.8660254037844387076, 1.000000000000000000, 0.8660254037844387076, 1.000000000000000000, 0.9330127018922171889, 0.9330127018922194093 ) ) 
 REPRESENTATION_ITEM ( '' )  );
#166871 = CARTESIAN_POINT ( 'NONE',  ( 0.1335669894368500255, -0.0009366757763962055587, -2.153671288142432250 ) ) ;
#166872 = CARTESIAN_POINT ( 'NONE',  ( 0.7257964430846426396, 0.8128130212789463904, -1.845628942776005088 ) ) ;
#166873 = AXIS2_PLACEMENT_3D ( 'NONE', #97672, #163729, #81399 ) ;
#166874 = CARTESIAN_POINT ( 'NONE',  ( 0.7499999999999885647, 0.5145833340161540814, 1.299038105676657340 ) ) ;
#166875 = CARTESIAN_POINT ( 'NONE',  ( 5.531840760993587125, -1.223730149660817501, -1.487915846976423984 ) ) ;
#166876 = EDGE_CURVE ( 'NONE', #104139, #2091, #171377, .T. ) ;
#166877 = CARTESIAN_POINT ( 'NONE',  ( -0.6823417656250003738, 11.65104166700806765, 1.181850606188754593 ) ) ;
#166878 = CARTESIAN_POINT ( 'NONE',  ( 2.725082634249659463, 1.605975871135911559, -1.534981474645187971 ) ) ;
#166879 = EDGE_LOOP ( 'NONE', ( #194624, #183300, #108131, #113451, #133007, #106877 ) ) ;
#166882 = PRESENTATION_LAYER_ASSIGNMENT (  '', '', ( #80294 ) ) ;
#166881 = CARTESIAN_POINT ( 'NONE',  ( -2.273105066167346422, 5.702484939155337607, 2.420000000000010587 ) ) ;
#166880 = CARTESIAN_POINT ( 'NONE',  ( 1.499999999999819034, 7.267697830503895950, -4.207111467970846341 ) ) ;
#166883 = CARTESIAN_POINT ( 'NONE',  ( 4.786522169170392971, 5.141580351323886688, 0.8077998227834035649 ) ) ;
#166884 = CARTESIAN_POINT ( 'NONE',  ( 9.901532256681887745, 10.44620914241737530, 0.000000000000000000 ) ) ;
#166885 = CARTESIAN_POINT ( 'NONE',  ( -11.07790593930098311, 12.30000000000000071, 0.6999999999999992895 ) ) ;
#166886 = SURFACE_SIDE_STYLE ('',( #21651 ) ) ;
#166887 = CARTESIAN_POINT ( 'NONE',  ( 4.493551464656197147, -1.740228352261258049, -0.03666429755099299970 ) ) ;
#166888 = CARTESIAN_POINT ( 'NONE',  ( 2.682025323810240280, -1.127217178123595565, -1.605522638798158264 ) ) ;
#166890 = CARTESIAN_POINT ( 'NONE',  ( -6.887178846062116833, 9.058127958537705027, -1.443375672974059665 ) ) ;
#166889 = CARTESIAN_POINT ( 'NONE',  ( 4.741601036477289810, 6.554953847355395880, 1.599625672291267398 ) ) ;
#166891 = FACE_OUTER_BOUND ( 'NONE', #181145, .T. ) ;
#166892 = CARTESIAN_POINT ( 'NONE',  ( 10.70146331988817323, 11.37946204949139251, 0.7998128361456341429 ) ) ;
#166893 = CARTESIAN_POINT ( 'NONE',  ( 0.4849267205471480269, 1.973383872003172224, 0.6002626889692606049 ) ) ;
#166894 = CARTESIAN_POINT ( 'NONE',  ( -6.669721502918952716, 9.868759955792373972, 1.199719254218452047 ) ) ;
#166895 = CARTESIAN_POINT ( 'NONE',  ( -3.592547517496941900, 5.214391408544949869, -1.443375672974051449 ) ) ;
#166896 = CARTESIAN_POINT ( 'NONE',  ( 1.341102801589135529, 0.4431706325995210527, 2.218532444564396577 ) ) ;
#166897 = VERTEX_POINT ( 'NONE', #520 ) ;
#166898 = CARTESIAN_POINT ( 'NONE',  ( 0.7499999999999885647, -0.2354166659838466402, 1.299038105676657340 ) ) ;
#166899 = CARTESIAN_POINT ( 'NONE',  ( 3.040157689216971715, 1.855973101128991054, 0.2326549598439253685 ) ) ;
#166900 = CARTESIAN_POINT ( 'NONE',  ( 1.881130407182354469, -0.4634198587198985475, -1.670964061236743348 ) ) ;
#166901 = CARTESIAN_POINT ( 'NONE',  ( 5.091441847573507928, -0.7891374179831472935, 2.044738775321436997 ) ) ;
#166902 = CARTESIAN_POINT ( 'NONE',  ( 5.421043267468262705, 2.129509263528307716, 0.8893739899358196199 ) ) ;
#166903 = CARTESIAN_POINT ( 'NONE',  ( 1.446242185974885963, 2.058501543756698915, 0.1019544441857832273 ) ) ;
#166904 = CARTESIAN_POINT ( 'NONE',  ( 3.169799299931614911, -1.156099248863748485, 1.560184043245048890 ) ) ;
#166905 = CARTESIAN_POINT ( 'NONE',  ( -3.090895833791289071, 6.549869539491048442, 1.040834085586084257E-14 ) ) ;
#166906 = CARTESIAN_POINT ( 'NONE',  ( 5.606678975738343951, 1.416997745663551633, -1.221222563005261552 ) ) ;
#166907 = CARTESIAN_POINT ( 'NONE',  ( 1.156250000000000888, -1.895863743164063031, 0.7852924748300492697 ) ) ;
#166908 = CARTESIAN_POINT ( 'NONE',  ( 4.100926828275982317, 7.458749316499424964, -0.6398019981258776800 ) ) ;
#166909 = CARTESIAN_POINT ( 'NONE',  ( 0.3152591496230552348, -1.397726865852641387, 1.025726801146044531 ) ) ;
#166910 = CARTESIAN_POINT ( 'NONE',  ( 4.177320726786311056, 5.966903162707725805, -1.443375672974068769 ) ) ;
#166911 = CARTESIAN_POINT ( 'NONE',  ( -1.360316468750062624, 1.619791667008073865, -0.7853790794159302147 ) ) ;
#166912 = CARTESIAN_POINT ( 'NONE',  ( 5.027970288326706338, -1.728003250605243180, 1.038991650911202713 ) ) ;
#166913 = CARTESIAN_POINT ( 'NONE',  ( -4.134873662043608178, 4.886736029548026217, 1.082531754730558626 ) ) ;
#166914 = CARTESIAN_POINT ( 'NONE',  ( 9.368847842243145152, 10.88907622316056312, 1.199719254218453823 ) ) ;
#166915 = CARTESIAN_POINT ( 'NONE',  ( 5.228604516725597229, 6.129068686715179126, -1.199719254218450271 ) ) ;
#166917 = CARTESIAN_POINT ( 'NONE',  ( 4.858757509019037357, 5.629766575900002401, 2.420000000000000373 ) ) ;
#166916 = CARTESIAN_POINT ( 'NONE',  ( 1.892912435568369744, 1.589020553905008626, -0.8988452475950716725 ) ) ;
#166918 = CARTESIAN_POINT ( 'NONE',  ( -5.906512197408906317, 6.919960980845699439, -1.199719254218453823 ) ) ;
#166919 = CARTESIAN_POINT ( 'NONE',  ( -8.654705636516467323E-15, -6.148216694138043614, -10.67870335800435733 ) ) ;
#166920 = FACE_OUTER_BOUND ( 'NONE', #132210, .T. ) ;
#166921 = EDGE_LOOP ( 'NONE', ( #83045, #184866, #59898, #26816 ) ) ;
#166922 = CARTESIAN_POINT ( 'NONE',  ( -5.844973620822877969, 7.912498205750389424, 1.443375672974058777 ) ) ;
#166923 = CARTESIAN_POINT ( 'NONE',  ( -2.117044542028253318, 5.621635732341564662, -0.7998128361456281477 ) ) ;
#166924 = CARTESIAN_POINT ( 'NONE',  ( -9.996439331977562404, 10.55693406359564790, 0.7998128361456462443 ) ) ;
#166925 = CARTESIAN_POINT ( 'NONE',  ( 0.2990895800742687793, -0.2513629124439535345, -2.004038569727568664 ) ) ;
#166927 = ORIENTED_EDGE ( 'NONE', *, *, #42815, .F. ) ;
#166926 = CARTESIAN_POINT ( 'NONE',  ( -0.05774110376318035420, -1.308430771297010908, -1.669371405835825550 ) ) ;
#166928 = CARTESIAN_POINT ( 'NONE',  ( -7.045397100956844127, 8.248660034984974132, -1.199719254218452047 ) ) ;
#166929 = VECTOR ( 'NONE', #16767, 1000.000000000000000 ) ;
#166930 = CARTESIAN_POINT ( 'NONE',  ( 3.845709127770629010, 7.638411082374393146, 0.7998128361456321445 ) ) ;
#166931 = CARTESIAN_POINT ( 'NONE',  ( 4.961820856888925491, 2.038780864349061250, -0.3001439806698430468 ) ) ;
#166932 = CARTESIAN_POINT ( 'NONE',  ( 5.221327349844218091, 1.987046161919112430, 0.3419379449052239450 ) ) ;
#166933 = ORIENTED_EDGE ( 'NONE', *, *, #187696, .F. ) ;
#166934 = ORIENTED_EDGE ( 'NONE', *, *, #105908, .F. ) ;
#166935 = CARTESIAN_POINT ( 'NONE',  ( 4.773438866691874338, 4.884607349446686619, -0.7620046207243836855 ) ) ;
#166936 = FACE_OUTER_BOUND ( 'NONE', #205039, .T. ) ;
#166937 =( BOUNDED_SURFACE ( )  B_SPLINE_SURFACE ( 1, 2, ( 
 ( #65019, #144212, #183834, #19191, #151355, #2924, #135114, #12014, #187032, #170791, #168653, #185959, #202192, #22382, #123214, #55981, #136173, #118904, #119982, #70061, #204324, #20257, #87418, #172947, #52768, #40815, #122134, #24526, #74370, #188099, #106923, #39730, #171862, #201130, #184888, #137248, #36512, #154553, #54914, #139378, #121065, #105835, #156695, #38665, #102598, #23456, #86341, #90635, #8285, #53848, #6132, #104744, #169721, #89568, #88492, #152413, #3992, #37591, #103673, #21311, #153484, #155617, #72201, #5055, #7202, #71130, #138309, #73275, #205410, #203268, #57050, #189178, #159881, #207551, #126398, #94904, #10415, #208607, #41890, #141545, #157761, #60239, #111201, #27747, #9361, #206484, #75433, #91712, #110135, #108001, #191293, #160955, #58114, #28819, #176147, #12545, #210755, #93843, #78620, #11486, #77558, #140472, #174028, #76487, #25599, #143681, #209673, #44016, #175084, #144744, #124273, #59171, #61317, #177205, #127477, #190231, #125330, #192358, #193448, #42959, #45092, #109068, #26671, #92775, #158819, #142597, #122854, #205043, #136877, #206121, #54548, #5757, #56687, #105462, #75068, #25239, #171496, #172578, #188815, #40449, #106551, #157401, #186670, #90262, #156330, #88119, #23087, #38297, #7914, #89202, #71836, #155255, #74001, #24159, #140094, #57751, #39365, #8993, #141181, #6837, #72915, #70763, #139020, #170421, #104375, #123911, #189878, #41521, #107633, #202903, #173665, #120695, #137945, #91341, #207190, #119613, #185598, #37229, #103300, #169362, #20947, #87044, #153116, #22009, #4688, #154189, #203967, #55613, #121768, #187737, #130731, #97119, #196724, #115529, #147987, #181524, #165282, #64592, #34208, #100281, #48364, #32092, #96053, #98178, #195667, #211890, #16876, #114477, #82957, #180475, #197771, #166347, #164226, #17938, #213997, #46230, #182585, #144823, #13695, #15814, #81899, #113416, #65617, #131767, #210830, #112347, #116591, #178359, #29967, #47302, #49408, #33152, #62455, #99233, #179423, #149030, #606, #66673, #162106, #31043, #80847 ),
 ( #129683, #145881, #132821, #198825, #50470, #79767, #128618, #63529, #163171, #14756, #146938, #184710, #55797, #150114, #138133, #87233, #121952, #171678, #4873, #204142, #137062, #54731, #84024, #1687, #20078, #133891, #37411, #70952, #119798, #118725, #154373, #39549, #67741, #103487, #170609, #153297, #199897, #22196, #19015, #151180, #187918, #68820, #105650, #134942, #36334, #202007, #2750, #51544, #117668, #168480, #101342, #169548, #85095, #72020, #88309, #3809, #183661, #152237, #200948, #167423, #35265, #52597, #86167, #186856, #102412, #69882, #5950, #135993, #53667, #21129, #203087, #120882, #38487, #104564, #23275, #10244, #206310, #107824, #24342, #40638, #123044, #208434, #156518, #57934, #188995, #27567, #158646, #42784, #111023, #89386, #141370, #106740, #59003, #41714, #108893, #207382, #205227, #8109, #44915, #92603, #174916, #73096, #26496, #209497, #124098, #60068, #109963, #7020, #125159, #155435, #90452, #142425, #75256, #61137, #76320, #74197, #127299, #140291, #191118, #192185, #175973, #91532, #190062, #193269, #173849, #25425, #43849, #157590, #126224, #9185, #93665, #159707, #11306, #77384, #139197, #56868, #114232, #177028, #128370, #30791, #213752, #96870, #178103, #195417, #212704, #64345, #179167, #130491, #162920, #165034, #211636, #29719, #15562, #181277, #13446, #32903, #95801, #45979, #210582, #79523, #194337, #112100, #80592, #358, #161857, #31853, #16627, #145641, #47047, #63272, #28645, #160778, #14500, #129434, #113163, #146688, #115286, #196478, #48120, #12371, #78451, #180230, #82710, #98981, #94732, #163987, #97929, #81649, #147736, #65374, #62213, #131521, #197524, #49168, #148788, #66430, #132573, #198576, #50223, #144569, #85920, #133644, #185534, #37162, #103240, #169300, #51291, #101087, #166101, #20884, #54488, #183413, #186610, #5695, #2499, #71772, #18763, #71521, #57431, #5442, #154937, #206866, #205800, #125712, #74751, #6521, #59553, #88883, #123592, #174405, #25982, #156003, #122529, #191673, #40122, #72598, #92090, #138698, #9736, #7590, #75811 ) ),
 .UNSPECIFIED., .F., .F., .T. ) 
 B_SPLINE_SURFACE_WITH_KNOTS ( ( 2, 2 ),
 ( 3, 2, 2, 2, 2, 2, 2, 2, 2, 2, 2, 2, 2, 2, 2, 2, 2, 2, 2, 2, 2, 2, 2, 2, 2, 2, 2, 2, 2, 2, 2, 2, 2, 2, 2, 2, 2, 2, 2, 2, 2, 2, 2, 2, 2, 2, 2, 2, 2, 2, 2, 2, 2, 2, 2, 2, 2, 2, 2, 2, 2, 2, 2, 2, 2, 2, 2, 2, 2, 2, 2, 2, 2, 2, 2, 2, 2, 2, 2, 2, 2, 2, 2, 2, 2, 2, 2, 2, 2, 2, 2, 2, 2, 2, 2, 2, 2, 2, 2, 2, 2, 2, 2, 2, 2, 2, 2, 2, 2, 2, 2, 2, 2, 2, 2, 2, 2, 2, 2, 2, 3 ),
 ( 0.000000000000000000, 1.000000000000000000 ),
 ( 0.000000000000000000, 0.008333333333333333218, 0.01666666666666666644, 0.02500000000000000139, 0.03333333333333333287, 0.04166666666666666435, 0.05000000000000000278, 0.05833333333333333426, 0.06666666666666666574, 0.07499999999999999722, 0.08333333333333332871, 0.09166666666666666019, 0.1000000000000000056, 0.1083333333333333370, 0.1166666666666666685, 0.1250000000000000000, 0.1333333333333333315, 0.1416666666666666630, 0.1499999999999999944, 0.1583333333333333259, 0.1666666666666666574, 0.1749999999999999889, 0.1833333333333333204, 0.1916666666666666796, 0.2000000000000000111, 0.2083333333333333426, 0.2166666666666666741, 0.2250000000000000056, 0.2333333333333333370, 0.2416666666666666685, 0.2500000000000000000, 0.2583333333333333592, 0.2666666666666666630, 0.2750000000000000222, 0.2833333333333333259, 0.2916666666666666852, 0.2999999999999999889, 0.3083333333333333481, 0.3166666666666666519, 0.3250000000000000111, 0.3333333333333333148, 0.3416666666666666741, 0.3499999999999999778, 0.3583333333333333370, 0.3666666666666666408, 0.3750000000000000000, 0.3833333333333333592, 0.3916666666666666630, 0.4000000000000000222, 0.4083333333333333259, 0.4166666666666666852, 0.4249999999999999889, 0.4333333333333333481, 0.4416666666666666519, 0.4500000000000000111, 0.4583333333333333148, 0.4666666666666666741, 0.4749999999999999778, 0.4833333333333333370, 0.4916666666666666408, 0.5000000000000000000, 0.5083333333333333037, 0.5166666666666667185, 0.5250000000000000222, 0.5333333333333333259, 0.5416666666666666297, 0.5500000000000000444, 0.5583333333333333481, 0.5666666666666666519, 0.5749999999999999556, 0.5833333333333333703, 0.5916666666666666741, 0.5999999999999999778, 0.6083333333333332815, 0.6166666666666666963, 0.6250000000000000000, 0.6333333333333333037, 0.6416666666666667185, 0.6500000000000000222, 0.6583333333333333259, 0.6666666666666666297, 0.6750000000000000444, 0.6833333333333333481, 0.6916666666666666519, 0.6999999999999999556, 0.7083333333333333703, 0.7166666666666666741, 0.7249999999999999778, 0.7333333333333332815, 0.7416666666666666963, 0.7500000000000000000, 0.7583333333333333037, 0.7666666666666667185, 0.7750000000000000222, 0.7833333333333333259, 0.7916666666666666297, 0.8000000000000000444, 0.8083333333333333481, 0.8166666666666666519, 0.8249999999999999556, 0.8333333333333333703, 0.8416666666666666741, 0.8499999999999999778, 0.8583333333333332815, 0.8666666666666666963, 0.8750000000000000000, 0.8833333333333333037, 0.8916666666666667185, 0.9000000000000000222, 0.9083333333333333259, 0.9166666666666666297, 0.9250000000000000444, 0.9333333333333333481, 0.9416666666666666519, 0.9499999999999999556, 0.9583333333333333703, 0.9666666666666666741, 0.9749999999999999778, 0.9833333333333332815, 0.9916666666666666963, 1.000000000000000000 ),
 .UNSPECIFIED. ) 
 GEOMETRIC_REPRESENTATION_ITEM ( )  RATIONAL_B_SPLINE_SURFACE ( (
 ( 1.000000000000000000, 0.8660254037844387076, 1.000000000000000000, 0.8660254037844387076, 1.000000000000000000, 0.8660254037844387076, 1.000000000000000000, 0.8660254037844387076, 1.000000000000000000, 0.8660254037844387076, 1.000000000000000000, 0.8660254037844387076, 1.000000000000000000, 0.8660254037844387076, 1.000000000000000000, 0.8660254037844387076, 1.000000000000000000, 0.8660254037844387076, 1.000000000000000000, 0.8660254037844387076, 1.000000000000000000, 0.8660254037844387076, 1.000000000000000000, 0.8660254037844387076, 1.000000000000000000, 0.8660254037844387076, 1.000000000000000000, 0.8660254037844387076, 1.000000000000000000, 0.8660254037844387076, 1.000000000000000000, 0.8660254037844387076, 1.000000000000000000, 0.8660254037844387076, 1.000000000000000000, 0.8660254037844387076, 1.000000000000000000, 0.8660254037844387076, 1.000000000000000000, 0.8660254037844387076, 1.000000000000000000, 0.8660254037844387076, 1.000000000000000000, 0.8660254037844387076, 1.000000000000000000, 0.8660254037844387076, 1.000000000000000000, 0.8660254037844387076, 1.000000000000000000, 0.8660254037844387076, 1.000000000000000000, 0.8660254037844387076, 1.000000000000000000, 0.8660254037844387076, 1.000000000000000000, 0.8660254037844387076, 1.000000000000000000, 0.8660254037844387076, 1.000000000000000000, 0.8660254037844387076, 1.000000000000000000, 0.8660254037844387076, 1.000000000000000000, 0.8660254037844387076, 1.000000000000000000, 0.8660254037844387076, 1.000000000000000000, 0.8660254037844387076, 1.000000000000000000, 0.8660254037844387076, 1.000000000000000000, 0.8660254037844387076, 1.000000000000000000, 0.8660254037844387076, 1.000000000000000000, 0.8660254037844387076, 1.000000000000000000, 0.8660254037844387076, 1.000000000000000000, 0.8660254037844387076, 1.000000000000000000, 0.8660254037844387076, 1.000000000000000000, 0.8660254037844387076, 1.000000000000000000, 0.8660254037844387076, 1.000000000000000000, 0.8660254037844387076, 1.000000000000000000, 0.8660254037844387076, 1.000000000000000000, 0.8660254037844387076, 1.000000000000000000, 0.8660254037844387076, 1.000000000000000000, 0.8660254037844387076, 1.000000000000000000, 0.8660254037844387076, 1.000000000000000000, 0.8660254037844387076, 1.000000000000000000, 0.8660254037844387076, 1.000000000000000000, 0.8660254037844387076, 1.000000000000000000, 0.8660254037844387076, 1.000000000000000000, 0.8660254037844387076, 1.000000000000000000, 0.8660254037844387076, 1.000000000000000000, 0.8660254037844387076, 1.000000000000000000, 0.8660254037844387076, 1.000000000000000000, 0.8660254037844387076, 1.000000000000000000, 0.8660254037844387076, 1.000000000000000000, 0.8660254037844387076, 1.000000000000000000, 0.8660254037844387076, 1.000000000000000000, 0.8660254037844387076, 1.000000000000000000, 0.8660254037844387076, 1.000000000000000000, 0.8660254037844387076, 1.000000000000000000, 0.8660254037844387076, 1.000000000000000000, 0.8660254037844387076, 1.000000000000000000, 0.8660254037844387076, 1.000000000000000000, 0.8660254037844387076, 1.000000000000000000, 0.8660254037844387076, 1.000000000000000000, 0.8660254037844387076, 1.000000000000000000, 0.8660254037844387076, 1.000000000000000000, 0.8660254037844387076, 1.000000000000000000, 0.8660254037844387076, 1.000000000000000000, 0.8660254037844387076, 1.000000000000000000, 0.8660254037844387076, 1.000000000000000000, 0.8660254037844387076, 1.000000000000000000, 0.8660254037844387076, 1.000000000000000000, 0.8660254037844387076, 1.000000000000000000, 0.8660254037844387076, 1.000000000000000000, 0.8660254037844387076, 1.000000000000000000, 0.8660254037844387076, 1.000000000000000000, 0.8660254037844387076, 1.000000000000000000, 0.8660254037844387076, 1.000000000000000000, 0.8660254037844387076, 1.000000000000000000, 0.8660254037844387076, 1.000000000000000000, 0.8660254037844387076, 1.000000000000000000, 0.8660254037844387076, 1.000000000000000000, 0.8660254037844387076, 1.000000000000000000, 0.8660254037844387076, 1.000000000000000000, 0.8660254037844387076, 1.000000000000000000, 0.8660254037844387076, 1.000000000000000000, 0.8660254037844387076, 1.000000000000000000, 0.8660254037844387076, 1.000000000000000000, 0.8660254037844387076, 1.000000000000000000, 0.8660254037844387076, 1.000000000000000000, 0.8660254037844387076, 1.000000000000000000, 0.8660254037844387076, 1.000000000000000000, 0.8660254037844387076, 1.000000000000000000, 0.8660254037844387076, 1.000000000000000000, 0.8660254037844387076, 1.000000000000000000, 0.8660254037844387076, 1.000000000000000000, 0.8660254037844387076, 1.000000000000000000, 0.8660254037844387076, 1.000000000000000000, 0.8660254037844387076, 1.000000000000000000, 0.8660254037844387076, 1.000000000000000000, 0.8660254037844387076, 1.000000000000000000, 0.8660254037844387076, 1.000000000000000000, 0.8660254037844387076, 1.000000000000000000, 0.8660254037844387076, 1.000000000000000000, 0.8660254037844387076, 1.000000000000000000, 0.8660254037844387076, 1.000000000000000000, 0.8660254037844387076, 1.000000000000000000, 0.8660254037844387076, 1.000000000000000000, 0.8660254037844387076, 1.000000000000000000, 0.8660254037844387076, 1.000000000000000000, 0.8660254037844387076, 1.000000000000000000, 0.8660254037844387076, 1.000000000000000000, 0.8660254037844387076, 1.000000000000000000, 0.8660254037844387076, 1.000000000000000000, 0.8660254037844387076, 1.000000000000000000),
 ( 1.000000000000000000, 0.8660254037844387076, 1.000000000000000000, 0.8660254037844387076, 1.000000000000000000, 0.8660254037844387076, 1.000000000000000000, 0.8660254037844387076, 1.000000000000000000, 0.8660254037844387076, 1.000000000000000000, 0.8660254037844387076, 1.000000000000000000, 0.8660254037844387076, 1.000000000000000000, 0.8660254037844387076, 1.000000000000000000, 0.8660254037844387076, 1.000000000000000000, 0.8660254037844387076, 1.000000000000000000, 0.8660254037844387076, 1.000000000000000000, 0.8660254037844387076, 1.000000000000000000, 0.8660254037844387076, 1.000000000000000000, 0.8660254037844387076, 1.000000000000000000, 0.8660254037844387076, 1.000000000000000000, 0.8660254037844387076, 1.000000000000000000, 0.8660254037844387076, 1.000000000000000000, 0.8660254037844387076, 1.000000000000000000, 0.8660254037844387076, 1.000000000000000000, 0.8660254037844387076, 1.000000000000000000, 0.8660254037844387076, 1.000000000000000000, 0.8660254037844387076, 1.000000000000000000, 0.8660254037844387076, 1.000000000000000000, 0.8660254037844387076, 1.000000000000000000, 0.8660254037844387076, 1.000000000000000000, 0.8660254037844387076, 1.000000000000000000, 0.8660254037844387076, 1.000000000000000000, 0.8660254037844387076, 1.000000000000000000, 0.8660254037844387076, 1.000000000000000000, 0.8660254037844387076, 1.000000000000000000, 0.8660254037844387076, 1.000000000000000000, 0.8660254037844387076, 1.000000000000000000, 0.8660254037844387076, 1.000000000000000000, 0.8660254037844387076, 1.000000000000000000, 0.8660254037844387076, 1.000000000000000000, 0.8660254037844387076, 1.000000000000000000, 0.8660254037844387076, 1.000000000000000000, 0.8660254037844387076, 1.000000000000000000, 0.8660254037844387076, 1.000000000000000000, 0.8660254037844387076, 1.000000000000000000, 0.8660254037844387076, 1.000000000000000000, 0.8660254037844387076, 1.000000000000000000, 0.8660254037844387076, 1.000000000000000000, 0.8660254037844387076, 1.000000000000000000, 0.8660254037844387076, 1.000000000000000000, 0.8660254037844387076, 1.000000000000000000, 0.8660254037844387076, 1.000000000000000000, 0.8660254037844387076, 1.000000000000000000, 0.8660254037844387076, 1.000000000000000000, 0.8660254037844387076, 1.000000000000000000, 0.8660254037844387076, 1.000000000000000000, 0.8660254037844387076, 1.000000000000000000, 0.8660254037844387076, 1.000000000000000000, 0.8660254037844387076, 1.000000000000000000, 0.8660254037844387076, 1.000000000000000000, 0.8660254037844387076, 1.000000000000000000, 0.8660254037844387076, 1.000000000000000000, 0.8660254037844387076, 1.000000000000000000, 0.8660254037844387076, 1.000000000000000000, 0.8660254037844387076, 1.000000000000000000, 0.8660254037844387076, 1.000000000000000000, 0.8660254037844387076, 1.000000000000000000, 0.8660254037844387076, 1.000000000000000000, 0.8660254037844387076, 1.000000000000000000, 0.8660254037844387076, 1.000000000000000000, 0.8660254037844387076, 1.000000000000000000, 0.8660254037844387076, 1.000000000000000000, 0.8660254037844387076, 1.000000000000000000, 0.8660254037844387076, 1.000000000000000000, 0.8660254037844387076, 1.000000000000000000, 0.8660254037844387076, 1.000000000000000000, 0.8660254037844387076, 1.000000000000000000, 0.8660254037844387076, 1.000000000000000000, 0.8660254037844387076, 1.000000000000000000, 0.8660254037844387076, 1.000000000000000000, 0.8660254037844387076, 1.000000000000000000, 0.8660254037844387076, 1.000000000000000000, 0.8660254037844387076, 1.000000000000000000, 0.8660254037844387076, 1.000000000000000000, 0.8660254037844387076, 1.000000000000000000, 0.8660254037844387076, 1.000000000000000000, 0.8660254037844387076, 1.000000000000000000, 0.8660254037844387076, 1.000000000000000000, 0.8660254037844387076, 1.000000000000000000, 0.8660254037844387076, 1.000000000000000000, 0.8660254037844387076, 1.000000000000000000, 0.8660254037844387076, 1.000000000000000000, 0.8660254037844387076, 1.000000000000000000, 0.8660254037844387076, 1.000000000000000000, 0.8660254037844387076, 1.000000000000000000, 0.8660254037844387076, 1.000000000000000000, 0.8660254037844387076, 1.000000000000000000, 0.8660254037844387076, 1.000000000000000000, 0.8660254037844387076, 1.000000000000000000, 0.8660254037844387076, 1.000000000000000000, 0.8660254037844387076, 1.000000000000000000, 0.8660254037844387076, 1.000000000000000000, 0.8660254037844387076, 1.000000000000000000, 0.8660254037844387076, 1.000000000000000000, 0.8660254037844387076, 1.000000000000000000, 0.8660254037844387076, 1.000000000000000000, 0.8660254037844387076, 1.000000000000000000, 0.8660254037844387076, 1.000000000000000000, 0.8660254037844387076, 1.000000000000000000, 0.8660254037844387076, 1.000000000000000000, 0.8660254037844387076, 1.000000000000000000, 0.8660254037844387076, 1.000000000000000000, 0.8660254037844387076, 1.000000000000000000, 0.8660254037844387076, 1.000000000000000000, 0.8660254037844387076, 1.000000000000000000, 0.8660254037844387076, 1.000000000000000000, 0.8660254037844387076, 1.000000000000000000, 0.8660254037844387076, 1.000000000000000000, 0.8660254037844387076, 1.000000000000000000, 0.8660254037844387076, 1.000000000000000000, 0.8660254037844387076, 1.000000000000000000, 0.8660254037844387076, 1.000000000000000000, 0.8660254037844387076, 1.000000000000000000, 0.8660254037844387076, 1.000000000000000000, 0.8660254037844387076, 1.000000000000000000) ) ) 
 REPRESENTATION_ITEM ( '' )  SURFACE ( )  );
#166938 = CARTESIAN_POINT ( 'NONE',  ( -6.577640801285370209, 7.702944352034914566, -1.199719254218452047 ) ) ;
#166939 = CARTESIAN_POINT ( 'NONE',  ( 4.966250736084032447, 8.070317005903060448, 1.090833899539983554 ) ) ;
#166940 = CARTESIAN_POINT ( 'NONE',  ( 4.763045971468515383, -2.015604388477490350, -0.05228862439247972116 ) ) ;
#166941 = CARTESIAN_POINT ( 'NONE',  ( 4.593604542485023146, -1.840816577468977533, -0.04244875611379012037 ) ) ;
#166942 = CARTESIAN_POINT ( 'NONE',  ( 0.07661050522435490506, 0.2583762315121455599, -1.746200777818290195 ) ) ;
#166943 = CARTESIAN_POINT ( 'NONE',  ( 2.508792734928457335, -0.8846401781386037388, -2.131589412884911106 ) ) ;
#166944 = CARTESIAN_POINT ( 'NONE',  ( 5.993586425693011144, 9.150212042353954800, -1.199719254218452047 ) ) ;
#166945 = CARTESIAN_POINT ( 'NONE',  ( 5.149776166300943814, 0.6834882490109328579, -2.050742609271530181 ) ) ;
#166947 = CARTESIAN_POINT ( 'NONE',  ( 8.121497709785879593, 9.433834401960398353, -1.199719254218445830 ) ) ;
#166946 = CARTESIAN_POINT ( 'NONE',  ( 3.415250174187448362, -1.861344788686780438, 0.7762291900053899241 ) ) ;
#166948 = CARTESIAN_POINT ( 'NONE',  ( 0.4681772292557941917, -1.829107974901639899, -0.6530565061142034056 ) ) ;
#166949 = CARTESIAN_POINT ( 'NONE',  ( -4.599240423533815125, 6.388866465587984322, 1.599625672291267398 ) ) ;
#166950 = EDGE_CURVE ( 'NONE', #117563, #212596, #91834, .T. ) ;
#166951 = PRODUCT_RELATED_PRODUCT_CATEGORY ( 'part', '', ( #107661 ) ) ;
#166952 = CARTESIAN_POINT ( 'NONE',  ( -9.586287156395091102, 15.23335157185452893, -7.218579095505596399 ) ) ;
#166953 = CARTESIAN_POINT ( 'NONE',  ( -6.005335696210345020, 5.970922831858983315, 0.7998128361456281477 ) ) ;
#166954 = CARTESIAN_POINT ( 'NONE',  ( 3.660894226558962128, -1.649352935060313552, -0.8826137995501317501 ) ) ;
#166955 = AXIS2_PLACEMENT_3D ( 'NONE', #190123, #80387, #141434 ) ;
#166958 = CARTESIAN_POINT ( 'NONE',  ( -6.784929528996132220, 6.880448970109080520, 0.000000000000000000 ) ) ;
#166957 = CARTESIAN_POINT ( 'NONE',  ( 0.7499999999999867883, -1.152083332650516434, -1.299038105676652011 ) ) ;
#166956 = CARTESIAN_POINT ( 'NONE',  ( 1.107505169401588274, 1.450017293480215352, 1.247013401884336403 ) ) ;
#166959 = CARTESIAN_POINT ( 'NONE',  ( 2.754729969050898841, 0.7443088323898851000, 2.077706851784946185 ) ) ;
#166960 = CARTESIAN_POINT ( 'NONE',  ( -2.093037498677872144, 1.000000000000000888, 11.70868840297834446 ) ) ;
#166961 = CARTESIAN_POINT ( 'NONE',  ( 4.542145155778077203, 5.257923088951247159, -1.199719254218452047 ) ) ;
#166962 = CARTESIAN_POINT ( 'NONE',  ( 7.309254211098760834, 8.660456346770972758, 1.082531754730549967 ) ) ;
#166963 = CARTESIAN_POINT ( 'NONE',  ( -3.924195396151603177, 6.665646164563756138, 1.199719254218464037 ) ) ;
#166964 = CARTESIAN_POINT ( 'NONE',  ( -5.899206235277530297, 9.896508017883515862, 0.7216878364870267237 ) ) ;
#166965 = CARTESIAN_POINT ( 'NONE',  ( 0.1749903794560749015, 0.004523422195312763391, -1.955468523092759536 ) ) ;
#166966 = CARTESIAN_POINT ( 'NONE',  ( 6.410760325301650298, 1.714854236211732941, -1.544436965994408828 ) ) ;
#166967 = CARTESIAN_POINT ( 'NONE',  ( 1.117545225965112188, 0.3861695934333775337, -1.923310697798483293 ) ) ;
#166968 = CARTESIAN_POINT ( 'NONE',  ( 4.047761193102417110, 1.490534549623608873, 1.425871689066391168 ) ) ;
#166969 = CARTESIAN_POINT ( 'NONE',  ( 4.500943810056890371, 8.194925511800951412, -0.7216878364870207285 ) ) ;
#166970 = CARTESIAN_POINT ( 'NONE',  ( 5.345657705538078730, 9.458627433094950021, 0.7998128361456331437 ) ) ;
#166971 = ORIENTED_EDGE ( 'NONE', *, *, #175161, .F. ) ;
#166972 = CARTESIAN_POINT ( 'NONE',  ( 7.958272981097359811, 9.347368568444167636, -1.082531754730537976 ) ) ;
#166973 = CARTESIAN_POINT ( 'NONE',  ( 1.364683531249988535, 4.176041667008081326, 0.7879004041258500513 ) ) ;
#166974 = FACE_OUTER_BOUND ( 'NONE', #187732, .T. ) ;
#166975 = CARTESIAN_POINT ( 'NONE',  ( 5.300874872818843286, 5.286701561151180506, 0.7216878364870317197 ) ) ;
#166976 = CARTESIAN_POINT ( 'NONE',  ( 6.320782530974223157, -1.539933897815339403, 1.530818809132200142 ) ) ;
#166978 = CARTESIAN_POINT ( 'NONE',  ( 6.216338285296751920, 1.720575329815833943, 0.6561210673821931127 ) ) ;
#166977 = CARTESIAN_POINT ( 'NONE',  ( 9.617648866954041864, -9.063431457505050304, -0.6035590660245153671 ) ) ;
#166979 = CARTESIAN_POINT ( 'NONE',  ( -5.015689319493858100, 6.483061930202996592, 1.345460504475339159 ) ) ;
#166980 = CARTESIAN_POINT ( 'NONE',  ( -10.42522259430890763, 5.087348912241797194, -5.944660150690117106 ) ) ;
#166981 = CARTESIAN_POINT ( 'NONE',  ( 1.862360739135361376, -1.326353699019737098, 1.319252464149045734 ) ) ;
#166983 = CARTESIAN_POINT ( 'NONE',  ( -5.926191280687664431, 6.129739482751896062, 0.8152664440823562675 ) ) ;
#166982 = AXIS2_PLACEMENT_3D ( 'NONE', #152954, #4529, #86887 ) ;
#166984 = FACE_OUTER_BOUND ( 'NONE', #126344, .T. ) ;
#166985 = CARTESIAN_POINT ( 'NONE',  ( 5.413027408713817046, 7.651055653456078076, -1.328921179265474262 ) ) ;
#166986 = CARTESIAN_POINT ( 'NONE',  ( -0.6823417656249969321, 4.780208333674755394, -1.181850606188749264 ) ) ;
#166987 = CARTESIAN_POINT ( 'NONE',  ( 1.119614361207950548, -0.4638517909370845071, 1.855054000551699778 ) ) ;
#166988 = CARTESIAN_POINT ( 'NONE',  ( 3.115802406598367824, -0.8709184464271730874, -1.540630773470308190 ) ) ;
#166989 = CARTESIAN_POINT ( 'NONE',  ( 0.3110002902955294468, 1.589785527739733695, -1.062417771062994287 ) ) ;
#166991 = CARTESIAN_POINT ( 'NONE',  ( 4.569893716599374933, -0.8992288252529623271, 1.691407037985042772 ) ) ;
#166990 = CARTESIAN_POINT ( 'NONE',  ( 1.429488589276664001, -3.154214574430208806, -3.050286313710991681 ) ) ;
#166992 = DIRECTION ( 'NONE',  ( 0.000000000000000000, 8.546850786086437571E-32, 1.000000000000000000 ) ) ;
#166993 = CARTESIAN_POINT ( 'NONE',  ( 5.758249387092365446, -1.969739562807392819, -0.001740234774137705337 ) ) ;
#166994 = CARTESIAN_POINT ( 'NONE',  ( 0.7211286721200690364, 1.601891702520108485, -1.389630591760198541 ) ) ;
#166995 = DIRECTION ( 'NONE',  ( 1.000000000000000000, 1.725633230170963762E-31, 8.638326563840814399E-31 ) ) ;
#166996 = CARTESIAN_POINT ( 'NONE',  ( 4.276139911362797363, -1.077190196239918851, 1.529178877381555335 ) ) ;
#166998 = ORIENTED_EDGE ( 'NONE', *, *, #109767, .F. ) ;
#166997 = CARTESIAN_POINT ( 'NONE',  ( 0.5217476098421744979, -0.9739702522407606144, -1.544006022310390192 ) ) ;
#167000 = CARTESIAN_POINT ( 'NONE',  ( -1.945152801660234188, -0.4725272983825999917, 0.7134944055886121017 ) ) ;
#166999 = CARTESIAN_POINT ( 'NONE',  ( 3.264504910713565078, 0.9923201075644829672, 1.971275125648555449 ) ) ;
#167001 = CARTESIAN_POINT ( 'NONE',  ( -1.364683531250012516, 4.801041667008083991, -0.7879004041258300672 ) ) ;
#167002 = CARTESIAN_POINT ( 'NONE',  ( 0.6606829430093235089, -0.6931630328321845003, -1.942862509804524906 ) ) ;
#167003 = CARTESIAN_POINT ( 'NONE',  ( 7.786460292950004636, 7.978625184730144149, 1.040834085586084257E-14 ) ) ;
#167004 = CARTESIAN_POINT ( 'NONE',  ( -7.994504133552415404, 12.47867192245318435, -0.7998128361456281477 ) ) ;
#167005 = DIRECTION ( 'NONE',  ( 0.000000000000000000, -1.000000000000000000, -6.661338147750945159E-16 ) ) ;
#167006 = CARTESIAN_POINT ( 'NONE',  ( -3.424659329065677493, -0.02067678355765355941, -0.4189035560211199494 ) ) ;
#167007 = CARTESIAN_POINT ( 'NONE',  ( 5.833751235630055376, 10.02806988486892514, 0.7998128361456331437 ) ) ;
#167008 = ORIENTED_EDGE ( 'NONE', *, *, #175161, .T. ) ;
#167009 = CARTESIAN_POINT ( 'NONE',  ( 3.314952806421948672, -1.569539724514938950, 1.350292352848787569 ) ) ;
#167010 = CARTESIAN_POINT ( 'NONE',  ( -1.500000000000011324, 3.920833333333357817, 0.8660254037844403729 ) ) ;
#167011 = CARTESIAN_POINT ( 'NONE',  ( 1.317891493549529391, -2.109231647155560108, 0.4722262556789079135 ) ) ;
#167012 = CARTESIAN_POINT ( 'NONE',  ( -6.510788175286835511, 6.826513026331759271, 0.5708727117093035375 ) ) ;
#167013 = CARTESIAN_POINT ( 'NONE',  ( 2.438154291397228501, -1.164718066671111885, -1.649793688766809430 ) ) ;
#167014 = CARTESIAN_POINT ( 'NONE',  ( 5.484430959185961463, 6.043327615839654499, 0.8208683321978844649 ) ) ;
#167016 = CARTESIAN_POINT ( 'NONE',  ( 7.293923454472069245, 11.45340176361870199, 0.7216878364870438212 ) ) ;
#167015 = CARTESIAN_POINT ( 'NONE',  ( -1.737499999999997824, -3.791666666666665186, 3.009438278150925683 ) ) ;
#167017 = DIRECTION ( 'NONE',  ( 1.000000000000000000, 0.000000000000000000, 8.638326563840826660E-31 ) ) ;
#167018 = CARTESIAN_POINT ( 'NONE',  ( 0.6379081216283178923, 2.014007883293071899, -0.1037844182863178755 ) ) ;
#167019 = CARTESIAN_POINT ( 'NONE',  ( 5.284801750429747536, 1.933107837519608685, -1.032524723389722787 ) ) ;
#167020 = CARTESIAN_POINT ( 'NONE',  ( 1.499999999999987121, 3.827083334016153415, -0.8660254037844323793 ) ) ;
#167021 = CARTESIAN_POINT ( 'NONE',  ( 3.234525475359388391, 1.209690070866603406, -1.481213593849866728 ) ) ;
#167022 = CARTESIAN_POINT ( 'NONE',  ( -5.579343907223557331, 6.467988298970945849, 1.199719254218450271 ) ) ;
#167023 = CARTESIAN_POINT ( 'NONE',  ( 4.487385655998885170, 5.298000022495898520, 1.082531754730560403 ) ) ;
#167025 = CARTESIAN_POINT ( 'NONE',  ( 0.8257962581623284892, 0.8146080751335778025, -1.844719337431327544 ) ) ;
#167024 = CARTESIAN_POINT ( 'NONE',  ( -9.232739420781982176, 12.75498451001223010, 1.082531754730558626 ) ) ;
#167026 = CARTESIAN_POINT ( 'NONE',  ( 0.6823417656249934904, 11.75520833367473017, 1.181850606188764807 ) ) ;
#167028 = CARTESIAN_POINT ( 'NONE',  ( -4.281342646865346602, 8.216926531310035031, 0.7998128361456352531 ) ) ;
#167027 = CARTESIAN_POINT ( 'NONE',  ( 0.6621918981609349331, 1.136352663792916662, 1.990853321008963395 ) ) ;
#167029 = CARTESIAN_POINT ( 'NONE',  ( 4.471539400256457242, 1.672567520934200136, -0.4206060815013599741 ) ) ;
#167030 = DIRECTION ( 'NONE',  ( 0.000000000000000000, 0.000000000000000000, 1.000000000000000000 ) ) ;
#167031 = CARTESIAN_POINT ( 'NONE',  ( 4.847203612085560387, 5.613824621309978724, -1.199719254218452047 ) ) ;
#167032 = CARTESIAN_POINT ( 'NONE',  ( 11.86686399458719698, 11.10928729775336876, 1.056461745586970258 ) ) ;
#167033 = CARTESIAN_POINT ( 'NONE',  ( 1.627322669196319849, 0.1476378700930695564, -1.956383933670035713 ) ) ;
#167034 = DIRECTION ( 'NONE',  ( -0.6250000000000005551, 0.000000000000000000, 0.7806247497997993445 ) ) ;
#167035 = CARTESIAN_POINT ( 'NONE',  ( 4.680589345215795838, 6.483773540883647435, -1.599625672291256295 ) ) ;
#167036 = CARTESIAN_POINT ( 'NONE',  ( 0.1755611466353629579, -0.002217706044341584935, -2.244164702216360219 ) ) ;
#167037 = EDGE_LOOP ( 'NONE', ( #148358, #16664, #39060, #7962, #91651 ) ) ;
#167039 = CIRCLE ( 'NONE', #28658, 0.5000000000000007772 ) ;
#167038 = CARTESIAN_POINT ( 'NONE',  ( 0.4091448426733998445, -1.664836780672280803, 1.230395522420649979 ) ) ;
#167040 = ORIENTED_EDGE ( 'NONE', *, *, #18222, .F. ) ;
#167041 = CARTESIAN_POINT ( 'NONE',  ( 4.072783076529101542, -1.339505953097392066, 1.219664821550008549 ) ) ;
#167042 = ORIENTED_EDGE ( 'NONE', *, *, #109079, .T. ) ;
#167044 = CARTESIAN_POINT ( 'NONE',  ( 6.717138760927786834, 6.801359740696030443, -0.7998128361456481317 ) ) ;
#167043 = MECHANICAL_DESIGN_GEOMETRIC_PRESENTATION_REPRESENTATION (  '', ( #125527 ), #139368 ) ;
#167045 = LINE ( 'NONE', #151866, #174242 ) ;
#167046 = CARTESIAN_POINT ( 'NONE',  ( 5.127533414443554705, -0.2600442617171055404, 1.792572003776324197 ) ) ;
#167047 = CARTESIAN_POINT ( 'NONE',  ( 5.031484404002867450, 8.884165881396448583, 0.7216878364870317197 ) ) ;
#167048 = SURFACE_SIDE_STYLE ('',( #34885 ) ) ;
#167049 = CARTESIAN_POINT ( 'NONE',  ( 5.645731234294472323, 6.129814942853209381, -0.7970442531908157324 ) ) ;
#167051 = CARTESIAN_POINT ( 'NONE',  ( 8.530051201292206287, 13.10347683481629488, 0.000000000000000000 ) ) ;
#167050 = CARTESIAN_POINT ( 'NONE',  ( 5.898848723475273559, 0.3636257040535681995, 1.824992291636283293 ) ) ;
#167052 = CARTESIAN_POINT ( 'NONE',  ( 3.831564657165886789, 0.6421465917123435618, -1.804920456748728474 ) ) ;
#167053 = CARTESIAN_POINT ( 'NONE',  ( -0.3000000000000103140, 3.372708439410163184, -0.5000000000000056621 ) ) ;
#167054 = CARTESIAN_POINT ( 'NONE',  ( -11.87992086682929660, 5.100687730227392969, -4.764507118098673111 ) ) ;
#167055 = EDGE_CURVE ( 'NONE', #23394, #212524, #212867, .T. ) ;
#167056 = PLANE ( 'NONE',  #11839 ) ;
#167057 = CARTESIAN_POINT ( 'NONE',  ( -0.6823417656250246877, -0.9489583329919115684, 1.181850606188755259 ) ) ;
#167058 = CARTESIAN_POINT ( 'NONE',  ( 5.504247177468175600, 8.405076892812779477, 1.082531754730558626 ) ) ;
#167059 = CARTESIAN_POINT ( 'NONE',  ( -2.764973262183167968, 5.313220341600567664, 1.199719254218462483 ) ) ;
#167060 = CARTESIAN_POINT ( 'NONE',  ( 1.253037233087474611, -1.703760181015579134, 1.330383891403746688 ) ) ;
#167061 = CARTESIAN_POINT ( 'NONE',  ( -6.473091995881817162, 6.516638514809040217, 0.7998128361456281477 ) ) ;
#167062 = CARTESIAN_POINT ( 'NONE',  ( 4.030516805012513082, 7.924296382481737844, 0.000000000000000000 ) ) ;
#167063 = CARTESIAN_POINT ( 'NONE',  ( 0.3932109892899987580, 1.349039491128176449, 1.230163767592551638 ) ) ;
#167064 = CARTESIAN_POINT ( 'NONE',  ( -4.283486466913726254, 7.084819080452935403, -1.199719254218452047 ) ) ;
#167065 = CARTESIAN_POINT ( 'NONE',  ( 3.856323340278215550, 0.6566615474184741563, 1.703573633380930374 ) ) ;
#167066 = CARTESIAN_POINT ( 'NONE',  ( 12.43309052428753070, 7.572468744233063376, 1.895192891247173606 ) ) ;
#167067 = CARTESIAN_POINT ( 'NONE',  ( 1.582132296805271787, 0.9858968508435607125, 1.638552900098678045 ) ) ;
#167068 = ORIENTED_EDGE ( 'NONE', *, *, #151730, .T. ) ;
#167069 = CARTESIAN_POINT ( 'NONE',  ( 2.207411625193840266, -1.579985490969371575, -1.175680343436244391 ) ) ;
#167070 = CARTESIAN_POINT ( 'NONE',  ( 5.038593826026604994, -1.663644762202406646, 1.001748047271956876 ) ) ;
#167071 = CARTESIAN_POINT ( 'NONE',  ( -3.546339698426324460, 6.295090860542775779, -1.199719254218450271 ) ) ;
#167073 = CARTESIAN_POINT ( 'NONE',  ( 4.271814301144261528, 0.4616217191124799002, -2.069597271375968273 ) ) ;
#167072 = CARTESIAN_POINT ( 'NONE',  ( 5.096939404094710468, 4.911127157724081371, 0.000000000000000000 ) ) ;
#167075 = EDGE_CURVE ( 'NONE', #78493, #168244, #21304, .T. ) ;
#167074 = CARTESIAN_POINT ( 'NONE',  ( 4.913904330310220558, 4.697586238308844919, 0.000000000000000000 ) ) ;
#167076 = CARTESIAN_POINT ( 'NONE',  ( 9.610031953988080744, 10.10612545594124967, -0.7998128361456281477 ) ) ;
#167077 = CARTESIAN_POINT ( 'NONE',  ( 6.078105975125470017, 6.038708432876411791, -0.3507111650211444109 ) ) ;
#167078 = DIRECTION ( 'NONE',  ( -1.000000000000000000, 0.000000000000000000, 2.345077562848782505E-16 ) ) ;
#167079 = ORIENTED_EDGE ( 'NONE', *, *, #112471, .F. ) ;
#167080 = CARTESIAN_POINT ( 'NONE',  ( -0.6823417656250039265, 13.06770833367473017, -1.181850606188755259 ) ) ;
#167081 = CARTESIAN_POINT ( 'NONE',  ( 5.337069745634900997, 6.255611453776062980, 1.199719254218452047 ) ) ;
#167082 = VECTOR ( 'NONE', #1533, 1000.000000000000000 ) ;
#167083 = CARTESIAN_POINT ( 'NONE',  ( 6.737475991348287785, 6.825086509519945999, -0.7998128361456481317 ) ) ;
#167084 = CARTESIAN_POINT ( 'NONE',  ( 11.86145017354043674, 12.59514365543877012, -1.100000000000000533 ) ) ;
#167085 = CARTESIAN_POINT ( 'NONE',  ( 5.514214477338500231, -0.8245889995748825196, -1.628937154514856545 ) ) ;
#167086 = CARTESIAN_POINT ( 'NONE',  ( -5.427790276013078952, 4.356734706464544971, 2.440341524156858455 ) ) ;
#167087 = CARTESIAN_POINT ( 'NONE',  ( -7.809133291791416909, 11.09411069285655493, 1.082531754730549967 ) ) ;
#167088 = CARTESIAN_POINT ( 'NONE',  ( -6.239605170154193026, 7.010755437975583426, 1.009914170685573875 ) ) ;
#167089 = CARTESIAN_POINT ( 'NONE',  ( 6.925078400183577010, 7.053014648177382995, 2.453806744102948745 ) ) ;
#167090 = CARTESIAN_POINT ( 'NONE',  ( 6.139502064137229986, -1.356240498024411600, -1.288626068300227523 ) ) ;
#167091 = CARTESIAN_POINT ( 'NONE',  ( 6.642605195691581699, 9.837124264027149678, 1.199719254218462483 ) ) ;
#167092 = CARTESIAN_POINT ( 'NONE',  ( 2.719263968888342653, -0.1887435353777958125, 1.917229668948018162 ) ) ;
#167093 = CARTESIAN_POINT ( 'NONE',  ( -5.461236948206311226, 5.265864615862458464, 0.7998128361456341429 ) ) ;
#167094 = CARTESIAN_POINT ( 'NONE',  ( 5.027376032568989572, 4.759693547618927489, 0.7998128361456341429 ) ) ;
#167095 = CARTESIAN_POINT ( 'NONE',  ( -1.364683531250000748, 8.921875000341403350, 0.000000000000000000 ) ) ;
#167096 = CARTESIAN_POINT ( 'NONE',  ( -4.924636110261798372, 6.768494766770632332, 1.599625672291267398 ) ) ;
#167097 = CARTESIAN_POINT ( 'NONE',  ( 2.659370686574860976, 6.254349567645977714, -0.7998128361456291469 ) ) ;
#167098 = CARTESIAN_POINT ( 'NONE',  ( -6.474900878978163021, 9.711745571186627402, -1.199719254218452047 ) ) ;
#167099 = AXIS2_PLACEMENT_3D ( 'NONE', #79791, #145905, #15838 ) ;
#167100 = CIRCLE ( 'NONE', #73704, 2.324999999999998845 ) ;
#167101 = ADVANCED_FACE ( 'NONE', ( #95964 ), #89275, .T. ) ;
#167102 = CARTESIAN_POINT ( 'NONE',  ( 1.529080078018136390, -1.786526079506415288, 1.135962973836294854 ) ) ;
#167103 = CARTESIAN_POINT ( 'NONE',  ( 8.378048858240820351, 11.86180853700128601, -1.199719254218446718 ) ) ;
#167104 = CARTESIAN_POINT ( 'NONE',  ( -6.178787966739591297, 5.309377612922442147, 2.438151698559690939 ) ) ;
#167105 = CARTESIAN_POINT ( 'NONE',  ( 5.998901810315326877, 0.3981486965325408134, 2.031442706791640074 ) ) ;
#167107 = CARTESIAN_POINT ( 'NONE',  ( 4.088248116760357931, 7.710168519003287813, -0.6407031029972446445 ) ) ;
#167106 = CARTESIAN_POINT ( 'NONE',  ( 1.768857366986800184, 1.761637791510446860, -0.5354853023365884201 ) ) ;
#167108 = CARTESIAN_POINT ( 'NONE',  ( 4.961921032921539521, 7.772363057508363759, -1.082531754730549078 ) ) ;
#167110 =( NAMED_UNIT ( * ) PLANE_ANGLE_UNIT ( ) SI_UNIT ( $, .RADIAN. ) );
#167109 = CARTESIAN_POINT ( 'NONE',  ( 3.851925040058331806, 5.587274861525073355, -1.443375672974066548 ) ) ;
#167111 = CARTESIAN_POINT ( 'NONE',  ( 1.693750089093534861, -0.7690282282955845927, 2.159540072747981654 ) ) ;
#167112 = CARTESIAN_POINT ( 'NONE',  ( -7.006746397889327405, 6.052176462752765218, 2.500000000000000000 ) ) ;
#167113 = VERTEX_POINT ( 'NONE', #177788 ) ;
#167114 = CARTESIAN_POINT ( 'NONE',  ( 7.578644679914702031, 10.82520731233375955, 1.082531754730558626 ) ) ;
#167115 = CARTESIAN_POINT ( 'NONE',  ( 0.5275904727545431827, -0.2913634075805496271, 1.991877199276798516 ) ) ;
#167116 = CARTESIAN_POINT ( 'NONE',  ( 0.8132426064601482318, -1.654215606812576400, -1.054277637385622857 ) ) ;
#167117 = CARTESIAN_POINT ( 'NONE',  ( -9.110189153378817295, 12.71597221466224603, 1.199719254218462483 ) ) ;
#167119 = CARTESIAN_POINT ( 'NONE',  ( 6.639320575229252341, 0.005161017367553630275, 1.896863882003448021 ) ) ;
#167118 = CARTESIAN_POINT ( 'NONE',  ( -9.176171038350775078, 9.599954387697719582, -0.7998128361456291469 ) ) ;
#167120 = CARTESIAN_POINT ( 'NONE',  ( 3.285556943750000514, -0.7510416661887079348, 1.896917185911906500 ) ) ;
#167122 = CARTESIAN_POINT ( 'NONE',  ( 1.885279724593362793, 1.217781634009064806, 1.284517237999055039 ) ) ;
#167121 = CARTESIAN_POINT ( 'NONE',  ( 3.714856679239968873, -0.1534820204720024339, 2.085054752100850894 ) ) ;
#167123 = CARTESIAN_POINT ( 'NONE',  ( -10.94245301910280865, 3.162178953954597471, 3.962121973755150073 ) ) ;
#167125 = CARTESIAN_POINT ( 'NONE',  ( 4.910265066218413743, 1.583196867009181608, -1.657922308084827545 ) ) ;
#167124 = CARTESIAN_POINT ( 'NONE',  ( 3.469446951953614189E-15, 5.229711127717882491, 1.214306433183764966E-14 ) ) ;
#167126 = CARTESIAN_POINT ( 'NONE',  ( 2.853125853291237579, 1.731928873650347311, -0.1707260732264591074 ) ) ;
#167127 = COLOUR_RGB ( '', 0.08235294, 0.09019608, 0.10196078) ;
#167128 = CARTESIAN_POINT ( 'NONE',  ( 3.999819011231439347, 4.625209253646830554, 1.199719254218464037 ) ) ;
#167129 = CARTESIAN_POINT ( 'NONE',  ( 6.222266154028957885, 6.224008365980749247, 0.7998128361456350310 ) ) ;
#167130 = CARTESIAN_POINT ( 'NONE',  ( 3.215853349543820183, -1.415750056632815168, -1.000566135699741066 ) ) ;
#167131 = CARTESIAN_POINT ( 'NONE',  ( 3.174467775116470936, -1.067885509202262773, -1.890316989176257234 ) ) ;
#167132 = CARTESIAN_POINT ( 'NONE',  ( 5.335297142177534369, 6.183267073083954735, -1.199719254218452047 ) ) ;
#167133 = CARTESIAN_POINT ( 'NONE',  ( 4.698454014923811428, 1.387101836239763131, -1.463925544105355803 ) ) ;
#167134 = CARTESIAN_POINT ( 'NONE',  ( 6.531249988543854634, -0.7852927567036558365, -1.895863743163934245 ) ) ;
#167135 = CARTESIAN_POINT ( 'NONE',  ( -1.499999999999997780, 3.931250000682819046, 1.214306433183764966E-14 ) ) ;
#167136 = CARTESIAN_POINT ( 'NONE',  ( 2.414956338186133422, 1.719780681555121982, 0.8681123839546500687 ) ) ;
#167137 = CARTESIAN_POINT ( 'NONE',  ( 0.6823417656249969321, 15.27604166700806410, -1.181850606188757036 ) ) ;
#167138 = CARTESIAN_POINT ( 'NONE',  ( 5.344044365905453731, -1.409322151232726750, -1.717068368634220299 ) ) ;
#167139 = VERTEX_POINT ( 'NONE', #145325 ) ;
#167140 = CARTESIAN_POINT ( 'NONE',  ( -0.1108833634137010304, 0.2458664895051872190, -1.931623620491630611 ) ) ;
#167141 = CARTESIAN_POINT ( 'NONE',  ( -0.7500000000000215383, 1.691666666666688634, 1.299038105676659116 ) ) ;
#167142 = CARTESIAN_POINT ( 'NONE',  ( 5.503720292143644777, 8.508425209887878538, 1.199719254218462483 ) ) ;
#167143 = CARTESIAN_POINT ( 'NONE',  ( 5.802526556524483681, 5.871961858807763335, 1.040834085586084257E-14 ) ) ;
#167144 = CARTESIAN_POINT ( 'NONE',  ( -0.4577034257980932552, -0.8887487162305418575, -3.253519940713586855 ) ) ;
#167145 = CARTESIAN_POINT ( 'NONE',  ( 6.004347769543215030, 1.959566550440184907, 0.09775035808561728656 ) ) ;
#167146 = CARTESIAN_POINT ( 'NONE',  ( 9.436111725431318931, 10.11114455586577776, -0.7216878364870257245 ) ) ;
#167147 = CARTESIAN_POINT ( 'NONE',  ( 0.4598555752060234925, 3.132870877575693935, 1.947419802861296123 ) ) ;
#167148 = CARTESIAN_POINT ( 'NONE',  ( 6.889870058830950938, -0.9756824853745720283, 2.038933460117636542 ) ) ;
#167149 = CARTESIAN_POINT ( 'NONE',  ( 5.391302360089590628, 6.318882837306503575, -1.199719254218452047 ) ) ;
#167150 = CARTESIAN_POINT ( 'NONE',  ( -3.499413046103020175, 7.096749297179887783, 0.7216878364870338292 ) ) ;
#167151 = CARTESIAN_POINT ( 'NONE',  ( 3.930177659428602865, 1.143423634368987196, 1.716560605327678513 ) ) ;
#167152 = CARTESIAN_POINT ( 'NONE',  ( -5.091250377131585125, 5.898545847196970726, 1.199719254218450271 ) ) ;
#167153 = CARTESIAN_POINT ( 'NONE',  ( 1.499999999999987121, 4.077083334016147198, -0.8660254037844323793 ) ) ;
#167154 = CARTESIAN_POINT ( 'NONE',  ( 0.6823417656249882723, -0.3239583329919110133, -1.181850606188749264 ) ) ;
#167155 = CARTESIAN_POINT ( 'NONE',  ( 6.309813054293936574, -1.856383540575656799, 0.2289572138471432372 ) ) ;
#167156 = CARTESIAN_POINT ( 'NONE',  ( 4.342224273253515676, 0.3742292800460333413, -1.693095411864028677 ) ) ;
#167157 = CARTESIAN_POINT ( 'NONE',  ( 4.704519267438088015, 1.517481324781422503, 0.8521212890505409643 ) ) ;
#167158 = CARTESIAN_POINT ( 'NONE',  ( 8.703971429848968100, 13.09845773489176679, 0.000000000000000000 ) ) ;
#167159 = CARTESIAN_POINT ( 'NONE',  ( 2.244040508683461166, 2.291928982054102004, 0.05232369179298743123 ) ) ;
#167160 = CARTESIAN_POINT ( 'NONE',  ( -1.364683531250012516, 3.592708333674750509, 0.7879004041258379498 ) ) ;
#167161 = CARTESIAN_POINT ( 'NONE',  ( 5.706606250695148042, 1.844387978369428582, 0.9845570724962575682 ) ) ;
#167162 = CARTESIAN_POINT ( 'NONE',  ( 0.5328340850149284602, -1.300071877079148841, -1.303948673260245439 ) ) ;
#167163 = DIRECTION ( 'NONE',  ( -3.347138415753902517E-16, -0.6000000000000018652, -0.7999999999999984901 ) ) ;
#167164 =( NAMED_UNIT ( * ) PLANE_ANGLE_UNIT ( ) SI_UNIT ( $, .RADIAN. ) );
#167165 = CARTESIAN_POINT ( 'NONE',  ( 1.459611520199757706, -1.915600648959712382, -0.6298732728240025169 ) ) ;
#167166 = CARTESIAN_POINT ( 'NONE',  ( 0.3401085955914602277, 2.185883683461706362, 0.1570275565265024931 ) ) ;
#167167 = CARTESIAN_POINT ( 'NONE',  ( 9.027736952715539331, 13.49050362732109143, -9.153502459270221436 ) ) ;
#167168 = CARTESIAN_POINT ( 'NONE',  ( -6.340409392685171674, 10.54889472477470846, 0.7998128361456481317 ) ) ;
#167169 = CARTESIAN_POINT ( 'NONE',  ( 5.738125327081736060, 7.717565519727259904, 1.599625672291267398 ) ) ;
#167170 = CARTESIAN_POINT ( 'NONE',  ( 4.090573159264241809, -1.219870178150096462, 1.734285844867427651 ) ) ;
#167171 = CARTESIAN_POINT ( 'NONE',  ( -1.364683531250000748, -0.9906249996585805295, 0.000000000000000000 ) ) ;
#167172 = CARTESIAN_POINT ( 'NONE',  ( 6.006453938882227561, -0.6616566355047011072, -1.701761020394356283 ) ) ;
#167173 = VERTEX_POINT ( 'NONE', #143194 ) ;
#167174 = CARTESIAN_POINT ( 'NONE',  ( -6.119526231721793330, 8.232809585132461194, 1.599625672291263179 ) ) ;
#167175 = CARTESIAN_POINT ( 'NONE',  ( 3.285556943749998737, -1.042708332855377451, -1.896917185911906500 ) ) ;
#167176 = CARTESIAN_POINT ( 'NONE',  ( -4.543954038874438162, 8.453030145328826350, 1.040834085586084257E-14 ) ) ;
#167177 = CARTESIAN_POINT ( 'NONE',  ( 3.586198609924298175, 1.125526462575956010, 1.676902781687271915 ) ) ;
#167178 = CARTESIAN_POINT ( 'NONE',  ( 6.405322867445039314, 1.831175526881479776, 1.231239259074583092 ) ) ;
#167179 = CARTESIAN_POINT ( 'NONE',  ( -2.986538976760251263, 6.706322249520737522, -0.7998128361456481317 ) ) ;
#167180 = CARTESIAN_POINT ( 'NONE',  ( 3.520197291191272448, 0.8326901208413343136, 1.664296038758736440 ) ) ;
#167181 = CARTESIAN_POINT ( 'NONE',  ( 10.40318394038753702, 11.03146944007395724, -0.7998128361456281477 ) ) ;
#167182 = CARTESIAN_POINT ( 'NONE',  ( 11.91294103507080848, 13.61460089956416297, -1.446263142085534747 ) ) ;
#167183 = CARTESIAN_POINT ( 'NONE',  ( -4.952806187693842510, 4.672695395264567786, 0.7998128361456341429 ) ) ;
#167184 = AXIS2_PLACEMENT_3D ( 'NONE', #68023, #182868, #87523 ) ;
#167185 = CARTESIAN_POINT ( 'NONE',  ( -7.157815033010924921, 10.43820240756634199, 1.199719254218453823 ) ) ;
#167186 = PRESENTATION_LAYER_ASSIGNMENT (  '', '', ( #194849 ) ) ;
#167188 = CARTESIAN_POINT ( 'NONE',  ( -4.351171265391168497, 7.394090626460979365, 1.174491979025530597 ) ) ;
#167187 = CARTESIAN_POINT ( 'NONE',  ( -6.099189001301292379, 8.209082816308541197, 1.599625672291263179 ) ) ;
#167189 = CARTESIAN_POINT ( 'NONE',  ( -0.6823417656250003738, -1.032291666325242607, -1.181850606188749264 ) ) ;
#167190 = CARTESIAN_POINT ( 'NONE',  ( 1.774300323613137165, -1.721452415463576635, 0.2060816229845687519 ) ) ;
#167191 = CARTESIAN_POINT ( 'NONE',  ( 1.323703871734905890, 1.676395044522845712, 0.4671252976603932350 ) ) ;
#167193 = CARTESIAN_POINT ( 'NONE',  ( 8.432808358020025707, 9.900993174853955026, 1.082531754730558626 ) ) ;
#167192 = CARTESIAN_POINT ( 'NONE',  ( 6.639320299308884010, -2.064767919570985821, 1.030881497364994681 ) ) ;
#167194 = CARTESIAN_POINT ( 'NONE',  ( -10.71030397718323890, 6.055815897892919075, -4.668189396100475008 ) ) ;
#167195 = CARTESIAN_POINT ( 'NONE',  ( 1.598976361298432014, 1.686402000465867301, -1.184152512226148923 ) ) ;
#167196 = ADVANCED_FACE ( 'NONE', ( #147421 ), #197737, .T. ) ;
#167197 = CARTESIAN_POINT ( 'NONE',  ( 0.1575669172422279607, -0.4392406603518673736, -1.974865693180789750 ) ) ;
#167198 = CARTESIAN_POINT ( 'NONE',  ( 0.006158830626129541130, 7.078243236992583398, -2.121324627965408993 ) ) ;
#167199 = CARTESIAN_POINT ( 'NONE',  ( -5.611095471209320174, 7.639640364534566075, 1.599625672291263179 ) ) ;
#167200 = CARTESIAN_POINT ( 'NONE',  ( 6.702024585102262400, -1.870183347854617040, 0.04844413084104796929 ) ) ;
#167202 = CARTESIAN_POINT ( 'NONE',  ( -7.268579750702160780, 8.613002809641560731, -1.082531754730549967 ) ) ;
#167201 = CARTESIAN_POINT ( 'NONE',  ( 5.097880177178074845, 1.288836597028759634, 1.412999258680311510 ) ) ;
#167203 = CARTESIAN_POINT ( 'NONE',  ( 6.533804136697315634, -1.437950210024591780, -1.674183229976949905 ) ) ;
#167204 = CARTESIAN_POINT ( 'NONE',  ( 1.224999999999928812, 2.208333334016110427, -0.7072540797573098059 ) ) ;
#167205 = CARTESIAN_POINT ( 'NONE',  ( -7.173763318588748383, -6.681223591462298828, -7.173763318588716409 ) ) ;
#167206 = CARTESIAN_POINT ( 'NONE',  ( 3.241808126998965811, 6.796210224891872542, 0.7216878364870257245 ) ) ;
#167207 = EDGE_CURVE ( 'NONE', #191915, #60728, #168678, .T. ) ;
#167208 = CARTESIAN_POINT ( 'NONE',  ( -7.014364370223741929, 9.276787413384745662, -1.599625672291271394 ) ) ;
#167209 = CARTESIAN_POINT ( 'NONE',  ( 6.428397668822618094, -0.9990526908794925554, -1.870407359624715937 ) ) ;
#167210 = ORIENTED_EDGE ( 'NONE', *, *, #181214, .T. ) ;
#167211 = CARTESIAN_POINT ( 'NONE',  ( 3.505163243484223479, 1.820685690116738531, -1.417681053453226703 ) ) ;
#167212 = CARTESIAN_POINT ( 'NONE',  ( 4.861744986159981075, -0.5251177144562025889, 1.890194517805739771 ) ) ;
#167213 = CARTESIAN_POINT ( 'NONE',  ( 0.7605091544688712402, -0.6555486260201286441, -1.849146037077718852 ) ) ;
#167214 = CARTESIAN_POINT ( 'NONE',  ( 4.067082894419602468, 3.847277586352047862, -0.7216878364870188411 ) ) ;
#167215 = DIRECTION ( 'NONE',  ( 8.638326563840814399E-31, 0.000000000000000000, 1.000000000000000000 ) ) ;
#167216 = VERTEX_POINT ( 'NONE', #94047 ) ;
#167217 = CARTESIAN_POINT ( 'NONE',  ( 0.1986506717676014555, 1.455101728037408337, -1.538369530143603559 ) ) ;
#167219 = CARTESIAN_POINT ( 'NONE',  ( -8.076906825439122528, 10.44614393447756129, -1.599625672291263179 ) ) ;
#167218 = CARTESIAN_POINT ( 'NONE',  ( -3.574546055497324737, 7.322054164722185732, 0.7998128361456341429 ) ) ;
#167220 = CARTESIAN_POINT ( 'NONE',  ( -7.334597915313094241, 9.580116872663850813, 1.040834085586084257E-14 ) ) ;
#167221 = CARTESIAN_POINT ( 'NONE',  ( 3.028372864778381413, 1.157752252206078358, 1.836431199091348665 ) ) ;
#167222 = CARTESIAN_POINT ( 'NONE',  ( 0.2923534576129138141, 2.707453654964923739, 2.053134718767547273 ) ) ;
#167223 = CARTESIAN_POINT ( 'NONE',  ( 2.373420902723611725, -1.847293605357634982, -1.041186957106011723 ) ) ;
#167224 = CARTESIAN_POINT ( 'NONE',  ( -1.499999999999997780, 3.181250000682818602, 1.214306433183764966E-14 ) ) ;
#167225 = CARTESIAN_POINT ( 'NONE',  ( 9.053093885623066939, 11.58502883802551153, -1.599625672291262513 ) ) ;
#167226 = CARTESIAN_POINT ( 'NONE',  ( 11.89197369110779512, 11.30000000000000071, -0.8056055387119873679 ) ) ;
#167227 = CARTESIAN_POINT ( 'NONE',  ( 6.604365638557201379, 6.767254738080503706, -0.09251035838216993545 ) ) ;
#167228 = CARTESIAN_POINT ( 'NONE',  ( 1.809912028077927282, -2.045576594096469414, 0.2490995888081939946 ) ) ;
#167230 = CARTESIAN_POINT ( 'NONE',  ( 3.469446951953614189E-15, 6.400000000000023448, 1.214306433183764966E-14 ) ) ;
#167229 = CARTESIAN_POINT ( 'NONE',  ( -9.826962411806732689, 10.35921099006301382, -0.7998128361456291469 ) ) ;
#167231 = CARTESIAN_POINT ( 'NONE',  ( 1.364683531249988757, 2.384375000341422357, 1.214306433183764966E-14 ) ) ;
#167232 = CARTESIAN_POINT ( 'NONE',  ( 0.07735805125224680390, 0.7159309182679198802, -2.172969595131315934 ) ) ;
#167233 = CARTESIAN_POINT ( 'NONE',  ( -10.91970695577496997, -5.907420853759282053, 5.204170427930421283E-15 ) ) ;
#167234 = ORIENTED_EDGE ( 'NONE', *, *, #190530, .F. ) ;
#167235 = CARTESIAN_POINT ( 'NONE',  ( 4.090413894173472009, -1.098427525215146749, 1.565146720495188104 ) ) ;
#167236 = CARTESIAN_POINT ( 'NONE',  ( 1.335668079023267119, -2.045225487398461883, 0.9674528744543411385 ) ) ;
#167237 = CARTESIAN_POINT ( 'NONE',  ( -2.103486388414573138, 5.605817886458954291, 1.040834085586084257E-14 ) ) ;
#167239 = ADVANCED_FACE ( 'NONE', ( #191504 ), #39953, .F. ) ;
#167238 = CARTESIAN_POINT ( 'NONE',  ( 1.230386416485089729, 1.215489027575139769, -1.343484786563201805 ) ) ;
#167240 = CARTESIAN_POINT ( 'NONE',  ( 1.270553553854154361, -0.2845990055821822629, -1.894349495789057647 ) ) ;
#167241 = CARTESIAN_POINT ( 'NONE',  ( 1.680221237283368696, -1.148429780529091948, -1.722445320287042447 ) ) ;
#167242 = CARTESIAN_POINT ( 'NONE',  ( -0.6823417656250246877, 0.3635416670080895973, 1.181850606188755259 ) ) ;
#167243 = CARTESIAN_POINT ( 'NONE',  ( 0.3035114269093022732, -0.5280327476409033549, 1.899365994968700955 ) ) ;
#167244 = CARTESIAN_POINT ( 'NONE',  ( 5.865835041973252117, 1.897565194821029033, -0.3318024074076031948 ) ) ;
#167246 = CARTESIAN_POINT ( 'NONE',  ( 6.450676980830294838, 6.774405823990504949, -0.3487213023658369826 ) ) ;
#167245 = CARTESIAN_POINT ( 'NONE',  ( 0.2238089703245670359, -0.1066217210726662923, 2.305362286893299917 ) ) ;
#167247 = CARTESIAN_POINT ( 'NONE',  ( -1.364683531250000748, 2.259375000341422357, 1.214306433183764966E-14 ) ) ;
#167248 = CARTESIAN_POINT ( 'NONE',  ( 4.299324853187779460, -1.796095115987613955, 1.014086197209535634 ) ) ;
#167249 = CIRCLE ( 'NONE', #98149, 1.250000000000000888 ) ;
#167251 = CARTESIAN_POINT ( 'NONE',  ( -6.470265622219711688, 8.571729197388226140, -1.599625672291263179 ) ) ;
#167250 = VECTOR ( 'NONE', #3527, 1000.000000000000000 ) ;
#167252 = CARTESIAN_POINT ( 'NONE',  ( 6.428537391173986038, 10.65171072301167854, 0.7998128361456462443 ) ) ;
#167253 = CARTESIAN_POINT ( 'NONE',  ( 0.000000000000000000, 0.03624871340549007392, 0.000000000000000000 ) ) ;
#167254 = CARTESIAN_POINT ( 'NONE',  ( 6.830610463186557624, 6.863467050006115677, 1.040834085586084257E-14 ) ) ;
#167256 = CARTESIAN_POINT ( 'NONE',  ( -0.7499999999999972244, 4.358333333333352932, -1.299038105676652011 ) ) ;
#167255 = CARTESIAN_POINT ( 'NONE',  ( 5.086996280900090817, -0.2547426189827053378, -2.090417274992136587 ) ) ;
#167257 = EDGE_CURVE ( 'NONE', #150264, #153847, #49757, .T. ) ;
#167258 = CARTESIAN_POINT ( 'NONE',  ( 0.9069515603133030401, 0.6301693757862131262, 2.077734764916533639 ) ) ;
#167260 = CARTESIAN_POINT ( 'NONE',  ( -1.364683531250000748, 1.321875000341421469, 0.000000000000000000 ) ) ;
#167259 = AXIS2_PLACEMENT_3D ( 'NONE', #41257, #40175, #105191 ) ;
#167261 = CARTESIAN_POINT ( 'NONE',  ( 4.886082254767631916, -1.023713625618065004, 1.903838226609423590 ) ) ;
#167262 = CARTESIAN_POINT ( 'NONE',  ( 5.813150814160550794, 1.649844410012293539, -1.164645984317608463 ) ) ;
#167263 = FACE_OUTER_BOUND ( 'NONE', #194000, .T. ) ;
#167264 = TOROIDAL_SURFACE ( 'NONE', #73876, 1.829047314007947955, 0.05000000000000000278 ) ;
#167267 = CARTESIAN_POINT ( 'NONE',  ( 4.690757960648213931, 8.416375354157496602, 0.7216878364870438212 ) ) ;
#167266 = CARTESIAN_POINT ( 'NONE',  ( 3.285556943749998737, -1.305208332855376296, -1.896917185911906500 ) ) ;
#167265 = CARTESIAN_POINT ( 'NONE',  ( -3.099815351088664794, 14.55179009333156159, -11.55525895789692292 ) ) ;
#167268 = CARTESIAN_POINT ( 'NONE',  ( -5.631432701629818460, 7.663367133358481631, 1.599625672291263179 ) ) ;
#167269 = CARTESIAN_POINT ( 'NONE',  ( 3.977750132953357998, -0.7672935630990398437, 1.865046046545227654 ) ) ;
#167270 = CARTESIAN_POINT ( 'NONE',  ( -7.655550293210764856, 12.08322577538792331, 0.000000000000000000 ) ) ;
#167272 = CARTESIAN_POINT ( 'NONE',  ( -7.553300976144787349, 8.945177572657957654, -1.082531754730549967 ) ) ;
#167271 = CARTESIAN_POINT ( 'NONE',  ( -2.981903720001798597, 5.566305875722335372, -1.199719254218446718 ) ) ;
#167274 = CARTESIAN_POINT ( 'NONE',  ( 0.6823417656249969321, 8.526041667008064096, -1.181850606188757036 ) ) ;
#167273 = CARTESIAN_POINT ( 'NONE',  ( 4.873979933848565871, 1.241796773192262116, 1.769252301715443565 ) ) ;
#167275 = DIRECTION ( 'NONE',  ( 0.000000000000000000, -1.000000000000000000, 0.000000000000000000 ) ) ;
#167276 = CARTESIAN_POINT ( 'NONE',  ( -2.788906526875773208E-15, 13.18750000000000000, -1.499999999999998446 ) ) ;
#167278 = CARTESIAN_POINT ( 'NONE',  ( 5.782827418265350516, 1.646828846085298448, -1.163285542026312847 ) ) ;
#167277 = CARTESIAN_POINT ( 'NONE',  ( -6.005898860729463884, 9.950706404252290582, 0.7216878364870458196 ) ) ;
#167279 = CARTESIAN_POINT ( 'NONE',  ( -1.500000000000011324, 4.879166666666690411, -0.8660254037844313801 ) ) ;
#167280 = CARTESIAN_POINT ( 'NONE',  ( 0.8555558213108410692, 1.723155885897029282, -0.08016331026279581440 ) ) ;
#167281 = CARTESIAN_POINT ( 'NONE',  ( 6.333594036239346359, 7.418223126147930557, 1.199719254218453823 ) ) ;
#167283 = CARTESIAN_POINT ( 'NONE',  ( 6.343235766347262938, 8.493804042195527870, -1.599625672291281386 ) ) ;
#167282 = CARTESIAN_POINT ( 'NONE',  ( 6.954969614130424027, 11.05795561655343384, 1.040834085586084257E-14 ) ) ;
#167284 = FACE_OUTER_BOUND ( 'NONE', #54308, .T. ) ;
#167285 = CARTESIAN_POINT ( 'NONE',  ( 5.184763189090160651, -0.2277032997176874074, -1.856539885857370953 ) ) ;
#167286 = CARTESIAN_POINT ( 'NONE',  ( 0.1705643940957324023, 0.7724326726834315204, 1.859191304955130297 ) ) ;
#167287 = CARTESIAN_POINT ( 'NONE',  ( 6.539320575229274901, 7.053161517996441532, 2.494893549996656912 ) ) ;
#167288 = CARTESIAN_POINT ( 'NONE',  ( -6.794044373779495771, 8.059378203231773341, 1.082531754730549078 ) ) ;
#167289 = EDGE_LOOP ( 'NONE', ( #123846, #213612, #107994, #14905 ) ) ;
#167291 = CARTESIAN_POINT ( 'NONE',  ( 0.5972800738224989248, -0.2930464221381039458, 1.994874516246990748 ) ) ;
#167290 = CARTESIAN_POINT ( 'NONE',  ( 1.998837940877351116, -2.080155006269391205, -0.4107514010402503746 ) ) ;
#167292 = CARTESIAN_POINT ( 'NONE',  ( 1.107327745774109529, 1.372724574380719043, 1.182278994020573792 ) ) ;
#167293 = CARTESIAN_POINT ( 'NONE',  ( 6.013923656113508542, 9.173938811177871244, -1.199719254218452047 ) ) ;
#167294 = CARTESIAN_POINT ( 'NONE',  ( 6.104392421991035711, -0.7735064434604683736, -2.018760209060527444 ) ) ;
#167295 = ORIENTED_EDGE ( 'NONE', *, *, #29276, .T. ) ;
#167296 = CARTESIAN_POINT ( 'NONE',  ( 8.111855979677986994, 8.358253485912799263, 1.040834085586084257E-14 ) ) ;
#167298 = CARTESIAN_POINT ( 'NONE',  ( -0.04785004733596533166, -1.249461711056678803, 1.452303129844798590 ) ) ;
#167297 = CARTESIAN_POINT ( 'NONE',  ( -5.416646063859567484, 6.278174148379618735, 1.199719254218450271 ) ) ;
#167299 = DIRECTION ( 'NONE',  ( 0.000000000000000000, -1.000000000000000000, 0.000000000000000000 ) ) ;
#167300 = CARTESIAN_POINT ( 'NONE',  ( 0.000000000000000000, 13.88000000000000078, 0.000000000000000000 ) ) ;
#167301 = CARTESIAN_POINT ( 'NONE',  ( 6.114364089638786304, 8.156510742710487705, 1.443375672974076540 ) ) ;
#167302 = CARTESIAN_POINT ( 'NONE',  ( -1.364683531250014514, -0.4489583329919089039, -0.7879004041258359514 ) ) ;
#167303 = CARTESIAN_POINT ( 'NONE',  ( 3.931501358282940117, 4.649468341827285300, -1.082531754730543083 ) ) ;
#167304 = CARTESIAN_POINT ( 'NONE',  ( -2.462777459176719308, 6.024990802348131780, -0.7998128361456281477 ) ) ;
#167305 = CARTESIAN_POINT ( 'NONE',  ( 4.575171270262055501, 0.003154952768896768234, -2.161883445794945846 ) ) ;
#167306 = CARTESIAN_POINT ( 'NONE',  ( -6.631346530859867805, 6.909194838857525944, 0.000000000000000000 ) ) ;
#167307 = CARTESIAN_POINT ( 'NONE',  ( 5.722950238744200391, 7.770137593325314285, 1.443375672974065660 ) ) ;
#167308 = CARTESIAN_POINT ( 'NONE',  ( 2.162495577681341707, 2.120227376586072854, 0.04728746717985036346 ) ) ;
#167309 = CARTESIAN_POINT ( 'NONE',  ( 6.563509198815888901, 0.3086105522638155629, -1.799150958419073909 ) ) ;
#167310 = CARTESIAN_POINT ( 'NONE',  ( 2.337131052746133975, -1.762546391092616238, 0.8830908230641126844 ) ) ;
#167311 = CARTESIAN_POINT ( 'NONE',  ( 4.289254230599209627, -0.005406649120142519548, -1.912571728590661380 ) ) ;
#167312 = ORIENTED_EDGE ( 'NONE', *, *, #70073, .F. ) ;
#167313 = CARTESIAN_POINT ( 'NONE',  ( 9.500587730663498931, -7.019129742886753398, -0.03636482241200242327 ) ) ;
#167314 = CARTESIAN_POINT ( 'NONE',  ( 5.705506402468259353, -1.551454039220935055, -1.213164361648248368 ) ) ;
#167315 = CARTESIAN_POINT ( 'NONE',  ( 1.851409727902778357, 1.936748846533197677, -0.1429498737708263245 ) ) ;
#167316 = ORIENTED_EDGE ( 'NONE', *, *, #163875, .F. ) ;
#167317 = CARTESIAN_POINT ( 'NONE',  ( -3.637330350216213759, 7.465578851886037093, -0.7998128361456481317 ) ) ;
#167319 = CARTESIAN_POINT ( 'NONE',  ( 6.743487189264861570, -7.020359948792185278, -6.692370362267389794 ) ) ;
#167318 = CARTESIAN_POINT ( 'NONE',  ( -6.563555762791521531, 9.711213252348503744, 1.082531754730549967 ) ) ;
#167322 = ADVANCED_FACE ( 'NONE', ( #142810, #89785 ), #58325, .T. ) ;
#167321 = CARTESIAN_POINT ( 'NONE',  ( 5.844973620822844218, 6.952128991449046502, 1.082531754730549967 ) ) ;
#167320 = CARTESIAN_POINT ( 'NONE',  ( 6.928380191783277908, 8.041863964290678624, 1.199719254218462483 ) ) ;
#167324 = ORIENTED_EDGE ( 'NONE', *, *, #38452, .T. ) ;
#167323 = CARTESIAN_POINT ( 'NONE',  ( 4.934190575774549892, -1.026228162776990027, -1.613408319405706504 ) ) ;
#167325 = CARTESIAN_POINT ( 'NONE',  ( 3.809358915828209735, 1.892446193107431451, 1.135094405146239049 ) ) ;
#167326 = CARTESIAN_POINT ( 'NONE',  ( 2.116530880626496192, -1.040147864624408003, -1.946245422063937802 ) ) ;
#167327 = CARTESIAN_POINT ( 'NONE',  ( 1.569519686356874999, 8.730458328475176444, 2.495327313683093351 ) ) ;
#167328 = CARTESIAN_POINT ( 'NONE',  ( 0.1879522776407696050, 1.101030317643518330, 1.563299796079109072 ) ) ;
#167329 = TOROIDAL_SURFACE ( 'NONE', #11627, 10.92000000000000171, 0.08000000000000000167 ) ;
#167330 = CARTESIAN_POINT ( 'NONE',  ( -10.50000000000000355, 12.59281572507203606, 3.599999999999998312 ) ) ;
#167331 = CARTESIAN_POINT ( 'NONE',  ( 6.764898216730270697, -7.628386336122854772, -6.764898216727333491 ) ) ;
#167332 = CARTESIAN_POINT ( 'NONE',  ( 3.350112325975619587, -0.8415805752714689003, 1.891790567983504312 ) ) ;
#167333 = CARTESIAN_POINT ( 'NONE',  ( -6.112028321662274166, 6.025121218227761588, 0.7998128361456341429 ) ) ;
#167334 = CARTESIAN_POINT ( 'NONE',  ( -6.265474751258844677, 6.912123529488261475, 0.7890932636151950508 ) ) ;
#167336 = CARTESIAN_POINT ( 'NONE',  ( 1.481558191429487970, 1.997200094811113491, -0.8276061316847342919 ) ) ;
#167335 = CARTESIAN_POINT ( 'NONE',  ( -5.264643720808155791, 5.036505850564608089, 0.000000000000000000 ) ) ;
#167337 = CARTESIAN_POINT ( 'NONE',  ( 4.124703146219878214, 0.1084699374758208573, 2.189010777610411740 ) ) ;
#167338 = DIRECTION ( 'NONE',  ( 0.000000000000000000, 8.546850786086437571E-32, 1.000000000000000000 ) ) ;
#167339 = CARTESIAN_POINT ( 'NONE',  ( 3.716343503921665459, 6.389465617000312569, -1.082531754730549967 ) ) ;
#167340 = CARTESIAN_POINT ( 'NONE',  ( 1.419999999999822737, 7.176846818246208848, 4.202462424328221147 ) ) ;
#167341 = CARTESIAN_POINT ( 'NONE',  ( 0.6823417656249934904, 14.25520833367473195, 1.181850606188764807 ) ) ;
#167342 = CARTESIAN_POINT ( 'NONE',  ( -6.629010762438975135, 6.698543742459062145, -0.7998128361456362523 ) ) ;
#167343 = UNCERTAINTY_MEASURE_WITH_UNIT (LENGTH_MEASURE( 1.000000000000000082E-05 ), #171423, 'distance_accuracy_value', 'NONE');
#167344 = CARTESIAN_POINT ( 'NONE',  ( 5.748594953515238082, 1.706903099953221759, -0.3051902176867369865 ) ) ;
#167345 = CARTESIAN_POINT ( 'NONE',  ( -2.266184231778562541, 5.795632037050281404, 1.040834085586084257E-14 ) ) ;
#167346 = CARTESIAN_POINT ( 'NONE',  ( 3.801679563076823420, -1.564429233171928058, -1.355977067927462754 ) ) ;
#167347 = CARTESIAN_POINT ( 'NONE',  ( 5.132460035084068117, 0.6155034331737432307, 2.025765117643091529 ) ) ;
#167348 = CARTESIAN_POINT ( 'NONE',  ( 6.799577732453452761, 7.891594428405881878, -1.199719254218446718 ) ) ;
#167349 = CARTESIAN_POINT ( 'NONE',  ( -0.6823417656249969321, 4.217708333674755394, -1.181850606188749264 ) ) ;
#167350 = CARTESIAN_POINT ( 'NONE',  ( 2.957809129533952142, -0.6224678976109696560, 1.868526426519439898 ) ) ;
#167351 = CARTESIAN_POINT ( 'NONE',  ( 1.054777118923880597, 0.3758132965740559883, 1.874924941132802836 ) ) ;
#167352 = CARTESIAN_POINT ( 'NONE',  ( 5.050848094970262991, -1.934468200101526758, -1.229489151810001735 ) ) ;
#167353 = CARTESIAN_POINT ( 'NONE',  ( 3.105874302609371362, -1.823586186413633126, 0.09019715141062728536 ) ) ;
#167354 = EDGE_CURVE ( 'NONE', #162324, #65240, #101547, .T. ) ;
#167355 = CARTESIAN_POINT ( 'NONE',  ( 5.011674058906918638, 5.875983152593414971, 1.199719254218452047 ) ) ;
#167356 = CARTESIAN_POINT ( 'NONE',  ( 5.463572716182824252, 7.397254140345190798, 1.443375672974062551 ) ) ;
#167357 = CARTESIAN_POINT ( 'NONE',  ( -7.314787569772770226, 8.492672571945082183, -1.199719254218452935 ) ) ;
#167358 = ORIENTED_EDGE ( 'NONE', *, *, #156758, .T. ) ;
#167359 = CARTESIAN_POINT ( 'NONE',  ( 3.445567785929729343, -1.858493022056451949, 0.7744065704922193927 ) ) ;
#167360 = CARTESIAN_POINT ( 'NONE',  ( 4.698074428120575519, 0.8425069249109422564, -1.771795133841248981 ) ) ;
#167361 = CARTESIAN_POINT ( 'NONE',  ( -6.938021921891187382, 9.117444880338284818, -1.599625672291263179 ) ) ;
#167362 = CARTESIAN_POINT ( 'NONE',  ( -4.089755892816631544, 7.923132308261379819, -0.7998128361456281477 ) ) ;
#167363 = CARTESIAN_POINT ( 'NONE',  ( 0.1755611466353811378, 5.720003923744535257, -2.838048273117784959 ) ) ;
#167365 = CARTESIAN_POINT ( 'NONE',  ( 5.770295338139614927, -1.120113875738535825, 1.370259874377998788 ) ) ;
#167364 = CARTESIAN_POINT ( 'NONE',  ( 0.2750908068406934803, 1.949304727321942599, -0.7563943737528535660 ) ) ;
#167366 = DIRECTION ( 'NONE',  ( -0.7592566023653044560, -0.6507913734559596097, -1.725633230170963762E-31 ) ) ;
#167367 = CARTESIAN_POINT ( 'NONE',  ( 1.570551226722196381, -2.081687204081467346, -0.6850663153453034893 ) ) ;
#167368 = CARTESIAN_POINT ( 'NONE',  ( -0.07713737713477014646, -1.067615817814296042, -1.374817276609247907 ) ) ;
#167369 = CARTESIAN_POINT ( 'NONE',  ( 8.450809820019639318, 8.753699632978056755, -0.7998128361456291469 ) ) ;
#167370 = CARTESIAN_POINT ( 'NONE',  ( 0.1335669894368317900, 1.324834237272943360, -2.404533294357531048 ) ) ;
#167371 = CARTESIAN_POINT ( 'NONE',  ( 0.9258787065367773961, 1.030881334376580805, -1.382772916119678897 ) ) ;
#167372 = CARTESIAN_POINT ( 'NONE',  ( 1.247910673863032116, -2.242740372501272006, -0.5020730165456227523 ) ) ;
#167373 = CARTESIAN_POINT ( 'NONE',  ( 0.2752733618501881363, 2.042644424557562122, -0.7945232813236638991 ) ) ;
#167374 = CARTESIAN_POINT ( 'NONE',  ( 2.508667999599442755, -0.8457060194008919618, -2.038605049697986615 ) ) ;
#167375 = CARTESIAN_POINT ( 'NONE',  ( 6.654729725391004713, -0.5723678854598751586, -2.094333189781839355 ) ) ;
#167376 = DIRECTION ( 'NONE',  ( 0.000000000000000000, 1.000000000000000000, 0.000000000000000000 ) ) ;
#167377 = CARTESIAN_POINT ( 'NONE',  ( 1.323616076398025587, -1.537765720040217055, -1.455736727087880489 ) ) ;
#167378 = CARTESIAN_POINT ( 'NONE',  ( 1.874158809982156670, 3.299964346911599122, 0.3999999999999681033 ) ) ;
#167379 = CARTESIAN_POINT ( 'NONE',  ( 5.051747076446268636, 0.6043308924107357871, -1.829198057362067198 ) ) ;
#167380 = VERTEX_POINT ( 'NONE', #73498 ) ;
#167382 = CARTESIAN_POINT ( 'NONE',  ( 1.499999999999991118, 5.754166666666685970, 0.8660254037844524744 ) ) ;
#167381 = CARTESIAN_POINT ( 'NONE',  ( 1.945279335750784711, -1.843959696387540204, -1.361743503316152681 ) ) ;
#167383 = CARTESIAN_POINT ( 'NONE',  ( 3.011882680530176604, 6.665613560593854459, 0.7998128361456341429 ) ) ;
#167384 = CARTESIAN_POINT ( 'NONE',  ( 5.144429221381498607, 8.089252293998699272, -1.199719254218452047 ) ) ;
#167385 = CARTESIAN_POINT ( 'NONE',  ( 4.846434531455360073, 1.142681229152305633, -1.904705486840562179 ) ) ;
#167386 = CARTESIAN_POINT ( 'NONE',  ( -6.697364695470783502, 10.75741654478384035, 0.7216878364870458196 ) ) ;
#167387 = EDGE_CURVE ( 'NONE', #34146, #197417, #49039, .T. ) ;
#167388 = CARTESIAN_POINT ( 'NONE',  ( -0.08000000000000714873, -9.999999999999994671, 10.91970695577494865 ) ) ;
#167389 = CARTESIAN_POINT ( 'NONE',  ( 6.493992391265805075, 6.678671999339316656, 1.040834085586084257E-14 ) ) ;
#167390 = CARTESIAN_POINT ( 'NONE',  ( -6.832946231163084860, 10.91559500309152675, 0.000000000000000000 ) ) ;
#167391 = CARTESIAN_POINT ( 'NONE',  ( 4.719646871332936477, 8.520355426614829142, -0.7216878364870357165 ) ) ;
#167392 = VERTEX_POINT ( 'NONE', #157980 ) ;
#167393 = CARTESIAN_POINT ( 'NONE',  ( 3.076796235938107138, -0.8146265060355701859, 1.844709937164576097 ) ) ;
#167395 = CARTESIAN_POINT ( 'NONE',  ( 0.7431262955939599291, -0.2488486719821168813, -2.047412193126110225 ) ) ;
#167394 = CARTESIAN_POINT ( 'NONE',  ( 7.935599982700328958, 8.152621489438862667, 0.7998128361456481317 ) ) ;
#167396 = CARTESIAN_POINT ( 'NONE',  ( -11.86239285000045740, 13.79999999999998472, 1.812080536912751061 ) ) ;
#167397 = CARTESIAN_POINT ( 'NONE',  ( 4.706088717274885092, 8.504537580213796133, 0.7216878364870317197 ) ) ;
#167398 = CIRCLE ( 'NONE', #1318, 0.1000000000000000472 ) ;
#167399 = DIRECTION ( 'NONE',  ( 0.000000000000000000, -1.000000000000000000, -9.023263958591317418E-17 ) ) ;
#167400 = CARTESIAN_POINT ( 'NONE',  ( 1.364683531249990311, 3.384375000341416140, 1.214306433183764966E-14 ) ) ;
#167401 = CARTESIAN_POINT ( 'NONE',  ( 4.084055714405177895, -2.167483682527316713, -0.3223708474724209516 ) ) ;
#167402 = CARTESIAN_POINT ( 'NONE',  ( 1.846327496167538884, 0.3419342931599393398, -1.987046799686801757 ) ) ;
#167403 = CARTESIAN_POINT ( 'NONE',  ( 1.346931166825489967, 0.5339940059071214273, -1.762130705996706181 ) ) ;
#167404 = CARTESIAN_POINT ( 'NONE',  ( 5.829661053323575537, 1.133102282163217955, -1.992656795126966252 ) ) ;
#167405 = CARTESIAN_POINT ( 'NONE',  ( 2.888418961059231904, 1.578855305991919478, -0.9468669452540460219 ) ) ;
#167406 = CARTESIAN_POINT ( 'NONE',  ( 9.745613490124728884, 10.26430391476735338, 0.7998128361456462443 ) ) ;
#167407 = CARTESIAN_POINT ( 'NONE',  ( 3.838725952263983388, 0.2674066485093031242, 1.805754746396167176 ) ) ;
#167408 = CARTESIAN_POINT ( 'NONE',  ( 4.940077362011475515, -1.704937458037486531, -1.076318853994034930 ) ) ;
#167409 = CARTESIAN_POINT ( 'NONE',  ( -9.189729191964438826, 9.615772233580322848, 1.040834085586084257E-14 ) ) ;
#167411 = CARTESIAN_POINT ( 'NONE',  ( -7.618755976236585958, 7.853246491889623648, 0.000000000000000000 ) ) ;
#167410 = CARTESIAN_POINT ( 'NONE',  ( 4.926805006903203221, 2.163674774341369123, 0.6614253976126910350 ) ) ;
#167412 = CARTESIAN_POINT ( 'NONE',  ( 6.510775453876758156, 1.563058401041140133, -1.411553977168745977 ) ) ;
#167413 = B_SPLINE_CURVE_WITH_KNOTS ( 'NONE', 3,
 ( #150019, #136970, #118637, #86072, #68730, #18917, #35171, #120786, #134851, #184622 ),
 .UNSPECIFIED., .F., .F.,
 ( 4, 2, 2, 2, 4 ),
 ( 0.0001270906692242517301, 0.0005866303604698383176, 0.001046170051715425041, 0.001505709742961011764, 0.001965249434206598270 ),
 .UNSPECIFIED. ) ;
#167414 = CARTESIAN_POINT ( 'NONE',  ( -1.947569660854454598, 3.752493983412270140, -0.4616071351974295189 ) ) ;
#167415 = CARTESIAN_POINT ( 'NONE',  ( 3.561042923925850978, 1.633862107263984065, -1.271492733312264090 ) ) ;
#167416 = CARTESIAN_POINT ( 'NONE',  ( 3.623053363349855172, 5.249981562040033189, 1.599625672291267398 ) ) ;
#167417 = CARTESIAN_POINT ( 'NONE',  ( -0.6801582343750420812, 1.880208333674727950, -1.178068619123883165 ) ) ;
#167418 = APPLICATION_PROTOCOL_DEFINITION ( 'draft international standard', 'automotive_design', 1998, #173739 ) ;
#167420 = CARTESIAN_POINT ( 'NONE',  ( 1.770020429662170658, 0.9901332625182661662, 1.652458556229096320 ) ) ;
#167419 = CARTESIAN_POINT ( 'NONE',  ( -7.853197290813634268, 10.18514947741448573, 1.599625672291295375 ) ) ;
#167421 = DIRECTION ( 'NONE',  ( 0.8003905296791061774, 0.000000000000000000, -0.5994789404140897782 ) ) ;
#167422 = CARTESIAN_POINT ( 'NONE',  ( 6.948121156015312216, -0.8458062566301125518, 1.777170381402736865 ) ) ;
#167423 = CARTESIAN_POINT ( 'NONE',  ( 5.682275777458854371, 5.801945626556378244, 0.7216878364870328300 ) ) ;
#167424 = CARTESIAN_POINT ( 'NONE',  ( 5.872608658597049391, 5.988986745869715023, 0.2392922861021197500 ) ) ;
#167425 = CARTESIAN_POINT ( 'NONE',  ( -4.437596350374534815, 4.071617251725375475, -0.7998128361456221525 ) ) ;
#167426 = CARTESIAN_POINT ( 'NONE',  ( 1.318920400837508167, -0.8056321388932115024, -2.070341401348996691 ) ) ;
#167427 = CARTESIAN_POINT ( 'NONE',  ( 2.801903084826493640, -0.6620233120280398786, 1.999254901717039790 ) ) ;
#167428 = CARTESIAN_POINT ( 'NONE',  ( -5.399890319992785237, 9.521898816625391504, 0.7998128361456291469 ) ) ;
#167429 = CARTESIAN_POINT ( 'NONE',  ( 7.800018446563675489, 7.994443030612759848, -0.7998128361456281477 ) ) ;
#167430 = CARTESIAN_POINT ( 'NONE',  ( 0.8536796107712171233, -0.6749765833247187707, 1.734523287792593571 ) ) ;
#167431 = CARTESIAN_POINT ( 'NONE',  ( 7.474622759835693131, 7.614814729430110951, -0.7998128361456281477 ) ) ;
#167432 = CARTESIAN_POINT ( 'NONE',  ( 4.473300617505036492, 7.306268922809479704, -1.199719254218452047 ) ) ;
#167433 = CARTESIAN_POINT ( 'NONE',  ( -6.956742217587851052, 7.288823140040177506, 0.000000000000000000 ) ) ;
#167434 = CARTESIAN_POINT ( 'NONE',  ( -8.703971430293361067, 9.256980878204810637, 0.7216878364870438212 ) ) ;
#167435 = CARTESIAN_POINT ( 'NONE',  ( 1.055114822555893728, 0.4192091730233596381, 2.078585086915801128 ) ) ;
#167436 = CARTESIAN_POINT ( 'NONE',  ( -4.911796789900812144, 8.952456364851418158, 0.7998128361456291469 ) ) ;
#167438 = CARTESIAN_POINT ( 'NONE',  ( 4.211346380768822506, -1.629847038978438079, -1.091715234301626314 ) ) ;
#167437 = CARTESIAN_POINT ( 'NONE',  ( 0.6124999999999967137, 0.5833333333333314830, 1.060881119635929348 ) ) ;
#167439 = CARTESIAN_POINT ( 'NONE',  ( 2.905317003618158367, 1.825515667692039878, 1.157497049167732550 ) ) ;
#167440 = CARTESIAN_POINT ( 'NONE',  ( 2.243484787601189634, 1.840893492186860492, 0.04347913094143729396 ) ) ;
#167441 = CARTESIAN_POINT ( 'NONE',  ( -4.061901113999940804, 7.558576442610514867, -0.4421990992426305112 ) ) ;
#167442 = CARTESIAN_POINT ( 'NONE',  ( 4.254006295369892499, 7.509857431501010261, -1.008242097476583554 ) ) ;
#167443 = EDGE_CURVE ( 'NONE', #133576, #140339, #62800, .T. ) ;
#167444 = CARTESIAN_POINT ( 'NONE',  ( 4.909954989264024405, 1.196826376938535219, -1.263709391550037031 ) ) ;
#167445 = CARTESIAN_POINT ( 'NONE',  ( 5.666945020832170776, 7.634521829102760115, 1.443375672974062551 ) ) ;
#167446 = CARTESIAN_POINT ( 'NONE',  ( -10.02511099414689077, 5.770000865873268658, 5.887978427067937837 ) ) ;
#167447 = CARTESIAN_POINT ( 'NONE',  ( 2.149508875876861236, -1.735919364271593768, -1.288018159417112729 ) ) ;
#167448 = CARTESIAN_POINT ( 'NONE',  ( 3.163435312993330140, -0.5825663732807913053, -1.930122257003751063 ) ) ;
#167449 = CARTESIAN_POINT ( 'NONE',  ( 0.8312129145573650124, 0.1600495679085281175, 2.155820468135719814 ) ) ;
#167450 = CARTESIAN_POINT ( 'NONE',  ( 3.186357099593698283, -1.942036093696447363, -0.3385421596419062595 ) ) ;
#167451 = CIRCLE ( 'NONE', #132988, 0.09999999999999971412 ) ;
#167452 = CARTESIAN_POINT ( 'NONE',  ( 6.509000000000010999, 0.007656933339201045172, 1.900274884395843245 ) ) ;
#167453 = CARTESIAN_POINT ( 'NONE',  ( 3.491681510897004959, -1.939965067831977530, -0.09248793024771610749 ) ) ;
#167456 = ORIENTED_EDGE ( 'NONE', *, *, #28350, .F. ) ;
#167455 = CARTESIAN_POINT ( 'NONE',  ( -3.011319516011047082, 6.527306845405913549, 0.7216878364870328300 ) ) ;
#167454 = CARTESIAN_POINT ( 'NONE',  ( -10.10046125205658463, 11.84658821789661509, -1.082531754730537976 ) ) ;
#167457 = CARTESIAN_POINT ( 'NONE',  ( -4.950135482320926705, 6.868520377498098739, -1.443375672974066548 ) ) ;
#167458 = CARTESIAN_POINT ( 'NONE',  ( 6.059568310664962709, 6.034194215389424798, 0.7998128361456352531 ) ) ;
#167459 = EDGE_CURVE ( 'NONE', #196686, #80044, #173514, .T. ) ;
#167460 = CARTESIAN_POINT ( 'NONE',  ( -4.492547798081878874, 6.334668079219206049, 1.599625672291263179 ) ) ;
#167461 = CARTESIAN_POINT ( 'NONE',  ( -5.173318132066234476, 8.193232366456022930, -1.199719254218453823 ) ) ;
#167462 = CARTESIAN_POINT ( 'NONE',  ( -10.43941509239824228, 11.28166515066052966, 1.040834085586084257E-14 ) ) ;
#167463 = CARTESIAN_POINT ( 'NONE',  ( 6.633790087849154027, -1.500048720590658302, -1.753619728580549708 ) ) ;
#167464 = CARTESIAN_POINT ( 'NONE',  ( 3.285556943749998737, -2.705208332855374209, -1.896917185911906500 ) ) ;
#167465 = CARTESIAN_POINT ( 'NONE',  ( 4.451973756923766068, -0.7546651901383871763, 1.810992078419524365 ) ) ;
#167466 = CARTESIAN_POINT ( 'NONE',  ( 1.705704151892040832, 1.882474636155605507, 0.7231385473688843879 ) ) ;
#167467 = EDGE_LOOP ( 'NONE', ( #42343, #68509, #64639, #37726 ) ) ;
#167468 = CARTESIAN_POINT ( 'NONE',  ( 3.714152660773429648, 1.129254856714853261, -1.790882643308453703 ) ) ;
#167469 = CARTESIAN_POINT ( 'NONE',  ( -1.201851678989727383E-14, 3.243750000682814161, 1.732050807568877637 ) ) ;
#167471 = CARTESIAN_POINT ( 'NONE',  ( -5.096975683733680818, 8.033889833409558534, -1.199719254218452047 ) ) ;
#167470 = CARTESIAN_POINT ( 'NONE',  ( 0.07459516483344308391, 2.893589955008399883, -2.244599473808198020 ) ) ;
#167472 = CARTESIAN_POINT ( 'NONE',  ( 3.363068133243895197, 1.796009578954290253, -0.4044003374430102382 ) ) ;
#167473 = ORIENTED_EDGE ( 'NONE', *, *, #140577, .T. ) ;
#167474 = UNCERTAINTY_MEASURE_WITH_UNIT (LENGTH_MEASURE( 1.000000000000000082E-05 ), #30665, 'distance_accuracy_value', 'NONE');
#167475 = CARTESIAN_POINT ( 'NONE',  ( -9.833741488613570780, 10.36711991300432345, 0.7998128361456462443 ) ) ;
#167476 = CARTESIAN_POINT ( 'NONE',  ( 0.3999999999999442890, 3.322650755865476757, 0.5865692111442147860 ) ) ;
#167477 = CARTESIAN_POINT ( 'NONE',  ( 4.851869265964163347, -1.501451181749386743, -1.497782127133556518 ) ) ;
#167478 = CARTESIAN_POINT ( 'NONE',  ( 6.825078400183573812, 0.002648415797040087893, 1.855566311045192540 ) ) ;
#167479 = CARTESIAN_POINT ( 'NONE',  ( 5.777746017718023097, 9.892454120646377191, 0.7998128361456462443 ) ) ;
#167480 = CARTESIAN_POINT ( 'NONE',  ( 5.430957059787441032, 0.1471976826952873518, 2.055563341089384988 ) ) ;
#167483 = CARTESIAN_POINT ( 'NONE',  ( 2.489598673502769977, -1.836455140896048999, -0.1334285330320400531 ) ) ;
#167482 = CARTESIAN_POINT ( 'NONE',  ( 0.3966288646398182238, 0.3121968076400126746, 1.834509442227350462 ) ) ;
#167481 = DIRECTION ( 'NONE',  ( 0.000000000000000000, 1.000000000000000000, 0.000000000000000000 ) ) ;
#167484 = CARTESIAN_POINT ( 'NONE',  ( 10.07100917685271035, 10.64393221595000938, 0.7998128361456462443 ) ) ;
#167485 = CARTESIAN_POINT ( 'NONE',  ( 4.299316086327568343, 7.453850760076471182, -1.115744863390004671 ) ) ;
#167486 = CARTESIAN_POINT ( 'NONE',  ( -4.848826244296223109, 5.027555131033083491, -0.8732430475888955934 ) ) ;
#167487 = CARTESIAN_POINT ( 'NONE',  ( 10.98677171181892476, -7.666863022245585135, -0.5458515184425005717 ) ) ;
#167488 = CARTESIAN_POINT ( 'NONE',  ( 2.473496279428960776, 0.1070396533628548558, -2.204406164007084445 ) ) ;
#167489 = CARTESIAN_POINT ( 'NONE',  ( 5.220128827380259295, -1.204132088723122385, -1.915181361845545105 ) ) ;
#167490 = CARTESIAN_POINT ( 'NONE',  ( -6.371969008742801144, 10.37778824360119145, 0.7216878364870458196 ) ) ;
#167491 = CARTESIAN_POINT ( 'NONE',  ( 4.851724922005476337, -1.286371495869711667, -1.275854292049487304 ) ) ;
#167492 = CARTESIAN_POINT ( 'NONE',  ( 3.661272352971048694, 1.801931492627879106, -0.6507149165355142761 ) ) ;
#167493 = CARTESIAN_POINT ( 'NONE',  ( -1.001543065824772872E-14, 5.634375000341415252, 1.575800808251672791 ) ) ;
#167494 = CARTESIAN_POINT ( 'NONE',  ( 4.381683959536594841, 1.286834623079432083, 1.493660651562748853 ) ) ;
#167495 = CARTESIAN_POINT ( 'NONE',  ( 5.119927267529915227, -1.001353885182048931, -1.579878405157906673 ) ) ;
#167496 = CARTESIAN_POINT ( 'NONE',  ( 5.160548226176637776, -0.6268552802725676498, -1.752456121274186263 ) ) ;
#167497 = CARTESIAN_POINT ( 'NONE',  ( -0.04763828917917976857, -1.313539345393003321, 1.530161206715647149 ) ) ;
#167499 = CARTESIAN_POINT ( 'NONE',  ( 2.104260374134783174, -2.105582044810641484, 0.05271062337313356383 ) ) ;
#167498 = CARTESIAN_POINT ( 'NONE',  ( -10.64045162862669081, 11.30828174301964140, -0.7998128361456221525 ) ) ;
#167500 = EDGE_CURVE ( 'NONE', #190224, #109852, #59386, .T. ) ;
#167501 = CARTESIAN_POINT ( 'NONE',  ( 7.913155211870404493, 12.38376484715752213, 0.7998128361456462443 ) ) ;
#167503 = CARTESIAN_POINT ( 'NONE',  ( 0.000000000000000000, 2.800000000000024691, 1.214306433183764966E-14 ) ) ;
#167502 = CARTESIAN_POINT ( 'NONE',  ( 0.000000000000000000, 6.499999999999999112, 0.000000000000000000 ) ) ;
#167504 = CARTESIAN_POINT ( 'NONE',  ( 2.953504815971871977, -1.868289524550557523, 1.003269902519101864 ) ) ;
#167505 = CARTESIAN_POINT ( 'NONE',  ( -9.590330253158105833, -9.597646708343960498, 0.1673998372498867182 ) ) ;
#167506 = CARTESIAN_POINT ( 'NONE',  ( 2.039325177177089721, 0.004250232316239943575, 2.019972748817438823 ) ) ;
#167507 = CARTESIAN_POINT ( 'NONE',  ( 1.364683531249986537, 2.155208333674751398, -0.7879004041258239610 ) ) ;
#167508 = CARTESIAN_POINT ( 'NONE',  ( -3.633221978782299910, 5.261844946711204507, -1.443375672974053447 ) ) ;
#167509 = EDGE_CURVE ( 'NONE', #82895, #66830, #42087, .T. ) ;
#167510 = CARTESIAN_POINT ( 'NONE',  ( 4.857899112398166075, 4.561970474086296079, 1.040834085586084257E-14 ) ) ;
#167511 = EDGE_LOOP ( 'NONE', ( #210330, #12062, #209539, #153430 ) ) ;
#167512 = CARTESIAN_POINT ( 'NONE',  ( 2.126461914815626297, 1.246462439515462650, -1.765816729463750123 ) ) ;
#167513 = CARTESIAN_POINT ( 'NONE',  ( 6.609999999999973674, -0.005249217919313375023, 2.280159464062641916 ) ) ;
#167515 = CARTESIAN_POINT ( 'NONE',  ( 3.606105671554957759, 4.269840040644637291, -1.082531754730543083 ) ) ;
#167514 = CARTESIAN_POINT ( 'NONE',  ( 5.246079093845007257, 5.085123462432798114, 0.7998128361456352531 ) ) ;
#167516 = FACE_OUTER_BOUND ( 'NONE', #113388, .T. ) ;
#167517 = CARTESIAN_POINT ( 'NONE',  ( 1.499999999999997113, 4.035416667349482012, 0.8660254037844477004 ) ) ;
#167518 = CARTESIAN_POINT ( 'NONE',  ( -7.212574532790100079, 9.437756259720353924, -1.443375672974059665 ) ) ;
#167519 = CARTESIAN_POINT ( 'NONE',  ( 1.435386855117400717, -1.590506285900999295, -1.507976327226906443 ) ) ;
#167520 = CARTESIAN_POINT ( 'NONE',  ( -1.084202172485504434E-15, -6.705807707623162806, -10.34804402329775108 ) ) ;
#167522 = CARTESIAN_POINT ( 'NONE',  ( -8.012344526598182026E-15, 12.54687500034139980, -1.575800808251669460 ) ) ;
#167521 = CARTESIAN_POINT ( 'NONE',  ( 1.200488511320395579, -2.262689073810118412, 0.002107776778791786276 ) ) ;
#167523 = CARTESIAN_POINT ( 'NONE',  ( -7.133561379084627063, 11.47423870890741782, 0.7998128361456481317 ) ) ;
#167524 = CARTESIAN_POINT ( 'NONE',  ( -4.406036734316890247, 7.123831375802920363, -1.082531754730548412 ) ) ;
#167525 = CARTESIAN_POINT ( 'NONE',  ( -1.364683531250000748, 2.071875000341422357, 1.214306433183764966E-14 ) ) ;
#167526 = CARTESIAN_POINT ( 'NONE',  ( 4.596293493935747598, 8.372084169494645067, 0.08663659024946840370 ) ) ;
#167527 = CARTESIAN_POINT ( 'NONE',  ( -0.7500000000000006661, 9.208333333333332149, -1.299038105676657340 ) ) ;
#167528 = CARTESIAN_POINT ( 'NONE',  ( 3.949580097687496405, 0.5788178622721011912, -1.624998464860913705 ) ) ;
#167529 = CARTESIAN_POINT ( 'NONE',  ( 3.715816618597135523, 6.492813934075403637, -1.199719254218453823 ) ) ;
#167530 = CARTESIAN_POINT ( 'NONE',  ( 1.616075582413665002, 1.193477697079999178, -1.306907023524202183 ) ) ;
#167531 =( BOUNDED_SURFACE ( )  B_SPLINE_SURFACE ( 1, 2, ( 
 ( #84095, #169612, #153366, #152301, #3874, #69947, #120948, #136059, #202072, #53732, #186919, #21194, #88371, #37474, #103552, #87297, #38549, #104627, #170674, #154437, #172830, #156579, #24401, #105714, #74256, #73156, #76374, #42843, #10301, #139263, #90514, #56931, #23339, #59057, #91594, #8172, #108950, #123104, #140350, #189061, #205293, #122017, #206369, #158702, #40698, #57995, #174970, #142481, #143559, #124158, #110018, #26552, #208489, #106801, #92660, #190120, #187985, #41774, #107886, #173914, #25488, #157646, #9243, #75315, #77442, #39611, #141431, #155501, #171742, #176031, #89449, #60125, #207438, #125214, #191176, #126284, #192242, #43904, #27624, #93724, #159763, #209553, #7084, #11363, #129491, #97988, #128426, #178160, #181337, #82770, #162979, #63331, #14557, #195473, #28702, #160836, #32964, #62266, #80655, #12427, #94787, #147793, #144625, #78507, #112157, #210639, #47105, #148844, #115346, #99039, #111081, #177085, #96928, #113220, #49225, #194393, #145697, #127356, #48177, #31911, #29775, #46036, #179225, #15622, #95859, #161915, #13505, #81712, #114290, #165094, #79578, #64399, #30850, #211695, #146745, #212764, #130543, #196535, #180288, #164047, #44973, #213811, #65431, #131581, #197583, #16686, #61197, #193325, #149921, #116401, #152051, #184521, #183466, #135802, #1490, #35073, #67555, #166154, #417, #18817, #37222, #17741, #167231, #201826, #103296, #22003, #101143, #202897, #53471, #87039, #133699, #119608, #84904, #66488, #199704, #51350, #68631, #117474, #150991, #2556, #36142, #170414, #132629, #134753, #34019, #198634, #54542, #182389, #153111, #200762, #52412, #118538, #20943, #102225, #168295, #19891, #85976, #3620, #88114, #50282, #83829, #69700, #169357, #185593, #4685, #120689, #100093, #70759, #136872, #186665, #38292, #104370, #39359, #59874, #155250, #41515, #105455, #187730, #26296, #23082, #171491, #205037, #89197, #175777, #55608, #58810, #40445, #142229, #173660, #109770, #25233, #6831, #154184, #137940, #107628, #56682, #72910, #126025, #75063, #71830, #188809, #108695, #106545, #141175, #139015, #190926, #122847, #191987, #208243, #92411, #172572, #91336, #27371, #24154, #203961, #90257, #156325, #158450, #5752, #7907, #174723, #73996, #57746, #8988, #207186, #140089, #121764, #42590, #43653, #206114, #123904, #189873, #157394, #124964, #10051, #76126, #146491, #94537, #180036, #65185, #144380, #44718, #176832, #210379, #163793, #195218, #145446, #161662, #77184, #162730, #131339, #45787, #178980, #196283, #97736, #160576, #62021, #64152, #29520, #95613, #194137, #30594, #80397, #13257, #159510, #12184, #111904, #60945, #197333, #181089, #48975, #115092, #78256, #147542, #47930, #79329, #114043, #128176, #177907, #14302, #112968, #93471, #211444, #63077, #129245, #127101, #46854, #96680, #212511, #31658, #28446, #130294, #15371, #81464, #213563, #11109, #143306 ),
 ( #110824, #193066, #209297, #198386, #170, #99847, #132386, #36964, #82514, #118287, #149665, #69445, #84654, #185341, #150743, #116152, #148601, #3378, #103045, #182139, #66237, #135553, #117219, #1244, #183217, #184273, #53223, #98788, #16435, #50028, #119354, #85717, #32707, #52160, #33769, #2305, #17496, #165911, #164843, #83583, #133446, #35897, #67305, #101974, #199452, #168042, #51094, #19644, #34822, #100897, #166986, #151804, #18576, #68381, #201577, #134511, #200515, #145053, #164464, #33390, #62681, #32331, #12856, #129917, #81078, #213192, #211056, #99468, #48595, #49644, #132006, #128840, #115767, #112579, #163408, #77874, #31276, #64819, #78931, #98399, #198016, #194821, #177520, #95220, #46457, #82134, #113652, #63757, #80003, #209988, #147165, #181756, #178591, #97351, #114713, #16050, #30199, #96288, #196957, #162340, #13923, #146108, #14983, #130965, #212119, #143996, #195903, #47539, #193751, #11799, #61630, #127796, #45397, #179656, #65856, #180708, #148226, #214228, #111514, #29132, #161270, #118195, #136529, #6490, #4344, #135460, #169009, #104022, #202549, #7558, #200422, #151713, #54199, #22733, #53125, #102949, #106199, #73644, #87762, #120339, #153838, #186315, #167947, #121415, #3282, #5408, #36865, #119258, #172226, #187387, #184183, #20607, #154906, #86693, #39018, #185243, #88849, #152762, #23815, #188456, #72565, #69349, #137599, #52069, #70411, #35803, #37950, #170069, #138663, #101881, #21655, #204685, #201483, #71486, #55268, #105100, #203616, #19548, #56335, #89920, #155972, #171141, #85626, #122494, #40088, #205766, #159160, #192705, #140819, #11827, #111546, #190578, #90985, #8635, #42235, #210020, #27013, #191638, #207897, #123560, #208953, #177555, #92057, #10759, #28093, #144025, #206833, #108349, #110483, #75781, #141888, #25950, #76832, #126746, #59520, #57395, #58466, #158113, #107279, #29164, #12889, #95255, #161305, #124620, #193783, #94189, #125679, #160229, #9704, #45430, #176482, #189524, #139742, #174371, #43302, #109422, #173299, #175427, #93119, #142953, #77904, #74716, #60588, #44361, #61663, #127830, #41170, #24880, #157047, #82164, #214258, #16081, #13954, #115801, #194857, #891, #34485, #146140, #46490, #133097, #64851, #31306, #130998, #49676, #116867, #145087, #128875, #162374, #182869, #83227, #50741, #112612, #178624, #199095, #80037, #180739, #30235, #96320, #165558, #212153, #63789, #129947, #195934, #100559, #47572, #198047, #179687, #66958, #98430, #166630, #164495, #113685, #78967, #62714, #147196, #211091, #97382, #163439, #15019, #81108, #114741, #196988, #213221, #48625, #32366, #148258, #65890, #181789, #132037, #33423, #99501, #17151, #149311, #85377, #183937, #38767, #71235, #72308, #69099, #21414, #202299, #151459, #184991, #201235, #3031, #135223, #52876, #119012, #1961, #36616, #35549, #187138, #153589, #121169, #101628, #102702, #167694 ) ),
 .UNSPECIFIED., .F., .F., .T. ) 
 B_SPLINE_SURFACE_WITH_KNOTS ( ( 2, 2 ),
 ( 3, 2, 2, 2, 2, 2, 2, 2, 2, 2, 2, 2, 2, 2, 2, 2, 2, 2, 2, 2, 2, 2, 2, 2, 2, 2, 2, 2, 2, 2, 2, 2, 2, 2, 2, 2, 2, 2, 2, 2, 2, 2, 2, 2, 2, 2, 2, 2, 2, 2, 2, 2, 2, 2, 2, 2, 2, 2, 2, 2, 2, 2, 2, 2, 2, 2, 2, 2, 2, 2, 2, 2, 2, 2, 2, 2, 2, 2, 2, 2, 2, 2, 2, 2, 2, 2, 2, 2, 2, 2, 2, 2, 2, 2, 2, 2, 2, 2, 2, 2, 2, 2, 2, 2, 2, 2, 2, 2, 2, 2, 2, 2, 2, 2, 2, 2, 2, 2, 2, 2, 2, 2, 2, 2, 2, 2, 2, 2, 2, 2, 2, 2, 2, 2, 2, 2, 2, 2, 2, 2, 2, 2, 2, 2, 2, 2, 2, 2, 2, 2, 2, 2, 2, 2, 2, 2, 2, 2, 2, 2, 2, 2, 2, 2, 2, 2, 2, 2, 3 ),
 ( 0.000000000000000000, 1.000000000000000000 ),
 ( 0.000000000000000000, 0.005952380952380952051, 0.01190476190476190410, 0.01785714285714285615, 0.02380952380952380820, 0.02976190476190476025, 0.03571428571428571230, 0.04166666666666666435, 0.04761904761904761640, 0.05357142857142856845, 0.05952380952380952051, 0.06547619047619047949, 0.07142857142857142461, 0.07738095238095238360, 0.08333333333333332871, 0.08928571428571428770, 0.09523809523809523281, 0.1011904761904761918, 0.1071428571428571369, 0.1130952380952380959, 0.1190476190476190410, 0.1250000000000000000, 0.1309523809523809590, 0.1369047619047619180, 0.1428571428571428492, 0.1488095238095238082, 0.1547619047619047672, 0.1607142857142857262, 0.1666666666666666574, 0.1726190476190476164, 0.1785714285714285754, 0.1845238095238095344, 0.1904761904761904656, 0.1964285714285714246, 0.2023809523809523836, 0.2083333333333333426, 0.2142857142857142738, 0.2202380952380952328, 0.2261904761904761918, 0.2321428571428571508, 0.2380952380952380820, 0.2440476190476190410, 0.2500000000000000000, 0.2559523809523809312, 0.2619047619047619180, 0.2678571428571428492, 0.2738095238095238360, 0.2797619047619047672, 0.2857142857142856984, 0.2916666666666666852, 0.2976190476190476164, 0.3035714285714285476, 0.3095238095238095344, 0.3154761904761904656, 0.3214285714285714524, 0.3273809523809523836, 0.3333333333333333148, 0.3392857142857143016, 0.3452380952380952328, 0.3511904761904761640, 0.3571428571428571508, 0.3630952380952380820, 0.3690476190476190688, 0.3750000000000000000, 0.3809523809523809312, 0.3869047619047619180, 0.3928571428571428492, 0.3988095238095238360, 0.4047619047619047672, 0.4107142857142856984, 0.4166666666666666852, 0.4226190476190476164, 0.4285714285714285476, 0.4345238095238095344, 0.4404761904761904656, 0.4464285714285714524, 0.4523809523809523836, 0.4583333333333333148, 0.4642857142857143016, 0.4702380952380952328, 0.4761904761904761640, 0.4821428571428571508, 0.4880952380952380820, 0.4940476190476190688, 0.5000000000000000000, 0.5059523809523809312, 0.5119047619047618625, 0.5178571428571429047, 0.5238095238095238360, 0.5297619047619047672, 0.5357142857142856984, 0.5416666666666666297, 0.5476190476190476719, 0.5535714285714286031, 0.5595238095238095344, 0.5654761904761904656, 0.5714285714285713969, 0.5773809523809523281, 0.5833333333333333703, 0.5892857142857143016, 0.5952380952380952328, 0.6011904761904761640, 0.6071428571428570953, 0.6130952380952381375, 0.6190476190476190688, 0.6250000000000000000, 0.6309523809523809312, 0.6369047619047618625, 0.6428571428571429047, 0.6488095238095238360, 0.6547619047619047672, 0.6607142857142856984, 0.6666666666666666297, 0.6726190476190476719, 0.6785714285714286031, 0.6845238095238095344, 0.6904761904761904656, 0.6964285714285713969, 0.7023809523809523281, 0.7083333333333333703, 0.7142857142857143016, 0.7202380952380952328, 0.7261904761904761640, 0.7321428571428570953, 0.7380952380952381375, 0.7440476190476190688, 0.7500000000000000000, 0.7559523809523809312, 0.7619047619047618625, 0.7678571428571429047, 0.7738095238095238360, 0.7797619047619047672, 0.7857142857142856984, 0.7916666666666666297, 0.7976190476190476719, 0.8035714285714286031, 0.8095238095238095344, 0.8154761904761904656, 0.8214285714285713969, 0.8273809523809523281, 0.8333333333333333703, 0.8392857142857143016, 0.8452380952380952328, 0.8511904761904761640, 0.8571428571428570953, 0.8630952380952381375, 0.8690476190476190688, 0.8750000000000000000, 0.8809523809523809312, 0.8869047619047618625, 0.8928571428571429047, 0.8988095238095238360, 0.9047619047619047672, 0.9107142857142856984, 0.9166666666666666297, 0.9226190476190476719, 0.9285714285714286031, 0.9345238095238095344, 0.9404761904761904656, 0.9464285714285713969, 0.9523809523809523281, 0.9583333333333333703, 0.9642857142857143016, 0.9702380952380952328, 0.9761904761904761640, 0.9821428571428570953, 0.9880952380952381375, 0.9940476190476190688, 1.000000000000000000 ),
 .UNSPECIFIED. ) 
 GEOMETRIC_REPRESENTATION_ITEM ( )  RATIONAL_B_SPLINE_SURFACE ( (
 ( 1.000000000000000000, 0.8660254037844387076, 1.000000000000000000, 0.8660254037844387076, 1.000000000000000000, 0.8660254037844387076, 1.000000000000000000, 0.8660254037844387076, 1.000000000000000000, 0.8660254037844387076, 1.000000000000000000, 0.8660254037844387076, 1.000000000000000000, 0.8660254037844387076, 1.000000000000000000, 0.8660254037844387076, 1.000000000000000000, 0.8660254037844387076, 1.000000000000000000, 0.8660254037844387076, 1.000000000000000000, 0.8660254037844387076, 1.000000000000000000, 0.8660254037844387076, 1.000000000000000000, 0.8660254037844387076, 1.000000000000000000, 0.8660254037844387076, 1.000000000000000000, 0.8660254037844387076, 1.000000000000000000, 0.8660254037844387076, 1.000000000000000000, 0.8660254037844387076, 1.000000000000000000, 0.8660254037844387076, 1.000000000000000000, 0.8660254037844387076, 1.000000000000000000, 0.8660254037844387076, 1.000000000000000000, 0.8660254037844387076, 1.000000000000000000, 0.8660254037844387076, 1.000000000000000000, 0.8660254037844387076, 1.000000000000000000, 0.8660254037844387076, 1.000000000000000000, 0.8660254037844387076, 1.000000000000000000, 0.8660254037844387076, 1.000000000000000000, 0.8660254037844387076, 1.000000000000000000, 0.8660254037844387076, 1.000000000000000000, 0.8660254037844387076, 1.000000000000000000, 0.8660254037844387076, 1.000000000000000000, 0.8660254037844387076, 1.000000000000000000, 0.8660254037844387076, 1.000000000000000000, 0.8660254037844387076, 1.000000000000000000, 0.8660254037844387076, 1.000000000000000000, 0.8660254037844387076, 1.000000000000000000, 0.8660254037844387076, 1.000000000000000000, 0.8660254037844387076, 1.000000000000000000, 0.8660254037844387076, 1.000000000000000000, 0.8660254037844387076, 1.000000000000000000, 0.8660254037844387076, 1.000000000000000000, 0.8660254037844387076, 1.000000000000000000, 0.8660254037844387076, 1.000000000000000000, 0.8660254037844387076, 1.000000000000000000, 0.8660254037844387076, 1.000000000000000000, 0.8660254037844387076, 1.000000000000000000, 0.8660254037844387076, 1.000000000000000000, 0.8660254037844387076, 1.000000000000000000, 0.8660254037844387076, 1.000000000000000000, 0.8660254037844387076, 1.000000000000000000, 0.8660254037844387076, 1.000000000000000000, 0.8660254037844387076, 1.000000000000000000, 0.8660254037844387076, 1.000000000000000000, 0.8660254037844387076, 1.000000000000000000, 0.8660254037844387076, 1.000000000000000000, 0.8660254037844387076, 1.000000000000000000, 0.8660254037844387076, 1.000000000000000000, 0.8660254037844387076, 1.000000000000000000, 0.8660254037844387076, 1.000000000000000000, 0.8660254037844387076, 1.000000000000000000, 0.8660254037844387076, 1.000000000000000000, 0.8660254037844387076, 1.000000000000000000, 0.8660254037844387076, 1.000000000000000000, 0.8660254037844387076, 1.000000000000000000, 0.8660254037844387076, 1.000000000000000000, 0.8660254037844387076, 1.000000000000000000, 0.8660254037844387076, 1.000000000000000000, 0.8660254037844387076, 1.000000000000000000, 0.8660254037844387076, 1.000000000000000000, 0.8660254037844387076, 1.000000000000000000, 0.8660254037844387076, 1.000000000000000000, 0.8660254037844387076, 1.000000000000000000, 0.8660254037844387076, 1.000000000000000000, 0.8660254037844387076, 1.000000000000000000, 0.8660254037844387076, 1.000000000000000000, 0.8660254037844387076, 1.000000000000000000, 0.8660254037844387076, 1.000000000000000000, 0.8660254037844387076, 1.000000000000000000, 0.8660254037844387076, 1.000000000000000000, 0.8660254037844387076, 1.000000000000000000, 0.8660254037844387076, 1.000000000000000000, 0.8660254037844387076, 1.000000000000000000, 0.8660254037844387076, 1.000000000000000000, 0.8660254037844387076, 1.000000000000000000, 0.8660254037844387076, 1.000000000000000000, 0.8660254037844387076, 1.000000000000000000, 0.8660254037844387076, 1.000000000000000000, 0.8660254037844387076, 1.000000000000000000, 0.8660254037844387076, 1.000000000000000000, 0.8660254037844387076, 1.000000000000000000, 0.8660254037844387076, 1.000000000000000000, 0.8660254037844387076, 1.000000000000000000, 0.8660254037844387076, 1.000000000000000000, 0.8660254037844387076, 1.000000000000000000, 0.8660254037844387076, 1.000000000000000000, 0.8660254037844387076, 1.000000000000000000, 0.8660254037844387076, 1.000000000000000000, 0.8660254037844387076, 1.000000000000000000, 0.8660254037844387076, 1.000000000000000000, 0.8660254037844387076, 1.000000000000000000, 0.8660254037844387076, 1.000000000000000000, 0.8660254037844387076, 1.000000000000000000, 0.8660254037844387076, 1.000000000000000000, 0.8660254037844387076, 1.000000000000000000, 0.8660254037844387076, 1.000000000000000000, 0.8660254037844387076, 1.000000000000000000, 0.8660254037844387076, 1.000000000000000000, 0.8660254037844387076, 1.000000000000000000, 0.8660254037844387076, 1.000000000000000000, 0.8660254037844387076, 1.000000000000000000, 0.8660254037844387076, 1.000000000000000000, 0.8660254037844387076, 1.000000000000000000, 0.8660254037844387076, 1.000000000000000000, 0.8660254037844387076, 1.000000000000000000, 0.8660254037844387076, 1.000000000000000000, 0.8660254037844387076, 1.000000000000000000, 0.8660254037844387076, 1.000000000000000000, 0.8660254037844387076, 1.000000000000000000, 0.8660254037844387076, 1.000000000000000000, 0.8660254037844387076, 1.000000000000000000, 0.8660254037844387076, 1.000000000000000000, 0.8660254037844387076, 1.000000000000000000, 0.8660254037844387076, 1.000000000000000000, 0.8660254037844387076, 1.000000000000000000, 0.8660254037844387076, 1.000000000000000000, 0.8660254037844387076, 1.000000000000000000, 0.8660254037844387076, 1.000000000000000000, 0.8660254037844387076, 1.000000000000000000, 0.8660254037844387076, 1.000000000000000000, 0.8660254037844387076, 1.000000000000000000, 0.8660254037844387076, 1.000000000000000000, 0.8660254037844387076, 1.000000000000000000, 0.8660254037844387076, 1.000000000000000000, 0.8660254037844387076, 1.000000000000000000, 0.8660254037844387076, 1.000000000000000000, 0.8660254037844387076, 1.000000000000000000, 0.8660254037844387076, 1.000000000000000000, 0.8660254037844387076, 1.000000000000000000, 0.8660254037844387076, 1.000000000000000000, 0.8660254037844387076, 1.000000000000000000, 0.8660254037844387076, 1.000000000000000000, 0.8660254037844387076, 1.000000000000000000, 0.8660254037844387076, 1.000000000000000000, 0.8660254037844387076, 1.000000000000000000, 0.8660254037844387076, 1.000000000000000000, 0.8660254037844387076, 1.000000000000000000, 0.8660254037844387076, 1.000000000000000000, 0.8660254037844387076, 1.000000000000000000, 0.8660254037844387076, 1.000000000000000000, 0.8660254037844387076, 1.000000000000000000, 0.8660254037844387076, 1.000000000000000000, 0.8660254037844387076, 1.000000000000000000, 0.8660254037844387076, 1.000000000000000000, 0.8660254037844387076, 1.000000000000000000, 0.8660254037844387076, 1.000000000000000000, 0.8660254037844387076, 1.000000000000000000, 0.8660254037844387076, 1.000000000000000000, 0.8660254037844387076, 1.000000000000000000, 0.8660254037844387076, 1.000000000000000000, 0.8660254037844387076, 1.000000000000000000, 0.8660254037844387076, 1.000000000000000000, 0.8660254037844387076, 1.000000000000000000, 0.8660254037844387076, 1.000000000000000000, 0.8660254037844387076, 1.000000000000000000, 0.8660254037844387076, 1.000000000000000000, 0.8660254037844387076, 1.000000000000000000, 0.8660254037844387076, 1.000000000000000000, 0.8660254037844387076, 1.000000000000000000, 0.8660254037844387076, 1.000000000000000000),
 ( 1.000000000000000000, 0.8660254037844387076, 1.000000000000000000, 0.8660254037844387076, 1.000000000000000000, 0.8660254037844387076, 1.000000000000000000, 0.8660254037844387076, 1.000000000000000000, 0.8660254037844387076, 1.000000000000000000, 0.8660254037844387076, 1.000000000000000000, 0.8660254037844387076, 1.000000000000000000, 0.8660254037844387076, 1.000000000000000000, 0.8660254037844387076, 1.000000000000000000, 0.8660254037844387076, 1.000000000000000000, 0.8660254037844387076, 1.000000000000000000, 0.8660254037844387076, 1.000000000000000000, 0.8660254037844387076, 1.000000000000000000, 0.8660254037844387076, 1.000000000000000000, 0.8660254037844387076, 1.000000000000000000, 0.8660254037844387076, 1.000000000000000000, 0.8660254037844387076, 1.000000000000000000, 0.8660254037844387076, 1.000000000000000000, 0.8660254037844387076, 1.000000000000000000, 0.8660254037844387076, 1.000000000000000000, 0.8660254037844387076, 1.000000000000000000, 0.8660254037844387076, 1.000000000000000000, 0.8660254037844387076, 1.000000000000000000, 0.8660254037844387076, 1.000000000000000000, 0.8660254037844387076, 1.000000000000000000, 0.8660254037844387076, 1.000000000000000000, 0.8660254037844387076, 1.000000000000000000, 0.8660254037844387076, 1.000000000000000000, 0.8660254037844387076, 1.000000000000000000, 0.8660254037844387076, 1.000000000000000000, 0.8660254037844387076, 1.000000000000000000, 0.8660254037844387076, 1.000000000000000000, 0.8660254037844387076, 1.000000000000000000, 0.8660254037844387076, 1.000000000000000000, 0.8660254037844387076, 1.000000000000000000, 0.8660254037844387076, 1.000000000000000000, 0.8660254037844387076, 1.000000000000000000, 0.8660254037844387076, 1.000000000000000000, 0.8660254037844387076, 1.000000000000000000, 0.8660254037844387076, 1.000000000000000000, 0.8660254037844387076, 1.000000000000000000, 0.8660254037844387076, 1.000000000000000000, 0.8660254037844387076, 1.000000000000000000, 0.8660254037844387076, 1.000000000000000000, 0.8660254037844387076, 1.000000000000000000, 0.8660254037844387076, 1.000000000000000000, 0.8660254037844387076, 1.000000000000000000, 0.8660254037844387076, 1.000000000000000000, 0.8660254037844387076, 1.000000000000000000, 0.8660254037844387076, 1.000000000000000000, 0.8660254037844387076, 1.000000000000000000, 0.8660254037844387076, 1.000000000000000000, 0.8660254037844387076, 1.000000000000000000, 0.8660254037844387076, 1.000000000000000000, 0.8660254037844387076, 1.000000000000000000, 0.8660254037844387076, 1.000000000000000000, 0.8660254037844387076, 1.000000000000000000, 0.8660254037844387076, 1.000000000000000000, 0.8660254037844387076, 1.000000000000000000, 0.8660254037844387076, 1.000000000000000000, 0.8660254037844387076, 1.000000000000000000, 0.8660254037844387076, 1.000000000000000000, 0.8660254037844387076, 1.000000000000000000, 0.8660254037844387076, 1.000000000000000000, 0.8660254037844387076, 1.000000000000000000, 0.8660254037844387076, 1.000000000000000000, 0.8660254037844387076, 1.000000000000000000, 0.8660254037844387076, 1.000000000000000000, 0.8660254037844387076, 1.000000000000000000, 0.8660254037844387076, 1.000000000000000000, 0.8660254037844387076, 1.000000000000000000, 0.8660254037844387076, 1.000000000000000000, 0.8660254037844387076, 1.000000000000000000, 0.8660254037844387076, 1.000000000000000000, 0.8660254037844387076, 1.000000000000000000, 0.8660254037844387076, 1.000000000000000000, 0.8660254037844387076, 1.000000000000000000, 0.8660254037844387076, 1.000000000000000000, 0.8660254037844387076, 1.000000000000000000, 0.8660254037844387076, 1.000000000000000000, 0.8660254037844387076, 1.000000000000000000, 0.8660254037844387076, 1.000000000000000000, 0.8660254037844387076, 1.000000000000000000, 0.8660254037844387076, 1.000000000000000000, 0.8660254037844387076, 1.000000000000000000, 0.8660254037844387076, 1.000000000000000000, 0.8660254037844387076, 1.000000000000000000, 0.8660254037844387076, 1.000000000000000000, 0.8660254037844387076, 1.000000000000000000, 0.8660254037844387076, 1.000000000000000000, 0.8660254037844387076, 1.000000000000000000, 0.8660254037844387076, 1.000000000000000000, 0.8660254037844387076, 1.000000000000000000, 0.8660254037844387076, 1.000000000000000000, 0.8660254037844387076, 1.000000000000000000, 0.8660254037844387076, 1.000000000000000000, 0.8660254037844387076, 1.000000000000000000, 0.8660254037844387076, 1.000000000000000000, 0.8660254037844387076, 1.000000000000000000, 0.8660254037844387076, 1.000000000000000000, 0.8660254037844387076, 1.000000000000000000, 0.8660254037844387076, 1.000000000000000000, 0.8660254037844387076, 1.000000000000000000, 0.8660254037844387076, 1.000000000000000000, 0.8660254037844387076, 1.000000000000000000, 0.8660254037844387076, 1.000000000000000000, 0.8660254037844387076, 1.000000000000000000, 0.8660254037844387076, 1.000000000000000000, 0.8660254037844387076, 1.000000000000000000, 0.8660254037844387076, 1.000000000000000000, 0.8660254037844387076, 1.000000000000000000, 0.8660254037844387076, 1.000000000000000000, 0.8660254037844387076, 1.000000000000000000, 0.8660254037844387076, 1.000000000000000000, 0.8660254037844387076, 1.000000000000000000, 0.8660254037844387076, 1.000000000000000000, 0.8660254037844387076, 1.000000000000000000, 0.8660254037844387076, 1.000000000000000000, 0.8660254037844387076, 1.000000000000000000, 0.8660254037844387076, 1.000000000000000000, 0.8660254037844387076, 1.000000000000000000, 0.8660254037844387076, 1.000000000000000000, 0.8660254037844387076, 1.000000000000000000, 0.8660254037844387076, 1.000000000000000000, 0.8660254037844387076, 1.000000000000000000, 0.8660254037844387076, 1.000000000000000000, 0.8660254037844387076, 1.000000000000000000, 0.8660254037844387076, 1.000000000000000000, 0.8660254037844387076, 1.000000000000000000, 0.8660254037844387076, 1.000000000000000000, 0.8660254037844387076, 1.000000000000000000, 0.8660254037844387076, 1.000000000000000000, 0.8660254037844387076, 1.000000000000000000, 0.8660254037844387076, 1.000000000000000000, 0.8660254037844387076, 1.000000000000000000, 0.8660254037844387076, 1.000000000000000000, 0.8660254037844387076, 1.000000000000000000, 0.8660254037844387076, 1.000000000000000000, 0.8660254037844387076, 1.000000000000000000, 0.8660254037844387076, 1.000000000000000000, 0.8660254037844387076, 1.000000000000000000, 0.8660254037844387076, 1.000000000000000000, 0.8660254037844387076, 1.000000000000000000, 0.8660254037844387076, 1.000000000000000000, 0.8660254037844387076, 1.000000000000000000, 0.8660254037844387076, 1.000000000000000000, 0.8660254037844387076, 1.000000000000000000, 0.8660254037844387076, 1.000000000000000000, 0.8660254037844387076, 1.000000000000000000, 0.8660254037844387076, 1.000000000000000000, 0.8660254037844387076, 1.000000000000000000, 0.8660254037844387076, 1.000000000000000000, 0.8660254037844387076, 1.000000000000000000, 0.8660254037844387076, 1.000000000000000000, 0.8660254037844387076, 1.000000000000000000, 0.8660254037844387076, 1.000000000000000000, 0.8660254037844387076, 1.000000000000000000, 0.8660254037844387076, 1.000000000000000000, 0.8660254037844387076, 1.000000000000000000, 0.8660254037844387076, 1.000000000000000000, 0.8660254037844387076, 1.000000000000000000, 0.8660254037844387076, 1.000000000000000000, 0.8660254037844387076, 1.000000000000000000, 0.8660254037844387076, 1.000000000000000000, 0.8660254037844387076, 1.000000000000000000, 0.8660254037844387076, 1.000000000000000000, 0.8660254037844387076, 1.000000000000000000, 0.8660254037844387076, 1.000000000000000000) ) ) 
 REPRESENTATION_ITEM ( '' )  SURFACE ( )  );
#167532 = CARTESIAN_POINT ( 'NONE',  ( 5.157340341976529352, -1.861842412690998039, -1.184373046124863160 ) ) ;
#167533 = ORIENTED_EDGE ( 'NONE', *, *, #107860, .F. ) ;
#167534 = CARTESIAN_POINT ( 'NONE',  ( 4.517835093568582927, -0.5347929126107499043, 1.947652422195633504 ) ) ;
#167535 = CARTESIAN_POINT ( 'NONE',  ( -6.947627372360122955, 7.070263120700404968, 0.000000000000000000 ) ) ;
#167536 = CARTESIAN_POINT ( 'NONE',  ( 4.780875152847498200, 1.674876996157638187, -1.122516304564516565 ) ) ;
#167537 = ORIENTED_EDGE ( 'NONE', *, *, #35147, .T. ) ;
#167538 = CARTESIAN_POINT ( 'NONE',  ( 2.676452114398766291, -1.789519730395791486, -0.5449050523786898026 ) ) ;
#167539 = TOROIDAL_SURFACE ( 'NONE', #50049, 9.580000000000003624, 0.08000000000000000167 ) ;
#167540 = CARTESIAN_POINT ( 'NONE',  ( -10.91812205866965257, -9.932868363016991609, 0.1856806763506273772 ) ) ;
#167541 = CARTESIAN_POINT ( 'NONE',  ( 1.617294888471169312, 1.591762500684265946, 1.059657513450793953 ) ) ;
#167542 = CARTESIAN_POINT ( 'NONE',  ( 0.000000000000000000, 7.000000000000000000, 0.000000000000000000 ) ) ;
#167543 = CARTESIAN_POINT ( 'NONE',  ( -11.55090974143167060, 4.033601484819619110, -5.407241547083907918 ) ) ;
#167544 = CARTESIAN_POINT ( 'NONE',  ( 1.124100812432971934E-16, 1.500000000000001332, -2.025000000000007905 ) ) ;
#167545 = CIRCLE ( 'NONE', #74169, 11.92000000000000171 ) ;
#167546 = CARTESIAN_POINT ( 'NONE',  ( -1.364683531250012516, 2.342708333674752286, 0.7879004041258379498 ) ) ;
#167547 = CARTESIAN_POINT ( 'NONE',  ( 0.2988868148526523383, -0.2362956723594503705, -1.897694653714178781 ) ) ;
#167548 = CARTESIAN_POINT ( 'NONE',  ( 4.421367491832258523, 8.172362817197399210, 0.7216878364870257245 ) ) ;
#167549 = CARTESIAN_POINT ( 'NONE',  ( 2.172246964874047670, -0.9220853831424129510, -1.731647142839589648 ) ) ;
#167550 = DIRECTION ( 'NONE',  ( -0.000000000000000000, -1.000000000000000000, -0.000000000000000000 ) ) ;
#167551 = CARTESIAN_POINT ( 'NONE',  ( -3.959863383643135393, 6.777535159962392086, 1.199719254218452935 ) ) ;
#167552 = CARTESIAN_POINT ( 'NONE',  ( 5.519825572852568030, -0.5132647233585425628, 2.057443900658859182 ) ) ;
#167554 = CARTESIAN_POINT ( 'NONE',  ( -10.78227258717170578, 6.269840026405313793, 4.500979083849748541 ) ) ;
#167553 = CARTESIAN_POINT ( 'NONE',  ( 8.452618703115982512, 11.94880668935564216, 1.199719254218450271 ) ) ;
#167555 = CARTESIAN_POINT ( 'NONE',  ( 0.3329892237508432773, -1.712944741146247063, 0.7519245212838022718 ) ) ;
#167556 = CARTESIAN_POINT ( 'NONE',  ( -1.201851678989727383E-14, 2.821875000341418804, 1.575800808251672791 ) ) ;
#167558 = CARTESIAN_POINT ( 'NONE',  ( 0.7912717950901988484, -0.05365516122857225123, -2.012662812414119706 ) ) ;
#167557 = CIRCLE ( 'NONE', #115829, 10.75000000000000000 ) ;
#167559 = ORIENTED_EDGE ( 'NONE', *, *, #158769, .T. ) ;
#167560 = CARTESIAN_POINT ( 'NONE',  ( 0.6502104730865595483, 1.047635159188778031, 1.839821444870335165 ) ) ;
#167561 = CARTESIAN_POINT ( 'NONE',  ( 11.96846072664349769, 6.616964094891172543, -0.9998397279549741112 ) ) ;
#167562 = CARTESIAN_POINT ( 'NONE',  ( 2.805202726412972858, -1.722705984639979704, 1.148039668612794051 ) ) ;
#167563 = CARTESIAN_POINT ( 'NONE',  ( 4.848976215542928792, 5.686169002002086970, 1.199719254218452047 ) ) ;
#167564 = CARTESIAN_POINT ( 'NONE',  ( 4.736594563127852098, 6.619389305106191834, -1.599625672291273171 ) ) ;
#167565 = VERTEX_POINT ( 'NONE', #148907 ) ;
#167567 = CARTESIAN_POINT ( 'NONE',  ( 3.842846474469570062, 6.570739089268092137, -1.199719254218452047 ) ) ;
#167566 = CARTESIAN_POINT ( 'NONE',  ( 4.558587588987070838, -1.867386427489168055, -0.9401465391167336261 ) ) ;
#167570 = ORIENTED_EDGE ( 'NONE', *, *, #104659, .F. ) ;
#167569 = CARTESIAN_POINT ( 'NONE',  ( 3.035611470257699285, -1.745090209790541191, 0.4855505718092138490 ) ) ;
#167568 = CARTESIAN_POINT ( 'NONE',  ( 2.555444900642935391, 0.4891320457309326075, -1.758753460580727790 ) ) ;
#167571 = CARTESIAN_POINT ( 'NONE',  ( 6.182275136424624229, -1.184133725572718676, 1.862117674348878760 ) ) ;
#167572 = FILL_AREA_STYLE ('',( #15957 ) ) ;
#167573 = CARTESIAN_POINT ( 'NONE',  ( 9.258966325506428063, 13.63624071251986081, -6.830021722722439570 ) ) ;
#167574 = CARTESIAN_POINT ( 'NONE',  ( 5.825267882404531861, -0.05969703229705652925, 2.206138628428089277 ) ) ;
#167575 = CARTESIAN_POINT ( 'NONE',  ( -0.6823417656250039265, 9.380208333674728394, -1.181850606188755259 ) ) ;
#167576 = ORIENTED_EDGE ( 'NONE', *, *, #5717, .T. ) ;
#167577 = CARTESIAN_POINT ( 'NONE',  ( 3.510326737904199135, -1.910220267131033323, -0.09114558060911714943 ) ) ;
#167578 = CARTESIAN_POINT ( 'NONE',  ( -2.774614992291035698, 6.388801257648172971, 1.040834085586084257E-14 ) ) ;
#167579 = CARTESIAN_POINT ( 'NONE',  ( 6.598014311344812199, 10.84943379654430906, 1.040834085586084257E-14 ) ) ;
#167580 = MECHANICAL_DESIGN_GEOMETRIC_PRESENTATION_REPRESENTATION (  '', ( #112307 ), #63839 ) ;
#167581 = CARTESIAN_POINT ( 'NONE',  ( 1.360316468749971364, 0.04687500034143698979, -3.469446951953614189E-14 ) ) ;
#167582 = CARTESIAN_POINT ( 'NONE',  ( 4.975479186090852046, 6.827811688571220117, 1.443375672974062551 ) ) ;
#167583 = DIRECTION ( 'NONE',  ( 0.000000000000000000, 1.000000000000000000, 0.000000000000000000 ) ) ;
#167584 = CARTESIAN_POINT ( 'NONE',  ( 7.679631683607862414, 14.45130440965375662, -9.163852989591987352 ) ) ;
#167585 = CARTESIAN_POINT ( 'NONE',  ( -8.804225388950451148, 15.46908216042836060, -8.203526012298418379 ) ) ;
#167586 = CARTESIAN_POINT ( 'NONE',  ( -11.89835103415199313, 12.27106914167534057, -1.561208891256348652 ) ) ;
#167587 = CARTESIAN_POINT ( 'NONE',  ( 3.426877311086639288, 0.04264493303338459662, 1.870215716092846314 ) ) ;
#167588 = CARTESIAN_POINT ( 'NONE',  ( 1.500000000000001332, 10.87499999999999645, 0.000000000000000000 ) ) ;
#167589 = CARTESIAN_POINT ( 'NONE',  ( -0.2409995289980224054, 7.629137130509101361, -2.600476469121244527 ) ) ;
#167591 = CARTESIAN_POINT ( 'NONE',  ( -7.727784370109414880, 8.118095974656867497, 0.7216878364870578100 ) ) ;
#167590 = COLOUR_RGB ( '', 0.40784314, 0.44705882, 0.49803922) ;
#167592 = CARTESIAN_POINT ( 'NONE',  ( -11.86145016429273014, 12.69999999999999929, -1.100000000000000311 ) ) ;
#167593 = CARTESIAN_POINT ( 'NONE',  ( 4.822949958159288286, 6.649860922651058992, -1.599625672291256295 ) ) ;
#167594 = CARTESIAN_POINT ( 'NONE',  ( 0.5847281401991512029, 1.882922653073782815, 0.5772291209212175866 ) ) ;
#167595 = CARTESIAN_POINT ( 'NONE',  ( 0.9840001696646907270, -2.016598147255070472, 0.002831364411433334727 ) ) ;
#167596 = CARTESIAN_POINT ( 'NONE',  ( -10.14557902172788495, 10.73093036830436553, 1.040834085586084257E-14 ) ) ;
#167597 = CARTESIAN_POINT ( 'NONE',  ( 7.205232291019763480, 7.370802192470005565, -0.7998128361456341429 ) ) ;
#167598 = CARTESIAN_POINT ( 'NONE',  ( 2.889872605471108802, 6.605953636083950364, -2.500000000000002220 ) ) ;
#167599 = CARTESIAN_POINT ( 'NONE',  ( 0.9904705247469265394, -0.5356807779838267392, -2.124848333686576662 ) ) ;
#167600 = CARTESIAN_POINT ( 'NONE',  ( 6.270122753791413928, 0.9430518052575274091, 1.563124558401955300 ) ) ;
#167601 = CARTESIAN_POINT ( 'NONE',  ( -2.676845263694313637, 5.210404343363602919, -1.199719254218446718 ) ) ;
#167602 = AXIS2_PLACEMENT_3D ( 'NONE', #59131, #43974, #172904 ) ;
#167603 = CARTESIAN_POINT ( 'NONE',  ( 4.584065335196261692, 7.401807753487379848, 1.082531754730549078 ) ) ;
#167604 = CARTESIAN_POINT ( 'NONE',  ( 9.582915646760733708, 10.07448976417602893, 0.7998128361456462443 ) ) ;
#167605 = CARTESIAN_POINT ( 'NONE',  ( 4.325214697959421706, 5.004837554829479451, 1.199719254218462483 ) ) ;
#167606 = CARTESIAN_POINT ( 'NONE',  ( 5.885648082108177803, 9.880690172519326353, 0.7216878364870317197 ) ) ;
#167607 = ORIENTED_EDGE ( 'NONE', *, *, #144373, .F. ) ;
#167609 = CARTESIAN_POINT ( 'NONE',  ( 0.5748582965167781111, -1.456639466575420538, 1.389732462146851200 ) ) ;
#167608 = CARTESIAN_POINT ( 'NONE',  ( 3.614658571667620279, -0.1319153736358945894, 1.836568937333193485 ) ) ;
#167610 = CARTESIAN_POINT ( 'NONE',  ( 2.917634960997887994, 0.7719352619847442698, 2.165007881682521784 ) ) ;
#167612 = CARTESIAN_POINT ( 'NONE',  ( 0.9185399124422718442, -1.353032588479759157, 1.277947871810279246 ) ) ;
#167611 = CARTESIAN_POINT ( 'NONE',  ( 3.189213936345663747, 2.817530495244580102, -2.450448857954562243 ) ) ;
#167613 = CARTESIAN_POINT ( 'NONE',  ( -3.285556943750000070, -3.959374999522043304, 0.000000000000000000 ) ) ;
#167614 = CARTESIAN_POINT ( 'NONE',  ( -5.362413449404877852, 6.214902764849178141, -1.199719254218446718 ) ) ;
#167615 = LINE ( 'NONE', #5076, #88142 ) ;
#167616 = CARTESIAN_POINT ( 'NONE',  ( 4.763870730211980487, 0.5944114921396548290, -1.817767169311027997 ) ) ;
#167617 = CARTESIAN_POINT ( 'NONE',  ( -9.592557376868645846, 11.15007068022363157, -1.199719254218441611 ) ) ;
#167618 = CARTESIAN_POINT ( 'NONE',  ( 6.206332990038123221, 6.936436922908462144, -0.8583981852504622978 ) ) ;
#167619 = CARTESIAN_POINT ( 'NONE',  ( -6.834718835064852449, 8.106831741398025315, 1.082531754730549078 ) ) ;
#167621 = CARTESIAN_POINT ( 'NONE',  ( 1.902992089709685031, 1.553661375375714471, 1.041555772207984676 ) ) ;
#167620 = CARTESIAN_POINT ( 'NONE',  ( 3.579701903670178709, -1.028438467219190411, 1.820211688285853446 ) ) ;
#167622 = CARTESIAN_POINT ( 'NONE',  ( 6.805829924380108586, 8.963220883242035697, 1.443375672974076540 ) ) ;
#167623 = LINE ( 'NONE', #181716, #70623 ) ;
#167624 = CARTESIAN_POINT ( 'NONE',  ( 2.665247472508886606, 0.9327722559238416089, 1.469172323213832065 ) ) ;
#167625 = CARTESIAN_POINT ( 'NONE',  ( 2.984766373302843778, 6.633977868828633717, -0.7998128361456291469 ) ) ;
#167626 = CARTESIAN_POINT ( 'NONE',  ( 4.353923116202039978, 1.724447095217627401, -0.04574849716902986557 ) ) ;
#167627 = CARTESIAN_POINT ( 'NONE',  ( -6.388916700537716764, 8.476822122092563916, 1.599625672291283607 ) ) ;
#167628 = CARTESIAN_POINT ( 'NONE',  ( 4.159861740090546434, 1.033864333764370702, 1.932389678422803181 ) ) ;
#167629 = CARTESIAN_POINT ( 'NONE',  ( 6.041676539500916654, -1.595688354349385607, -1.524751901930617715 ) ) ;
#167630 = CARTESIAN_POINT ( 'NONE',  ( 0.000000000000000000, -8.233137084989836652, 0.000000000000000000 ) ) ;
#167631 = CARTESIAN_POINT ( 'NONE',  ( 3.995131740874768411, 0.3131294011963717816, 2.148239739743092347 ) ) ;
#167632 = CARTESIAN_POINT ( 'NONE',  ( 2.139018802738294589, -1.631172329757241801, 0.8201644002571031322 ) ) ;
#167633 = CARTESIAN_POINT ( 'NONE',  ( 3.104453987849314700, 4.644948957289396496, 0.000000000000000000 ) ) ;
#167634 = CARTESIAN_POINT ( 'NONE',  ( 5.155504860159462410, 2.039786097693491396, -0.5674642188294597434 ) ) ;
#167635 = VERTEX_POINT ( 'NONE', #134814 ) ;
#167637 = CARTESIAN_POINT ( 'NONE',  ( 1.364683531249990311, 2.696875000341415696, 1.214306433183764966E-14 ) ) ;
#167636 = CARTESIAN_POINT ( 'NONE',  ( 5.970342212645192603, -2.175549559325986149, -0.7227481681704952532 ) ) ;
#167638 = CARTESIAN_POINT ( 'NONE',  ( 2.367870383881045981, 5.914265881169853856, 0.000000000000000000 ) ) ;
#167639 = CARTESIAN_POINT ( 'NONE',  ( 1.049659257133638945, -1.915429643647760249, 0.9100379840868355608 ) ) ;
#167640 = CARTESIAN_POINT ( 'NONE',  ( -5.450014563013544588, 5.460697866378308341, 0.7216878364870317197 ) ) ;
#167641 = EDGE_CURVE ( 'NONE', #159908, #40273, #180441, .T. ) ;
#167642 = CARTESIAN_POINT ( 'NONE',  ( 3.226477370372305753, 4.787309570232886280, 1.443375672974062551 ) ) ;
#167643 = CARTESIAN_POINT ( 'NONE',  ( -4.867013957181525186, 8.622007350113015889, 0.7216878364870458196 ) ) ;
#167645 = CARTESIAN_POINT ( 'NONE',  ( -0.7500000000000179856, 12.82291666734946389, 1.299038105676658228 ) ) ;
#167644 = DIRECTION ( 'NONE',  ( -1.000000000000000000, 7.109522442527888164E-16, 0.000000000000000000 ) ) ;
#167647 = ORIENTED_EDGE ( 'NONE', *, *, #96671, .T. ) ;
#167646 = CARTESIAN_POINT ( 'NONE',  ( 1.735333443468607184, 2.074102030253548445, 0.7956244722606919950 ) ) ;
#167648 = CARTESIAN_POINT ( 'NONE',  ( 6.100232455412330168, -0.2440331339308223768, 2.001510902166554473 ) ) ;
#167650 = CARTESIAN_POINT ( 'NONE',  ( 4.469619655223175947, -0.3576850913847802182, 2.031185480813563426 ) ) ;
#167649 = CARTESIAN_POINT ( 'NONE',  ( 4.416205349749311004, 6.175325546172740765, 1.599625672291267398 ) ) ;
#167652 = CARTESIAN_POINT ( 'NONE',  ( -0.2409995289980246258, 1.355929887833319469, -2.254219809973062816 ) ) ;
#167651 = CARTESIAN_POINT ( 'NONE',  ( 5.342795052237045539, 8.390955439988655229, -1.199719254218450271 ) ) ;
#167653 = CARTESIAN_POINT ( 'NONE',  ( 5.677832469072920496, 9.846164657218904992, 0.000000000000000000 ) ) ;
#167654 = CARTESIAN_POINT ( 'NONE',  ( -3.285556943749998737, -1.480208332855375453, 1.896917185911908499 ) ) ;
#167655 =( NAMED_UNIT ( * ) PLANE_ANGLE_UNIT ( ) SI_UNIT ( $, .RADIAN. ) );
#167656 = CARTESIAN_POINT ( 'NONE',  ( 0.5684512833941969268, -1.969177116664261762, -0.7025944222667882544 ) ) ;
#167657 = CARTESIAN_POINT ( 'NONE',  ( 4.729138786257041538, 2.011204126674607462, 0.1455352507326590494 ) ) ;
#167658 = CARTESIAN_POINT ( 'NONE',  ( 4.071694929070113211, -1.056692140236010102, 1.507659738195665788 ) ) ;
#167659 = CARTESIAN_POINT ( 'NONE',  ( 6.657217119509961201, 7.725507046638470321, -1.199719254218446718 ) ) ;
#167660 = CARTESIAN_POINT ( 'NONE',  ( 1.008351294761783423, 1.310062561100222123, -1.121974927168223335 ) ) ;
#167661 = CARTESIAN_POINT ( 'NONE',  ( -0.2351498743046881446, -0.1506043639611966134, -1.983733596389973597 ) ) ;
#167662 = CARTESIAN_POINT ( 'NONE',  ( 1.266696122786495904, 2.121433860451333420, -0.8855928530677835697 ) ) ;
#167663 = CARTESIAN_POINT ( 'NONE',  ( -4.740547266272593596, 8.682388910626682943, -0.7998128361456281477 ) ) ;
#167664 = CARTESIAN_POINT ( 'NONE',  ( 1.142281600899584193, 0.9165754381605104584, -2.068608644781688710 ) ) ;
#167665 = CARTESIAN_POINT ( 'NONE',  ( 3.123755640277770418, -2.029568314945415786, 0.5621985482912382759 ) ) ;
#167666 = CARTESIAN_POINT ( 'NONE',  ( -4.634908411025374875, 6.500755460986618495, 1.599625672291263179 ) ) ;
#167667 = CARTESIAN_POINT ( 'NONE',  ( 6.636879889089462026, 7.701780277814560982, -1.199719254218446718 ) ) ;
#167668 = CARTESIAN_POINT ( 'NONE',  ( 5.926322542504858681, 8.007405281046052536, -1.443375672974078761 ) ) ;
#167669 = CARTESIAN_POINT ( 'NONE',  ( 6.593749840436431420, -1.895867669153237456, -0.7852924748296338242 ) ) ;
#167670 = CARTESIAN_POINT ( 'NONE',  ( -4.629219384062206011, 7.488174150459498968, -1.199719254218452047 ) ) ;
#167671 = CARTESIAN_POINT ( 'NONE',  ( 6.927853306458749749, 8.145212281365775908, 1.082531754730558626 ) ) ;
#167672 = CARTESIAN_POINT ( 'NONE',  ( 4.981510052282690282, 6.816019998287410786, 1.424969591591069396 ) ) ;
#167673 = CARTESIAN_POINT ( 'NONE',  ( -3.785751206713858785, 5.439795712631356750, 1.599625672291267398 ) ) ;
#167674 = CARTESIAN_POINT ( 'NONE',  ( 5.449557989901563815, -2.008192194917140849, 0.9499826718327757380 ) ) ;
#167675 = CARTESIAN_POINT ( 'NONE',  ( 3.873126987144244193, 2.063651454400210028, -0.7377723227853100196 ) ) ;
#167677 = EDGE_CURVE ( 'NONE', #15524, #65102, #147984, .T. ) ;
#167676 = CARTESIAN_POINT ( 'NONE',  ( -6.573005544526917099, 6.562927978236513304, -0.7998128361456291469 ) ) ;
#167678 = CARTESIAN_POINT ( 'NONE',  ( -10.50000000000000000, 13.40000000000000036, -3.600000000000002309 ) ) ;
#167679 = CARTESIAN_POINT ( 'NONE',  ( 5.635196431686764207, -0.04651148872366302894, -1.961470878453225763 ) ) ;
#167680 = CARTESIAN_POINT ( 'NONE',  ( -0.6823417656250003738, 2.217708333674753174, -1.181850606188749264 ) ) ;
#167681 = CARTESIAN_POINT ( 'NONE',  ( 6.890000000000005898, 2.048573291599069091, 2.305811639209849773 ) ) ;
#167682 = CARTESIAN_POINT ( 'NONE',  ( -4.609409038966245653, 6.400729850259146758, -1.443375672974053447 ) ) ;
#167683 = CARTESIAN_POINT ( 'NONE',  ( 4.746395313581045272, 1.087821826000658909, -1.820160695957805608 ) ) ;
#167684 = CARTESIAN_POINT ( 'NONE',  ( -7.946487431385463651, 8.443525889470736345, 0.7216878364870317197 ) ) ;
#167685 = ORIENTED_EDGE ( 'NONE', *, *, #184597, .T. ) ;
#167686 = CARTESIAN_POINT ( 'NONE',  ( -5.261973015879593873, 8.192700047617899273, 1.082531754730549967 ) ) ;
#167687 = CARTESIAN_POINT ( 'NONE',  ( 4.924636110261782385, 6.768494766770632332, 1.599625672291267398 ) ) ;
#167688 = CARTESIAN_POINT ( 'NONE',  ( 4.827609030688454261, 0.9420861819694618111, -1.581835861328761528 ) ) ;
#167689 = UNCERTAINTY_MEASURE_WITH_UNIT (LENGTH_MEASURE( 1.000000000000000082E-05 ), #213440, 'distance_accuracy_value', 'NONE');
#167690 = DIRECTION ( 'NONE',  ( 0.000000000000000000, 1.000000000000000000, 0.000000000000000000 ) ) ;
#167691 = CARTESIAN_POINT ( 'NONE',  ( -1.364683531250012516, 2.842708333674754506, 0.7879004041258379498 ) ) ;
#167692 = CARTESIAN_POINT ( 'NONE',  ( 1.223704041615133464, 1.677047869609141983, 0.4652235607782040372 ) ) ;
#167693 = CARTESIAN_POINT ( 'NONE',  ( 1.274579945453880647, 3.715243558054538653, 0.4827076737218298219 ) ) ;
#167694 = CARTESIAN_POINT ( 'NONE',  ( -1.364683531250000748, -1.178124999658580752, 0.000000000000000000 ) ) ;
#167695 = FACE_OUTER_BOUND ( 'NONE', #794, .T. ) ;
#167696 = CARTESIAN_POINT ( 'NONE',  ( 5.770447993230207295, -1.374857387916775364, 1.668144713590607120 ) ) ;
#167697 = CIRCLE ( 'NONE', #39843, 0.08000000000000020983 ) ;
#167698 = CARTESIAN_POINT ( 'NONE',  ( -3.273404022695637572, 5.906389562198459231, 1.199719254218462483 ) ) ;
#167699 = CARTESIAN_POINT ( 'NONE',  ( -7.836249598574384301, 8.244638741199329601, 1.040834085586084257E-14 ) ) ;
#167700 = CARTESIAN_POINT ( 'NONE',  ( 4.926735330553584369, 2.067573386176469796, 0.6309256262674377558 ) ) ;
#167701 = CARTESIAN_POINT ( 'NONE',  ( 0.6823417656249882723, 2.926041667008084879, -1.181850606188754593 ) ) ;
#167702 = CARTESIAN_POINT ( 'NONE',  ( 5.184826486558015368, -0.2386506126292788632, -1.956774853079599197 ) ) ;
#167703 = CARTESIAN_POINT ( 'NONE',  ( 4.112396791320716005, 0.5851491843551993588, -1.632232688200731197 ) ) ;
#167704 = CIRCLE ( 'NONE', #70872, 0.1000000000000000333 ) ;
#167705 = CARTESIAN_POINT ( 'NONE',  ( 1.259612756803454525, 2.158328104161820526, -0.3793702838810895095 ) ) ;
#167706 = CARTESIAN_POINT ( 'NONE',  ( 2.274872074667996458, -1.419342104801555982, 1.819364073307845997 ) ) ;
#167707 = CARTESIAN_POINT ( 'NONE',  ( 4.639950097937448170, 0.8846809987467202374, -1.861387103252240660 ) ) ;
#167708 = CARTESIAN_POINT ( 'NONE',  ( 6.409718653046240000, -0.9196952807892575521, -1.710506293091022201 ) ) ;
#167709 = CARTESIAN_POINT ( 'NONE',  ( -7.714226216051410567, 9.062647342557177410, 1.082531754730558626 ) ) ;
#167710 = CARTESIAN_POINT ( 'NONE',  ( -6.466312919074983512, 6.508729591867735031, -0.7998128361456362523 ) ) ;
#167711 = CARTESIAN_POINT ( 'NONE',  ( -9.585712967628772674, 15.23494795713225436, 7.219336745831919977 ) ) ;
#167712 = EDGE_CURVE ( 'NONE', #141673, #70696, #31724, .T. ) ;
#167713 = SURFACE_STYLE_USAGE ( .BOTH. , #101646 ) ;
#167714 = CARTESIAN_POINT ( 'NONE',  ( 1.213517774399593740, 1.944071949784083264, 0.5350861613380719639 ) ) ;
#167715 = CARTESIAN_POINT ( 'NONE',  ( -7.687109908824056426, 8.070642436490613747, 0.7216878364870438212 ) ) ;
#167716 = CARTESIAN_POINT ( 'NONE',  ( 3.434799832723956836, 2.152550277175222515, 0.4854691814954179563 ) ) ;
#167717 = CARTESIAN_POINT ( 'NONE',  ( -3.285556943749998737, -1.567708332855375142, 1.896917185911908499 ) ) ;
#167718 = CARTESIAN_POINT ( 'NONE',  ( 1.305250306655120207, -1.462593314309963866, -1.150481100809984891 ) ) ;
#167719 =( BOUNDED_CURVE ( )  B_SPLINE_CURVE ( 3, ( #114762, #164515, #35564, #165577 ),
 .UNSPECIFIED., .F., .T. ) 
 B_SPLINE_CURVE_WITH_KNOTS ( ( 4, 4 ),
 ( 0.4999999999999995004, 1.000000000000000000 ),
 .UNSPECIFIED. ) 
 CURVE ( )  GEOMETRIC_REPRESENTATION_ITEM ( )  RATIONAL_B_SPLINE_CURVE ( ( 1.000000000000000444, 0.3333333333333333148, 0.3333333333333326487, 1.000000000000000000 ) ) 
 REPRESENTATION_ITEM ( '' )  );
#167720 = CIRCLE ( 'NONE', #185014, 11.68000000000000149 ) ;
#167721 = CARTESIAN_POINT ( 'NONE',  ( -0.1263102688159843667, 6.363441598446241798, 3.117922131261609664 ) ) ;
#167722 = CARTESIAN_POINT ( 'NONE',  ( -9.499668754385638181, -7.473374494045003757, -0.07933194154487506478 ) ) ;
#167724 = CARTESIAN_POINT ( 'NONE',  ( 6.925078400183537042, 4.686282476709005884, 2.806848198465234479 ) ) ;
#167723 = CARTESIAN_POINT ( 'NONE',  ( -4.609429383499759503, 8.467968972964683871, -0.3232828671759068739 ) ) ;
#167725 = CARTESIAN_POINT ( 'NONE',  ( 6.597600327481837112, -1.840612352326329804, 0.05063316525460298534 ) ) ;
#167726 = VERTEX_POINT ( 'NONE', #107455 ) ;
#167727 = CARTESIAN_POINT ( 'NONE',  ( 3.256764320543267921, -1.561506546599530143, 1.345091337369247242 ) ) ;
#167728 = CARTESIAN_POINT ( 'NONE',  ( 0.6801582343749865700, 2.307291667008083635, -1.178068619123879834 ) ) ;
#167729 = CARTESIAN_POINT ( 'NONE',  ( -4.693093728624763372, 8.627026450037540428, 0.7998128361456481317 ) ) ;
#167730 = CARTESIAN_POINT ( 'NONE',  ( 1.893228994919902153, -0.1012422250811425839, -2.017274448259358977 ) ) ;
#167731 = CARTESIAN_POINT ( 'NONE',  ( -1.500000000000001332, -0.09999999999997510880, 0.000000000000000000 ) ) ;
#167732 = CARTESIAN_POINT ( 'NONE',  ( 5.020596955762157698, 4.751784624677624080, 1.040834085586084257E-14 ) ) ;
#167733 = CARTESIAN_POINT ( 'NONE',  ( 2.465760480296646850, 2.021364445465044124, -0.4007626210408669620 ) ) ;
#167734 = EDGE_CURVE ( 'NONE', #148685, #18470, #163138, .T. ) ;
#167736 = CARTESIAN_POINT ( 'NONE',  ( -1.364683531250014514, 13.58854166700806587, -0.7879004041258335089 ) ) ;
#167735 = LINE ( 'NONE', #66999, #163032 ) ;
#167737 = CARTESIAN_POINT ( 'NONE',  ( 5.686755365928134687, 8.721966129303114101, 1.199719254218462483 ) ) ;
#167738 = CARTESIAN_POINT ( 'NONE',  ( -0.2409995289980003397, 0.7158067089181943121, -2.082568332340509087 ) ) ;
#167739 = VECTOR ( 'NONE', #202139, 1000.000000000000000 ) ;
#167740 = CARTESIAN_POINT ( 'NONE',  ( 5.514374426699260923, -0.9893691592960799364, -1.972764877262770833 ) ) ;
#167741 = CARTESIAN_POINT ( 'NONE',  ( 5.688527969385528849, 8.794310509995222347, -1.199719254218452047 ) ) ;
#167742 = CARTESIAN_POINT ( 'NONE',  ( 1.317891493549529391, -2.109231647155560108, 0.4722262556789079135 ) ) ;
#167743 = CARTESIAN_POINT ( 'NONE',  ( -5.151735183512911043, 6.073074471262228435, 1.082531754730548412 ) ) ;
#167744 = CARTESIAN_POINT ( 'NONE',  ( 2.061732777098632230, 1.244387006429502396, 1.586668050434843158 ) ) ;
#167745 = CARTESIAN_POINT ( 'NONE',  ( 2.267358445155386981, -2.297842707097216053, 0.05573287391750710029 ) ) ;
#167746 = CARTESIAN_POINT ( 'NONE',  ( -0.5707955116133547335, 6.595905893872795467, 3.427874525163681074 ) ) ;
#167747 = DIRECTION ( 'NONE',  ( -0.6249999999999993339, 2.638740015698311463E-15, 0.7806247497998004548 ) ) ;
#167748 = CARTESIAN_POINT ( 'NONE',  ( 2.377632874612686020, 1.149002834218125102, 1.476114537088555112 ) ) ;
#167749 = AXIS2_PLACEMENT_3D ( 'NONE', #68668, #84941, #147830 ) ;
#167750 = CARTESIAN_POINT ( 'NONE',  ( 3.151577601795185757, 1.966304690962265234, -0.4465026806126579095 ) ) ;
#167751 = CARTESIAN_POINT ( 'NONE',  ( -1.364683531250000748, 1.509375000341421691, 0.000000000000000000 ) ) ;
#167753 = CARTESIAN_POINT ( 'NONE',  ( 5.637368906844186789, -1.904612104999114708, 0.8991850809280316215 ) ) ;
#167752 = CARTESIAN_POINT ( 'NONE',  ( -8.701635661872465732, 9.046329781806354831, 1.040834085586084257E-14 ) ) ;
#167754 = EDGE_CURVE ( 'NONE', #147625, #30835, #31750, .T. ) ;
#167755 = CARTESIAN_POINT ( 'NONE',  ( 7.955937213120826357, 8.176348258262782664, 0.7998128361456481317 ) ) ;
#167756 = CARTESIAN_POINT ( 'NONE',  ( -8.213542131780492639, 8.476887330032372603, 1.040834085586084257E-14 ) ) ;
#167757 = CARTESIAN_POINT ( 'NONE',  ( 6.539320575229280230, 7.629137130509070275, 2.703262396134015866 ) ) ;
#167758 = CARTESIAN_POINT ( 'NONE',  ( 5.010023637874760460, -0.7231455074051349463, 1.886094130455595375 ) ) ;
#167759 = CARTESIAN_POINT ( 'NONE',  ( -1.001543065824772872E-14, 5.571875000341416140, 1.575800808251672791 ) ) ;
#167760 = AXIS2_PLACEMENT_3D ( 'NONE', #158040, #204610, #159087 ) ;
#167761 = EDGE_CURVE ( 'NONE', #102576, #182627, #3986, .T. ) ;
#167762 = CARTESIAN_POINT ( 'NONE',  ( 1.164971494057164492, 1.564520514315300481, -1.344193796132137964 ) ) ;
#167763 = CARTESIAN_POINT ( 'NONE',  ( 6.778713617152772208, 10.85232362007950258, -0.7216878364870267237 ) ) ;
#167764 = CARTESIAN_POINT ( 'NONE',  ( 7.205232291019763480, 7.370802192470005565, -0.7998128361456341429 ) ) ;
#167765 = CARTESIAN_POINT ( 'NONE',  ( 5.468734858265785093, 7.473552982767158070, 1.599625672291269396 ) ) ;
#167766 = CARTESIAN_POINT ( 'NONE',  ( -1.364683531250000748, 0.07187500034142035865, 0.000000000000000000 ) ) ;
#167768 = CARTESIAN_POINT ( 'NONE',  ( 9.367496997597594799, 3.481548657788670731, -7.500000000000007105 ) ) ;
#167767 = CARTESIAN_POINT ( 'NONE',  ( 6.391743074199808916, 6.421731439513382433, -0.7998128361456481317 ) ) ;
#167769 = CARTESIAN_POINT ( 'NONE',  ( 8.229436053370683624, 8.703356271795033905, 0.7216878364870458196 ) ) ;
#167770 = CARTESIAN_POINT ( 'NONE',  ( 3.315042099977282497, -1.646035655820307309, 1.415953490726479469 ) ) ;
#167772 = CARTESIAN_POINT ( 'NONE',  ( 1.364538772237647413, 0.1349417713633893900, -1.836341338755695940 ) ) ;
#167771 = CARTESIAN_POINT ( 'NONE',  ( -3.782361668532609134, 7.356579680022602652, 1.040834085586084257E-14 ) ) ;
#167773 = MANIFOLD_SOLID_BREP ( 'Fillet1', #178179 ) ;
#167774 = CARTESIAN_POINT ( 'NONE',  ( 1.364683531249988535, 2.863541667008082658, 0.7879004041258500513 ) ) ;
#167776 = CARTESIAN_POINT ( 'NONE',  ( 4.669572502782517454, 1.262004115398765780, 1.791526714441132873 ) ) ;
#167775 = B_SPLINE_CURVE_WITH_KNOTS ( 'NONE', 3,
 ( #152088, #3658, #125003, #141212, #159548, #92450, #62060, #143341, #111943, #209335, #107668, #109807, #175816, #177945, #58847, #27409, #157434, #145485, #77222, #93507, #11145, #210418, #9027, #108735, #78289, #76162, #79367, #173696, #158489, #60983, #127137, #193109, #128215, #29559, #25272, #28483, #211481, #10088, #44758, #142267, #26336, #75102, #110865, #91374, #176871, #94574, #42625, #174763, #45822, #95650, #207223, #160617, #12218, #161701, #208278, #59910, #63117, #144416, #126064, #194177, #190960, #192027, #43690, #13294, #129282, #195256, #68419, #81500, #32745, #164877, #16472, #15409, #146534, #18613, #100932, #147578, #34857, #167019, #130333, #165946, #82552, #132423, #47966, #30632, #196322, #162767, #212551, #150780, #114082, #50068, #17530, #213597, #80434, #199487, #149701, #14345, #180073, #83619, #65221, #84692, #113006, #182176, #131373, #116191, #33805, #1282, #197369, #148639, #99884, #134546, #205, #49011, #2342, #31696, #64192, #67340, #179016, #98828, #133485, #97771, #163831, #46892, #96718, #198424, #51133, #115130, #181125, #66275, #117254, #183254, #201610, #203747, #200550, #151839, #85759, #204812, #88977, #56463, #53260, #169137, #22864, #104154, #170202, #20732, #3416, #172351, #40219, #86827, #188586, #106328, #69482, #105230, #21786, #72697, #35933, #152891, #135590, #137728, #54334, #87895, #5535, #52197, #155032, #7689, #119390, #171270, #55392, #138792, #122625, #23941, #6617, #118323, #73772, #184309, #90045, #71615, #4469, #121547, #185378, #102011, #120473, #202685, #153968, #136660, #187518, #156103, #186445, #168081, #19679, #39149, #36998, #38082, #103081, #70541, #193915, #191774, #45562, #190708, #176614, #94319, #61794, #43430, #124748, #160360, #175558, #144160, #27149, #13022, #41303, #142012, #93253, #75909, #159287, #110614, #208027, #107411, #189652, #10886, #76961, #59655, #143087, #125812, #11963, #95390, #29296, #42369, #173434, #157175, #25014, #109554, #108480, #78036, #209080, #210152, #60717, #139868, #126880, #192838, #127962, #91116, #44497, #28226, #111678, #174504, #8769, #177685, #161441, #74852, #140951, #205899, #26080, #57533, #123690, #92195, #206964, #58593, #158243, #9833, #1017, #79099, #214382, #166755, #197111, #113814, #50869, #80167, #194988, #82287, #211223, #131123, #66012, #14077, #146273, #17274, #67081, #145217, #164620, #132161, #133216, #130074, #63918, #162507, #112744, #49800, #198167, #179814, #62849, #129011, #32485, #115926, #181914, #100677, #31433, #64969, #48750, #114863, #47700, #178757, #116991, #199222, #97510, #46623, #30369, #163568, #83350, #180864, #16205, #98559, #81237, #148381, #33546, #212284, #147319, #96456, #196069, #99619, #15151, #213346, #165685, #149435, #182991, #34608, #122363, #18351, #39960, #6356, #202416, #103891, #119128, #169939, #35671, #3148, #21523, #52992, #151581, #167816, #136400, #38883, #118066, #102820, #104968, #19416, #171009, #72426, #84429, #87635, #5275, #138528, #69218, #135337, #188319, #153706, #85494, #71352, #150518, #184052, #101749, #22606, #121280, #88714, #201351, #185108, #4215, #54071, #120206, #36733, #168875, #204551, #56200, #20479, #106067, #2079, #86566, #137468, #186181, #154773, #68152, #152628, #70284, #203482, #37815, #55135, #134286, #200291, #187256, #51942, #173171 ),
 .UNSPECIFIED., .F., .F.,
 ( 4, 1, 1, 1, 1, 1, 1, 1, 1, 1, 1, 1, 1, 1, 1, 1, 1, 1, 1, 1, 1, 1, 1, 1, 1, 1, 1, 1, 1, 1, 1, 1, 1, 1, 1, 1, 1, 1, 1, 1, 1, 1, 1, 1, 1, 1, 1, 1, 1, 1, 1, 1, 1, 1, 1, 1, 1, 1, 1, 1, 1, 1, 1, 1, 1, 1, 1, 1, 1, 1, 1, 1, 1, 1, 1, 1, 1, 1, 1, 1, 1, 1, 1, 1, 1, 1, 1, 1, 1, 1, 1, 1, 1, 1, 1, 1, 1, 1, 1, 1, 1, 1, 1, 1, 1, 1, 1, 1, 1, 1, 1, 1, 1, 1, 1, 1, 1, 1, 1, 1, 1, 1, 1, 1, 1, 1, 1, 1, 1, 1, 1, 1, 1, 1, 1, 1, 1, 1, 1, 1, 1, 1, 1, 1, 1, 1, 1, 1, 1, 1, 1, 1, 1, 1, 1, 1, 1, 1, 1, 1, 1, 1, 1, 1, 1, 1, 1, 1, 1, 1, 1, 1, 1, 1, 1, 1, 1, 1, 1, 1, 1, 1, 1, 1, 1, 1, 1, 1, 1, 1, 1, 1, 1, 1, 1, 1, 1, 1, 1, 1, 1, 1, 1, 1, 1, 1, 1, 1, 1, 1, 1, 1, 1, 1, 1, 1, 1, 1, 1, 1, 1, 1, 1, 1, 1, 1, 1, 1, 1, 1, 1, 1, 1, 1, 1, 1, 1, 1, 1, 1, 1, 1, 1, 1, 1, 1, 1, 1, 1, 1, 1, 1, 1, 1, 1, 1, 1, 1, 1, 1, 1, 1, 1, 1, 1, 1, 1, 1, 1, 1, 1, 1, 1, 1, 1, 1, 1, 1, 1, 1, 1, 1, 1, 1, 1, 1, 1, 1, 1, 1, 1, 1, 1, 1, 1, 1, 1, 1, 1, 1, 1, 1, 1, 1, 1, 1, 1, 1, 1, 1, 1, 1, 1, 1, 1, 1, 1, 1, 1, 1, 1, 1, 1, 1, 1, 1, 1, 1, 1, 1, 1, 1, 1, 1, 1, 1, 1, 1, 1, 1, 1, 1, 1, 1, 1, 1, 1, 1, 1, 1, 1, 1, 1, 1, 1, 1, 1, 1, 1, 1, 1, 1, 1, 1, 1, 1, 1, 1, 1, 1, 1, 1, 1, 1, 1, 1, 1, 1, 1, 1, 1, 1, 1, 1, 4 ),
 ( 0.000000000000000000, 0.002599888508634240914, 0.005208754120092145765, 0.007813069968323356138, 0.01041690100177071650, 0.01302019566086259385, 0.01562517182793091500, 0.01822893254318404960, 0.02083328139698771564, 0.02343764900838959594, 0.02604139750447371365, 0.02864615928571910553, 0.03124958462592061434, 0.03385442086835698666, 0.03645794792899405279, 0.03906256697173399878, 0.04166661757251870907, 0.04427067912273281725, 0.04687528696281444140, 0.04947881815967773017, 0.05208365228821221909, 0.05468707701066444909, 0.05729184299815447134, 0.05989557646906591704, 0.06249996333325048142, 0.06510433798480201595, 0.06770807906337909798, 0.07031283757201339801, 0.07291626355048291819, 0.07552109983967189577, 0.07812462590386089201, 0.08072924387304455940, 0.08333329402460390445, 0.08593735478041557296, 0.08854196204427712547, 0.09114549249794960672, 0.09375032597506528786, 0.09635375006294695510, 0.09895851527076646170, 0.1015622481948881828, 0.1041666342325376776, 0.1067710083972730206, 0.1093747487337090180, 0.1119795066911244419, 0.1145829320296284648, 0.1171877676425944481, 0.1197912931610935483, 0.1223959103579086161, 0.1249999600491941698, 0.1276040200539713398, 0.1302086268569593308, 0.1328121566649932417, 0.1354169895755736042, 0.1380204131161003600, 0.1406251776355303407, 0.1432289101024236955, 0.1458332954032181272, 0.1484376691708411133, 0.1510414088543486633, 0.1536461663508109643, 0.1562495911381983071, 0.1588544261652600487, 0.1614579512270202244, 0.1640625677415503691, 0.1666666170620310916, 0.1692706764052687440, 0.1718752828374313091, 0.1744788120887783289, 0.1770836445231302458, 0.1796870676051354199, 0.1822918315264069888, 0.1848955636252137269, 0.1874999482789682093, 0.1901043217392619777, 0.1927080608589964439, 0.1953128179847096746, 0.1979162423098047296, 0.2005210768412587219, 0.2031246015352002054, 0.2057292174574958665, 0.2083332664966131842, 0.2109373252677763377, 0.2135419314191336626, 0.2161454602027163274, 0.2187502922511180836, 0.2213537149634070833, 0.2239584783767220588, 0.2265622101965570623, 0.2291665942930569411, 0.2317709675357785548, 0.2343747061808670040, 0.2369794630260087243, 0.2395828869776091552, 0.2421877211037245237, 0.2447912455187418734, 0.2473958609388257068, 0.2499999097859964270, 0.2526039680745227334, 0.2552085740350705789, 0.2578121024397855843, 0.2604169341924902348, 0.2630203566238439872, 0.2656251196193780695, 0.2682288512493328225, 0.2708332348783377697, 0.2734376079932215875, 0.2760413462527663842, 0.2786461029074911444, 0.2812495265743710227, 0.2838543603853929120, 0.2864578846103582599, 0.2890624996182282747, 0.2916665483628478883, 0.2942706062581511572, 0.2968752121178640513, 0.2994787402325856385, 0.3020835717798243114, 0.3046869940190023440, 0.3072917566869088346, 0.3098954882160545599, 0.3124998714673014044, 0.3151042445440625506, 0.3177079825071445485, 0.3203127390615869707, 0.3229161625325003282, 0.3255209961186533163, 0.3281245202424198926, 0.3307291349280532256, 0.3333331836594992104, 0.3359372412509727956, 0.3385418470998076690, 0.3411453750133909280, 0.3437502064453764050, 0.3463536285811206206, 0.3489583910115333087, 0.3515621225289245477, 0.3541665054921307454, 0.3567708786204680238, 0.3593746163761498691, 0.3619793729204284771, 0.3645827962841124981, 0.3671876297356038710, 0.3697911538470093351, 0.3723957683003653041, 0.3749998171080005105, 0.3776038744850206963, 0.3802084804129200468, 0.3828120082142042468, 0.3854168396211344327, 0.3880202617421720235, 0.3906250240252089334, 0.3932287556198868494, 0.3958331383847540352, 0.3984375116543538153, 0.4010412492916836102, 0.4036460059159037717, 0.4062494292610819846, 0.4088542626681055392, 0.4114577868559751161, 0.4140624011669984950, 0.4166664501401745602, 0.4192705073921035863, 0.4218751134889988097, 0.4244786412668108966, 0.4270834727388717056, 0.4296868949339185950, 0.4322916571596854274, 0.4348953889206810253, 0.4374997715768980666, 0.4401041450774376140, 0.4427078826854516369, 0.4453126394797092824, 0.4479160628950952239, 0.4505208963478340434, 0.4531244207009840763, 0.4557290349596088697, 0.4583330841876695483, 0.4609371414038593850, 0.4635417477596745495, 0.4661452756028321986, 0.4687501072302013849, 0.4713535295879656695, 0.4739582918465587991, 0.4765620238628961447, 0.4791664065001429718, 0.4817707803212932793, 0.4843745179890200370, 0.4869792750434049911, 0.4895826986177053142, 0.4921875322063354874, 0.4947910568135764908, 0.4973956711097291539, 0.4999997206820134821, 0.5026037779518089943, 0.5052083846564635605, 0.5078119126537786743, 0.5104167445266291070, 0.5130201671358142201, 0.5156249295173244152, 0.5182286618780244103, 0.5208330445859747915, 0.5234374188174044651, 0.5260411566338674128, 0.5286459140384663913, 0.5312493378603841965, 0.5338541716750782040, 0.5364576966252184720, 0.5390623110488209635, 0.5416663610546670338, 0.5442704184674093115, 0.5468750256108222407, 0.5494785538511040013, 0.5520833860596070508, 0.5546868090089153158, 0.5572915716034309019, 0.5598953043975141153, 0.5624996872658396541, 0.5651040619972180767, 0.5677078000514395040, 0.5703125578963399445, 0.5729159820545779436, 0.5755208161855079885, 0.5781243415673570363, 0.5807289562083304268, 0.5833330067370782190, 0.5859370643821081304, 0.5885416720542003821, 0.5911452006262593040, 0.5937500332605881725, 0.5963534566387238556, 0.5989582195363342132, 0.6015619528528246551, 0.6041663359711972880, 0.6067707112921981727, 0.6093744496732020899, 0.6119792080484952601, 0.6145826326317597177, 0.6171874671691013337, 0.6197909930714722293, 0.6223956080197403651, 0.6249996591607356322, 0.6276037171273963766, 0.6302083254180952387, 0.6328118544107458332, 0.6354166875610788301, 0.6380201114567515264, 0.6406248747475506988, 0.6432286086754787080, 0.6458329921335752566, 0.6484373681338796436, 0.6510411069306952792, 0.6536458659264798854, 0.6562492910234830612, 0.6588541260574176661, 0.6614576525691320263, 0.6640622679146246377, 0.6666663197572214594, 0.6692703781348633418, 0.6718749871341050950, 0.6744785166361690898, 0.6770833503926931840, 0.6796867748946214816, 0.6822915386687108397, 0.6848952732971168578, 0.6874996571846213600, 0.6901040339539210589, 0.6927077732555863010, 0.6953125329619718187, 0.6979159586614360755, 0.7005207942821553013, 0.7031243214920454010, 0.7057289373247008779, 0.7083329899582661016, 0.7109370488362486418, 0.7135416586339821121, 0.7161451887342924483, 0.7187500231872065992, 0.7213534483841206324, 0.7239582127316128712, 0.7265619481495508847, 0.7291663325561579256, 0.7317707101841592898, 0.7343744500797240171, 0.7369792105868335774, 0.7395826369774940456, 0.7421874732752028470, 0.7447910012721150608, 0.7473956176818850050, 0.7499996711958007989, 0.7526037306634962842, 0.7552083413496862851, 0.7578118721370898925, 0.7604167073766084917, 0.7630201333572542710, 0.7656248983682768516, 0.7682286346648167230, 0.7708330196802359868, 0.7734373982566630223, 0.7760411388351919904, 0.7786459002331664880, 0.7812493274037752844, 0.7838541644686951582, 0.7864576933414935134, 0.7890623104183455139, 0.7916663649020125870, 0.7942704250488100692, 0.7968750367134410650, 0.7994785682768023038, 0.8020834043931583945, 0.8046868312463003603, 0.8072915970109983963, 0.8098953342752303053, 0.8124997199891885735, 0.8151040996037859365, 0.8177078409543626636, 0.8203126033333638656, 0.8229160313726919806, 0.8255208692950642968, 0.8281243991326340259, 0.8307290169665545454, 0.8333330725093962554, 0.8359371334247044372, 0.8385417461577832077, 0.8411452785859873105, 0.8437501156694361404, 0.8463535434838604932, 0.8489583100924004144, 0.8515620484134380774, 0.8541664349156833369, 0.8567708156582201084, 0.8593745578699503174, 0.8619793213201638604, 0.8645827503170061545, 0.8671875891870957087, 0.8697911200783463581, 0.8723957387593448409, 0.8749997954508100806, 0.8776038572240605351, 0.8802084711156200614, 0.8828120044975765746, 0.8854168426383988155, 0.8880202715029178462, 0.8906250390454908406, 0.8932287785124739532, 0.8958331658927787267, 0.8984375478530519654, 0.9010412910150662480, 0.9036460556267057465, 0.9062494856698833923, 0.9088543255779816255, 0.9114578576118502751, 0.9140624772299625889, 0.9166665351595286726, 0.9192705978801787303, 0.9218752130202838568, 0.9244787474449313036, 0.9270835867334279445, 0.9296870167368762594, 0.9322917853037333558, 0.9348955260058576799, 0.9374999143539141100, 0.9401042976215825409, 0.9427080418234272674, 0.9453128076877782560, 0.9479162388645026027, 0.9505210798953250828, 0.9531246131693177359, 0.9557292338404025367, 0.9583332930514818493, 0.9609373567081632705, 0.9635419734050364449, 0.9661455093234165847, 0.9687503490003109841, 0.9713537788664922124, 0.9739585512809396661, 0.9765622998769101226, 0.9791666815729623830, 0.9817710277688282972, 0.9843747994658795797, 0.9869797739623470401, 0.9895830763955310028, 0.9921869177308453303, 0.9947912343601759133, 0.9974001139318913189, 1.000000000000000000 ),
 .UNSPECIFIED. ) ;
#167777 = CARTESIAN_POINT ( 'NONE',  ( 6.983263157960333700, 2.949816178198962024, 2.606004571833001382 ) ) ;
#167778 = CARTESIAN_POINT ( 'NONE',  ( 5.155258101147136784, -1.908469616433384086, -1.214953784003909520 ) ) ;
#167779 = CARTESIAN_POINT ( 'NONE',  ( -7.067878151425722955, 7.140279352951794500, 0.7998128361456341429 ) ) ;
#167780 = CARTESIAN_POINT ( 'NONE',  ( -1.364683531249997417, 5.821875000341418804, 1.214306433183764966E-14 ) ) ;
#167781 = CARTESIAN_POINT ( 'NONE',  ( 4.937886321289528979, 7.980522944944189234, -1.013380012275147291 ) ) ;
#167782 = CARTESIAN_POINT ( 'NONE',  ( 0.7500000000000006661, 13.91666666666666785, -1.299038105676657340 ) ) ;
#167783 = CARTESIAN_POINT ( 'NONE',  ( -4.448483798615272100, 8.203998508444197313, 0.000000000000000000 ) ) ;
#167784 = CARTESIAN_POINT ( 'NONE',  ( 3.743459811148990291, 7.381470523066878009, -0.7216878364870338292 ) ) ;
#167785 = CARTESIAN_POINT ( 'NONE',  ( 4.973781575966475188, 1.018845774273930749, 1.446830399915491006 ) ) ;
#167786 = CARTESIAN_POINT ( 'NONE',  ( 3.264317399697822530, 2.013265973121576291, -0.002229150246490021157 ) ) ;
#167787 = CARTESIAN_POINT ( 'NONE',  ( 8.457588896826466751, 8.761608555919362828, 1.040834085586084257E-14 ) ) ;
#167788 = CARTESIAN_POINT ( 'NONE',  ( 1.659346488253128804, -1.806016679666972546, -1.082987972701171309 ) ) ;
#167789 = CARTESIAN_POINT ( 'NONE',  ( 0.9310837752575386039, -1.510843254991366402, -1.177573636344444896 ) ) ;
#167791 = CARTESIAN_POINT ( 'NONE',  ( 0.7499999999999902300, 2.733333333333351600, 1.299038105676669330 ) ) ;
#167790 = CARTESIAN_POINT ( 'NONE',  ( 0.6823417656249969321, 12.52604166700806232, -1.181850606188757036 ) ) ;
#167792 = CARTESIAN_POINT ( 'NONE',  ( 2.541402807867772840, 1.801932494976875576, -0.7955018757880153446 ) ) ;
#167793 = CARTESIAN_POINT ( 'NONE',  ( 0.5142528298564854605, 1.293200884458247657, -1.351890787750304135 ) ) ;
#167794 = CARTESIAN_POINT ( 'NONE',  ( 0.6077679335219284829, 0.6189715888181289705, -1.861716921216026055 ) ) ;
#167796 = ORIENTED_EDGE ( 'NONE', *, *, #64145, .T. ) ;
#167795 = CARTESIAN_POINT ( 'NONE',  ( -0.1933232215488022709, -0.4202133615931051835, -1.872389726556406897 ) ) ;
#167797 = CARTESIAN_POINT ( 'NONE',  ( 5.341549334104176872, 9.175631956522799726, 0.7216878364870438212 ) ) ;
#167798 = CARTESIAN_POINT ( 'NONE',  ( -1.402160292154681736E-14, 0.6343750003414162508, 1.575800808251672791 ) ) ;
#167799 = CARTESIAN_POINT ( 'NONE',  ( 5.928550619183989845, 1.803260976426118489, 0.4972845834502263584 ) ) ;
#167800 = CARTESIAN_POINT ( 'NONE',  ( 10.71502147350184231, 11.39527989537399755, 0.000000000000000000 ) ) ;
#167801 = CARTESIAN_POINT ( 'NONE',  ( 4.996967907133109676, 0.3485794866864948549, 2.040532872733556768 ) ) ;
#167802 = CARTESIAN_POINT ( 'NONE',  ( -1.225000000000060263, 2.729166666666693164, -0.7072540797573217963 ) ) ;
#167803 = CARTESIAN_POINT ( 'NONE',  ( -5.112833325684920993, 6.097965313788082931, -1.082531754730549967 ) ) ;
#167804 = CARTESIAN_POINT ( 'NONE',  ( 0.4423056438102772603, -0.9742743152163436671, 3.420118577353472133 ) ) ;
#167805 = CARTESIAN_POINT ( 'NONE',  ( -1.500000000000013101, 0.9208333333333594828, 0.8660254037844403729 ) ) ;
#167806 = CARTESIAN_POINT ( 'NONE',  ( 8.911787042884274257, 9.291506392986812912, 0.7998128361456462443 ) ) ;
#167807 = CARTESIAN_POINT ( 'NONE',  ( -9.179033691651859783, 10.66762638080401260, 1.199719254218462483 ) ) ;
#167808 = CARTESIAN_POINT ( 'NONE',  ( 5.345657705538078730, 9.458627433094950021, 0.7998128361456331437 ) ) ;
#167809 = CARTESIAN_POINT ( 'NONE',  ( -0.6823417656250212460, 1.051041667008083325, 1.181850606188755259 ) ) ;
#167810 = CARTESIAN_POINT ( 'NONE',  ( 1.499999999999987121, 1.004166666666687968, 0.8660254037844524744 ) ) ;
#167812 = CARTESIAN_POINT ( 'NONE',  ( 5.684946482831785275, 5.526859072925533134, -0.7998128361456231517 ) ) ;
#167811 = CARTESIAN_POINT ( 'NONE',  ( 5.019951445752288244, 1.940773837913706057, -0.2859759768028962146 ) ) ;
#167813 = CARTESIAN_POINT ( 'NONE',  ( 3.708361104356564297, -1.524809962200252444, -1.319026932540816599 ) ) ;
#167814 = CARTESIAN_POINT ( 'NONE',  ( 2.993272137104509678, -0.3688056758139393043, 1.879696595719517083 ) ) ;
#167815 = CARTESIAN_POINT ( 'NONE',  ( -1.911175648939902105, 3.243131119507697502, -0.4542559028653506692 ) ) ;
#167816 = CARTESIAN_POINT ( 'NONE',  ( 0.7498831369015903636, 2.188782640433343474, -0.1130235578899463078 ) ) ;
#167817 = CARTESIAN_POINT ( 'NONE',  ( 0.1331715793776782342, 4.090830978607494117, -2.508370148267160538 ) ) ;
#167818 = CARTESIAN_POINT ( 'NONE',  ( 3.040157689216971715, 1.855973101128991054, 0.2326549598439253685 ) ) ;
#167819 = CARTESIAN_POINT ( 'NONE',  ( -1.402160292154681736E-14, -0.6312499993171797330, -1.732050807568870754 ) ) ;
#167820 = CARTESIAN_POINT ( 'NONE',  ( -8.044065211609668253, 8.279164256499745633, 0.7998128361456602331 ) ) ;
#167822 = CARTESIAN_POINT ( 'NONE',  ( 4.693022120063472080, 1.842747525957793009, 1.042402977009656340 ) ) ;
#167821 = CARTESIAN_POINT ( 'NONE',  ( -5.422898255786198440, 7.349800603215774331, -1.443375672974052559 ) ) ;
#167823 = DIRECTION ( 'NONE',  ( -5.578564026256490882E-16, -1.000000000000000000, -9.066213480720158442E-32 ) ) ;
#167824 = CARTESIAN_POINT ( 'NONE',  ( 5.477033855465498924, 1.911541192706748715, 0.7957256658025002594 ) ) ;
#167826 = CARTESIAN_POINT ( 'NONE',  ( 6.720655732516663150, 7.051555433583626353, 2.871889998671435240 ) ) ;
#167825 = CARTESIAN_POINT ( 'NONE',  ( 1.136401537022444508, 0.4113854086121961351, 2.049693714879106121 ) ) ;
#167828 = ORIENTED_EDGE ( 'NONE', *, *, #93138, .F. ) ;
#167827 = CARTESIAN_POINT ( 'NONE',  ( 0.1645217639845691082, -1.537023147574669402, -0.7826882907640534404 ) ) ;
#167829 = CARTESIAN_POINT ( 'NONE',  ( 8.423693512792301163, 8.722063941212843119, 0.7998128361456481317 ) ) ;
#167830 = CARTESIAN_POINT ( 'NONE',  ( -15.75000000000000000, 12.69999999999999929, -1.800000000000001155 ) ) ;
#167831 = FACE_OUTER_BOUND ( 'NONE', #192182, .T. ) ;
#167832 = CARTESIAN_POINT ( 'NONE',  ( 6.846504384776753049, 9.010674420371453053, -1.443375672974058777 ) ) ;
#167833 = CARTESIAN_POINT ( 'NONE',  ( 0.6823417656249969321, 13.08854166700806942, -1.181850606188757036 ) ) ;
#167834 = ADVANCED_FACE ( 'NONE', ( #172397 ), #70583, .T. ) ;
#167836 = CARTESIAN_POINT ( 'NONE',  ( 0.7151241933986829391, 1.480140477221444373, 1.044027612606616140 ) ) ;
#167835 = CARTESIAN_POINT ( 'NONE',  ( 6.047819040147648373, 9.213483425884394507, 1.199719254218452047 ) ) ;
#167837 = CARTESIAN_POINT ( 'NONE',  ( -8.290974629956718189, 9.631557475493025322, -1.199719254218446718 ) ) ;
#167838 = CARTESIAN_POINT ( 'NONE',  ( 4.599240423533799138, 6.388866465587984322, 1.599625672291267398 ) ) ;
#167839 = CARTESIAN_POINT ( 'NONE',  ( -5.303700083894403505, 7.646886670761364968, 1.227282432737321294 ) ) ;
#167840 = CARTESIAN_POINT ( 'NONE',  ( 7.713663051532233972, 7.963971413067895355, -0.7998128361456341429 ) ) ;
#167841 = CARTESIAN_POINT ( 'NONE',  ( -6.396834479292370368, -8.176568542494905500, -7.055228938194266775 ) ) ;
#167842 = CARTESIAN_POINT ( 'NONE',  ( -11.55950211276791073, 11.29999999999998295, 3.221476510067111665 ) ) ;
#167843 = CARTESIAN_POINT ( 'NONE',  ( 4.518945272056516416, 4.166524327021037699, 0.7998128361456341429 ) ) ;
#167844 = ORIENTED_EDGE ( 'NONE', *, *, #205468, .T. ) ;
#167845 = CARTESIAN_POINT ( 'NONE',  ( 5.765249964824501028, 1.862012222821707308, -0.7743297468396084238 ) ) ;
#167846 = CARTESIAN_POINT ( 'NONE',  ( 0.7684181764250409552, 2.117871390293009526, -0.1079879263860619443 ) ) ;
#167847 = TOROIDAL_SURFACE ( 'NONE', #199040, 10.92000000000000171, 0.08000000000000000167 ) ;
#167848 = CARTESIAN_POINT ( 'NONE',  ( 10.93020303578476238, -8.258458176070773149, -0.1907874036681889707 ) ) ;
#167849 = CARTESIAN_POINT ( 'NONE',  ( -0.1394461523060987751, 0.6550469493228279205, -2.357635998629922902 ) ) ;
#167850 = CARTESIAN_POINT ( 'NONE',  ( -1.499999999999997780, 8.640473353474856566, -2.571377442220798670 ) ) ;
#167851 = CARTESIAN_POINT ( 'NONE',  ( -4.284013352238262407, 6.021101549076499637, -1.443375672974053447 ) ) ;
#167852 = VECTOR ( 'NONE', #57095, 1000.000000000000000 ) ;
#167853 = CARTESIAN_POINT ( 'NONE',  ( 7.782016984564049444, 11.06247500109133064, 1.082531754730557072 ) ) ;
#167854 = CARTESIAN_POINT ( 'NONE',  ( 3.186336211243359084, 1.097972430180796266, -1.634763817068272784 ) ) ;
#167856 = CARTESIAN_POINT ( 'NONE',  ( 0.9617728337494994006, -1.673954878106189925, -1.301583125534570673 ) ) ;
#167855 = B_SPLINE_CURVE_WITH_KNOTS ( 'NONE', 3,
 ( #64878, #182896, #183962, #197015, #48651, #83254 ),
 .UNSPECIFIED., .F., .F.,
 ( 4, 2, 4 ),
 ( 0.000000000000000000, 0.0003172254002810710651, 0.0006344508005621421302 ),
 .UNSPECIFIED. ) ;
#167857 = CARTESIAN_POINT ( 'NONE',  ( -7.040761844198392794, 7.108643661186573759, -0.7998128361456291469 ) ) ;
#167858 = CARTESIAN_POINT ( 'NONE',  ( -11.55950211276791428, 11.37999999999999901, -3.221476510067114329 ) ) ;
#167859 = CARTESIAN_POINT ( 'NONE',  ( 6.727182134110201162, 1.237345558575110083, 2.302850971298702198 ) ) ;
#167860 = CARTESIAN_POINT ( 'NONE',  ( 6.281208295753298643, 1.508423295503196648, 1.589913042345507455 ) ) ;
#167861 = CARTESIAN_POINT ( 'NONE',  ( -0.9486429539237204445, 3.038339070649072493, -1.028101543438967980 ) ) ;
#167862 = CARTESIAN_POINT ( 'NONE',  ( 4.559546607354286074, 0.4225000031176616710, -1.879333123156016860 ) ) ;
#167863 = CARTESIAN_POINT ( 'NONE',  ( -8.857554428429624593, 9.228235009456373206, 0.7998128361456462443 ) ) ;
#167864 = FACE_OUTER_BOUND ( 'NONE', #43107, .T. ) ;
#167865 = CARTESIAN_POINT ( 'NONE',  ( 1.418904949497600487, 1.480075412272121360, -1.637148382315711359 ) ) ;
#167866 = FILL_AREA_STYLE_COLOUR ( '', #9742 ) ;
#167867 = ORIENTED_EDGE ( 'NONE', *, *, #72583, .T. ) ;
#167868 = ORIENTED_EDGE ( 'NONE', *, *, #44567, .T. ) ;
#167869 = CARTESIAN_POINT ( 'NONE',  ( 6.438338856661699694, -1.056498591242978957, 1.661895973567611540 ) ) ;
#167870 = CARTESIAN_POINT ( 'NONE',  ( 0.5209107642259405146, -1.843744896352221829, 0.6102272969235060796 ) ) ;
#167871 = CARTESIAN_POINT ( 'NONE',  ( 6.063868583556772052, 1.884346855680006261, -1.315804018288849964 ) ) ;
#167873 = CARTESIAN_POINT ( 'NONE',  ( 4.100341000477321529, 1.851659804611929472, 0.1859286059659806256 ) ) ;
#167872 = CARTESIAN_POINT ( 'NONE',  ( -6.740338644649361832, 7.892758502626242567, -1.199719254218452047 ) ) ;
#167874 = CARTESIAN_POINT ( 'NONE',  ( 5.515134625708930649, 9.656350506627580543, 0.000000000000000000 ) ) ;
#167875 = FACE_OUTER_BOUND ( 'NONE', #65020, .T. ) ;
#167876 = CARTESIAN_POINT ( 'NONE',  ( -6.938021921891187382, 9.117444880338284818, -1.599625672291263179 ) ) ;
#167877 = CARTESIAN_POINT ( 'NONE',  ( -2.875737979874388284, 6.369128386579808954, -0.7216878364870458196 ) ) ;
#167878 = CARTESIAN_POINT ( 'NONE',  ( 0.7498831369015904746, 2.188782640433343474, -0.1130235578899463078 ) ) ;
#167879 = CARTESIAN_POINT ( 'NONE',  ( 3.714570900464269076, 7.277490450609545469, 0.7216878364870298324 ) ) ;
#167880 = ORIENTED_EDGE ( 'NONE', *, *, #83840, .F. ) ;
#167881 = EDGE_CURVE ( 'NONE', #141673, #152360, #39294, .T. ) ;
#167882 = DIRECTION ( 'NONE',  ( 0.000000000000000000, 0.000000000000000000, 1.000000000000000000 ) ) ;
#167883 = CARTESIAN_POINT ( 'NONE',  ( 0.4865809202317071813, -0.2202831055867389420, -1.812292406919484344 ) ) ;
#167884 = CARTESIAN_POINT ( 'NONE',  ( -4.623494077460110319, 5.352830164246910272, 1.199719254218462483 ) ) ;
#167885 = CARTESIAN_POINT ( 'NONE',  ( 2.848001011750156408, 0.2514756280368075081, -1.715647774213580501 ) ) ;
#167886 = CARTESIAN_POINT ( 'NONE',  ( 1.250000000000053069, 8.500000000000000000, 15.75000000000000000 ) ) ;
#167887 = CARTESIAN_POINT ( 'NONE',  ( -11.06299035296667732, 9.843162956239048356, -0.9087041361035911313 ) ) ;
#167888 = CARTESIAN_POINT ( 'NONE',  ( -5.926322542504887991, 6.086666852443358700, -0.7216878364870307205 ) ) ;
#167889 = CARTESIAN_POINT ( 'NONE',  ( 6.094357461763901362, -1.817385979143220309, -0.1739998769475574192 ) ) ;
#167890 = CARTESIAN_POINT ( 'NONE',  ( 3.608209768781400761, 1.961936380018937331, 0.004537341891153179319 ) ) ;
#167891 = EDGE_CURVE ( 'NONE', #90575, #115124, #98878, .T. ) ;
#167892 = CARTESIAN_POINT ( 'NONE',  ( -3.154860657348034577E-14, -1.124999999317153332, 1.414508159514557439 ) ) ;
#167893 = CARTESIAN_POINT ( 'NONE',  ( -8.503988664269602538, 10.94440607977979063, 1.599625672291269396 ) ) ;
#167894 = CARTESIAN_POINT ( 'NONE',  ( 6.287230548435207567, 8.358188277972981695, -1.599625672291262513 ) ) ;
#167895 = CARTESIAN_POINT ( 'NONE',  ( 4.477262591527907176, -1.894555094343739476, -0.9525379817736513433 ) ) ;
#167896 = CARTESIAN_POINT ( 'NONE',  ( 8.018721507839716267, 8.319872945426633137, -0.7998128361456341429 ) ) ;
#167897 = ADVANCED_FACE ( 'NONE', ( #156151 ), #155688, .T. ) ;
#167898 = CARTESIAN_POINT ( 'NONE',  ( -8.611400122974211868, 13.19838391011195888, 1.040834085586084257E-14 ) ) ;
#167899 = CIRCLE ( 'NONE', #78073, 0.05000000000000008604 ) ;
#167900 = CARTESIAN_POINT ( 'NONE',  ( 3.098552089154332556, 2.054082100768514607, 0.2579794602402472603 ) ) ;
#167902 = CARTESIAN_POINT ( 'NONE',  ( -1.364683531250000748, -0.4281249996585800854, 0.000000000000000000 ) ) ;
#167901 = CARTESIAN_POINT ( 'NONE',  ( 6.827182134110205247, 0.5943742033862747798, 1.864010940340610212 ) ) ;
#167904 = ORIENTED_EDGE ( 'NONE', *, *, #109904, .T. ) ;
#167903 = CARTESIAN_POINT ( 'NONE',  ( 4.741020875331694029, 2.125508857184394973, 0.6453399526389347329 ) ) ;
#167905 = CARTESIAN_POINT ( 'NONE',  ( 2.426789430794534130, -1.706071328008453625, -1.540741829672709118 ) ) ;
#167906 = CARTESIAN_POINT ( 'NONE',  ( 7.456621297836067086, 10.68284669990868174, 1.082531754730558626 ) ) ;
#167908 = CARTESIAN_POINT ( 'NONE',  ( -1.642778471875000035, -2.617708332855375186, -2.845375778867859751 ) ) ;
#167907 = CARTESIAN_POINT ( 'NONE',  ( 7.539742822975472158, 7.968990512992423447, -0.7216878364870317197 ) ) ;
#167909 = LINE ( 'NONE', #19507, #57813 ) ;
#167910 = LINE ( 'NONE', #101842, #192875 ) ;
#167911 = ORIENTED_EDGE ( 'NONE', *, *, #63078, .T. ) ;
#167913 = CYLINDRICAL_SURFACE ( 'NONE', #56318, 1.500000000000000222 ) ;
#167912 = CIRCLE ( 'NONE', #74538, 0.08000000000000020983 ) ;
#167914 = CARTESIAN_POINT ( 'NONE',  ( 4.482611839828003930, -1.244964735940889522, 1.451779576051547282 ) ) ;
#167915 = CARTESIAN_POINT ( 'NONE',  ( 0.000000000000000000, 0.4330127018922214077, 0.000000000000000000 ) ) ;
#167916 = CARTESIAN_POINT ( 'NONE',  ( 3.768305045387724928, -1.158492864085089114, 1.277938026295278418 ) ) ;
#167917 = CARTESIAN_POINT ( 'NONE',  ( 3.555875268649951959, 1.124244472066991518, 1.673854899288424347 ) ) ;
#167918 = CARTESIAN_POINT ( 'NONE',  ( 4.448018067569548428, -2.052855444095956550, -1.034378808386252624 ) ) ;
#167919 = CARTESIAN_POINT ( 'NONE',  ( 1.224999999999958789, 1.166666667349521624, 0.7072540797572417492 ) ) ;
#167920 = CARTESIAN_POINT ( 'NONE',  ( 0.1181803206181560040, -2.163391993613572151, 0.4351206515559591370 ) ) ;
#167921 = CARTESIAN_POINT ( 'NONE',  ( -6.780486220610195680, 7.083191143566240910, -0.7216878364870338292 ) ) ;
#167922 = CARTESIAN_POINT ( 'NONE',  ( 4.622157715239192832, 1.089468934077148399, -1.394508319181851697 ) ) ;
#167924 = CARTESIAN_POINT ( 'NONE',  ( 1.324644486801781040, 2.210297274253099520, 0.6072788910070088253 ) ) ;
#167923 = CARTESIAN_POINT ( 'NONE',  ( 7.201315867513990554, 8.430565262634994284, -1.199719254218452047 ) ) ;
#167925 = CARTESIAN_POINT ( 'NONE',  ( 6.404252597826388893, 1.360807738692754176, -1.240355271200761278 ) ) ;
#167926 = CARTESIAN_POINT ( 'NONE',  ( -8.093291352714894415, 8.406871097780989288, -0.7998128361456362523 ) ) ;
#167927 = CARTESIAN_POINT ( 'NONE',  ( 6.580031370938625557, -2.148343778048496411, -0.4316624935760752790 ) ) ;
#167928 = CARTESIAN_POINT ( 'NONE',  ( -5.490125858891038213, 5.369844688319787451, -0.7998128361456362523 ) ) ;
#167929 = CARTESIAN_POINT ( 'NONE',  ( 1.360316468749979801, -0.9322916663252904801, -0.7853790794159041244 ) ) ;
#167930 = DIRECTION ( 'NONE',  ( 0.000000000000000000, 1.000000000000000000, 0.000000000000000000 ) ) ;
#167931 = CARTESIAN_POINT ( 'NONE',  ( 6.877413708759195998, -0.1538780216673047430, 2.036608477593480959 ) ) ;
#167932 = CARTESIAN_POINT ( 'NONE',  ( 1.200408080392855181, 1.350732740426639822, -1.497504596960941958 ) ) ;
#167933 = CARTESIAN_POINT ( 'NONE',  ( 1.499999999999987566, -0.4437499993171847845, 0.000000000000000000 ) ) ;
#167934 = CARTESIAN_POINT ( 'NONE',  ( 5.742784330379758551, 0.3781152824756833231, 1.888869927322960329 ) ) ;
#167935 = CARTESIAN_POINT ( 'NONE',  ( -1.364683531250014514, 11.58854166700806410, -0.7879004041258335089 ) ) ;
#167936 = CARTESIAN_POINT ( 'NONE',  ( 0.9849990780092006126, -1.403669121040777457, 1.721781922543249799 ) ) ;
#167937 = ORIENTED_EDGE ( 'NONE', *, *, #117124, .T. ) ;
#167939 = CARTESIAN_POINT ( 'NONE',  ( 0.1399574524686736654, 8.210952333604119247, -2.038660652713630395 ) ) ;
#167938 = DIRECTION ( 'NONE',  ( -0.9885327375000381167, 0.000000000000000000, 0.1510067114093955609 ) ) ;
#167940 = DIRECTION ( 'NONE',  ( 0.000000000000000000, 1.000000000000000000, 0.000000000000000000 ) ) ;
#167941 = CARTESIAN_POINT ( 'NONE',  ( 9.887974103068218668, 10.43039129653476493, 0.7998128361456462443 ) ) ;
#167942 = CARTESIAN_POINT ( 'NONE',  ( 0.000000000000000000, -3.499999999999999556, 0.000000000000000000 ) ) ;
#167943 = DIRECTION ( 'NONE',  ( 0.000000000000000000, 0.000000000000000000, -1.000000000000000000 ) ) ;
#167944 = CARTESIAN_POINT ( 'NONE',  ( 3.755166387800693339, 1.726757624646685807, -0.2173075579294906912 ) ) ;
#167945 = CARTESIAN_POINT ( 'NONE',  ( 2.752341281506097470, -1.956419249932477955, -0.1471676765215298721 ) ) ;
#167947 = CARTESIAN_POINT ( 'NONE',  ( -0.6823417656250212460, 2.863541667008084879, 1.181850606188767472 ) ) ;
#167946 = CARTESIAN_POINT ( 'NONE',  ( 4.172158584703322681, 5.890604320285754980, -1.599625672291256295 ) ) ;
#167948 = CARTESIAN_POINT ( 'NONE',  ( -11.39849338755883323, 1.813773193624679925, 3.751625886033604917 ) ) ;
#167949 = CARTESIAN_POINT ( 'NONE',  ( 6.426224708462171087, 1.007414738832881351, 1.683299376423300853 ) ) ;
#167950 = CARTESIAN_POINT ( 'NONE',  ( -6.808165692356648258, 11.09461040772476714, 0.7998128361456481317 ) ) ;
#167951 = CARTESIAN_POINT ( 'NONE',  ( -4.622967192135580383, 5.456178481322002227, 1.082531754730558626 ) ) ;
#167952 = CARTESIAN_POINT ( 'NONE',  ( 5.225796113160614986, 0.8128206588041908542, -1.845625551132886288 ) ) ;
#167953 = CARTESIAN_POINT ( 'NONE',  ( 1.464152659907109966, 2.228779883755461100, -0.3883945716754066968 ) ) ;
#167954 = ORIENTED_EDGE ( 'NONE', *, *, #7569, .T. ) ;
#167955 = CARTESIAN_POINT ( 'NONE',  ( -1.500000000000001332, -0.5687499993171779566, 0.000000000000000000 ) ) ;
#167956 = CARTESIAN_POINT ( 'NONE',  ( 2.671000074538076863, 0.09590037325727870932, -1.868228684465601752 ) ) ;
#167957 = CARTESIAN_POINT ( 'NONE',  ( 1.494300775288709415, -1.721104260995092838, 0.2117000974225565491 ) ) ;
#167958 = CARTESIAN_POINT ( 'NONE',  ( 4.862908538974716421, 0.2148362657848035262, -2.180980218048253150 ) ) ;
#167959 = CARTESIAN_POINT ( 'NONE',  ( 5.122255714018879580, -1.229368216938999003, -1.952684467508845056 ) ) ;
#167960 = CARTESIAN_POINT ( 'NONE',  ( 1.551711473626409266, 0.5993144932881481202, -1.971807626030545268 ) ) ;
#167961 = CARTESIAN_POINT ( 'NONE',  ( 3.398316578678576949, 1.530473418458015100, -1.195227296853792920 ) ) ;
#167962 = CARTESIAN_POINT ( 'NONE',  ( -5.544921637864841379, 5.571422787038166291, -0.7216878364870197293 ) ) ;
#167963 = CARTESIAN_POINT ( 'NONE',  ( 6.204356031920277736, -0.6731288877953770511, -1.745422550748019219 ) ) ;
#167964 = CARTESIAN_POINT ( 'NONE',  ( 4.023704138721054591, 7.562441369377219225, 0.3480857562657164173 ) ) ;
#167965 = CARTESIAN_POINT ( 'NONE',  ( 6.784528966312857179, -1.956291195211720346, 0.4871289682274528299 ) ) ;
#167966 = EDGE_CURVE ( 'NONE', #33385, #137589, #15861, .T. ) ;
#167967 = CARTESIAN_POINT ( 'NONE',  ( 3.418064124421011041, 7.001842221884225559, -0.7216878364870338292 ) ) ;
#167968 = CARTESIAN_POINT ( 'NONE',  ( 0.6801582343749952297, 1.807291667008069425, -1.178068619123869398 ) ) ;
#167969 = CARTESIAN_POINT ( 'NONE',  ( 4.518204034511161815, -1.842447959940773705, 0.8197716922626956393 ) ) ;
#167970 = CARTESIAN_POINT ( 'NONE',  ( -4.921246571636213929, 4.843801876438091902, 0.7216878364870317197 ) ) ;
#167971 = CARTESIAN_POINT ( 'NONE',  ( 8.666686507633574621, 11.13422023037111330, 1.599625672291281386 ) ) ;
#167972 = CARTESIAN_POINT ( 'NONE',  ( 3.393283585170187688, 7.180857625999046867, 0.7998128361456271485 ) ) ;
#167974 = CARTESIAN_POINT ( 'NONE',  ( -6.895452369244193136, -6.747656629766889402, 6.524021554744679818 ) ) ;
#167973 = CARTESIAN_POINT ( 'NONE',  ( 2.596107596775329540, -1.820790993511243849, -0.1344670722737417168 ) ) ;
#167975 = CARTESIAN_POINT ( 'NONE',  ( -4.288121723672178476, 8.224835454251337552, -0.7998128361456362523 ) ) ;
#167976 = CARTESIAN_POINT ( 'NONE',  ( 11.39849338755880659, 1.813773193624685032, -3.751625886033683077 ) ) ;
#167977 = CARTESIAN_POINT ( 'NONE',  ( -7.553974597844363537, -6.709380320845435008, -7.821934338880122795 ) ) ;
#167978 = EDGE_LOOP ( 'NONE', ( #180522, #125452, #181401, #150152 ) ) ;
#167979 = CARTESIAN_POINT ( 'NONE',  ( -6.902509602688830626, 7.225551755991315162, -0.7216878364870338292 ) ) ;
#167980 = UNCERTAINTY_MEASURE_WITH_UNIT (LENGTH_MEASURE( 1.000000000000000082E-05 ), #193242, 'distance_accuracy_value', 'NONE');
#167981 = CARTESIAN_POINT ( 'NONE',  ( -2.981903720001798597, 5.566305875722335372, -1.199719254218446718 ) ) ;
#167982 = PLANE ( 'NONE',  #13138 ) ;
#167983 = CARTESIAN_POINT ( 'NONE',  ( 5.988927272769587695, -1.918439801222410201, -0.6316595152702029203 ) ) ;
#167985 = ORIENTED_EDGE ( 'NONE', *, *, #85069, .T. ) ;
#167984 = CARTESIAN_POINT ( 'NONE',  ( 6.516288422252827672, -2.220882151245454850, 0.05110445944340144542 ) ) ;
#167986 = CARTESIAN_POINT ( 'NONE',  ( -6.017840079619296567, 8.114175741012878973, -1.599625672291271394 ) ) ;
#167987 = CARTESIAN_POINT ( 'NONE',  ( 6.356075086708249167, 6.309842444114747373, -0.7998128361456281477 ) ) ;
#167988 = CARTESIAN_POINT ( 'NONE',  ( 4.856353099686935515, 0.7867916563346208925, 1.904994776275979129 ) ) ;
#167989 = CARTESIAN_POINT ( 'NONE',  ( 4.711564657724523819, 1.930417226389494090, 0.5826574956761670920 ) ) ;
#167990 = ORIENTED_EDGE ( 'NONE', *, *, #15653, .T. ) ;
#167991 = ORIENTED_EDGE ( 'NONE', *, *, #187759, .T. ) ;
#167992 = DIRECTION ( 'NONE',  ( 0.000000000000000000, -1.000000000000000000, -1.496258514059622730E-16 ) ) ;
#167993 = CARTESIAN_POINT ( 'NONE',  ( 3.623053363349855172, 5.249981562040033189, 1.599625672291267398 ) ) ;
#167995 = ORIENTED_EDGE ( 'NONE', *, *, #69670, .T. ) ;
#167994 = CARTESIAN_POINT ( 'NONE',  ( -4.769436176957319695, 8.786368983084006601, 0.7998128361456281477 ) ) ;
#167996 = CARTESIAN_POINT ( 'NONE',  ( 4.626831674679969808, 8.450518883791096059, -0.3637425496919588497 ) ) ;
#167997 = CARTESIAN_POINT ( 'NONE',  ( 5.097029748277864591, 1.038832625704217527, -1.727738606215820205 ) ) ;
#167998 = CARTESIAN_POINT ( 'NONE',  ( 4.066218318298571610, -1.718653781379267276, -0.6607852518168353395 ) ) ;
#167999 = CARTESIAN_POINT ( 'NONE',  ( -5.738512597764678702, 5.917411899002910758, 2.440166504834945904 ) ) ;
#168000 = CARTESIAN_POINT ( 'NONE',  ( 2.157223245065964967, -1.782429894076944521, 1.465742965790328700 ) ) ;
#168001 = CARTESIAN_POINT ( 'NONE',  ( 7.666209513884374438, 7.908608952478760834, 0.7998128361456281477 ) ) ;
#168002 = CARTESIAN_POINT ( 'NONE',  ( 4.604844690042746436, 1.674155836469687575, -1.367402732809947397 ) ) ;
#168003 = CARTESIAN_POINT ( 'NONE',  ( 8.446893396513862839, 9.813462703143045474, -1.199719254218445830 ) ) ;
#168004 = CARTESIAN_POINT ( 'NONE',  ( 0.08144728253534591622, -0.9147537949990096617, 1.713110483266879980 ) ) ;
#168005 = CARTESIAN_POINT ( 'NONE',  ( -4.629219384062206011, 7.488174150459498968, -1.199719254218452047 ) ) ;
#168006 = CARTESIAN_POINT ( 'NONE',  ( 3.866856096493505923, -0.6709599815711597692, 2.198256080205548635 ) ) ;
#168007 = CARTESIAN_POINT ( 'NONE',  ( 2.679885790744704899, 0.4618020869172074216, -0.1056289066552755923 ) ) ;
#168008 = CARTESIAN_POINT ( 'NONE',  ( -6.818824913030298696, 6.919993584815607335, 0.7998128361456341429 ) ) ;
#168009 = CARTESIAN_POINT ( 'NONE',  ( 3.994877460428855276, 1.580554378303768992, -1.000287695324620252 ) ) ;
#168010 = CARTESIAN_POINT ( 'NONE',  ( 0.4562421353364953802, 0.7503462943320489131, 1.823165437449389081 ) ) ;
#168011 = AXIS2_PLACEMENT_3D ( 'NONE', #33742, #86764, #99820 ) ;
#168013 = CARTESIAN_POINT ( 'NONE',  ( -7.435720902452096936, 7.639705572474380091, 0.000000000000000000 ) ) ;
#168012 = CARTESIAN_POINT ( 'NONE',  ( -1.500000000000001332, -0.8187499993171781787, 0.000000000000000000 ) ) ;
#168014 = CARTESIAN_POINT ( 'NONE',  ( 1.278255639411193245, 1.316999024263129092, 1.770685722221450709 ) ) ;
#168015 = EDGE_CURVE ( 'NONE', #78732, #77955, #93918, .T. ) ;
#168016 = CARTESIAN_POINT ( 'NONE',  ( 4.982944139801846362, 4.915782372631361419, 0.3243353321068405126 ) ) ;
#168017 = CARTESIAN_POINT ( 'NONE',  ( 5.190073875932979419, 4.949507698210251938, 0.7998128361456341429 ) ) ;
#168018 = CARTESIAN_POINT ( 'NONE',  ( -4.680589345215810049, 6.483773540883647435, -1.599625672291256295 ) ) ;
#168019 = CARTESIAN_POINT ( 'NONE',  ( -7.146556367734805626, 9.431011410480991231, 1.443375672974064550 ) ) ;
#168020 = CARTESIAN_POINT ( 'NONE',  ( 6.772342980177176841, -1.213407086615119423, 1.554582774731553707 ) ) ;
#168021 = CARTESIAN_POINT ( 'NONE',  ( 6.674459784896970227, -1.426286490538879903, 1.815071943837057500 ) ) ;
#168022 = CARTESIAN_POINT ( 'NONE',  ( 0.9241798626423223251, 0.9638202082158978667, 1.708698881219716137 ) ) ;
#168023 = CARTESIAN_POINT ( 'NONE',  ( 4.469619655223175947, -0.3576850913847802182, 2.031185480813563426 ) ) ;
#168024 = CARTESIAN_POINT ( 'NONE',  ( 6.317736394288140822, 7.433409217166723870, 1.082531754730558626 ) ) ;
#168025 = CARTESIAN_POINT ( 'NONE',  ( 7.503511670520385479, 7.718794801887437274, 0.7998128361456281477 ) ) ;
#168026 = EDGE_LOOP ( 'NONE', ( #104175, #15315, #120778, #46804, #87692 ) ) ;
#168027 = CARTESIAN_POINT ( 'NONE',  ( 8.581948047326003248, 9.114620264742901767, -0.7216878364870197293 ) ) ;
#168028 = CARTESIAN_POINT ( 'NONE',  ( -1.364683531250012516, 4.051041667008088432, -0.7879004041258300672 ) ) ;
#168029 = CARTESIAN_POINT ( 'NONE',  ( -10.56742348559178879, 4.157028815770352104, -5.593809627444244370 ) ) ;
#168030 = CARTESIAN_POINT ( 'NONE',  ( 4.243338890952890630, 5.973648010910253880, -1.443375672974051449 ) ) ;
#168031 = CARTESIAN_POINT ( 'NONE',  ( 6.057114314241694331, 1.778561107892376647, -1.245054071093915304 ) ) ;
#168032 = APPLICATION_CONTEXT ( 'automotive_design' ) ;
#168034 = CARTESIAN_POINT ( 'NONE',  ( 5.952668924537682038, -1.582617586749142102, -0.9407850039931386910 ) ) ;
#168033 = CARTESIAN_POINT ( 'NONE',  ( 9.623574082427451160, -9.090902906714891429, -0.4644248560400533465 ) ) ;
#168035 = EDGE_CURVE ( 'NONE', #180190, #58569, #128275, .T. ) ;
#168036 = CARTESIAN_POINT ( 'NONE',  ( -6.468692700515624949, 6.719432036793461904, 1.751973777778555601E-06 ) ) ;
#168037 = CARTESIAN_POINT ( 'NONE',  ( -11.89844258446856529, 12.27147310670038571, -1.560502987793169094 ) ) ;
#168038 = CARTESIAN_POINT ( 'NONE',  ( 1.159204581426832803, 0.3705859133612995349, -1.833297903905316772 ) ) ;
#168039 = CARTESIAN_POINT ( 'NONE',  ( -4.474540158260005285, 7.266292661500576955, 1.287230779100386968 ) ) ;
#168040 = DIRECTION ( 'NONE',  ( 0.000000000000000000, 0.000000000000000000, -1.000000000000000000 ) ) ;
#168041 = CARTESIAN_POINT ( 'NONE',  ( 5.178155719255617129, 7.862379301422712352, -1.251444257556088457 ) ) ;
#168042 = CARTESIAN_POINT ( 'NONE',  ( -1.001543065824772872E-14, 4.884375000341420581, 1.575800808251672791 ) ) ;
#168043 = CARTESIAN_POINT ( 'NONE',  ( 0.5746843702075511429, -1.384840223850939855, 1.318951758179337741 ) ) ;
#168044 = CARTESIAN_POINT ( 'NONE',  ( 3.027930095613054817, 0.9845384034416431174, -1.470494568931050905 ) ) ;
#168045 = PRESENTATION_LAYER_ASSIGNMENT (  '', '', ( #33216 ) ) ;
#168046 = CARTESIAN_POINT ( 'NONE',  ( 1.225099565173026761, 1.686864977381890451, 0.9006792851762451813 ) ) ;
#168048 = CARTESIAN_POINT ( 'NONE',  ( 4.112823271221511590, 0.09766498815510017695, 1.913256991299339793 ) ) ;
#168047 = CARTESIAN_POINT ( 'NONE',  ( -10.32861409551237486, 10.94447128771960287, 1.040834085586084257E-14 ) ) ;
#168049 = CARTESIAN_POINT ( 'NONE',  ( -1.347971487989957070E-14, -3.018749999044084475, 3.475000000000000089 ) ) ;
#168050 = CARTESIAN_POINT ( 'NONE',  ( 5.529738209476210642, 1.898601866877418942, -0.5236614360015124925 ) ) ;
#168051 = CARTESIAN_POINT ( 'NONE',  ( 1.125412309253082332, 1.872817075645373697, 0.9946839901537674056 ) ) ;
#168052 = FACE_OUTER_BOUND ( 'NONE', #49518, .T. ) ;
#168053 = CARTESIAN_POINT ( 'NONE',  ( 3.379631771358857950, 1.185797501207178861, 1.446808710765794315 ) ) ;
#168055 = EDGE_LOOP ( 'NONE', ( #149575, #187344, #185400, #130084 ) ) ;
#168054 = CARTESIAN_POINT ( 'NONE',  ( 6.410786927598755902, 1.272630858062718584, -1.164536656126140324 ) ) ;
#168057 = CARTESIAN_POINT ( 'NONE',  ( 3.877268743828276243, 4.586196958296845594, 1.082531754730560403 ) ) ;
#168056 = CARTESIAN_POINT ( 'NONE',  ( 3.299657469156279888, 1.739734091921738557, 1.357710657151039779 ) ) ;
#168058 = CARTESIAN_POINT ( 'NONE',  ( 0.6823417656249917140, 4.905208333674755394, 1.181850606188765695 ) ) ;
#168059 = CARTESIAN_POINT ( 'NONE',  ( 1.047418773927465629, 1.819938098697634343, -0.9707658663142370026 ) ) ;
#168060 = CARTESIAN_POINT ( 'NONE',  ( 7.474622759835693131, 7.614814729430110951, -0.7998128361456281477 ) ) ;
#168061 = CARTESIAN_POINT ( 'NONE',  ( -8.143643823302737061, 12.65266822716189843, 0.000000000000000000 ) ) ;
#168062 = CARTESIAN_POINT ( 'NONE',  ( -9.007749180432204739, 1.970899860167778073, -7.589917856500828286 ) ) ;
#168063 = CARTESIAN_POINT ( 'NONE',  ( -3.422413393345596688, -0.02203823224375053846, -0.4176190697224198001 ) ) ;
#168064 = EDGE_CURVE ( 'NONE', #133229, #115335, #55503, .T. ) ;
#168065 = TOROIDAL_SURFACE ( 'NONE', #50091, 1.829047314007947955, 0.05000000000000000278 ) ;
#168066 = CARTESIAN_POINT ( 'NONE',  ( -7.439168848973790382, -6.700000000000001066, -8.103009739378192577 ) ) ;
#168067 = ORIENTED_EDGE ( 'NONE', *, *, #157657, .F. ) ;
#168068 = CARTESIAN_POINT ( 'NONE',  ( 3.525891238081061640, 2.020528833579691597, -0.4508363271973143682 ) ) ;
#168069 = CARTESIAN_POINT ( 'NONE',  ( -1.201851678989727383E-14, 3.962500000000022116, 1.732050807568877637 ) ) ;
#168070 = CARTESIAN_POINT ( 'NONE',  ( 3.811813743736467419, 7.598866467667865443, 1.040834085586084257E-14 ) ) ;
#168071 = CARTESIAN_POINT ( 'NONE',  ( -6.477282242306868554, 6.848760321534919093, 0.6499626829332164624 ) ) ;
#168072 = CARTESIAN_POINT ( 'NONE',  ( 0.9615888033541221125, -1.593469042607889463, -1.240847856016368489 ) ) ;
#168073 = CARTESIAN_POINT ( 'NONE',  ( -1.500000000000011324, 5.879166666666686858, -0.8660254037844312691 ) ) ;
#168074 = ORIENTED_EDGE ( 'NONE', *, *, #167387, .T. ) ;
#168075 = AXIS2_PLACEMENT_3D ( 'NONE', #204920, #173545, #3512 ) ;
#168077 = CARTESIAN_POINT ( 'NONE',  ( 6.805829924380097040, 10.88395931184472154, 0.7216878364870438212 ) ) ;
#168076 = CARTESIAN_POINT ( 'NONE',  ( 0.07479286986303290696, 5.725009232006174287, -2.449550298930736059 ) ) ;
#168078 = CARTESIAN_POINT ( 'NONE',  ( 6.345077344222471716, -1.080897578067066878, 1.701688803805063266 ) ) ;
#168079 = CARTESIAN_POINT ( 'NONE',  ( 6.192599819808762618, 1.414433556397393543, -1.292206900294754490 ) ) ;
#168080 = CARTESIAN_POINT ( 'NONE',  ( 6.639320575229256782, 4.691717626494606996, 2.665852771288126366 ) ) ;
#168081 = CARTESIAN_POINT ( 'NONE',  ( 3.351304529449970371, 0.5305821810032870234, -2.126252377916526992 ) ) ;
#168082 = CARTESIAN_POINT ( 'NONE',  ( 1.499999999999989120, 2.785416667349484676, 0.8660254037844524744 ) ) ;
#168083 = CARTESIAN_POINT ( 'NONE',  ( 3.849791259674230748, -1.322437695595569673, -1.381667681676468140 ) ) ;
#168084 = CARTESIAN_POINT ( 'NONE',  ( -4.985647801523292344, 6.839675073242382553, -1.599625672291256295 ) ) ;
#168085 = CARTESIAN_POINT ( 'NONE',  ( 3.294268137996273715, 5.826768013428865522, -1.082531754730543971 ) ) ;
#168087 = CARTESIAN_POINT ( 'NONE',  ( 0.7379079170338509464, 2.013986002441462198, -0.1017714793793283723 ) ) ;
#168086 = CARTESIAN_POINT ( 'NONE',  ( -9.991996023147281747, 11.72004545083573568, 1.082531754730558626 ) ) ;
#168088 = CARTESIAN_POINT ( 'NONE',  ( -0.6823417656250039265, 11.38020833367473017, -1.181850606188755259 ) ) ;
#168089 = B_SPLINE_CURVE_WITH_KNOTS ( 'NONE', 3,
 ( #89700, #109202, #155750, #27874 ),
 .UNSPECIFIED., .F., .F.,
 ( 4, 4 ),
 ( 0.000000000000000000, 0.0003289350697890357504 ),
 .UNSPECIFIED. ) ;
#168091 = CARTESIAN_POINT ( 'NONE',  ( -5.468734858265826837, 7.473552982767158070, 1.599625672291263179 ) ) ;
#168090 = CARTESIAN_POINT ( 'NONE',  ( 0.3633196395196974793, 0.2168307188613327052, -2.282096724506751162 ) ) ;
#168093 = ORIENTED_EDGE ( 'NONE', *, *, #151057, .F. ) ;
#168092 = CARTESIAN_POINT ( 'NONE',  ( 4.664925512212582781, -1.541612441252750543, -0.7736475682248912245 ) ) ;
#168094 = CARTESIAN_POINT ( 'NONE',  ( 6.773376349083131132, 7.849261790823902629, 6.661184041420955992 ) ) ;
#168095 = CARTESIAN_POINT ( 'NONE',  ( 7.796102023057898123, 9.054206100777749455, -1.199719254218441611 ) ) ;
#168096 = CARTESIAN_POINT ( 'NONE',  ( 3.334415713957098681, 5.977569868670206787, -1.199719254218446718 ) ) ;
#168097 = DIRECTION ( 'NONE',  ( 8.638326563840814399E-31, -0.000000000000000000, 1.000000000000000000 ) ) ;
#168098 = CARTESIAN_POINT ( 'NONE',  ( 0.9417639971489067952, 1.314929008279978495, 1.456166070238865018 ) ) ;
#168099 =( NAMED_UNIT ( * ) SI_UNIT ( $, .STERADIAN. ) SOLID_ANGLE_UNIT ( ) );
#168100 = CARTESIAN_POINT ( 'NONE',  ( 5.366329872910639232, 5.155139694684188534, 1.040834085586084257E-14 ) ) ;
#168101 = CARTESIAN_POINT ( 'NONE',  ( 0.1751657365761521701, 0.7240325161481726557, -2.128694924679303213 ) ) ;
#168102 = ORIENTED_EDGE ( 'NONE', *, *, #74664, .F. ) ;
#168103 = CARTESIAN_POINT ( 'NONE',  ( 11.04536101718726293, 12.69999999999999929, -1.100000000000000311 ) ) ;
#168104 = VERTEX_POINT ( 'NONE', #129060 ) ;
#168105 = CARTESIAN_POINT ( 'NONE',  ( 3.844242791777858770, 0.9658850817777319131, -1.532267982868290579 ) ) ;
#168106 = ORIENTED_EDGE ( 'NONE', *, *, #191412, .T. ) ;
#168107 = CARTESIAN_POINT ( 'NONE',  ( 4.857564175446106525, 8.889184981320973122, 0.7998128361456331437 ) ) ;
#168108 = CARTESIAN_POINT ( 'NONE',  ( 4.947799714344386146, 4.737130853015369958, -0.7998128361456481317 ) ) ;
#168109 = CARTESIAN_POINT ( 'NONE',  ( 5.338451399618321602, 1.074232541698511900, -1.458426962581545361 ) ) ;
#168110 = CARTESIAN_POINT ( 'NONE',  ( 5.519577934094851202, 8.493239118869080784, 1.082531754730547524 ) ) ;
#168111 = CARTESIAN_POINT ( 'NONE',  ( 11.00605293250196226, 13.60925261358443095, -1.443095658425808114 ) ) ;
#168112 = CARTESIAN_POINT ( 'NONE',  ( 5.144285979226959959, 6.473071224410549718, -1.197504025336363576 ) ) ;
#168114 = CARTESIAN_POINT ( 'NONE',  ( 10.16199982864259788, 11.81442020729326536, 1.199719254218452047 ) ) ;
#168113 = CARTESIAN_POINT ( 'NONE',  ( 6.707467475981614413, -1.495571456699902546, -1.107353707014941069 ) ) ;
#168115 = CARTESIAN_POINT ( 'NONE',  ( 3.972214814312221343, -1.895280843596976350, -0.2773303961090283765 ) ) ;
#168116 = CARTESIAN_POINT ( 'NONE',  ( -6.439526774797413644, -8.199734048662943309, -6.984891963203985199 ) ) ;
#168117 = CARTESIAN_POINT ( 'NONE',  ( -10.91672646594461327, 4.673612064222224305, 4.467269497407427181 ) ) ;
#168118 = CARTESIAN_POINT ( 'NONE',  ( 9.499766273075866962, -9.919999999999998153, -0.06663900456893058488 ) ) ;
#168119 = CARTESIAN_POINT ( 'NONE',  ( 6.860062538834778678, 8.066123052471139587, -1.082531754730543083 ) ) ;
#168120 = CARTESIAN_POINT ( 'NONE',  ( -4.451154503988200339, 4.087435097607984957, 1.214306433183764966E-14 ) ) ;
#168121 = CARTESIAN_POINT ( 'NONE',  ( 0.9717996764858798375, 2.083101276202529384, -0.5774176476955604764 ) ) ;
#168122 = CARTESIAN_POINT ( 'NONE',  ( -6.394605727500880299, 7.489403432619674561, -1.199719254218452047 ) ) ;
#168123 = CARTESIAN_POINT ( 'NONE',  ( 5.716698046817569434, 6.698511138489155137, -1.199719254218452047 ) ) ;
#168124 = CARTESIAN_POINT ( 'NONE',  ( 0.8326870614539466642, 0.1294382003846420159, 1.821050407652326619 ) ) ;
#168125 = CARTESIAN_POINT ( 'NONE',  ( -6.227272627378437342, 6.159572908229946187, -0.7998128361456291469 ) ) ;
#168126 = CARTESIAN_POINT ( 'NONE',  ( 4.084828617465196210, -0.1788469021064206521, -1.816781805555576668 ) ) ;
#168127 = CARTESIAN_POINT ( 'NONE',  ( 10.81425746553161460, 10.30853785568457326, -6.489671246970442731 ) ) ;
#168128 = CARTESIAN_POINT ( 'NONE',  ( 1.529408426332915960, -0.2309274165002393187, 1.898302859121250297 ) ) ;
#168129 = CARTESIAN_POINT ( 'NONE',  ( 2.840245056987787287, -1.014795158497614036, 1.687856822838776916 ) ) ;
#168130 = CARTESIAN_POINT ( 'NONE',  ( 3.948723843360758323, -1.616405859212793894, -1.076207510925797139 ) ) ;
#168131 = CARTESIAN_POINT ( 'NONE',  ( -4.625266680917477835, 5.425174544939014964, -1.199719254218453823 ) ) ;
#168133 = CARTESIAN_POINT ( 'NONE',  ( 4.570628194609677841, 0.8141925398062774821, 1.958264201954627026 ) ) ;
#168132 = CARTESIAN_POINT ( 'NONE',  ( 5.259637247458703868, 5.100941308315409373, 0.000000000000000000 ) ) ;
#168134 = CARTESIAN_POINT ( 'NONE',  ( 0.000000000000000000, -11.15905291171102931, 0.000000000000000000 ) ) ;
#168135 = CARTESIAN_POINT ( 'NONE',  ( 7.587759525142423911, 12.00413654597487501, 0.7998128361456462443 ) ) ;
#168136 = CARTESIAN_POINT ( 'NONE',  ( 6.017762162252820346, 6.076696597586958681, 0.5614182107811436229 ) ) ;
#168137 = CARTESIAN_POINT ( 'NONE',  ( 0.7500000000000006661, 11.69791666734946389, -1.299038105676657340 ) ) ;
#168138 = ORIENTED_EDGE ( 'NONE', *, *, #92189, .F. ) ;
#168139 = CARTESIAN_POINT ( 'NONE',  ( 4.712340909201580885, 7.655425606447271214, -1.199719254218452047 ) ) ;
#168141 =( BOUNDED_CURVE ( )  B_SPLINE_CURVE ( 1, ( #43544, #28334 ),
 .UNSPECIFIED., .F., .T. ) 
 B_SPLINE_CURVE_WITH_KNOTS ( ( 2, 2 ),
 ( 0.000000000000000000, 1.644734566718861202E-05 ),
 .UNSPECIFIED. ) 
 CURVE ( )  GEOMETRIC_REPRESENTATION_ITEM ( )  RATIONAL_B_SPLINE_CURVE ( ( 0.9345202395942817652, 0.9345202395942817652 ) ) 
 REPRESENTATION_ITEM ( '' )  );
#168140 = CARTESIAN_POINT ( 'NONE',  ( 11.97178994924802353, 12.22000006202794609, -0.8322011300497145214 ) ) ;
#168143 = CARTESIAN_POINT ( 'NONE',  ( 6.051970301643104122, 1.040788372175960541, 1.727066800951609249 ) ) ;
#168142 = CARTESIAN_POINT ( 'NONE',  ( 3.475057130574196407, 0.04366187338752242769, -1.825333387291371512 ) ) ;
#168144 = CARTESIAN_POINT ( 'NONE',  ( 0.2388460773940295212, -2.007853281042128568, -0.5044432775610437902 ) ) ;
#168145 = CARTESIAN_POINT ( 'NONE',  ( -7.700668062882059850, 11.92793714009701311, -0.7216878364870267237 ) ) ;
#168146 = CARTESIAN_POINT ( 'NONE',  ( -5.012442140716328431, 8.020463026761962766, 1.150573971286508845 ) ) ;
#168147 = CARTESIAN_POINT ( 'NONE',  ( 6.935047222998001359, -6.682123388834269484, -6.658747417466178931 ) ) ;
#168148 = CARTESIAN_POINT ( 'NONE',  ( 4.645289301550183936, -1.446173438076237217, -1.186536486241091204 ) ) ;
#168149 = CARTESIAN_POINT ( 'NONE',  ( 6.968000882419564945, 10.21675256520979858, 1.199719254218460707 ) ) ;
#168150 = CARTESIAN_POINT ( 'NONE',  ( 3.176308805823165660, -1.146983237646619580, 1.547710939905672989 ) ) ;
#168151 = CARTESIAN_POINT ( 'NONE',  ( 0.1664695996868958416, 2.800000000000018030, 1.413346573192864497 ) ) ;
#168152 = EDGE_CURVE ( 'NONE', #207114, #85668, #603, .T. ) ;
#168153 = CARTESIAN_POINT ( 'NONE',  ( 4.029797971759831121, 5.724516938518342535, -1.599625672291255185 ) ) ;
#168154 = CARTESIAN_POINT ( 'NONE',  ( -1.364683531250010295, 9.442708333674733723, 0.7879004041258445001 ) ) ;
#168155 = CARTESIAN_POINT ( 'NONE',  ( -6.063521013809733518, 8.097193820909906137, 1.599625672291283607 ) ) ;
#168156 = FACE_OUTER_BOUND ( 'NONE', #95703, .T. ) ;
#168157 = CARTESIAN_POINT ( 'NONE',  ( -3.146901051703345331, 6.685485303713597283, 0.000000000000000000 ) ) ;
#168158 = STYLED_ITEM ( 'NONE', ( #144143 ), #126462 ) ;
#168159 = CARTESIAN_POINT ( 'NONE',  ( 1.704857254432812219, 1.976886250939764889, 0.7584849220025058347 ) ) ;
#168160 = CARTESIAN_POINT ( 'NONE',  ( 7.404724451357931336, 11.79059562655963056, 0.7998128361456462443 ) ) ;
#168161 = FACE_OUTER_BOUND ( 'NONE', #9633, .T. ) ;
#168162 = CARTESIAN_POINT ( 'NONE',  ( 6.526242037438201749, 1.059062773735760521, 1.778703558766213000 ) ) ;
#168164 = CARTESIAN_POINT ( 'NONE',  ( 4.078932850288060408, 7.722175824222965446, -0.6089670364913578604 ) ) ;
#168163 = CARTESIAN_POINT ( 'NONE',  ( 0.7140992756325339474, 1.701125707204936166, 0.7050099338341904165 ) ) ;
#168165 = CARTESIAN_POINT ( 'NONE',  ( 6.029976284357474903, -1.944044770632427976, 1.226447132130564999 ) ) ;
#168166 = CARTESIAN_POINT ( 'NONE',  ( 5.422898255786183341, 7.349800603215774331, -1.443375672974051449 ) ) ;
#168167 = CARTESIAN_POINT ( 'NONE',  ( 4.963693636378940788, 5.923969009597785274, -1.082531754730548412 ) ) ;
#168168 = CARTESIAN_POINT ( 'NONE',  ( 1.974976472051133136, -0.1153332747052069479, -2.289479170392795915 ) ) ;
#168169 = CARTESIAN_POINT ( 'NONE',  ( -5.717509255324703332, 7.006698007003612894, 2.500000000000000444 ) ) ;
#168170 = CARTESIAN_POINT ( 'NONE',  ( -6.635789839245807897, 6.706452665400368218, 0.7998128361456341429 ) ) ;
#168171 = CARTESIAN_POINT ( 'NONE',  ( 6.158146451363091245, -1.371594178524730534, 1.374984930127883143 ) ) ;
#168172 = ORIENTED_EDGE ( 'NONE', *, *, #11493, .T. ) ;
#168173 = CARTESIAN_POINT ( 'NONE',  ( 8.446366511189332016, 9.916811020218137429, -1.082531754730543083 ) ) ;
#168174 = ADVANCED_FACE ( 'NONE', ( #110655 ), #27191, .F. ) ;
#168175 = CARTESIAN_POINT ( 'NONE',  ( 1.125244999914726263, 1.777361856972861531, 0.9454465733411165917 ) ) ;
#168176 = CARTESIAN_POINT ( 'NONE',  ( -1.225000000000005640, 2.812500000682796486, -1.734723475976807094E-15 ) ) ;
#168178 = CARTESIAN_POINT ( 'NONE',  ( -11.92619526913700057, 19.00000000000000000, -1.328859060402686199 ) ) ;
#168177 = CARTESIAN_POINT ( 'NONE',  ( -6.516665389662827934, 10.75452672124865217, 0.000000000000000000 ) ) ;
#168179 = DIRECTION ( 'NONE',  ( 0.000000000000000000, -1.000000000000000000, 0.000000000000000000 ) ) ;
#168181 = CARTESIAN_POINT ( 'NONE',  ( 2.166550811918485753, -1.616863761265506794, -0.7202261968358366628 ) ) ;
#168180 = CARTESIAN_POINT ( 'NONE',  ( 3.187526948619547884, -0.8467841439671991433, 1.911654264539459191 ) ) ;
#168182 = CARTESIAN_POINT ( 'NONE',  ( -3.602337597214539753E-15, 12.06250000000000178, 1.500000000000001554 ) ) ;
#168184 = CARTESIAN_POINT ( 'NONE',  ( 4.857543142518937707, 2.267833309424868826, -0.3330599157496324514 ) ) ;
#168183 = CARTESIAN_POINT ( 'NONE',  ( -11.13994541198518640, 5.786402032167232257, -4.475860200623921870 ) ) ;
#168185 = CARTESIAN_POINT ( 'NONE',  ( 3.802475355173411842, 1.493833042257145305, 0.8925963562203437229 ) ) ;
#168186 = CARTESIAN_POINT ( 'NONE',  ( 8.204655514564224816, 12.72384853363364066, 1.040834085586084257E-14 ) ) ;
#168187 = CARTESIAN_POINT ( 'NONE',  ( 5.910428620914669473, 5.860197910680708944, 0.000000000000000000 ) ) ;
#168188 = CARTESIAN_POINT ( 'NONE',  ( 3.672919734203412112, -0.7009596788165352033, -1.586013134846143480 ) ) ;
#168189 = CARTESIAN_POINT ( 'NONE',  ( 3.877515590359277287, -0.1633623659567252084, 2.165103034678467431 ) ) ;
#168190 = CARTESIAN_POINT ( 'NONE',  ( 3.662674053986138656, 7.424870162959149589, 0.7998128361456321445 ) ) ;
#168191 = CARTESIAN_POINT ( 'NONE',  ( 4.979703994296570180, -0.7212954316567052881, 1.883311551353183511 ) ) ;
#168192 = CARTESIAN_POINT ( 'NONE',  ( 6.750000000000005329, 7.629137130509070275, 2.600000000000000533 ) ) ;
#168193 = CARTESIAN_POINT ( 'NONE',  ( 0.7499999999999902300, 3.764583334016149863, 1.299038105676669330 ) ) ;
#168194 = CARTESIAN_POINT ( 'NONE',  ( 1.799704718893188282, -0.6512145186477935610, 1.813102765825167273 ) ) ;
#168195 = CARTESIAN_POINT ( 'NONE',  ( -0.7500000000000179856, 8.572916667349467446, 1.299038105676658228 ) ) ;
#168196 = CARTESIAN_POINT ( 'NONE',  ( 6.099871961099720963, 1.531114646448136218, 1.609653004599376658 ) ) ;
#168197 = EDGE_LOOP ( 'NONE', ( #174054, #84983, #201734, #90992 ) ) ;
#168198 = CARTESIAN_POINT ( 'NONE',  ( -0.2108831679771168421, 6.948330828014878335, -2.492181822431015270 ) ) ;
#168199 = CARTESIAN_POINT ( 'NONE',  ( 1.499999999999987121, 2.004166666666684637, 0.8660254037844524744 ) ) ;
#168200 = CARTESIAN_POINT ( 'NONE',  ( 6.693975156845185737, 8.832723654451292816, 1.599625672291281386 ) ) ;
#168201 = CARTESIAN_POINT ( 'NONE',  ( 4.704316113817540668, 5.551085556617666228, -1.082531754730548412 ) ) ;
#168202 = CARTESIAN_POINT ( 'NONE',  ( 1.642778471875001811, -1.042708332855375009, 2.845375778867859751 ) ) ;
#168203 = CARTESIAN_POINT ( 'NONE',  ( 0.8740457437188209333, 0.4279768726487084285, -2.179530559632827824 ) ) ;
#168204 = CARTESIAN_POINT ( 'NONE',  ( 5.564887814092526419, 1.486691789297952093, -1.280227714881218670 ) ) ;
#168205 = CARTESIAN_POINT ( 'NONE',  ( 7.944714827928039291, 11.25228915168265864, 1.082531754730557072 ) ) ;
#168206 = CARTESIAN_POINT ( 'NONE',  ( -0.4152101148468765324, 3.244511181007482481, 1.956683416369788819 ) ) ;
#168207 = CARTESIAN_POINT ( 'NONE',  ( 0.4038910500440278106, -0.5768866637368921246, 2.083095904058133385 ) ) ;
#168208 = CARTESIAN_POINT ( 'NONE',  ( 4.583538449871731757, 7.505156070562471804, 1.199719254218451159 ) ) ;
#168209 = CARTESIAN_POINT ( 'NONE',  ( -5.980555157403903976, 6.149938236492225485, 0.000000000000000000 ) ) ;
#168210 = CARTESIAN_POINT ( 'NONE',  ( 4.141125080024585792, -0.1993089607698217136, -2.053009638179447371 ) ) ;
#168211 = CARTESIAN_POINT ( 'NONE',  ( -4.205000198532790279, 8.057583998263570635, 0.7998128361456341429 ) ) ;
#168212 = CARTESIAN_POINT ( 'NONE',  ( 0.7499999999999902300, 4.347916667349481123, -1.299038105676658228 ) ) ;
#168213 = CARTESIAN_POINT ( 'NONE',  ( -0.6823417656250003738, -1.032291666325242607, -1.181850606188749264 ) ) ;
#168214 = CARTESIAN_POINT ( 'NONE',  ( 5.571519856497625156, 1.802974293077023393, -0.4980454429602265698 ) ) ;
#168215 = CARTESIAN_POINT ( 'NONE',  ( 4.992643705478089444, -1.725105917503889641, 0.1769386724924902066 ) ) ;
#168216 = CARTESIAN_POINT ( 'NONE',  ( 2.823474877308090214, 0.9648067800103199421, -1.448311861076934104 ) ) ;
#168217 = CARTESIAN_POINT ( 'NONE',  ( 8.663296969007976855, 12.09063498294259809, -1.082531754730543083 ) ) ;
#168218 = CARTESIAN_POINT ( 'NONE',  ( 1.382826565882399272, -0.3421621995536459626, -2.266597836251768250 ) ) ;
#168219 = CARTESIAN_POINT ( 'NONE',  ( -1.201851678989727383E-14, 3.509375000341421469, -1.575800808251660134 ) ) ;
#168220 = CARTESIAN_POINT ( 'NONE',  ( 5.952696063536119908, -1.793662432779649540, -1.073965677532197072 ) ) ;
#168221 = CARTESIAN_POINT ( 'NONE',  ( -0.01213283819992416745, -0.3988646234997471618, -1.803908381610368261 ) ) ;
#168222 = AXIS2_PLACEMENT_3D ( 'NONE', #143738, #180452, #209732 ) ;
#168223 = CARTESIAN_POINT ( 'NONE',  ( 0.04582610853910489696, -10.00039265882532646, 11.00004154231811526 ) ) ;
#168224 = SURFACE_STYLE_USAGE ( .BOTH. , #102157 ) ;
#168225 = CARTESIAN_POINT ( 'NONE',  ( 1.811172873341511336, 1.158687402475454098, -1.650082692374904125 ) ) ;
#168226 = EDGE_CURVE ( 'NONE', #77503, #134499, #62461, .T. ) ;
#168227 = DIRECTION ( 'NONE',  ( 0.6507913734559712671, 0.7592566023652943530, 0.000000000000000000 ) ) ;
#168228 = CARTESIAN_POINT ( 'NONE',  ( 8.964365016547233722, 14.59103508737832300, -8.971863053630826812 ) ) ;
#168229 = CARTESIAN_POINT ( 'NONE',  ( -8.311311860377216476, 9.655284244316948872, -1.199719254218446718 ) ) ;
#168230 = CARTESIAN_POINT ( 'NONE',  ( 4.482942347612929979, 8.381849838857084123, 1.040834085586084257E-14 ) ) ;
#168231 = CARTESIAN_POINT ( 'NONE',  ( 2.965608807194367369, -1.734805745614193873, -1.219131234129526398 ) ) ;
#168232 = CARTESIAN_POINT ( 'NONE',  ( -1.402160292154681736E-14, -0.9281249996585830830, 1.575800808251672791 ) ) ;
#168233 = CARTESIAN_POINT ( 'NONE',  ( 5.197797600609998625, -0.6536857159176562293, 1.704833070275885598 ) ) ;
#168234 = ORIENTED_EDGE ( 'NONE', *, *, #171794, .T. ) ;
#168235 = CARTESIAN_POINT ( 'NONE',  ( -7.442499979258930587, 7.647614495415686164, -0.7998128361456362523 ) ) ;
#168236 = CARTESIAN_POINT ( 'NONE',  ( -1.737499999999997824, -3.747916665710750994, 3.009438278150925683 ) ) ;
#168237 = CARTESIAN_POINT ( 'NONE',  ( -4.855791571988752331, 8.816840600628864877, 0.7998128361456481317 ) ) ;
#168238 = CARTESIAN_POINT ( 'NONE',  ( 2.636978264590104537, 1.903244974434484371, 0.6766128908266034747 ) ) ;
#168239 = CARTESIAN_POINT ( 'NONE',  ( 6.247136877606230598, -1.867572634706683443, 1.175315980461520304 ) ) ;
#168240 = CARTESIAN_POINT ( 'NONE',  ( 8.218213668177886788, 12.73966637951625813, 0.7998128361456462443 ) ) ;
#168241 = CARTESIAN_POINT ( 'NONE',  ( 3.906960136656021376, -1.523566986099005316, 1.068299854780943692 ) ) ;
#168242 = CARTESIAN_POINT ( 'NONE',  ( 7.703003830858588863, 12.13858823597705872, -0.7998128361456291469 ) ) ;
#168243 = CARTESIAN_POINT ( 'NONE',  ( -9.953865251629775202, 4.532720649454268447, -6.624712979280865888 ) ) ;
#168244 = VERTEX_POINT ( 'NONE', #26124 ) ;
#168245 = CARTESIAN_POINT ( 'NONE',  ( -4.277761160311629673, 4.949475094240346706, 1.199719254218462483 ) ) ;
#168246 = CARTESIAN_POINT ( 'NONE',  ( -9.020252271793614440, 9.418049160047695878, 0.7998128361456462443 ) ) ;
#168247 = CARTESIAN_POINT ( 'NONE',  ( 4.863791234866603475, 1.805334366393744450, -0.2710410529033688842 ) ) ;
#168249 = CARTESIAN_POINT ( 'NONE',  ( -4.503925953283787642, 7.237052973511334919, 1.308369160636771333 ) ) ;
#168248 = CARTESIAN_POINT ( 'NONE',  ( -5.562588163356775972, 9.711712967216715953, 0.7998128361456291469 ) ) ;
#168250 = CARTESIAN_POINT ( 'NONE',  ( -0.6823417656250246877, -1.198958332991911790, 1.181850606188755259 ) ) ;
#168251 = CARTESIAN_POINT ( 'NONE',  ( 1.756802591741468245, -1.724947740463366852, -0.1754148046573481556 ) ) ;
#168252 = CARTESIAN_POINT ( 'NONE',  ( 1.271012957286155709, 1.034212954684173180, 1.399518829098946204 ) ) ;
#168254 = CARTESIAN_POINT ( 'NONE',  ( 9.110716038703335684, 9.731516254683127087, -0.7216878364870197293 ) ) ;
#168253 = CARTESIAN_POINT ( 'NONE',  ( 5.426528828858072195, 1.378586375901286187, -1.850541897242431677 ) ) ;
#168255 = CARTESIAN_POINT ( 'NONE',  ( 6.204464077730128757, 7.037555732820855781, 1.030856974308017149 ) ) ;
#168256 = CARTESIAN_POINT ( 'NONE',  ( 1.370465108300226609, -1.309671233245520483, 1.591056919209728138 ) ) ;
#168257 = CARTESIAN_POINT ( 'NONE',  ( 5.307127064745490230, 8.279066444590018392, -1.199719254218452935 ) ) ;
#168258 = CARTESIAN_POINT ( 'NONE',  ( 0.4212496859960760953, 0.7689994822442263178, 1.863884711849304487 ) ) ;
#168259 = CARTESIAN_POINT ( 'NONE',  ( 7.188044520085388633, 15.44694694233605148, -9.560164038293452293 ) ) ;
#168260 = CARTESIAN_POINT ( 'NONE',  ( -4.749098946536820520, 8.762642214260091933, 0.7998128361456281477 ) ) ;
#168261 = CARTESIAN_POINT ( 'NONE',  ( 0.1804621682222322943, -1.911711055282316662, -0.4813082943134691094 ) ) ;
#168263 = CARTESIAN_POINT ( 'NONE',  ( -7.919371124158132602, 8.411890197705517380, -0.7216878364870338292 ) ) ;
#168262 = CARTESIAN_POINT ( 'NONE',  ( 3.129067941553372645, 1.730785544086024696, 0.8136490247460312908 ) ) ;
#168264 = CARTESIAN_POINT ( 'NONE',  ( 5.760442859251142522, 0.8911043219209063837, 2.019162844794204048 ) ) ;
#168265 = CARTESIAN_POINT ( 'NONE',  ( 1.224999999999991651, 2.437500000682837786, -4.336808689942017736E-14 ) ) ;
#168266 = EDGE_CURVE ( 'NONE', #63230, #18446, #145542, .T. ) ;
#168267 = CARTESIAN_POINT ( 'NONE',  ( -7.146556367734805626, 9.431011410480991231, 1.443375672974064550 ) ) ;
#168268 = CARTESIAN_POINT ( 'NONE',  ( 4.326460416092276162, 7.101268681199365496, -1.082531754730548412 ) ) ;
#168269 = CARTESIAN_POINT ( 'NONE',  ( -4.082413651046300274, 6.816547455312373494, 1.082531754730549967 ) ) ;
#168270 = CARTESIAN_POINT ( 'NONE',  ( 6.322909428431959356, 1.571596504679906303, -1.423730336690950393 ) ) ;
#168271 = CARTESIAN_POINT ( 'NONE',  ( 3.962222562901392742, 2.290579029535879219, -0.2790985642298955405 ) ) ;
#168272 = CARTESIAN_POINT ( 'NONE',  ( 5.336364984333265227, -1.091323163865608459, 1.630109012322231266 ) ) ;
#168273 = CARTESIAN_POINT ( 'NONE',  ( 0.8835585337332927391, -1.864609544942645414, 0.6100022000963196689 ) ) ;
#168274 = CARTESIAN_POINT ( 'NONE',  ( 8.220324289656684158, 15.16505199276374150, 8.682849841995956552 ) ) ;
#168275 = CARTESIAN_POINT ( 'NONE',  ( -11.92619526913699879, 13.39999999999998259, 1.328859060402684644 ) ) ;
#168276 = ORIENTED_EDGE ( 'NONE', *, *, #109130, .F. ) ;
#168277 = CARTESIAN_POINT ( 'NONE',  ( 6.385953923436008317, -2.015982004707029596, 0.05432014494890363698 ) ) ;
#168278 = EDGE_CURVE ( 'NONE', #146971, #129573, #176576, .T. ) ;
#168279 = CARTESIAN_POINT ( 'NONE',  ( -6.970863535720637216, 11.28442455831609337, 0.7998128361456481317 ) ) ;
#168280 = CARTESIAN_POINT ( 'NONE',  ( 0.005434845660363255178, -0.7843016415976924449, -1.664241202765592176 ) ) ;
#168282 = AXIS2_PLACEMENT_3D ( 'NONE', #90306, #172626, #22055 ) ;
#168281 = CARTESIAN_POINT ( 'NONE',  ( 3.573241956510754491, 1.960547127731948613, 0.9329660139856699175 ) ) ;
#168283 = B_SPLINE_CURVE_WITH_KNOTS ( 'NONE', 3,
 ( #208601, #151621, #26664, #3187, #120245, #109061, #201393 ),
 .UNSPECIFIED., .F., .F.,
 ( 4, 3, 4 ),
 ( 2.109323616200222937E-18, 2.617081137855649704E-05, 3.552777339501059120E-05 ),
 .UNSPECIFIED. ) ;
#168284 = CARTESIAN_POINT ( 'NONE',  ( 0.4149352601330746348, 2.754396095944236400, 1.956746367768555706 ) ) ;
#168286 = ADVANCED_FACE ( 'NONE', ( #46667 ), #61435, .T. ) ;
#168285 = CARTESIAN_POINT ( 'NONE',  ( 0.6332531790259123827, 1.961634380476449335, 0.8060562103610890983 ) ) ;
#168287 = CARTESIAN_POINT ( 'NONE',  ( 1.499999999999989120, 2.056250000682817269, 1.214306433183764966E-14 ) ) ;
#168288 = CARTESIAN_POINT ( 'NONE',  ( 9.890836756369282057, 11.49806328964105617, -1.199719254218440723 ) ) ;
#168289 = CARTESIAN_POINT ( 'NONE',  ( 11.97929049433706084, 13.79999999999999893, -0.7046979865771820783 ) ) ;
#168290 = CARTESIAN_POINT ( 'NONE',  ( 6.400241882075590638, 6.902609158730609096, 0.7749192096189911894 ) ) ;
#168291 = VERTEX_POINT ( 'NONE', #148425 ) ;
#168292 = CARTESIAN_POINT ( 'NONE',  ( 1.739600335799436737, -1.490509515545968666, -1.423327880080206720 ) ) ;
#168294 = CARTESIAN_POINT ( 'NONE',  ( 6.204464077730128757, 7.037555732820855781, 1.030856974308017149 ) ) ;
#168293 = LINE ( 'NONE', #186663, #77233 ) ;
#168295 = CARTESIAN_POINT ( 'NONE',  ( -0.6823417656250003738, 1.717708333674752730, -1.181850606188749264 ) ) ;
#168296 = CARTESIAN_POINT ( 'NONE',  ( 0.7499999999999920064, 5.483333333333353821, 1.299038105676669330 ) ) ;
#168297 = ORIENTED_EDGE ( 'NONE', *, *, #14021, .F. ) ;
#168298 = CARTESIAN_POINT ( 'NONE',  ( 4.002528454542265024, -1.891902218777557598, -0.2775262981309714605 ) ) ;
#168299 = CARTESIAN_POINT ( 'NONE',  ( -1.520658191422891603, -0.9880266363068606061, 3.134631954704482748 ) ) ;
#168300 = CARTESIAN_POINT ( 'NONE',  ( 6.561402770032070286, 0.3947617697056918784, -2.227681008968500631 ) ) ;
#168301 = CARTESIAN_POINT ( 'NONE',  ( -4.115063316947640715, 4.759660943649018705, 1.199719254218462483 ) ) ;
#168302 = CARTESIAN_POINT ( 'NONE',  ( 1.757782220650351723, 0.6909716962627761028, -1.674832866754811578 ) ) ;
#168303 = CARTESIAN_POINT ( 'NONE',  ( 0.9365811914238668656, -1.507994439141499221, 1.181323522483549437 ) ) ;
#168304 = CARTESIAN_POINT ( 'NONE',  ( 1.856005582152659317, -0.6995316168164237292, 1.948720873434762080 ) ) ;
#168305 = CARTESIAN_POINT ( 'NONE',  ( -0.6823417656250003738, 0.03020833367475134201, -1.181850606188749264 ) ) ;
#168306 = CARTESIAN_POINT ( 'NONE',  ( 0.8132764231247009423, -0.2916495841569742842, 1.949667021961091429 ) ) ;
#168307 = CARTESIAN_POINT ( 'NONE',  ( 5.795520199677122619, 1.460474902364042649, 1.256451531516086684 ) ) ;
#168309 = CARTESIAN_POINT ( 'NONE',  ( 5.960708871395055120, 7.108654626955757116, 1.090683939682752124 ) ) ;
#168308 = CARTESIAN_POINT ( 'NONE',  ( 0.5577797733781300060, -1.952719008213155139, -1.229525757098411942 ) ) ;
#168310 = CARTESIAN_POINT ( 'NONE',  ( -1.402160292154681736E-14, 1.946875000341422579, -1.575800808251660134 ) ) ;
#168311 = VECTOR ( 'NONE', #195238, 1000.000000000000000 ) ;
#168312 = CARTESIAN_POINT ( 'NONE',  ( 4.246570442813556667, -2.039787899008322469, -0.3057716575347816934 ) ) ;
#168313 = CARTESIAN_POINT ( 'NONE',  ( -7.549192604710863286, 7.701812881784464437, -0.7998128361456291469 ) ) ;
#168314 = CARTESIAN_POINT ( 'NONE',  ( 8.613507663383630941, 8.943513783569379427, -0.7998128361456221525 ) ) ;
#168315 = CARTESIAN_POINT ( 'NONE',  ( 0.000000000000000000, 18.91999999999999815, 11.92000000000000171 ) ) ;
#168316 = ADVANCED_FACE ( 'NONE', ( #15193 ), #47745, .F. ) ;
#168317 = CARTESIAN_POINT ( 'NONE',  ( 4.873266149108180123, 7.772895376346490970, 1.199719254218462483 ) ) ;
#168319 = CARTESIAN_POINT ( 'NONE',  ( -1.201851678989727383E-14, 4.337500000000023448, -1.732050807568863648 ) ) ;
#168318 = CARTESIAN_POINT ( 'NONE',  ( 5.526436043951506782, 1.257118228488460110, -1.689427636868174210 ) ) ;
#168320 = CIRCLE ( 'NONE', #78479, 0.5000000000000004441 ) ;
#168321 = CARTESIAN_POINT ( 'NONE',  ( 6.848098043024292814, -0.8888149443028300345, 1.868052569137634400 ) ) ;
#168322 = CARTESIAN_POINT ( 'NONE',  ( -1.201851678989727383E-14, 1.634375000341421025, 1.575800808251672791 ) ) ;
#168323 = CARTESIAN_POINT ( 'NONE',  ( 4.868538603872567982, -1.416007186031362330, 1.633285015310452115 ) ) ;
#168324 = CARTESIAN_POINT ( 'NONE',  ( 4.319013676512412303, 1.559734590277090716, -1.283057401373039141 ) ) ;
#168325 = CARTESIAN_POINT ( 'NONE',  ( 6.720655732516676473, 3.678797444539682271, 2.787578482799071278 ) ) ;
#168328 = CARTESIAN_POINT ( 'NONE',  ( 6.819388077993785657, 7.058300300521964665, 1.040834085586084257E-14 ) ) ;
#168327 = CARTESIAN_POINT ( 'NONE',  ( -1.642778471875000035, -1.567708332855376252, -2.845375778867859751 ) ) ;
#168326 = CARTESIAN_POINT ( 'NONE',  ( 0.000000000000000000, -0.9200000000000041478, 0.000000000000000000 ) ) ;
#168329 = CARTESIAN_POINT ( 'NONE',  ( -4.782994330570982555, 8.802186828966616972, 0.000000000000000000 ) ) ;
#168330 = CARTESIAN_POINT ( 'NONE',  ( 2.676970549635893537, 1.727063564601112100, -1.040793759654296213 ) ) ;
#168331 = CARTESIAN_POINT ( 'NONE',  ( -8.799405390469187793, 10.22472669609091689, -1.199719254218446718 ) ) ;
#168333 = CARTESIAN_POINT ( 'NONE',  ( -0.6823417656250212460, 3.113541667008084879, 1.181850606188767472 ) ) ;
#168332 = CARTESIAN_POINT ( 'NONE',  ( -3.079673448598517549, 6.744702790006905424, 1.040834085586084257E-14 ) ) ;
#168334 = CARTESIAN_POINT ( 'NONE',  ( 1.499999999999996891, 12.64583333333333215, -0.8660254037844378194 ) ) ;
#168335 = CARTESIAN_POINT ( 'NONE',  ( 2.554955805669727020, 1.016282880930317933, -12.02012201174058603 ) ) ;
#168336 = CARTESIAN_POINT ( 'NONE',  ( 6.589320575229281829, 7.629137130509070275, 2.703262396134015866 ) ) ;
#168338 = CARTESIAN_POINT ( 'NONE',  ( 4.745720352911135365, 1.994069623535676961, -0.2986464557954356946 ) ) ;
#168337 = CARTESIAN_POINT ( 'NONE',  ( -6.507550544435101614, 10.53596670190887963, 0.000000000000000000 ) ) ;
#168339 = CARTESIAN_POINT ( 'NONE',  ( -1.500000000000011324, 4.920833333333354709, 0.8660254037844403729 ) ) ;
#168340 = CARTESIAN_POINT ( 'NONE',  ( 0.4688601960516668443, 0.1741500657085493509, -1.716052735907805937 ) ) ;
#168341 = CARTESIAN_POINT ( 'NONE',  ( 6.710359684120930091, 6.793450817754725257, 0.7998128361456352531 ) ) ;
#168343 = FACE_OUTER_BOUND ( 'NONE', #32316, .T. ) ;
#168342 = CARTESIAN_POINT ( 'NONE',  ( 9.083599731475992201, 9.699880562917908122, 0.7216878364870438212 ) ) ;
#168344 = CARTESIAN_POINT ( 'NONE',  ( -11.16790076368576834, 7.276266301664604086, 4.397334502061439387 ) ) ;
#168345 = CARTESIAN_POINT ( 'NONE',  ( 5.782452155351484713, -1.824793809246130438, -0.4103911052399379367 ) ) ;
#168346 = CARTESIAN_POINT ( 'NONE',  ( 6.293232695293600187, -0.1032093112793490142, -2.010699630015537309 ) ) ;
#168347 = DIRECTION ( 'NONE',  ( -1.000000000000000000, 0.000000000000000000, 0.000000000000000000 ) ) ;
#168348 = ORIENTED_EDGE ( 'NONE', *, *, #136238, .F. ) ;
#168349 = VECTOR ( 'NONE', #2903, 1000.000000000000000 ) ;
#168350 = CARTESIAN_POINT ( 'NONE',  ( -5.600926855776882540, 8.588146194164741232, -1.082531754730549967 ) ) ;
#168351 = ORIENTED_EDGE ( 'NONE', *, *, #150248, .T. ) ;
#168352 = CARTESIAN_POINT ( 'NONE',  ( 9.449669878600614581, 12.04770082983265844, -1.443375672974058777 ) ) ;
#168353 = CARTESIAN_POINT ( 'NONE',  ( 0.8433753223025289847, 0.3905737783656983431, -1.978056610397058490 ) ) ;
#168354 = CARTESIAN_POINT ( 'NONE',  ( 5.691390622686558487, 9.861982503101517139, 0.7998128361456341429 ) ) ;
#168355 = CARTESIAN_POINT ( 'NONE',  ( 6.262596564776618635, -1.532251275270900326, 1.525113613579494709 ) ) ;
#168356 = VECTOR ( 'NONE', #109192, 1000.000000000000000 ) ;
#168357 = CARTESIAN_POINT ( 'NONE',  ( 7.962716289927667113, 8.184257181204083409, -0.7998128361456291469 ) ) ;
#168359 = CARTESIAN_POINT ( 'NONE',  ( 0.1982580178685423022, 1.319089833320963079, -1.389493073782912091 ) ) ;
#168358 = CARTESIAN_POINT ( 'NONE',  ( -4.446184310277715213, 7.274633231044262516, -1.199719254218452047 ) ) ;
#168360 = CARTESIAN_POINT ( 'NONE',  ( -11.94655611907589865, 9.947990554530955265, -1.134828163062138628 ) ) ;
#168361 = CARTESIAN_POINT ( 'NONE',  ( 6.602457619730767391, 7.765583980183128787, 1.082531754730558626 ) ) ;
#168362 = CARTESIAN_POINT ( 'NONE',  ( -1.364683531250014514, -0.4072916663252447167, 0.7879004041258379498 ) ) ;
#168364 = VERTEX_POINT ( 'NONE', #167858 ) ;
#168363 = CARTESIAN_POINT ( 'NONE',  ( 3.714570900464278846, 5.356752022006865843, 1.443375672974062551 ) ) ;
#168365 = CARTESIAN_POINT ( 'NONE',  ( -3.755772246185468788, 4.340488027759846545, -1.199719254218452047 ) ) ;
#168366 = CONICAL_SURFACE ( 'NONE', #164968, 1.903066852858540603, 0.4537856055185301996 ) ;
#168367 = CARTESIAN_POINT ( 'NONE',  ( 3.661132068870280420, -1.905464569931826446, -1.020879743040298271 ) ) ;
#168368 = CARTESIAN_POINT ( 'NONE',  ( -5.316205630334251531, 9.216340645449683677, -0.7216878364870338292 ) ) ;
#168369 = CARTESIAN_POINT ( 'NONE',  ( 6.265276383290871109, 7.442482214328385304, -1.082531754730548412 ) ) ;
#168370 = CARTESIAN_POINT ( 'NONE',  ( 0.8090202166558431163, -0.5209130535433897924, -2.055487714681260236 ) ) ;
#168371 = CARTESIAN_POINT ( 'NONE',  ( -1.499999999999997780, 3.931250000682819046, 1.214306433183764966E-14 ) ) ;
#168372 = CARTESIAN_POINT ( 'NONE',  ( 2.055877211876644406, 1.966332055899377762, -0.1412752051469425008 ) ) ;
#168373 = EDGE_LOOP ( 'NONE', ( #116807, #89546, #192227, #187235 ) ) ;
#168374 = CARTESIAN_POINT ( 'NONE',  ( 4.814553946184248368, 7.670711132973337065, -1.082531754730548412 ) ) ;
#168375 = CARTESIAN_POINT ( 'NONE',  ( 6.109808257530946918, 0.5734047718448382902, -1.884209069281018500 ) ) ;
#168376 = CARTESIAN_POINT ( 'NONE',  ( 0.5681770160902823719, -1.828317568802136250, -0.6549081214334094847 ) ) ;
#168377 = ORIENTED_EDGE ( 'NONE', *, *, #141945, .T. ) ;
#168378 = CARTESIAN_POINT ( 'NONE',  ( -4.878955176071358757, 6.785476686873604280, -1.599625672291271394 ) ) ;
#168380 = CARTESIAN_POINT ( 'NONE',  ( 6.938893903907228378E-15, 10.64264068711930733, 1.214306433183764966E-14 ) ) ;
#168379 = CARTESIAN_POINT ( 'NONE',  ( -3.851398154733808088, 6.650992392901508232, -1.199719254218450271 ) ) ;
#168382 = CARTESIAN_POINT ( 'NONE',  ( 6.495764994278809823, 7.711385593814346073, 1.082531754730549967 ) ) ;
#168381 = CARTESIAN_POINT ( 'NONE',  ( 5.933664784275179294, 10.07435934829639912, -0.7998128361456291469 ) ) ;
#168384 = ORIENTED_EDGE ( 'NONE', *, *, #31325, .T. ) ;
#168383 = CARTESIAN_POINT ( 'NONE',  ( 4.565046243057500952, -1.533749416048999947, 1.141898535029245432 ) ) ;
#168385 = CARTESIAN_POINT ( 'NONE',  ( 3.211752199052122503, -0.4303563718574506813, 2.164345902561148005 ) ) ;
#168386 = CARTESIAN_POINT ( 'NONE',  ( 2.345003271878861373, 0.4830727525354863716, 2.153096645625157457 ) ) ;
#168387 = DIRECTION ( 'NONE',  ( 0.000000000000000000, 0.000000000000000000, -1.000000000000000000 ) ) ;
#168388 = CARTESIAN_POINT ( 'NONE',  ( 0.1352199593073095951, -0.09384731153385186819, 1.910084486482076294 ) ) ;
#168389 = CARTESIAN_POINT ( 'NONE',  ( -10.29915967087783102, 4.864502100071391943, 6.165526146199510116 ) ) ;
#168390 = CARTESIAN_POINT ( 'NONE',  ( 10.99931692196006949, -8.074346042903146170, -0.1488091642035823670 ) ) ;
#168391 = CARTESIAN_POINT ( 'NONE',  ( -6.684387857553246270, -6.724344753046691103, -6.908358566921309674 ) ) ;
#168392 = CARTESIAN_POINT ( 'NONE',  ( 2.998552181135269556, 2.054425100943928051, 0.2560010573490826835 ) ) ;
#168393 = CARTESIAN_POINT ( 'NONE',  ( -5.922214171070950606, 5.803671375871217286, -0.7998128361456291469 ) ) ;
#168394 = CARTESIAN_POINT ( 'NONE',  ( -4.721755537811513470, 8.238515690766082145, -0.6557258408305451924 ) ) ;
#168396 = CARTESIAN_POINT ( 'NONE',  ( 0.3741789627117291239, 1.245922373857488274, 1.766349570875298758 ) ) ;
#168395 = CARTESIAN_POINT ( 'NONE',  ( -3.242371291962510504, 6.934516940598226320, 1.040834085586084257E-14 ) ) ;
#168397 = CARTESIAN_POINT ( 'NONE',  ( 2.489988787850425656, -2.185901284972164405, -0.1580625509675498419 ) ) ;
#168398 = CARTESIAN_POINT ( 'NONE',  ( -5.798199202927275309, 6.683866596142988392, 0.9905280086691092833 ) ) ;
#168399 = CARTESIAN_POINT ( 'NONE',  ( 4.014622883422321209, 5.777089012116397804, -1.443375672974068769 ) ) ;
#168400 = CARTESIAN_POINT ( 'NONE',  ( 1.499999999999990896, 4.806250000682819490, 1.214306433183764966E-14 ) ) ;
#168401 = ADVANCED_FACE ( 'NONE', ( #166797 ), #133260, .T. ) ;
#168402 = CARTESIAN_POINT ( 'NONE',  ( -0.6823417656250039265, 13.63020833367473195, -1.181850606188755259 ) ) ;
#168403 = CARTESIAN_POINT ( 'NONE',  ( -5.468734858265826837, 7.473552982767158070, 1.599625672291263179 ) ) ;
#168404 = CARTESIAN_POINT ( 'NONE',  ( 6.434187037261335007, -1.398866626055271123, -1.024706079042293938 ) ) ;
#168405 = CARTESIAN_POINT ( 'NONE',  ( -4.386226389220933441, 5.076017861301227008, -1.199719254218446718 ) ) ;
#168406 = CARTESIAN_POINT ( 'NONE',  ( 3.432542862244458703, -1.236986750340131946, 1.659893174209552624 ) ) ;
#168407 = CARTESIAN_POINT ( 'NONE',  ( 4.200857891667449273, 1.936436120981197773, 0.8564517604346032487 ) ) ;
#168408 = CARTESIAN_POINT ( 'NONE',  ( 5.880485940025228508, 7.883652901494672349, 1.599625672291267398 ) ) ;
#168409 = CARTESIAN_POINT ( 'NONE',  ( -1.201851678989727383E-14, 5.196875000341421469, -1.575800808251660134 ) ) ;
#168410 = CARTESIAN_POINT ( 'NONE',  ( 3.186336211243359084, 1.097972430180796266, -1.634763817068272784 ) ) ;
#168411 = CARTESIAN_POINT ( 'NONE',  ( 0.5801457039020865292, 0.9447208859736742070, 1.662703529197881558 ) ) ;
#168412 = CARTESIAN_POINT ( 'NONE',  ( 4.857543142518937707, 2.267833309424868826, -0.3330599157496324514 ) ) ;
#168413 = CARTESIAN_POINT ( 'NONE',  ( 2.912524513316586461, 1.322148455168963510, -1.259233298254287536 ) ) ;
#168414 = CARTESIAN_POINT ( 'NONE',  ( 7.024532985656128936, 9.288650798055913427, 1.443375672974065660 ) ) ;
#168415 = CARTESIAN_POINT ( 'NONE',  ( 6.114364089638795186, 7.196141528409145671, 1.082531754730558626 ) ) ;
#168416 = CARTESIAN_POINT ( 'NONE',  ( -5.194745412330402878, 9.212286747694129474, 0.000000000000000000 ) ) ;
#168417 = CARTESIAN_POINT ( 'NONE',  ( 4.008068315354725186, -0.7665524943986418149, 1.861746286504823988 ) ) ;
#168418 = CARTESIAN_POINT ( 'NONE',  ( 4.838696733575553743, -1.901848327180942766, -0.4805237247276354928 ) ) ;
#168419 = CARTESIAN_POINT ( 'NONE',  ( -7.100719765255177229, 9.307259030929609267, -1.599625672291263179 ) ) ;
#168420 = AXIS2_PLACEMENT_3D ( 'NONE', #45836, #109820, #60998 ) ;
#168421 = CARTESIAN_POINT ( 'NONE',  ( -5.870844209917351009, 6.808071985447069707, -1.199719254218446718 ) ) ;
#168422 = CARTESIAN_POINT ( 'NONE',  ( 0.07556134207195497332, 5.719716873484223640, -2.838244455430352087 ) ) ;
#168424 = CARTESIAN_POINT ( 'NONE',  ( 5.576936095668227900, -0.04655786065462656775, -1.769397458738901197 ) ) ;
#168423 = CARTESIAN_POINT ( 'NONE',  ( 6.720655732516684466, -0.001531948155393536137, 2.073773125298985054 ) ) ;
#168425 = CARTESIAN_POINT ( 'NONE',  ( 6.589320575229280053, 7.629137130509070275, 2.496737603865983868 ) ) ;
#168426 = CARTESIAN_POINT ( 'NONE',  ( 1.974822964535282610, -0.1094934731284517848, -2.188836591978132518 ) ) ;
#168427 = CARTESIAN_POINT ( 'NONE',  ( -0.02444708455723310775, -1.687298116421297456, -0.4264520246781302593 ) ) ;
#168428 = CARTESIAN_POINT ( 'NONE',  ( 5.913327553854682783, 10.05063257947248800, -0.7998128361456291469 ) ) ;
#168429 = CARTESIAN_POINT ( 'NONE',  ( 0.1335669894368890498, 2.867242032283002562, -2.641834823421157719 ) ) ;
#168430 = CARTESIAN_POINT ( 'NONE',  ( 1.084105852307458040, -1.681943224540465964, -0.3816912691657590728 ) ) ;
#168431 = CARTESIAN_POINT ( 'NONE',  ( 0.4744793627779358980, 2.001106834215804042, 1.130494720166761891 ) ) ;
#168432 = CARTESIAN_POINT ( 'NONE',  ( 0.1346727191937693857, 0.3808678606769915209, 2.158067550307264604 ) ) ;
#168433 = CARTESIAN_POINT ( 'NONE',  ( 3.422699507934781060, 1.400174360247144589, -1.705827624971032686 ) ) ;
#168434 = CARTESIAN_POINT ( 'NONE',  ( 0.5323791783840629011, 1.248846938226945369, 1.775765033185220387 ) ) ;
#168435 = CARTESIAN_POINT ( 'NONE',  ( 11.84668730067608244, 10.19999999999998153, 1.319999999999998286 ) ) ;
#168436 = CARTESIAN_POINT ( 'NONE',  ( 0.9896463964080002285, -0.5083134511523321741, 2.055333615346987663 ) ) ;
#168437 = CARTESIAN_POINT ( 'NONE',  ( 6.781144757626056396, -7.161464053357567749, -6.776370306708062508 ) ) ;
#168438 = CARTESIAN_POINT ( 'NONE',  ( 5.737312389570451643, -1.741366515823379757, 0.8240431586447917178 ) ) ;
#168439 = ORIENTED_EDGE ( 'NONE', *, *, #171367, .T. ) ;
#168441 = CARTESIAN_POINT ( 'NONE',  ( 1.499999999999989120, 5.504166666666685970, 0.8660254037844524744 ) ) ;
#168440 = CARTESIAN_POINT ( 'NONE',  ( 1.154322298621703435, 0.9348496236407450866, 2.093279060508267175 ) ) ;
#168442 = CARTESIAN_POINT ( 'NONE',  ( 4.871457266011829823, 4.577788319968905562, -0.7998128361456221525 ) ) ;
#168443 = CARTESIAN_POINT ( 'NONE',  ( 4.794779880727245036, 8.745660294157122649, -0.7998128361456281477 ) ) ;
#168444 = CARTESIAN_POINT ( 'NONE',  ( 3.668779877082572138, 0.8004024921177651519, 2.072244876181651652 ) ) ;
#168445 = CARTESIAN_POINT ( 'NONE',  ( -8.690413276679693766, 9.241163032322203819, 1.040834085586084257E-14 ) ) ;
#168446 = CARTESIAN_POINT ( 'NONE',  ( 0.5773502691896192918, -2.500000000000002220, 1.000000000000004441 ) ) ;
#168447 = CARTESIAN_POINT ( 'NONE',  ( 5.422898255786183341, 7.349800603215774331, -1.443375672974051449 ) ) ;
#168448 = CARTESIAN_POINT ( 'NONE',  ( -7.334597914868722590, 11.50085530074811935, -0.7216878364870267237 ) ) ;
#168449 = CARTESIAN_POINT ( 'NONE',  ( 5.180624094197585627, 8.097792972322238825, -1.082531754730548412 ) ) ;
#168450 = CARTESIAN_POINT ( 'NONE',  ( 1.652970434142877920, 1.038994816082598804, 1.728001345923817267 ) ) ;
#168452 = CARTESIAN_POINT ( 'NONE',  ( 0.9188877648007650611, -1.496628706349166338, 1.419512306474308261 ) ) ;
#168451 = CARTESIAN_POINT ( 'NONE',  ( 7.670162217029129259, 9.971608557999250166, 1.599625672291281386 ) ) ;
#168453 = CARTESIAN_POINT ( 'NONE',  ( -1.772826578343109416, 3.949999999999995293, -0.4000000000000270561 ) ) ;
#168454 = CARTESIAN_POINT ( 'NONE',  ( 4.841670253411575864, 8.662716039039905169, -0.7216878364870458196 ) ) ;
#168455 = CARTESIAN_POINT ( 'NONE',  ( 0.1867156058280826092, 1.363667594142993877, 1.237386390646778578 ) ) ;
#168456 = CARTESIAN_POINT ( 'NONE',  ( 10.79920600060117586, -6.027819618361855092, 9.269928574751062911E-15 ) ) ;
#168457 = CARTESIAN_POINT ( 'NONE',  ( 1.364683531249990311, 4.134375000341417028, 1.214306433183764966E-14 ) ) ;
#168458 = CARTESIAN_POINT ( 'NONE',  ( 1.776017750421728270, 1.753029812786778940, -0.9963028777105964462 ) ) ;
#168459 = CARTESIAN_POINT ( 'NONE',  ( -0.09456490281532430042, -0.7861721075429689565, -1.663503389917226460 ) ) ;
#168460 = CARTESIAN_POINT ( 'NONE',  ( 5.495737418514557326, -2.292545469083116849, -0.002927036808696506075 ) ) ;
#168461 = CARTESIAN_POINT ( 'NONE',  ( 3.644333108393753573, -1.504320797718930791, 1.061230752167609204 ) ) ;
#168462 = CARTESIAN_POINT ( 'NONE',  ( 7.801827329660018684, 11.18955008699033726, 1.199719254218460707 ) ) ;
#168463 = PRESENTATION_STYLE_ASSIGNMENT (( #2734 ) ) ;
#168464 = CARTESIAN_POINT ( 'NONE',  ( 4.453998568579462969, 1.825179399820752169, -0.04523609120457571658 ) ) ;
#168465 = CARTESIAN_POINT ( 'NONE',  ( 4.887342357109405455, -0.6819942819097268849, -1.897698409216505233 ) ) ;
#168466 = CARTESIAN_POINT ( 'NONE',  ( -9.179033691651859783, 10.66762638080401260, 1.199719254218462483 ) ) ;
#168468 = CARTESIAN_POINT ( 'NONE',  ( -5.921879234118920365, 10.13088588310589699, 0.000000000000000000 ) ) ;
#168467 = CARTESIAN_POINT ( 'NONE',  ( 3.872163259867720253, 1.254437384476282835, 1.882731698358128369 ) ) ;
#168469 = CARTESIAN_POINT ( 'NONE',  ( 6.088920695360399371, -0.3053041885118645271, -2.083579958893892137 ) ) ;
#168470 = CARTESIAN_POINT ( 'NONE',  ( -6.050681693448748177, 10.28115541899069463, 0.7998128361456291469 ) ) ;
#168471 = CARTESIAN_POINT ( 'NONE',  ( 3.789561645344252661, -1.914057400617325433, 0.7896510022299551013 ) ) ;
#168472 = CARTESIAN_POINT ( 'NONE',  ( 3.029357257649615054, 5.621668336311468117, -1.199719254218446718 ) ) ;
#168473 = CARTESIAN_POINT ( 'NONE',  ( -1.360316468750021768, 1.421875000341424222, -4.510281037539698445E-14 ) ) ;
#168474 = APPLICATION_PROTOCOL_DEFINITION ( 'draft international standard', 'automotive_design', 1998, #181919 ) ;
#168476 = CARTESIAN_POINT ( 'NONE',  ( 2.279798536657418495, 1.185040197188882871, 1.518827336823719953 ) ) ;
#168475 = CARTESIAN_POINT ( 'NONE',  ( -9.504429378379839477, 11.04725468198666150, 1.199719254218462483 ) ) ;
#168477 = UNCERTAINTY_MEASURE_WITH_UNIT (LENGTH_MEASURE( 1.000000000000000082E-05 ), #97201, 'distance_accuracy_value', 'NONE');
#168478 = CARTESIAN_POINT ( 'NONE',  ( -10.56513397747884397, 11.25900096514340198, 3.405015282931166620 ) ) ;
#168479 = CARTESIAN_POINT ( 'NONE',  ( 0.5023235590321275534, 1.964037083787707028, 0.1483792944171925254 ) ) ;
#168480 = CARTESIAN_POINT ( 'NONE',  ( 5.546694241322223107, 5.643767167730274537, -0.7216878364870458196 ) ) ;
#168481 = CARTESIAN_POINT ( 'NONE',  ( 5.863316726098953602, 5.994608360591326068, -0.2888550730815123702 ) ) ;
#168482 = CARTESIAN_POINT ( 'NONE',  ( -0.4019237886466871523, 10.97991455036742359, -1.499999999999998668 ) ) ;
#168483 = CARTESIAN_POINT ( 'NONE',  ( -3.144601563365788444, 5.756120026313656268, -1.199719254218452935 ) ) ;
#168484 = CARTESIAN_POINT ( 'NONE',  ( 1.600152846412273844, 1.536270192620782238, 1.604750372702767214 ) ) ;
#168485 = CARTESIAN_POINT ( 'NONE',  ( 3.821394775679032740, -0.1568257194812898159, 2.100186923160925812 ) ) ;
#168486 = CARTESIAN_POINT ( 'NONE',  ( -7.208094944320834863, 8.438474185576302133, -1.199719254218452047 ) ) ;
#168487 = CARTESIAN_POINT ( 'NONE',  ( 7.396136491454752715, 8.587579647240744407, 1.199719254218462483 ) ) ;
#168488 = CARTESIAN_POINT ( 'NONE',  ( 0.5724163261710726314, 1.287614217418028506, -1.343956351914729952 ) ) ;
#168489 = CARTESIAN_POINT ( 'NONE',  ( 5.666418135507635512, 8.698239360479199433, 1.199719254218462483 ) ) ;
#168490 = CARTESIAN_POINT ( 'NONE',  ( 5.009901455449552010, 5.803638771901306725, -1.199719254218452047 ) ) ;
#168491 = CARTESIAN_POINT ( 'NONE',  ( -5.139949633356594383, 9.010708648975750634, 0.000000000000000000 ) ) ;
#168493 = CARTESIAN_POINT ( 'NONE',  ( -7.049876689426097798, 11.16868053773170821, -0.7216878364870267237 ) ) ;
#168492 = CIRCLE ( 'NONE', #33658, 0.08000000000000025147 ) ;
#168494 = CARTESIAN_POINT ( 'NONE',  ( 1.687894460584405731, 2.027760172737497424, -0.6205009303206151516 ) ) ;
#168495 = CARTESIAN_POINT ( 'NONE',  ( -6.505933609711270549, 8.683618192786854095, -1.599625672291271394 ) ) ;
#168497 = CARTESIAN_POINT ( 'NONE',  ( 4.457442142980160504, 1.574409630067734156, 1.170308293268598421 ) ) ;
#168496 = CARTESIAN_POINT ( 'NONE',  ( 1.224999999999979661, 0.6249999999999866773, -2.775557561562891351E-14 ) ) ;
#168498 = CARTESIAN_POINT ( 'NONE',  ( 2.940462584922590938, 2.145230175562794717, 0.2658940370997217584 ) ) ;
#168499 = CARTESIAN_POINT ( 'NONE',  ( 2.014959344526063845, -1.785600367564584179, 0.4486904387498573676 ) ) ;
#168500 = CARTESIAN_POINT ( 'NONE',  ( -4.245996903372413200, 7.323364108789364835, -0.8915694317389293300 ) ) ;
#168501 = CARTESIAN_POINT ( 'NONE',  ( 4.241972025877470465, 0.4673694910880517583, 1.676319072879989047 ) ) ;
#168502 = CARTESIAN_POINT ( 'NONE',  ( -8.752560982292409975, 14.99999996918461775, -9.356054898121708874 ) ) ;
#168503 = CARTESIAN_POINT ( 'NONE',  ( 4.175548123328908900, 7.815297210618305179, -0.7216878364870197293 ) ) ;
#168504 = CARTESIAN_POINT ( 'NONE',  ( -11.40891844150367618, 9.366729182080655747, 1.257950088934312705 ) ) ;
#168505 = CIRCLE ( 'NONE', #102800, 0.07999999999999986289 ) ;
#168506 = CARTESIAN_POINT ( 'NONE',  ( 1.411231610350563992, 1.906656261001705488, 1.018656936289302539 ) ) ;
#168507 = CARTESIAN_POINT ( 'NONE',  ( 3.585314394424500062, 1.281165535658060017, -1.556669873624405120 ) ) ;
#168508 = DIRECTION ( 'NONE',  ( 3.706092522800016599E-15, 0.000000000000000000, 1.000000000000000000 ) ) ;
#168509 = CARTESIAN_POINT ( 'NONE',  ( 0.7433210806352362754, -1.853469564684958382, 1.112228649290482263 ) ) ;
#168510 = CARTESIAN_POINT ( 'NONE',  ( 3.854335392261270421, 0.7083531993744094368, 1.839989435513892380 ) ) ;
#168511 = CARTESIAN_POINT ( 'NONE',  ( 6.609000000000053276, 0.5717736360873815205, 2.152148306911850995 ) ) ;
#168512 = CARTESIAN_POINT ( 'NONE',  ( 2.946749062660087848, -1.589232290113586910, -1.115973732403415131 ) ) ;
#168515 = VERTEX_POINT ( 'NONE', #199267 ) ;
#168514 = CARTESIAN_POINT ( 'NONE',  ( -4.665414256878304577, 5.575976400180357118, -1.082531754730549967 ) ) ;
#168513 = CARTESIAN_POINT ( 'NONE',  ( 3.179715765502657554, 5.975770656120749535, -2.420000000000002149 ) ) ;
#168516 = STYLED_ITEM ( 'NONE', ( #42 ), #145158 ) ;
#168517 = CARTESIAN_POINT ( 'NONE',  ( -5.438229012412911345, 5.517224400669388018, -0.7216878364870338292 ) ) ;
#168518 = CARTESIAN_POINT ( 'NONE',  ( -0.1110810684433141682, 4.095429159110416606, -2.351882046268341409 ) ) ;
#168519 = CARTESIAN_POINT ( 'NONE',  ( 5.574337433874081427, 6.532423756721743580, -1.199719254218452047 ) ) ;
#168520 = CARTESIAN_POINT ( 'NONE',  ( -4.118644803501354978, 8.027112380718707030, 0.7998128361456352531 ) ) ;
#168522 = ORIENTED_EDGE ( 'NONE', *, *, #132650, .F. ) ;
#168521 = CARTESIAN_POINT ( 'NONE',  ( -6.770317605177755382, 8.992066187497757213, 1.599625672291269396 ) ) ;
#168523 = CARTESIAN_POINT ( 'NONE',  ( -8.717529583462656717, 11.19353715217169309, 1.443375672974064550 ) ) ;
#168524 = CARTESIAN_POINT ( 'NONE',  ( 0.4115098346569624477, 1.921242953230850148, 1.085561749797583797 ) ) ;
#168525 = CARTESIAN_POINT ( 'NONE',  ( 2.520460663003311730, -4.091624451297095177, -2.338645729556988240 ) ) ;
#168526 = CARTESIAN_POINT ( 'NONE',  ( 3.783995958019512607, -1.164969938643352299, -1.578273546942794647 ) ) ;
#168527 = CARTESIAN_POINT ( 'NONE',  ( 7.934546212495622086, 10.28005655271014795, -1.599625672291262513 ) ) ;
#168528 = CARTESIAN_POINT ( 'NONE',  ( 1.231092510272915552, 2.014232830173094513, 0.09613330637052441840 ) ) ;
#168529 = ORIENTED_EDGE ( 'NONE', *, *, #2174, .F. ) ;
#168530 = CARTESIAN_POINT ( 'NONE',  ( 3.081382859721363499, 1.672078201027054734, 1.298909159995583318 ) ) ;
#168531 = CARTESIAN_POINT ( 'NONE',  ( -0.7500000000000215383, 1.222916667349485564, 1.299038105676659116 ) ) ;
#168533 = CARTESIAN_POINT ( 'NONE',  ( -4.205000198532790279, 8.057583998263570635, 0.7998128361456341429 ) ) ;
#168532 = CARTESIAN_POINT ( 'NONE',  ( -10.10343170205533880, 2.974000657017113802, 5.833219012925197511 ) ) ;
#168534 = CARTESIAN_POINT ( 'NONE',  ( 2.695044507329581673, -0.5773736025265225891, 1.748335772842606106 ) ) ;
#168535 = ORIENTED_EDGE ( 'NONE', *, *, #68949, .F. ) ;
#168536 = CARTESIAN_POINT ( 'NONE',  ( -7.296259222448620463, 11.66405285949874759, 0.7998128361456481317 ) ) ;
#168537 = CARTESIAN_POINT ( 'NONE',  ( -3.294268138440636928, 6.787137228248626641, 1.040834085586084257E-14 ) ) ;
#168539 = ADVANCED_FACE ( 'NONE', ( #117039 ), #190462, .T. ) ;
#168538 = CARTESIAN_POINT ( 'NONE',  ( 4.430007776716601953, -2.079114408633813582, 0.4165480963118637914 ) ) ;
#168540 = CARTESIAN_POINT ( 'NONE',  ( -10.30245174296178057, 3.603753425775780617, -5.948123287112075275 ) ) ;
#168541 = CARTESIAN_POINT ( 'NONE',  ( 7.800018446563675489, 7.994443030612759848, -0.7998128361456281477 ) ) ;
#168542 = CARTESIAN_POINT ( 'NONE',  ( 5.975869988448771153, 1.224042345451004765, 1.657734310933855815 ) ) ;
#168544 = CARTESIAN_POINT ( 'NONE',  ( 2.700538275128167687, 1.556679782967337999, 0.9830204120172959525 ) ) ;
#168543 = CARTESIAN_POINT ( 'NONE',  ( -5.876569516519495551, 8.943415971659659292, 1.199719254218452047 ) ) ;
#168545 = CARTESIAN_POINT ( 'NONE',  ( 9.908311333488716954, 10.45411806535867782, 0.7998128361456462443 ) ) ;
#168546 = DIRECTION ( 'NONE',  ( -0.9366510587354612838, 1.084202172485500963E-14, -0.3502638921866474409 ) ) ;
#168547 = DIRECTION ( 'NONE',  ( -0.000000000000000000, 1.000000000000000000, -0.000000000000000000 ) ) ;
#168548 = FILL_AREA_STYLE_COLOUR ( '', #77116 ) ;
#168549 = CARTESIAN_POINT ( 'NONE',  ( 2.702037527177497012, -0.6914408288211832954, 2.095836555436859872 ) ) ;
#168550 = CARTESIAN_POINT ( 'NONE',  ( 4.974029133664690683, 1.296991790296280422, 1.853570637303619817 ) ) ;
#168551 = CARTESIAN_POINT ( 'NONE',  ( -6.832946231607472498, 9.955225789308602913, 1.082531754730549967 ) ) ;
#168552 = CARTESIAN_POINT ( 'NONE',  ( 4.675916410682629198, 1.790815896176844335, -0.2727875059450618478 ) ) ;
#168553 = CARTESIAN_POINT ( 'NONE',  ( 4.575340585108073732, 1.423666108326137048, 1.282088096497513652 ) ) ;
#168554 = CARTESIAN_POINT ( 'NONE',  ( 0.6823417656249917140, 4.655208333674755394, 1.181850606188765695 ) ) ;
#168555 = CARTESIAN_POINT ( 'NONE',  ( 4.135589226209329006, -1.358636868218986216, -1.428786634662780219 ) ) ;
#168556 = CARTESIAN_POINT ( 'NONE',  ( 5.401189721097995111, 1.529905263132097071, 1.076157610686766075 ) ) ;
#168557 = CARTESIAN_POINT ( 'NONE',  ( 5.178104514100493994, -0.9952990805809349695, -1.572330789729664779 ) ) ;
#168558 = CARTESIAN_POINT ( 'NONE',  ( -1.364683531250010295, 5.280208333674758059, 0.7879004041258379498 ) ) ;
#168559 = CARTESIAN_POINT ( 'NONE',  ( -0.1179535434602772825, -2.016182236903838465, -0.04464881524945257807 ) ) ;
#168561 = CARTESIAN_POINT ( 'NONE',  ( 2.280028682641733973, 1.296546612978483504, 1.659573824544317455 ) ) ;
#168560 = CARTESIAN_POINT ( 'NONE',  ( -2.589244150085650009, 5.964609241834465614, 0.7216878364870317197 ) ) ;
#168562 = CARTESIAN_POINT ( 'NONE',  ( 4.175548122884573665, 3.973820352894515295, 1.214306433183764966E-14 ) ) ;
#168564 = CARTESIAN_POINT ( 'NONE',  ( 0.07479286986305544449, 6.948552162806721277, -2.450557996216149892 ) ) ;
#168563 = CARTESIAN_POINT ( 'NONE',  ( -1.001543065824772872E-14, 5.384375000341415252, 1.575800808251672791 ) ) ;
#168565 = CARTESIAN_POINT ( 'NONE',  ( -9.616417370072172233, -9.251786168353179463, 0.2979722244324810032 ) ) ;
#168566 = CARTESIAN_POINT ( 'NONE',  ( 2.426041109754235592, -1.997208190617974166, 0.3004318525065238776 ) ) ;
#168567 = CARTESIAN_POINT ( 'NONE',  ( -1.364683531250000748, 1.509375000341421691, 0.000000000000000000 ) ) ;
#168568 = CARTESIAN_POINT ( 'NONE',  ( -4.473827502829599290, 4.321812962830357208, 0.7216878364870317197 ) ) ;
#168569 = CARTESIAN_POINT ( 'NONE',  ( 2.998324526916512411, 6.649795714711241423, 0.000000000000000000 ) ) ;
#168570 = VERTEX_POINT ( 'NONE', #212325 ) ;
#168571 = CARTESIAN_POINT ( 'NONE',  ( 2.267066545249882381, -1.975312647937790711, -0.8782872871702240847 ) ) ;
#168572 = CARTESIAN_POINT ( 'NONE',  ( -0.3282377607281391496, 0.05133545031538289116, 1.224999999999979217 ) ) ;
#168574 = FACE_OUTER_BOUND ( 'NONE', #192639, .T. ) ;
#168573 = CARTESIAN_POINT ( 'NONE',  ( 5.086243903782109221, 5.962981304947771122, -1.199719254218452047 ) ) ;
#168575 = DIRECTION ( 'NONE',  ( 1.000000000000000000, 0.000000000000000000, 0.000000000000000000 ) ) ;
#168576 = CARTESIAN_POINT ( 'NONE',  ( -7.927630635717298979, -6.615717645446903994, 7.626802973668175056 ) ) ;
#168577 = CARTESIAN_POINT ( 'NONE',  ( -7.212574532790092974, 10.39812547402169862, -1.082531754730543971 ) ) ;
#168578 = AXIS2_PLACEMENT_3D ( 'NONE', #44394, #81145, #77940 ) ;
#168579 = CARTESIAN_POINT ( 'NONE',  ( 0.2401087780563165297, 2.186128513634697512, 0.1550312349237955856 ) ) ;
#168580 = CARTESIAN_POINT ( 'NONE',  ( -10.95855051086948606, -7.723431457505092190, 0.6286713519884027379 ) ) ;
#168582 = CARTESIAN_POINT ( 'NONE',  ( 0.6823417656249969321, 11.77604166700806054, -1.181850606188757036 ) ) ;
#168581 = CARTESIAN_POINT ( 'NONE',  ( 1.077466299836680630, -0.05792418700063763082, -2.261926406141855583 ) ) ;
#168583 = CARTESIAN_POINT ( 'NONE',  ( -9.267161690140662600, 10.77044237904097734, -1.199719254218441611 ) ) ;
#168584 = CARTESIAN_POINT ( 'NONE',  ( -4.324687812634898876, 6.068555086205916105, 1.443375672974064550 ) ) ;
#168585 = CARTESIAN_POINT ( 'NONE',  ( 0.6823417656249899377, 1.905208333674752952, 1.181850606188755259 ) ) ;
#168586 = CARTESIAN_POINT ( 'NONE',  ( 4.700249516990034238, 8.244041944096728969, -0.6212051699984559860 ) ) ;
#168587 = CARTESIAN_POINT ( 'NONE',  ( 1.500000000000001332, 9.875000000000001776, 0.000000000000000000 ) ) ;
#168588 = CARTESIAN_POINT ( 'NONE',  ( 3.492533829797561218, -0.3379890457658150105, -1.691244694301207829 ) ) ;
#168589 = CARTESIAN_POINT ( 'NONE',  ( 5.065906673361608270, 5.939254536123854677, -1.199719254218450271 ) ) ;
#168590 = CARTESIAN_POINT ( 'NONE',  ( 2.600565598370237819, 1.424089007750706237, -1.050482986540713926 ) ) ;
#168591 = CARTESIAN_POINT ( 'NONE',  ( 2.754543805099545217, 1.998131736582898332, 0.2443565819899694291 ) ) ;
#168592 = CARTESIAN_POINT ( 'NONE',  ( 9.103410076571945453, 12.70806329172093818, 1.199719254218450271 ) ) ;
#168593 = CARTESIAN_POINT ( 'NONE',  ( 5.104599427727727345, -0.7392731805347593221, -2.079399364341961487 ) ) ;
#168594 = ORIENTED_EDGE ( 'NONE', *, *, #75095, .F. ) ;
#168595 = CARTESIAN_POINT ( 'NONE',  ( 4.377216478116826792, -1.806098078589046807, -0.9042721688041258643 ) ) ;
#168596 = CARTESIAN_POINT ( 'NONE',  ( -7.435720902452096936, 7.639705572474380091, 0.000000000000000000 ) ) ;
#168597 = CARTESIAN_POINT ( 'NONE',  ( 4.552361342037492875, -1.314984614574012944, 1.528753174698034067 ) ) ;
#168599 = EDGE_LOOP ( 'NONE', ( #131674, #17439, #159188, #170112, #147694 ) ) ;
#168598 = CARTESIAN_POINT ( 'NONE',  ( 4.746265919983247983, 0.9249516081627707775, -1.557494045171695651 ) ) ;
#168600 = ORIENTED_EDGE ( 'NONE', *, *, #200299, .T. ) ;
#168601 = CARTESIAN_POINT ( 'NONE',  ( 2.430351462470367707, 1.813921419787648315, 0.4566771774890953095 ) ) ;
#168602 = CARTESIAN_POINT ( 'NONE',  ( -10.41509302999113018, 1.813436143228244424, 5.960384690635835092 ) ) ;
#168603 = CARTESIAN_POINT ( 'NONE',  ( 1.845825534506392085, -1.251752223804462272, -1.445855903880132631 ) ) ;
#168604 = CARTESIAN_POINT ( 'NONE',  ( 0.7500000000000006661, 9.583333333333332149, 1.299038105676657340 ) ) ;
#168605 = CIRCLE ( 'NONE', #130657, 0.08000000000000020983 ) ;
#168606 = CARTESIAN_POINT ( 'NONE',  ( -10.21576913194658864, 4.000029896383376027, -7.512182378973799146 ) ) ;
#168607 = CARTESIAN_POINT ( 'NONE',  ( -1.201851678989727383E-14, 3.509375000341421469, -1.575800808251660134 ) ) ;
#168608 = CARTESIAN_POINT ( 'NONE',  ( 0.3516297456669579269, -1.353986107606550249, -1.350798769753497552 ) ) ;
#168609 = CARTESIAN_POINT ( 'NONE',  ( 4.855228407469603269, 7.718164671139588151, -1.082531754730548412 ) ) ;
#168610 = CARTESIAN_POINT ( 'NONE',  ( 2.066782613880484565, 1.455849762852476248, -1.315278764014264912 ) ) ;
#168611 = CARTESIAN_POINT ( 'NONE',  ( -7.334597915313094241, 9.580116872663850813, 1.040834085586084257E-14 ) ) ;
#168612 = CARTESIAN_POINT ( 'NONE',  ( -4.762657100150483380, 8.778460060142702304, 0.000000000000000000 ) ) ;
#168613 = CARTESIAN_POINT ( 'NONE',  ( 3.744478000529618100, 1.131475959888720295, -1.793321066073015224 ) ) ;
#168615 = PLANE ( 'NONE',  #109066 ) ;
#168614 = CARTESIAN_POINT ( 'NONE',  ( 7.723341061279088038, 12.16231500480096983, -0.7998128361456291469 ) ) ;
#168616 = CARTESIAN_POINT ( 'NONE',  ( 5.536387714897482049, 1.941722972556509053, 0.3397322875919612795 ) ) ;
#168617 = CARTESIAN_POINT ( 'NONE',  ( -1.364683531250014514, 0.9885416670080898749, -0.7879004041258289570 ) ) ;
#168618 = CARTESIAN_POINT ( 'NONE',  ( 1.125244999914726263, 1.777361856972861531, 0.9454465733411165917 ) ) ;
#168619 = ORIENTED_EDGE ( 'NONE', *, *, #42815, .T. ) ;
#168620 = CARTESIAN_POINT ( 'NONE',  ( 1.564221677423253798, -1.129412574612179920, 1.790659096458546706 ) ) ;
#168621 = CARTESIAN_POINT ( 'NONE',  ( 11.96769518616268080, 6.617733873879387829, 1.006560610218020679 ) ) ;
#168622 = CARTESIAN_POINT ( 'NONE',  ( 2.400909748719297188, 0.4512941399696759337, 2.020426262116347349 ) ) ;
#168623 = CARTESIAN_POINT ( 'NONE',  ( 5.065906673361608270, 5.939254536123854677, -1.199719254218450271 ) ) ;
#168624 = CARTESIAN_POINT ( 'NONE',  ( 6.574778147984297938, 6.635272358928617997, -0.7998128361456481317 ) ) ;
#168625 = VERTEX_POINT ( 'NONE', #134327 ) ;
#168627 = CARTESIAN_POINT ( 'NONE',  ( 3.032219910950674890, 6.689340329417765574, 0.7998128361456321445 ) ) ;
#168626 = CARTESIAN_POINT ( 'NONE',  ( 4.839831225001551829, 2.085006553764104265, 0.1541250707555453237 ) ) ;
#168630 = ORIENTED_EDGE ( 'NONE', *, *, #126323, .T. ) ;
#168629 = CARTESIAN_POINT ( 'NONE',  ( 1.084272394670304118, -1.149816064065724230, 1.399778539804387822 ) ) ;
#168628 = CARTESIAN_POINT ( 'NONE',  ( 2.731258071184277103, -1.704167518380688140, 0.6551187846031493178 ) ) ;
#168631 = CARTESIAN_POINT ( 'NONE',  ( 6.533804136697315634, -1.437950210024591780, -1.674183229976949905 ) ) ;
#168632 =( NAMED_UNIT ( * ) PLANE_ANGLE_UNIT ( ) SI_UNIT ( $, .RADIAN. ) );
#168633 = CARTESIAN_POINT ( 'NONE',  ( 8.825993893598074180, 13.26473029764630773, -7.662602092427571954 ) ) ;
#168634 = CARTESIAN_POINT ( 'NONE',  ( 5.667066814448853407, -1.992748536412903615, -0.9483587796220711574 ) ) ;
#168635 = CARTESIAN_POINT ( 'NONE',  ( -1.364683531250000748, 9.921875000341398021, 0.000000000000000000 ) ) ;
#168636 = VERTEX_POINT ( 'NONE', #165729 ) ;
#168637 = CARTESIAN_POINT ( 'NONE',  ( 3.897043152223302886, -0.1904361752127527174, -1.902785305300330743 ) ) ;
#168639 = CARTESIAN_POINT ( 'NONE',  ( -3.704402285031864306, 5.344888637335695414, -1.599625672291256295 ) ) ;
#168638 = VECTOR ( 'NONE', #205853, 1000.000000000000000 ) ;
#168640 = CARTESIAN_POINT ( 'NONE',  ( 8.620286740190458374, 8.951422706510690830, 1.040834085586084257E-14 ) ) ;
#168641 = CARTESIAN_POINT ( 'NONE',  ( 6.777786256569462431, -2.009253640576996514, 0.4989836931604470505 ) ) ;
#168642 = CARTESIAN_POINT ( 'NONE',  ( 1.360316468749939833, 0.02604166700813021276, 0.7853790794158660438 ) ) ;
#168643 = CARTESIAN_POINT ( 'NONE',  ( 5.965224399888476192, 6.061776009399090448, 1.040834085586084257E-14 ) ) ;
#168644 = CARTESIAN_POINT ( 'NONE',  ( 6.550331612656306035, -1.695486744446069727, 1.388264742925699569 ) ) ;
#168645 = CARTESIAN_POINT ( 'NONE',  ( 6.142241479726070708, 7.081583759122534794, -1.089790755372788800 ) ) ;
#168646 = CIRCLE ( 'NONE', #19903, 11.92000000000000171 ) ;
#168647 = CARTESIAN_POINT ( 'NONE',  ( -3.475000000000000533, -2.100000000000000977, 0.000000000000000000 ) ) ;
#168648 = EDGE_CURVE ( 'NONE', #210028, #30243, #106586, .T. ) ;
#168649 = CARTESIAN_POINT ( 'NONE',  ( 3.180766902908559235, -0.1340872481324743570, -1.865776598943262199 ) ) ;
#168650 = CARTESIAN_POINT ( 'NONE',  ( -1.642778471875000035, -0.9552083328553742092, -2.845375778867859751 ) ) ;
#168651 = DIRECTION ( 'NONE',  ( -0.6507913734559640506, -0.7592566023653004592, 0.000000000000000000 ) ) ;
#168652 = CARTESIAN_POINT ( 'NONE',  ( -6.399085315970142851, 8.488685506763726352, -1.443375672974059665 ) ) ;
#168653 = CARTESIAN_POINT ( 'NONE',  ( 4.543917759235442944, 5.330267469643351852, 1.199719254218452935 ) ) ;
#168654 = CARTESIAN_POINT ( 'NONE',  ( 6.647575389402066826, 6.649926130590872120, 1.040834085586084257E-14 ) ) ;
#168655 = CARTESIAN_POINT ( 'NONE',  ( 6.508651864089095795, 0.6437109847576475419, 1.967739590238902991 ) ) ;
#168656 = CARTESIAN_POINT ( 'NONE',  ( 0.8961114988408731552, -0.9091644883451601711, -1.799914091915676639 ) ) ;
#168657 = CARTESIAN_POINT ( 'NONE',  ( -7.811469059767924605, 12.26513100303794168, -0.7998128361456281477 ) ) ;
#168658 = CARTESIAN_POINT ( 'NONE',  ( 6.261886844665240481, 8.398896966899865646, 1.599625672291268286 ) ) ;
#168659 = CIRCLE ( 'NONE', #75288, 0.07999999999999998779 ) ;
#168660 = CARTESIAN_POINT ( 'NONE',  ( 1.201424296212102893, -0.5295503721958020327, 2.126384922054704862 ) ) ;
#168661 = CARTESIAN_POINT ( 'NONE',  ( 6.375623774462673587, 1.745513195383348926, -0.5351242734627087438 ) ) ;
#168662 = CARTESIAN_POINT ( 'NONE',  ( -4.634189577772691138, 4.300976017023221409, 1.214306433183764966E-14 ) ) ;
#168663 = EDGE_CURVE ( 'NONE', #157709, #90486, #200809, .T. ) ;
#168664 = CARTESIAN_POINT ( 'NONE',  ( 4.746763178560250651, 7.591621904078704297, 1.082531754730549078 ) ) ;
#168665 = CARTESIAN_POINT ( 'NONE',  ( 10.57266086055835075, 11.22919251360659310, 0.000000000000000000 ) ) ;
#168666 = CARTESIAN_POINT ( 'NONE',  ( 4.379447312414087357, 5.068108938359919158, -1.199719254218452047 ) ) ;
#168667 = CARTESIAN_POINT ( 'NONE',  ( 8.014278199453778839, 8.522615118883788199, 0.000000000000000000 ) ) ;
#168668 = ORIENTED_EDGE ( 'NONE', *, *, #111248, .T. ) ;
#168670 = CARTESIAN_POINT ( 'NONE',  ( 0.4693897461072121802, -1.701762708260607715, -1.075143862628368474 ) ) ;
#168669 = CARTESIAN_POINT ( 'NONE',  ( 3.333393596924072444, 0.8250370302015205271, -1.646115572170883112 ) ) ;
#168671 = CARTESIAN_POINT ( 'NONE',  ( 1.810362406828632365, -1.941531176516932522, 1.229804462443480295 ) ) ;
#168673 = CARTESIAN_POINT ( 'NONE',  ( 0.9712807694385624524, -0.2802886605943204490, 1.839611564956656453 ) ) ;
#168672 = CARTESIAN_POINT ( 'NONE',  ( 2.738383840280320669, 6.138605547061593448, 0.7216878364870338292 ) ) ;
#168674 = CARTESIAN_POINT ( 'NONE',  ( -1.737500000000000266, -0.7583333333333330817, -3.009438278150923907 ) ) ;
#168675 = CARTESIAN_POINT ( 'NONE',  ( -5.253948220495577637, 6.088359997788290734, 1.199719254218450271 ) ) ;
#168676 = CARTESIAN_POINT ( 'NONE',  ( 0.000000000000000000, 2.817530495244580102, 1.214306433183764966E-14 ) ) ;
#168677 = CARTESIAN_POINT ( 'NONE',  ( 4.113462262696740979, 1.539102623358613586, 1.134910093507961237 ) ) ;
#168679 = CARTESIAN_POINT ( 'NONE',  ( -8.513630394377489807, 12.01998699582738972, -1.199719254218446718 ) ) ;
#168678 = B_SPLINE_CURVE_WITH_KNOTS ( 'NONE', 3,
 ( #211326, #129120, #97615, #209185, #195097, #112846, #14181, #212387, #15255, #196167, #126986, #160460, #108213, #25809, #172082, #8496, #27954, #206697, #205623, #10619, #209878, #126604, #192567, #76694, #109282, #91919 ),
 .UNSPECIFIED., .F., .F.,
 ( 4, 2, 1, 1, 1, 1, 2, 2, 2, 2, 2, 2, 2, 2, 4 ),
 ( 0.02490545872912452649, 0.02512859161056170063, 0.02535172449199887129, 0.02579799025487321956, 0.02669052178062191263, 0.02847558483211929531, 0.03204571093511406066, 0.03918596314110360523, 0.05346646755308270826, 0.06774697196506181129, 0.08202747637704091432, 0.09630798078902001735, 0.1105884852009991343, 0.1248689896129782373, 0.1391494940249573542 ),
 .UNSPECIFIED. ) ;
#168680 = CARTESIAN_POINT ( 'NONE',  ( 6.479309170914094196, 6.755949689298615723, 0.1985876171829506487 ) ) ;
#168681 = CARTESIAN_POINT ( 'NONE',  ( -5.953438850176548947, 9.959779401932374654, 0.000000000000000000 ) ) ;
#168683 = CARTESIAN_POINT ( 'NONE',  ( 2.711613914024712191, -1.850561042518297672, 0.2725550856255419818 ) ) ;
#168682 = CARTESIAN_POINT ( 'NONE',  ( 4.282818888323718376, 1.866831796845986435, -0.9415434926851961039 ) ) ;
#168684 = CARTESIAN_POINT ( 'NONE',  ( 8.161645285746708112, 9.584636257201740506, -1.082531754730543083 ) ) ;
#168685 = CARTESIAN_POINT ( 'NONE',  ( 3.188928480291308265, 8.980740528189235405, 2.451733079074510879 ) ) ;
#168686 = CARTESIAN_POINT ( 'NONE',  ( 2.876183954794831354, -0.1304463317927692101, -1.735623171917876073 ) ) ;
#168687 = CARTESIAN_POINT ( 'NONE',  ( 3.486418057008484617, 7.219238166485217434, 1.040834085586084257E-14 ) ) ;
#168689 = FACE_OUTER_BOUND ( 'NONE', #57825, .T. ) ;
#168688 = DIRECTION ( 'NONE',  ( -0.1510067114093955887, 0.000000000000000000, 0.9885327375000383388 ) ) ;
#168690 = CARTESIAN_POINT ( 'NONE',  ( 4.441862337843591746, 0.7341043403586414717, -1.561010781705338912 ) ) ;
#168691 = CARTESIAN_POINT ( 'NONE',  ( 4.001666433686186686, -2.185622478633037602, 0.1623105178310546570 ) ) ;
#168692 = CARTESIAN_POINT ( 'NONE',  ( 6.551417122825020201, -1.769646310455678995, -1.318412661681533260 ) ) ;
#168693 = CARTESIAN_POINT ( 'NONE',  ( -1.115562610750309283E-14, 8.562500000000000000, 1.500000000000001554 ) ) ;
#168694 = CARTESIAN_POINT ( 'NONE',  ( 3.397511025282150321, -1.916906860828609727, 1.019255427985159779 ) ) ;
#168695 = CARTESIAN_POINT ( 'NONE',  ( 2.631258204695927194, -1.703542010001803275, 0.6570300758180421807 ) ) ;
#168696 = CARTESIAN_POINT ( 'NONE',  ( 0.3562053913853078790, -1.961198556353323186, -0.05404869553313899899 ) ) ;
#168697 = CARTESIAN_POINT ( 'NONE',  ( 4.856716432673345629, -1.994826133969303195, -0.7102248925668596113 ) ) ;
#168698 = EDGE_CURVE ( 'NONE', #55454, #193812, #82288, .T. ) ;
#168699 = ORIENTED_EDGE ( 'NONE', *, *, #36264, .T. ) ;
#168701 = CARTESIAN_POINT ( 'NONE',  ( -1.201851678989727383E-14, 3.134375000341420137, 1.575800808251672791 ) ) ;
#168700 = CARTESIAN_POINT ( 'NONE',  ( 5.073898020828643496, -1.275178753180395530, 1.904781575909524349 ) ) ;
#168702 = CARTESIAN_POINT ( 'NONE',  ( 6.720655732516650716, 2.975630972093906923, 2.379814465338329743 ) ) ;
#168703 = CARTESIAN_POINT ( 'NONE',  ( 10.56588178375152864, 11.22128359066528169, -0.7998128361456281477 ) ) ;
#168704 = CARTESIAN_POINT ( 'NONE',  ( 0.4695848928168535608, -1.793611485386744420, -1.130822890709509254 ) ) ;
#168705 = CARTESIAN_POINT ( 'NONE',  ( -3.768803514918943609, 7.340761834139994058, 0.7216878364870317197 ) ) ;
#168706 = FACE_OUTER_BOUND ( 'NONE', #197957, .T. ) ;
#168707 = CARTESIAN_POINT ( 'NONE',  ( -4.541618270453545492, 8.242379048930368768, 0.7216878364870458196 ) ) ;
#168708 =( BOUNDED_CURVE ( )  B_SPLINE_CURVE ( 2, ( #4283, #71424, #69289, #35744, #34678, #21594, #120277, #88784, #171076 ),
 .UNSPECIFIED., .F., .T. ) 
 B_SPLINE_CURVE_WITH_KNOTS ( ( 3, 2, 2, 2, 3 ),
 ( 0.2031250000000002220, 0.2083333333333333426, 0.2187500000000000000, 0.2291666666666666574, 0.2343749999999998057 ),
 .UNSPECIFIED. ) 
 CURVE ( )  GEOMETRIC_REPRESENTATION_ITEM ( )  RATIONAL_B_SPLINE_CURVE ( ( 0.9330127018922194093, 0.9330127018922221849, 1.000000000000000000, 0.8660254037844387076, 1.000000000000000000, 0.8660254037844387076, 1.000000000000000000, 0.9330127018922218518, 0.9330127018922194093 ) ) 
 REPRESENTATION_ITEM ( '' )  );
#168710 = CARTESIAN_POINT ( 'NONE',  ( 1.499999999999993117, 11.38541666734946567, 0.8660254037844409281 ) ) ;
#168709 = CARTESIAN_POINT ( 'NONE',  ( 6.883263157960362477, -0.004191378316371896506, 2.053658919477070910 ) ) ;
#168711 = ORIENTED_EDGE ( 'NONE', *, *, #27074, .T. ) ;
#168712 = CARTESIAN_POINT ( 'NONE',  ( 5.115861365725078436, 0.1511377038382749338, 2.010826595755777824 ) ) ;
#168714 = CARTESIAN_POINT ( 'NONE',  ( 4.399324768961708543, -1.796976987717312291, 1.012281656189101264 ) ) ;
#168713 = CARTESIAN_POINT ( 'NONE',  ( 5.311043488251262268, 7.219303374425030562, -1.599625672291256295 ) ) ;
#168716 = CARTESIAN_POINT ( 'NONE',  ( 3.475000000000000533, -2.945833333333332416, -2.006292185433951047 ) ) ;
#168715 = CARTESIAN_POINT ( 'NONE',  ( 6.367489420273535039, 7.457767740854454708, -1.199719254218452047 ) ) ;
#168717 = EDGE_CURVE ( 'NONE', #114731, #183021, #199748, .T. ) ;
#168718 = CARTESIAN_POINT ( 'NONE',  ( 6.984385409695311964, 8.177479728513226576, 1.199719254218452935 ) ) ;
#168719 = CARTESIAN_POINT ( 'NONE',  ( -1.642778471874998480, -0.4010416661887096224, 2.845375778867863303 ) ) ;
#168720 = CARTESIAN_POINT ( 'NONE',  ( 1.257518954445002723, 2.989770990628810132, 0.7750000000000100142 ) ) ;
#168721 = CARTESIAN_POINT ( 'NONE',  ( 0.5860218096905758234, -2.075098906900944673, -0.2538066186672620628 ) ) ;
#168722 = CARTESIAN_POINT ( 'NONE',  ( 5.080704010962952211, -0.7231418808758652839, 1.882473355234378865 ) ) ;
#168723 = CARTESIAN_POINT ( 'NONE',  ( 4.739718475747470627, 1.836682745182907972, 0.1304020654292817605 ) ) ;
#168724 = EDGE_CURVE ( 'NONE', #121123, #29604, #142592, .T. ) ;
#168725 = CARTESIAN_POINT ( 'NONE',  ( 6.654354466208897811, 6.657835053532175529, 0.7998128361456341429 ) ) ;
#168726 = CARTESIAN_POINT ( 'NONE',  ( 0.3578718668165404293, 0.6529773653428347924, 1.596609206317510132 ) ) ;
#168727 = CARTESIAN_POINT ( 'NONE',  ( -2.428882075142555497, 5.985446187641602300, 1.040834085586084257E-14 ) ) ;
#168728 = CARTESIAN_POINT ( 'NONE',  ( 0.9327830709247152408, -1.816692068203207056, -1.408362870467388950 ) ) ;
#168729 = CARTESIAN_POINT ( 'NONE',  ( -6.575868197828002693, 7.630599971342813426, 1.199719254218450271 ) ) ;
#168730 = CARTESIAN_POINT ( 'NONE',  ( 1.036823874139713997, 2.229064601995099260, 0.3862009557947677640 ) ) ;
#168731 = CARTESIAN_POINT ( 'NONE',  ( 2.912826151168836031, 1.525034000978764626, -1.452760968584436707 ) ) ;
#168732 = CARTESIAN_POINT ( 'NONE',  ( -6.120580001926503755, 6.105374521861167914, -0.7998128361456362523 ) ) ;
#168733 = B_SPLINE_CURVE_WITH_KNOTS ( 'NONE', 3,
 ( #208171, #110757, #159436, #44642, #11034, #146419, #77112, #59803, #143236, #58741, #124893, #209225, #42517, #108623, #174651, #192989, #213490, #130217, #131268, #81385, #165835, #15298, #117142, #147468, #98709, #17420, #197255, #198310, #67234, #100822, #66158, #34749, #65112, #164768, #64074, #48894, #182061, #196211, #166907, #115014, #33693, #16359, #51020, #83503, #149585, #183145, #181011, #82437, #1169, #32632, #49951, #133368, #18500, #132303, #84579, #148527, #93, #47852, #116071, #99769, #113963, #199374, #150666, #2228, #68304, #212432, #179960, #31583, #97658, #163716, #11795, #4061, #170860, #188169, #94969, #211876, #33138, #51526, #210563, #180214, #204965, #91265, #74147, #88259, #122992, #124050, #56823, #172720, #23229, #205181, #170562, #8060, #140240, #55750, #4826, #171632, #91482, #206262, #188950, #57887, #173804, #21083, #107779, #38438, #138084, #169501, #141324, #24298, #70905, #203043, #87186, #187875, #71975, #90402, #121906, #153251, #75213, #53620, #119753, #137016, #25382, #156472, #190016, #204098, #39502, #54684, #41668, #157542, #185732, #186810, #9139, #37365, #105600, #89341, #22145, #155389, #6972, #120834, #40590, #154328, #103440, #104518, #73053, #5902, #139152, #106695, #93619, #142381, #44871, #60023, #193224, #192138, #211589, #43803, #10198, #76273, #128327, #58959, #208390, #45935, #14453, #113115, #13399, #178054, #63225, #110976, #27520, #126175, #109916, #62168, #125114, #11262, #29672, #112054, #175927, #179120, #159661, #77339, #79475, #95756, #176982, #46998, #143452, #209449, #108844, #80544, #161808, #158599, #61094, #174870, #127253, #28600, #145593, #94688, #26450, #207337, #191072, #42738, #160730, #30743, #12323, #129388, #78404, #144524, #210534, #195367, #96824, #92559, #194290, #162873, #167134, #148747, #198532, #49124, #82663, #50179, #31807, #83729, #115242 ),
 .UNSPECIFIED., .F., .F.,
 ( 4, 1, 1, 1, 1, 1, 1, 1, 1, 1, 1, 1, 1, 1, 1, 1, 1, 1, 1, 1, 1, 1, 1, 1, 1, 1, 1, 1, 1, 1, 1, 1, 1, 1, 1, 1, 1, 1, 1, 1, 1, 1, 1, 1, 1, 1, 1, 1, 1, 1, 1, 1, 1, 1, 1, 1, 1, 1, 1, 1, 1, 1, 1, 1, 1, 1, 1, 1, 1, 1, 1, 1, 1, 1, 1, 1, 1, 1, 1, 1, 1, 1, 1, 1, 1, 1, 1, 1, 1, 1, 1, 1, 1, 1, 1, 1, 1, 1, 1, 1, 1, 1, 1, 1, 1, 1, 1, 1, 1, 1, 1, 1, 1, 1, 1, 1, 1, 1, 1, 1, 1, 1, 1, 1, 1, 1, 1, 1, 1, 1, 1, 1, 1, 1, 1, 1, 1, 1, 1, 1, 1, 1, 1, 1, 1, 1, 1, 1, 1, 1, 1, 1, 1, 1, 1, 1, 1, 1, 1, 1, 1, 1, 1, 1, 1, 1, 1, 1, 1, 1, 1, 1, 1, 1, 1, 1, 1, 1, 1, 1, 1, 1, 1, 1, 1, 1, 1, 1, 1, 1, 1, 1, 1, 1, 1, 1, 1, 1, 1, 1, 1, 1, 1, 1, 1, 1, 1, 1, 1, 1, 1, 1, 1, 1, 1, 1, 4 ),
 ( 0.000000000000000000, 0.004629629629629626771, 0.009259259259259253541, 0.01388888888888887771, 0.01851851851851850361, 0.02314814814814812952, 0.02777777777777775542, 0.03240740740740737785, 0.03703703703703700723, 0.04166666666666662966, 0.04629629629629625903, 0.05092592592592588147, 0.05555555555555549696, 0.06018518518518511939, 0.06481481481481474183, 0.06944444444444436426, 0.07407407407407398670, 0.07870370370370359525, 0.08333333333333321769, 0.08796296296296284012, 0.09259259259259246255, 0.09722222222222209886, 0.1018518518518517213, 0.1064814814814813299, 0.1111111111111109523, 0.1157407407407405747, 0.1203703703703701972, 0.1249999999999998196, 0.1296296296296294281, 0.1342592592592590506, 0.1388888888888886730, 0.1435185185185182954, 0.1481481481481479179, 0.1527777777777775403, 0.1574074074074071627, 0.1620370370370367852, 0.1666666666666664076, 0.1712962962962960300, 0.1759259259259256525, 0.1805555555555552749, 0.1851851851851848973, 0.1898148148148145198, 0.1944444444444441145, 0.1990740740740737091, 0.2037037037037033038, 0.2083333333333328985, 0.2129629629629625209, 0.2175925925925921156, 0.2222222222222217103, 0.2268518518518513050, 0.2314814814814808996, 0.2361111111111104943, 0.2407407407407401168, 0.2453703703703697114, 0.2499999999999993061, 0.2546296296296289285, 0.2592592592592585232, 0.2638888888888881179, 0.2685185185185177126, 0.2731481481481473073, 0.2777777777777769019, 0.2824074074074064966, 0.2870370370370360913, 0.2916666666666656860, 0.2962962962962952806, 0.3009259259259249308, 0.3055555555555545255, 0.3101851851851841202, 0.3148148148148137149, 0.3194444444444433095, 0.3240740740740729042, 0.3287037037037024989, 0.3333333333333320936, 0.3379629629629616883, 0.3425925925925912829, 0.3472222222222209331, 0.3518518518518505278, 0.3564814814814801225, 0.3611111111111097172, 0.3657407407407393118, 0.3703703703703689065, 0.3749999999999985567, 0.3796296296296282069, 0.3842592592592578571, 0.3888888888888874518, 0.3935185185185171020, 0.3981481481481467521, 0.4027777777777764023, 0.4074074074074060525, 0.4120370370370357027, 0.4166666666666652974, 0.4212962962962949476, 0.4259259259259245978, 0.4305555555555542480, 0.4351851851851838981, 0.4398148148148135483, 0.4444444444444431430, 0.4490740740740727932, 0.4537037037037024434, 0.4583333333333320936, 0.4629629629629617438, 0.4675925925925913940, 0.4722222222222209886, 0.4768518518518506388, 0.4814814814814802890, 0.4861111111111099392, 0.4907407407407395894, 0.4953703703703692396, 0.4999999999999988898, 0.5046296296296285400, 0.5092592592592581902, 0.5138888888888878403, 0.5185185185185173795, 0.5231481481481470297, 0.5277777777777766799, 0.5324074074074063301, 0.5370370370370359803, 0.5416666666666656305, 0.5462962962962952806, 0.5509259259259249308, 0.5555555555555545810, 0.5601851851851842312, 0.5648148148148138814, 0.5694444444444435316, 0.5740740740740730708, 0.5787037037037027210, 0.5833333333333323711, 0.5879629629629620213, 0.5925925925925916715, 0.5972222222222213217, 0.6018518518518509719, 0.6064814814814806221, 0.6111111111111102723, 0.6157407407407399225, 0.6203703703703695727, 0.6249999999999992228, 0.6296296296296287620, 0.6342592592592584122, 0.6388888888888880624, 0.6435185185185177126, 0.6481481481481473628, 0.6527777777777770130, 0.6574074074074066631, 0.6620370370370363133, 0.6666666666666659635, 0.6712962962962956137, 0.6759259259259252639, 0.6805555555555549141, 0.6851851851851845643, 0.6898148148148141034, 0.6944444444444437536, 0.6990740740740734038, 0.7037037037037030540, 0.7083333333333327042, 0.7129629629629623544, 0.7175925925925920046, 0.7222222222222216548, 0.7268518518518513050, 0.7314814814814809552, 0.7361111111111106053, 0.7407407407407402555, 0.7453703703703697947, 0.7499999999999994449, 0.7546296296296290951, 0.7592592592592586342, 0.7638888888888882844, 0.7685185185185179346, 0.7731481481481475848, 0.7777777777777772350, 0.7824074074074068852, 0.7870370370370365354, 0.7916666666666661856, 0.7962962962962958358, 0.8009259259259254859, 0.8055555555555551361, 0.8101851851851847863, 0.8148148148148143255, 0.8194444444444439757, 0.8240740740740736259, 0.8287037037037032761, 0.8333333333333329263, 0.8379629629629625764, 0.8425925925925922266, 0.8472222222222218768, 0.8518518518518515270, 0.8564814814814811772, 0.8611111111111108274, 0.8657407407407404776, 0.8703703703703701278, 0.8749999999999996669, 0.8796296296296293171, 0.8842592592592589673, 0.8888888888888886175, 0.8935185185185182677, 0.8981481481481479179, 0.9027777777777775681, 0.9074074074074072183, 0.9120370370370368684, 0.9166666666666665186, 0.9212962962962961688, 0.9259259259259258190, 0.9305555555555553582, 0.9351851851851850084, 0.9398148148148146586, 0.9444444444444443088, 0.9490740740740739589, 0.9537037037037036091, 0.9583333333333332593, 0.9629629629629629095, 0.9675925925925925597, 0.9722222222222222099, 0.9768518518518518601, 0.9814814814814815103, 0.9861111111111110494, 0.9907407407407406996, 0.9953703703703703498, 1.000000000000000000 ),
 .UNSPECIFIED. ) ;
#168734 = CARTESIAN_POINT ( 'NONE',  ( 6.262976894508937242, 9.394224579314053969, -1.199719254218440723 ) ) ;
#168735 = CARTESIAN_POINT ( 'NONE',  ( 5.465345319640213972, 8.429967735338637524, -1.082531754730548412 ) ) ;
#168736 = CARTESIAN_POINT ( 'NONE',  ( -7.074657228232555717, 7.148188275893099686, 1.040834085586084257E-14 ) ) ;
#168737 = CARTESIAN_POINT ( 'NONE',  ( 7.266807146800403849, 7.580289214129690478, 1.040834085586084257E-14 ) ) ;
#168738 = CARTESIAN_POINT ( 'NONE',  ( 4.748509658595381211, 7.014904321862622361, 1.395353610025750646 ) ) ;
#168739 = CARTESIAN_POINT ( 'NONE',  ( -3.623053363349869382, 5.249981562040033189, 1.599625672291267398 ) ) ;
#168740 = CARTESIAN_POINT ( 'NONE',  ( 5.554997651100567424, 0.4332456915393156915, 2.178594967391647597 ) ) ;
#168741 = CARTESIAN_POINT ( 'NONE',  ( 1.922082643403967506, 1.260107670313360240, -1.792737600334909365 ) ) ;
#168742 = CARTESIAN_POINT ( 'NONE',  ( -4.900382456335551140, 7.804531068111707270, 1.199719254218464037 ) ) ;
#168743 = CARTESIAN_POINT ( 'NONE',  ( -4.767627293860968507, 5.591261926706423857, -1.199719254218453823 ) ) ;
#168744 = CARTESIAN_POINT ( 'NONE',  ( 5.283633159863808437, -1.863482887291990409, 0.6137318589548645953 ) ) ;
#168745 = CARTESIAN_POINT ( 'NONE',  ( -1.364683531250000748, 2.259375000341422357, 1.214306433183764966E-14 ) ) ;
#168746 = CARTESIAN_POINT ( 'NONE',  ( 6.890000000000006786, 1.992106636881568305, 2.580154195607385237 ) ) ;
#168747 = CARTESIAN_POINT ( 'NONE',  ( -5.775410249741523394, 5.840326167560965231, 0.7216878364870317197 ) ) ;
#168749 = CARTESIAN_POINT ( 'NONE',  ( 4.078469121099765005, 1.002472831208834680, 1.868716877859360137 ) ) ;
#168748 = AXIS2_PLACEMENT_3D ( 'NONE', #100994, #149766, #183316 ) ;
#168750 = CARTESIAN_POINT ( 'NONE',  ( -5.465345320084574965, 9.390336950158399532, 0.000000000000000000 ) ) ;
#168751 = ORIENTED_EDGE ( 'NONE', *, *, #161480, .F. ) ;
#168753 = CARTESIAN_POINT ( 'NONE',  ( 6.737200384369169903, -1.933438233944267060, 0.9670071574134844195 ) ) ;
#168752 = CARTESIAN_POINT ( 'NONE',  ( -5.966997003790228682, 8.054858819212300958, -1.443375672974066548 ) ) ;
#168754 = CARTESIAN_POINT ( 'NONE',  ( 5.900823170445728572, 7.907379670318584353, 1.599625672291267398 ) ) ;
#168755 = CARTESIAN_POINT ( 'NONE',  ( 4.722110844128335039, 1.763445737372179689, 0.5296355584529164329 ) ) ;
#168756 = PRESENTATION_STYLE_ASSIGNMENT (( #199090 ) ) ;
#168757 = CARTESIAN_POINT ( 'NONE',  ( 0.6823417656249899377, 2.905208333674754062, 1.181850606188765695 ) ) ;
#168758 = CARTESIAN_POINT ( 'NONE',  ( 0.5557209801456406417, -1.262220463910254331, 1.198535436172887714 ) ) ;
#168759 = CARTESIAN_POINT ( 'NONE',  ( 1.286956418854607431, 3.652345658002486672, 0.4592741676706121323 ) ) ;
#168760 = CARTESIAN_POINT ( 'NONE',  ( 0.1472015564608893656, 3.384172088701932424, 2.075648132225481390 ) ) ;
#168761 = CARTESIAN_POINT ( 'NONE',  ( 5.155217493315787713, -1.824165352752779246, -1.159627250419709155 ) ) ;
#168762 = CARTESIAN_POINT ( 'NONE',  ( -3.490334480514268645, 6.159475096320226939, -1.199719254218452935 ) ) ;
#168763 = CARTESIAN_POINT ( 'NONE',  ( -7.253248993186740989, 9.485209796849769504, 1.443375672974090751 ) ) ;
#168764 = VECTOR ( 'NONE', #7520, 1000.000000000000114 ) ;
#168765 = CARTESIAN_POINT ( 'NONE',  ( 4.276362541559985075, -1.246951984143488623, 1.765614359104182629 ) ) ;
#168766 = CARTESIAN_POINT ( 'NONE',  ( 0.6823417656249899377, 3.676041667008085767, -1.181850606188754593 ) ) ;
#168767 = CARTESIAN_POINT ( 'NONE',  ( 5.079350664050449105, 1.840474797211266944, -0.7068060451330003824 ) ) ;
#168768 = CARTESIAN_POINT ( 'NONE',  ( 4.077271355118361029, 1.226738060269889408, -1.225556752838660168 ) ) ;
#168769 = CARTESIAN_POINT ( 'NONE',  ( 0.5389544483674936215, -1.876709678404146153, 1.131566444868239874 ) ) ;
#168770 = CARTESIAN_POINT ( 'NONE',  ( 1.958496456072187142, 2.301298802517747877, -0.1708829291464097622 ) ) ;
#168771 = CARTESIAN_POINT ( 'NONE',  ( 4.481748981177747559, 1.343215529357727478, 1.562995469165892493 ) ) ;
#168772 = CARTESIAN_POINT ( 'NONE',  ( 6.251511512115349056, 1.936530502255621622, -0.1475284815631947022 ) ) ;
#168774 = ORIENTED_EDGE ( 'NONE', *, *, #186635, .T. ) ;
#168773 = CARTESIAN_POINT ( 'NONE',  ( -7.497295758232736418, 7.849192594134070333, -0.7216878364870267237 ) ) ;
#168775 = CARTESIAN_POINT ( 'NONE',  ( -5.387385936583832802, 7.378645907471495846, -1.599625672291271394 ) ) ;
#168776 = FACE_OUTER_BOUND ( 'NONE', #17102, .T. ) ;
#168777 = CARTESIAN_POINT ( 'NONE',  ( -3.383641855062333281, 6.105276709951447778, -1.199719254218452047 ) ) ;
#168778 = CARTESIAN_POINT ( 'NONE',  ( -5.517805330637490790, 9.381263952478319013, 0.7216878364870458196 ) ) ;
#168779 = CARTESIAN_POINT ( 'NONE',  ( 2.995379075007987613, 1.893430763284314811, -1.133229021217339483 ) ) ;
#168780 = CARTESIAN_POINT ( 'NONE',  ( -3.285556943749998737, -2.267708332855375986, 1.896917185911908499 ) ) ;
#168781 = CARTESIAN_POINT ( 'NONE',  ( 0.5845111633032008536, 1.778450750175617712, 0.5478710867917855332 ) ) ;
#168782 = CARTESIAN_POINT ( 'NONE',  ( -6.427974226210522168, 6.671927150099951298, 0.000000000000000000 ) ) ;
#168783 = CARTESIAN_POINT ( 'NONE',  ( 0.7499999999999902300, 5.597916667349482900, -1.299038105676658228 ) ) ;
#168784 = CARTESIAN_POINT ( 'NONE',  ( -9.500479199177402023, -7.792108994755980511, 0.01138762994425606724 ) ) ;
#168786 = CARTESIAN_POINT ( 'NONE',  ( 6.825078400183550720, 0.5766433668599518780, 2.097246334241170906 ) ) ;
#168785 = CARTESIAN_POINT ( 'NONE',  ( -5.188065202531182862, 7.850521293832936287, -1.269213148129512136 ) ) ;
#168787 = CARTESIAN_POINT ( 'NONE',  ( 5.982333729491329244, -0.2747192703472668418, -1.820405398140816589 ) ) ;
#168788 = ORIENTED_EDGE ( 'NONE', *, *, #55029, .T. ) ;
#168789 = CARTESIAN_POINT ( 'NONE',  ( 3.274343757225039120, -1.228935477529419451, 1.654214949985348904 ) ) ;
#168790 = CARTESIAN_POINT ( 'NONE',  ( -3.956095110007852622E-14, 2.328125000341396689, -1.570758158831800255 ) ) ;
#168791 = CARTESIAN_POINT ( 'NONE',  ( -4.880045225915050189, 7.780804299287790826, 1.199719254218464037 ) ) ;
#168792 = CARTESIAN_POINT ( 'NONE',  ( 2.736978119973699108, 1.902454848370996210, 0.6784627630139413723 ) ) ;
#168793 = EDGE_CURVE ( 'NONE', #184329, #179126, #168283, .T. ) ;
#168794 = CARTESIAN_POINT ( 'NONE',  ( 2.686486993802192913, 6.285985259411197568, 0.7998128361456362523 ) ) ;
#168795 = CARTESIAN_POINT ( 'NONE',  ( 1.622021928100621624, -1.144040325636319189, -1.713970819250490552 ) ) ;
#168797 = CARTESIAN_POINT ( 'NONE',  ( -1.364683531250010295, 12.88020833367473372, 0.7879004041258445001 ) ) ;
#168796 = CARTESIAN_POINT ( 'NONE',  ( -1.499999999999997780, 7.240846818246208905, -4.154462424328208670 ) ) ;
#168798 = CARTESIAN_POINT ( 'NONE',  ( 6.830610463186557624, 6.863467050006115677, 1.040834085586084257E-14 ) ) ;
#168799 =( BOUNDED_CURVE ( )  B_SPLINE_CURVE ( 3, ( #154817, #57313, #123477, #41082 ),
 .UNSPECIFIED., .F., .T. ) 
 B_SPLINE_CURVE_WITH_KNOTS ( ( 4, 4 ),
 ( 0.000000000000000000, 0.4999999999999986677 ),
 .UNSPECIFIED. ) 
 CURVE ( )  GEOMETRIC_REPRESENTATION_ITEM ( )  RATIONAL_B_SPLINE_CURVE ( ( 1.000000000000000222, 0.3333333333333352022, 0.3333333333333334259, 0.9999999999999984457 ) ) 
 REPRESENTATION_ITEM ( '' )  );
#168800 = CARTESIAN_POINT ( 'NONE',  ( 2.696596522755183578, 2.993039318081675226, 2.500000000000000444 ) ) ;
#168801 = CARTESIAN_POINT ( 'NONE',  ( 5.180388087185870738, -1.228261608319089149, 1.833297759731546073 ) ) ;
#168802 = CARTESIAN_POINT ( 'NONE',  ( 1.229993901927586286, -1.370328181169593096, -1.671761099108048265 ) ) ;
#168803 = CARTESIAN_POINT ( 'NONE',  ( -5.761852096127856981, 5.824508321678349532, 0.000000000000000000 ) ) ;
#168804 = CARTESIAN_POINT ( 'NONE',  ( 0.9718890779336667451, -0.9023411006064323558, 1.803417998987096427 ) ) ;
#168805 = AXIS2_PLACEMENT_3D ( 'NONE', #71637, #171292, #22884 ) ;
#168806 = CARTESIAN_POINT ( 'NONE',  ( 1.968534425330380921, 1.910819170882430695, 1.277001204893423170 ) ) ;
#168807 = CARTESIAN_POINT ( 'NONE',  ( 4.647606103345025552, 8.407977806742819027, 0.6343139517084724899 ) ) ;
#168808 = CARTESIAN_POINT ( 'NONE',  ( 6.322915745023367506, 1.413667134151237459, -1.287952294376143447 ) ) ;
#168810 = VERTEX_POINT ( 'NONE', #192351 ) ;
#168809 = CARTESIAN_POINT ( 'NONE',  ( 3.092648394857516525, 6.449253795920727228, -0.4031905389056261724 ) ) ;
#168811 = CARTESIAN_POINT ( 'NONE',  ( 1.639302681421180852, -1.352760811461351187, -1.292285834730775074 ) ) ;
#168812 = CARTESIAN_POINT ( 'NONE',  ( 3.801970467005914678, -1.040791964576088358, -1.727064642965264740 ) ) ;
#168814 = CARTESIAN_POINT ( 'NONE',  ( 11.55950211276791428, 13.87999999999998302, 3.221476510067112109 ) ) ;
#168813 = CARTESIAN_POINT ( 'NONE',  ( -1.201851678989727383E-14, 2.321875000341416584, 1.575800808251672791 ) ) ;
#168816 = CARTESIAN_POINT ( 'NONE',  ( 5.619784395276031574, -2.055015178219528948, 0.4601488667864346849 ) ) ;
#168815 = CARTESIAN_POINT ( 'NONE',  ( -7.690499447449645309, 9.995335326823163058, 1.599625672291295375 ) ) ;
#168817 = CARTESIAN_POINT ( 'NONE',  ( 5.798083248138522272, 9.916180889470295412, 0.7998128361456462443 ) ) ;
#168819 = CARTESIAN_POINT ( 'NONE',  ( -7.985916173649233230, 9.275655943134292869, -1.199719254218446718 ) ) ;
#168818 = CARTESIAN_POINT ( 'NONE',  ( 3.562760505341037831, 7.378580699531681830, -1.734723475976807094E-15 ) ) ;
#168820 = DIRECTION ( 'NONE',  ( -0.000000000000000000, -1.000000000000000000, 0.000000000000000000 ) ) ;
#168821 = CARTESIAN_POINT ( 'NONE',  ( 4.781513128076603003, 0.1936695275622651868, -2.010448953515688419 ) ) ;
#168822 = CARTESIAN_POINT ( 'NONE',  ( -1.402160292154681736E-14, -0.3812499993171785673, -1.732050807568870754 ) ) ;
#168823 = CARTESIAN_POINT ( 'NONE',  ( 0.7255239074139888666, 0.2060675592777498066, -2.052282084198739920 ) ) ;
#168824 = CARTESIAN_POINT ( 'NONE',  ( 8.595506201384013778, 10.09080732544527592, 1.082531754730558626 ) ) ;
#168825 = CARTESIAN_POINT ( 'NONE',  ( 6.170896192875352959, 7.228408975556602556, 1.199719254218453823 ) ) ;
#168826 = CARTESIAN_POINT ( 'NONE',  ( -0.6823417656250003738, -0.7197916663252492686, -1.181850606188749264 ) ) ;
#168828 = CARTESIAN_POINT ( 'NONE',  ( 3.146123468421266001, 6.442327133617253843, 0.5169845646841256803 ) ) ;
#168827 = CARTESIAN_POINT ( 'NONE',  ( 5.879395890181562834, 6.888325289080478697, -1.199719254218452047 ) ) ;
#168829 = CARTESIAN_POINT ( 'NONE',  ( 8.581948047326003248, 9.114620264742901767, -0.7216878364870197293 ) ) ;
#168831 = PLANE ( 'NONE',  #121515 ) ;
#168830 = CARTESIAN_POINT ( 'NONE',  ( 3.420551359632235222, 0.9736478647841840806, 1.940675715818460878 ) ) ;
#168833 = CARTESIAN_POINT ( 'NONE',  ( 1.786409390178132162, 1.601450680722369846, -0.9084932335857234253 ) ) ;
#168832 = CARTESIAN_POINT ( 'NONE',  ( -4.392478581147607031, 7.108013530438723748, 1.082531754730560403 ) ) ;
#168834 = MANIFOLD_SOLID_BREP ( 'Sweep1[1]', #174487 ) ;
#168835 = CARTESIAN_POINT ( 'NONE',  ( -0.6823417656249969321, 3.717708333674754506, -1.181850606188749264 ) ) ;
#168836 = CARTESIAN_POINT ( 'NONE',  ( 3.825867475279482566, 1.171244075711602051, -1.852137614134836907 ) ) ;
#168837 = CARTESIAN_POINT ( 'NONE',  ( 3.019342412789784547, 6.452475500722323787, 0.1501914610189964416 ) ) ;
#168838 = CARTESIAN_POINT ( 'NONE',  ( 5.102513680054168610, -0.7571875712604788644, -2.132187818420825831 ) ) ;
#168839 = CARTESIAN_POINT ( 'NONE',  ( -6.175902666224832416, 7.163973517805802160, -1.199719254218446718 ) ) ;
#168841 = CIRCLE ( 'NONE', #3226, 0.08000000000000020983 ) ;
#168840 = DIRECTION ( 'NONE',  ( -0.1430349330369308225, 0.000000000000000000, -0.9897176405071906879 ) ) ;
#168842 = CARTESIAN_POINT ( 'NONE',  ( 5.010605496441194795, 7.906410611435644498, -1.080668833775387139 ) ) ;
#168843 = CARTESIAN_POINT ( 'NONE',  ( -1.500000000000015099, 13.47916666666667140, -0.8660254037844309360 ) ) ;
#168844 = CARTESIAN_POINT ( 'NONE',  ( -4.773879485343255347, 8.583626809626847987, 0.000000000000000000 ) ) ;
#168845 = CARTESIAN_POINT ( 'NONE',  ( 5.397554552016226914, 6.430140077841320689, 1.082531754730549078 ) ) ;
#168846 = CARTESIAN_POINT ( 'NONE',  ( 5.079261616685217362, 1.651278277306899911, -0.6370931631965012221 ) ) ;
#168847 = CARTESIAN_POINT ( 'NONE',  ( 6.795661308947685164, 8.951357498570873261, -1.599625672291262513 ) ) ;
#168848 = CARTESIAN_POINT ( 'NONE',  ( 1.712088352014268899, -2.090129137712465557, 0.2570578816783394283 ) ) ;
#168850 = CARTESIAN_POINT ( 'NONE',  ( -1.500000000000011324, 2.920833333333352932, 0.8660254037844403729 ) ) ;
#168849 = CARTESIAN_POINT ( 'NONE',  ( -1.364683531250000748, 11.35937500034139802, 0.000000000000000000 ) ) ;
#168851 = CARTESIAN_POINT ( 'NONE',  ( 2.418351439525995961, 0.8393807748916733980, 1.781860320225916228 ) ) ;
#168852 = AXIS2_PLACEMENT_3D ( 'NONE', #210373, #80389, #146485 ) ;
#168853 = CARTESIAN_POINT ( 'NONE',  ( 0.3911966820569385828, 1.383097094795827209, 1.259704262696823118 ) ) ;
#168854 = CARTESIAN_POINT ( 'NONE',  ( -1.500000000000005773, 5.410416667349489117, -0.8660254037844342667 ) ) ;
#168856 = ORIENTED_EDGE ( 'NONE', *, *, #158080, .T. ) ;
#168855 = CARTESIAN_POINT ( 'NONE',  ( 5.308800944376626418, -0.4481363076810992996, -1.755139329022289196 ) ) ;
#168857 = CARTESIAN_POINT ( 'NONE',  ( 6.832946231607457399, 7.074118146404578589, -0.7216878364870257245 ) ) ;
#168858 = CARTESIAN_POINT ( 'NONE',  ( -0.6823417656250003738, -0.4697916663252491021, -1.181850606188749264 ) ) ;
#168859 = EDGE_CURVE ( 'NONE', #9969, #101274, #83567, .T. ) ;
#168860 = CARTESIAN_POINT ( 'NONE',  ( 5.805500895539822181, -0.4530025297027095443, 1.814837910242727226 ) ) ;
#168861 = CARTESIAN_POINT ( 'NONE',  ( 5.401260523219934662, -1.778462342247935979, 1.059464396209061521 ) ) ;
#168862 = DIRECTION ( 'NONE',  ( 7.387867266669436732E-31, -1.000000000000000000, -8.546850786086424434E-32 ) ) ;
#168863 = CARTESIAN_POINT ( 'NONE',  ( -4.272227801637618505, 7.998366511970260717, 0.7216878364870338292 ) ) ;
#168864 = CARTESIAN_POINT ( 'NONE',  ( -0.7500000000000006661, 0.6083333333333564852, -1.299038105676652011 ) ) ;
#168865 = CARTESIAN_POINT ( 'NONE',  ( 7.884230021546724920, 9.157022099014721306, 1.199719254218462483 ) ) ;
#168866 = CARTESIAN_POINT ( 'NONE',  ( -9.691380875670077444, 10.20103253123691189, 0.7998128361456462443 ) ) ;
#168867 = CARTESIAN_POINT ( 'NONE',  ( 4.993145711582793744, 9.047363440147082159, -0.7998128361456481317 ) ) ;
#168868 = CARTESIAN_POINT ( 'NONE',  ( -1.402160292154681736E-14, -0.4281249996585808071, 1.575800808251672791 ) ) ;
#168869 = CARTESIAN_POINT ( 'NONE',  ( -0.7500000000000006661, 0.8583333333333567072, -1.299038105676652011 ) ) ;
#168871 = CARTESIAN_POINT ( 'NONE',  ( 6.498435699651741615, 6.475929825882159818, -0.7998128361456281477 ) ) ;
#168870 = CARTESIAN_POINT ( 'NONE',  ( 4.809014631063706524, -1.576880339463518022, 1.167019128429528374 ) ) ;
#168872 = CARTESIAN_POINT ( 'NONE',  ( 3.743517394402117837, -1.942243990624907823, -0.5404084370827857420 ) ) ;
#168873 = CARTESIAN_POINT ( 'NONE',  ( 2.219824929201766217, 0.8990433841352833966, -1.691613514901336490 ) ) ;
#168874 = SPHERICAL_SURFACE ( 'NONE', #141786, 0.08000000000000000167 ) ;
#168875 = CARTESIAN_POINT ( 'NONE',  ( 0.2049558871960316941, 1.909868400323280424, 1.074723926240577221 ) ) ;
#168876 = CARTESIAN_POINT ( 'NONE',  ( 0.1333692844072802142, 2.017199222642913625, -2.468757726274827036 ) ) ;
#168877 = CARTESIAN_POINT ( 'NONE',  ( 1.721729502718066795, -1.034818790731323990, -1.558030248997283040 ) ) ;
#168878 = CARTESIAN_POINT ( 'NONE',  ( -1.364683531249997417, 5.009375000341425022, 1.214306433183764966E-14 ) ) ;
#168879 = CARTESIAN_POINT ( 'NONE',  ( 4.113543134289789016, 1.619545278408863975, 1.195698625712667384 ) ) ;
#168880 = CARTESIAN_POINT ( 'NONE',  ( -6.723954117373590833, 9.932031339322813679, -1.199719254218440723 ) ) ;
#168882 = CARTESIAN_POINT ( 'NONE',  ( 4.833676624637527119, 0.6627930923091308602, -2.010898772050497829 ) ) ;
#168881 = CARTESIAN_POINT ( 'NONE',  ( -5.585596099150193616, 6.579245539505756746, -1.082531754730544860 ) ) ;
#168883 = CARTESIAN_POINT ( 'NONE',  ( 6.513344551206667887E-14, -9.900000000000005684, -9.500331257164612353 ) ) ;
#168884 = CARTESIAN_POINT ( 'NONE',  ( 6.584440175795505112, 1.195396180001909059, -1.690200020538407566 ) ) ;
#168886 = CARTESIAN_POINT ( 'NONE',  ( 6.620655732516628866, 4.686767102414819419, 2.836268676114994669 ) ) ;
#168885 = CARTESIAN_POINT ( 'NONE',  ( 1.417645169044414288, -1.164320182712182294, -1.736329362061867387 ) ) ;
#168888 = VERTEX_POINT ( 'NONE', #156688 ) ;
#168887 = CARTESIAN_POINT ( 'NONE',  ( 6.756878055424797580, -1.408711550780303634, 1.160885376127060775 ) ) ;
#168889 = EDGE_CURVE ( 'NONE', #11196, #198793, #54110, .T. ) ;
#168890 = CARTESIAN_POINT ( 'NONE',  ( 8.762647353133951711, 9.117510088278095282, 1.040834085586084257E-14 ) ) ;
#168891 = CARTESIAN_POINT ( 'NONE',  ( -5.886439722289627419, 6.118937485343680649, -0.7679415244158313003 ) ) ;
#168892 = DIRECTION ( 'NONE',  ( -1.276756478318931402E-15, 1.000000000000000000, 0.000000000000000000 ) ) ;
#168893 = DIRECTION ( 'NONE',  ( 5.578564026256490882E-16, 1.000000000000000000, 9.066213480720158442E-32 ) ) ;
#168894 = CARTESIAN_POINT ( 'NONE',  ( 7.768458830506048685, 8.165549511786275971, -0.7216878364870267237 ) ) ;
#168895 = CARTESIAN_POINT ( 'NONE',  ( -1.907862554904952379, 3.236716050607317818, 0.4606469147255249363 ) ) ;
#168897 = CARTESIAN_POINT ( 'NONE',  ( 0.8206315121990900296, 1.372318096965993384, -1.182507040619881877 ) ) ;
#168896 = CARTESIAN_POINT ( 'NONE',  ( 6.831329296439236032, 9.063246493969506545, -1.599625672291267398 ) ) ;
#168898 = CARTESIAN_POINT ( 'NONE',  ( -7.320512876374914768, 10.62801655815766999, 1.199719254218453823 ) ) ;
#168899 = CIRCLE ( 'NONE', #41058, 0.07999999999999984901 ) ;
#168900 = CARTESIAN_POINT ( 'NONE',  ( 6.166260936116925606, 6.088392601758203071, 0.7998128361456341429 ) ) ;
#168901 = CYLINDRICAL_SURFACE ( 'NONE', #73120, 1.250000000000000000 ) ;
#168902 = CARTESIAN_POINT ( 'NONE',  ( -11.33772463945043718, 10.89999999999999147, 3.600000000000075140 ) ) ;
#168903 = CARTESIAN_POINT ( 'NONE',  ( 9.571693261567954636, 12.19006144329456731, 1.443375672974076540 ) ) ;
#168904 = ORIENTED_EDGE ( 'NONE', *, *, #932, .T. ) ;
#168905 = CARTESIAN_POINT ( 'NONE',  ( 6.187125092307005580, 1.678016663812756937, 1.117817459622950649 ) ) ;
#168906 = CARTESIAN_POINT ( 'NONE',  ( 0.3992906662320141464, -0.2637550127744873185, -2.103967267096308991 ) ) ;
#168907 = DIRECTION ( 'NONE',  ( -0.000000000000000000, -1.000000000000000000, -0.000000000000000000 ) ) ;
#168908 = CIRCLE ( 'NONE', #86039, 0.5000000000000011102 ) ;
#168909 = CARTESIAN_POINT ( 'NONE',  ( 0.1405533004714383249, 7.629137130509051623, -2.879722665736083709 ) ) ;
#168910 = CARTESIAN_POINT ( 'NONE',  ( -1.576106191276491542, 8.678179183658462748, -2.499999999999308109 ) ) ;
#168911 = CARTESIAN_POINT ( 'NONE',  ( -3.307826292054304673, 6.802955074131234348, -0.7216878364870267237 ) ) ;
#168912 = CARTESIAN_POINT ( 'NONE',  ( 10.07334494527360569, 10.85458331234846696, 0.000000000000000000 ) ) ;
#168913 = CARTESIAN_POINT ( 'NONE',  ( 3.977371423044063103, -0.1491618029233315879, 1.963883198941584585 ) ) ;
#168914 = CARTESIAN_POINT ( 'NONE',  ( 4.130482583401101415, 0.5405105419177670401, 1.942537254285629400 ) ) ;
#168915 = CARTESIAN_POINT ( 'NONE',  ( -5.669280788808708671, 9.765911353585494226, 0.7998128361456481317 ) ) ;
#168916 = CARTESIAN_POINT ( 'NONE',  ( 1.737499999999999378, -1.866666666666665808, -3.009438278150925683 ) ) ;
#168917 = CARTESIAN_POINT ( 'NONE',  ( -2.788906526875773208E-15, 10.18750000000000000, -1.499999999999998446 ) ) ;
#168918 = CARTESIAN_POINT ( 'NONE',  ( 4.787173061057010237, 1.622617466453496471, 1.473133629693436975 ) ) ;
#168919 = CARTESIAN_POINT ( 'NONE',  ( 3.895595285070167169, 2.800000000000017586, 0.7750000000000135669 ) ) ;
#168920 = CARTESIAN_POINT ( 'NONE',  ( 2.608320942171663326, -0.7355144804263250569, -1.780640224430999563 ) ) ;
#168921 = CARTESIAN_POINT ( 'NONE',  ( -6.832419346282942563, 10.05857410638369487, 1.199719254218453823 ) ) ;
#168922 = CARTESIAN_POINT ( 'NONE',  ( -0.02948999725180430354, 5.724051133006486936, -2.520349822069901879 ) ) ;
#168923 = DIRECTION ( 'NONE',  ( -5.551115123125783935E-17, 0.7071067811865536790, 0.7071067811865413555 ) ) ;
#168924 = EDGE_CURVE ( 'NONE', #10807, #35390, #172139, .T. ) ;
#168925 = PRESENTATION_STYLE_ASSIGNMENT (( #69266 ) ) ;
#168926 = ORIENTED_EDGE ( 'NONE', *, *, #16828, .F. ) ;
#168927 = CARTESIAN_POINT ( 'NONE',  ( 3.418064124421011041, 7.001842221884225559, -0.7216878364870338292 ) ) ;
#168928 = ORIENTED_EDGE ( 'NONE', *, *, #71800, .F. ) ;
#168929 = CARTESIAN_POINT ( 'NONE',  ( 5.401205523299864808, -1.691175329543142647, 1.008977833701154125 ) ) ;
#168931 = CARTESIAN_POINT ( 'NONE',  ( 4.512362120423671463, -2.012691318418479813, -0.04721358428917859368 ) ) ;
#168930 = CARTESIAN_POINT ( 'NONE',  ( 0.5384922876028491734, -1.664970009179422616, 0.9995421319052009146 ) ) ;
#168932 = CARTESIAN_POINT ( 'NONE',  ( 5.940817214068299990, 1.361788364613376601, 1.851425077211141801 ) ) ;
#168934 = CARTESIAN_POINT ( 'NONE',  ( 4.205779932802704124, 0.6304169756579135475, -1.751020666094662337 ) ) ;
#168933 = CARTESIAN_POINT ( 'NONE',  ( 11.92619526913699879, 10.89999999999998259, 1.328859060402684644 ) ) ;
#168935 = CARTESIAN_POINT ( 'NONE',  ( 5.352436782344940802, 9.466536356036257871, 0.000000000000000000 ) ) ;
#168936 = CARTESIAN_POINT ( 'NONE',  ( -10.98765602437504185, -5.221050908132831125, 1.680513367352532070E-15 ) ) ;
#168937 = DIRECTION ( 'NONE',  ( 0.000000000000000000, 0.000000000000000000, -1.000000000000000000 ) ) ;
#168938 = CARTESIAN_POINT ( 'NONE',  ( -5.371001409308059138, 9.417918744168066070, -0.7998128361456231517 ) ) ;
#168939 = CARTESIAN_POINT ( 'NONE',  ( -3.386157300525472369, -0.9633972889761682756, 0.4263094016780412665 ) ) ;
#168940 = CARTESIAN_POINT ( 'NONE',  ( 0.2225716830646235489, 2.098996182288978218, 0.6302611576235671587 ) ) ;
#168941 = CARTESIAN_POINT ( 'NONE',  ( 4.175548123328908900, 7.815297210618305179, -0.7216878364870197293 ) ) ;
#168942 = ORIENTED_EDGE ( 'NONE', *, *, #54130, .F. ) ;
#168943 = CARTESIAN_POINT ( 'NONE',  ( 11.29517787156874498, -8.030538574678857344, -0.1971580631239572556 ) ) ;
#168944 = CARTESIAN_POINT ( 'NONE',  ( -1.138412281109779656E-15, -6.105866302528341727, -10.72111444838821193 ) ) ;
#168945 = CARTESIAN_POINT ( 'NONE',  ( 0.6975366375942676500, -0.6598540886826111951, 1.702458561391326342 ) ) ;
#168946 = CARTESIAN_POINT ( 'NONE',  ( -4.599240423533815125, 6.388866465587984322, 1.599625672291267398 ) ) ;
#168947 = CARTESIAN_POINT ( 'NONE',  ( 2.566726881135486416, -0.8894074178381355944, 1.488501414198806883 ) ) ;
#168948 = CARTESIAN_POINT ( 'NONE',  ( 6.609000000000009756, 0.005669918681722520802, 1.900160851458796873 ) ) ;
#168949 = CARTESIAN_POINT ( 'NONE',  ( -4.950135482320926705, 6.868520377498098739, -1.443375672974066770 ) ) ;
#168950 = CARTESIAN_POINT ( 'NONE',  ( 5.813091150998386247, 1.612263477354998864, 0.8566026058636074803 ) ) ;
#168951 = CARTESIAN_POINT ( 'NONE',  ( 2.887496479553632422, -1.832211488775811414, 0.7015765724691160887 ) ) ;
#168952 = CARTESIAN_POINT ( 'NONE',  ( -1.225000000000034284, -0.4166666659838699771, 0.7072540797572656190 ) ) ;
#168953 = CARTESIAN_POINT ( 'NONE',  ( -8.992082194361570302, 11.51384853155376220, 1.599625672291269396 ) ) ;
#168954 = CARTESIAN_POINT ( 'NONE',  ( 6.612626235163189925, 8.737816579155630592, -1.599625672291262513 ) ) ;
#168955 = CARTESIAN_POINT ( 'NONE',  ( 5.004590575528129470, -2.104527602236761386, -0.2589986953433416894 ) ) ;
#168956 = CARTESIAN_POINT ( 'NONE',  ( 7.075376061485196821, 9.347967719856493218, 1.599625672291268286 ) ) ;
#168957 = CARTESIAN_POINT ( 'NONE',  ( -10.32183501870554387, 10.93656236477829502, 0.7998128361456462443 ) ) ;
#168958 = CARTESIAN_POINT ( 'NONE',  ( 1.411079811451225074, -1.634442866182721277, 1.270590680402396311 ) ) ;
#168960 = CARTESIAN_POINT ( 'NONE',  ( 0.6823417656249882723, -0.01145833299191073573, -1.181850606188749264 ) ) ;
#168959 = SURFACE_STYLE_USAGE ( .BOTH. , #105056 ) ;
#168962 = EDGE_LOOP ( 'NONE', ( #855, #22619, #2707, #8315 ) ) ;
#168961 = CARTESIAN_POINT ( 'NONE',  ( 4.196076301648347773, 1.450992468586336459, 1.681961854464069983 ) ) ;
#168963 = CARTESIAN_POINT ( 'NONE',  ( 3.305630555216050759, 1.456526447221625276, -1.778376517212407748 ) ) ;
#168964 = CARTESIAN_POINT ( 'NONE',  ( 7.605760987586388744, 11.81721221891873697, 1.040834085586084257E-14 ) ) ;
#168966 = CARTESIAN_POINT ( 'NONE',  ( 3.285556943750000514, -2.763541666188707335, 1.896917185911906500 ) ) ;
#168965 = CARTESIAN_POINT ( 'NONE',  ( 3.984117037569365305, 5.741498858621315371, 1.599625672291261402 ) ) ;
#168967 = EDGE_CURVE ( 'NONE', #77536, #191870, #27829, .T. ) ;
#168968 = DIRECTION ( 'NONE',  ( 0.000000000000000000, 1.000000000000000000, 0.000000000000000000 ) ) ;
#168969 = CARTESIAN_POINT ( 'NONE',  ( 6.609000000000038177, 0.002801690667396730672, 2.000160786441218530 ) ) ;
#168970 = ORIENTED_EDGE ( 'NONE', *, *, #211914, .T. ) ;
#168971 = CARTESIAN_POINT ( 'NONE',  ( -0.2663167167779803557, -9.037303891206464712, 9.496500708127756596 ) ) ;
#168972 = EDGE_CURVE ( 'NONE', #144836, #199252, #35229, .T. ) ;
#168973 = CARTESIAN_POINT ( 'NONE',  ( 3.340010735810138520, -1.142844047782382466, -1.533173144288489276 ) ) ;
#168974 = CARTESIAN_POINT ( 'NONE',  ( -0.4702976403610291678, 6.650664745223592966, -3.344716071613587971 ) ) ;
#168975 = CARTESIAN_POINT ( 'NONE',  ( 4.278129899785966472, -0.9921777787025712891, 1.410595609005516504 ) ) ;
#168976 = CARTESIAN_POINT ( 'NONE',  ( 3.960172920142067898, -1.157100329752266621, 1.651342637023434090 ) ) ;
#168977 =( BOUNDED_SURFACE ( )  B_SPLINE_SURFACE ( 3, 2, ( 
 ( #151894, #119447, #154025 ),
 ( #18666, #54391, #55450 ),
 ( #3469, #38139, #155092 ),
 ( #186508, #56524, #121602 ),
 ( #22922, #170258, #187574 ),
 ( #53315, #70601, #37055 ),
 ( #72755, #169196, #136715 ),
 ( #184366, #20789, #39199 ) ),
 .UNSPECIFIED., .F., .F., .T. ) 
 B_SPLINE_SURFACE_WITH_KNOTS ( ( 4, 2, 2, 4 ),
 ( 3, 3 ),
 ( 5.421010862427522170E-20, 0.0004401918256853566084, 0.0006602877385280349126, 0.0008803836513707132168 ),
 ( 0.000000000000000000, 1.000000000000000000 ),
 .UNSPECIFIED. ) 
 GEOMETRIC_REPRESENTATION_ITEM ( )  RATIONAL_B_SPLINE_SURFACE ( (
 ( 1.000000000000000000, 0.6787756258918292707, 1.000000000000000000),
 ( 1.000000000000000000, 0.6284487096097822745, 1.000000000000000000),
 ( 1.000000000000000000, 0.5704014816686249212, 1.000000000000000000),
 ( 1.000000000000000000, 0.4882303283128048288, 1.000000000000000000),
 ( 1.000000000000000000, 0.4617370933884766271, 1.000000000000000000),
 ( 1.000000000000000000, 0.4222438920366224369, 1.000000000000000000),
 ( 1.000000000000000000, 0.4105126989450484376, 1.000000000000000000),
 ( 1.000000000000000000, 0.4127341956165116454, 1.000000000000000000) ) ) 
 REPRESENTATION_ITEM ( '' )  SURFACE ( )  );
#168978 = CARTESIAN_POINT ( 'NONE',  ( 4.114144448104863017, 0.1132377192244668207, 2.296027709189680799 ) ) ;
#168979 = CARTESIAN_POINT ( 'NONE',  ( 11.52463353791760703, 11.37999999999998302, 3.346594096177640587 ) ) ;
#168980 = CARTESIAN_POINT ( 'NONE',  ( 6.639294477394681593, -1.882217795646949687, 0.9450163710809048601 ) ) ;
#168981 = CARTESIAN_POINT ( 'NONE',  ( -4.828112100242279325, 8.646898193675708555, -0.7216878364870338292 ) ) ;
#168982 = CARTESIAN_POINT ( 'NONE',  ( 4.376060336092471026, -1.020005645217741064, 1.445989269263460386 ) ) ;
#168984 = CARTESIAN_POINT ( 'NONE',  ( 0.3930492761001015967, 1.902410075555853064, -1.278529456123769892 ) ) ;
#168983 = CARTESIAN_POINT ( 'NONE',  ( 7.212011367826596242, 7.378711115411311638, 0.000000000000000000 ) ) ;
#168985 = CARTESIAN_POINT ( 'NONE',  ( 6.492148756324659153, -0.4961259030743305209, -1.772972609911625419 ) ) ;
#168986 = CARTESIAN_POINT ( 'NONE',  ( -6.420668264523499147, 9.648474187656182366, 1.199719254218452935 ) ) ;
#168987 = STYLED_ITEM ( 'NONE', ( #80926 ), #39677 ) ;
#168988 = CARTESIAN_POINT ( 'NONE',  ( 6.052700813158568671, -1.877759139263988075, -1.129571069393126459 ) ) ;
#168989 = CARTESIAN_POINT ( 'NONE',  ( -4.492547798081878874, 6.334668079219206049, 1.599625672291263179 ) ) ;
#168990 = CARTESIAN_POINT ( 'NONE',  ( 1.360316468750003782, -0.1822916663252708847, -0.7853790794158961308 ) ) ;
#168991 = CARTESIAN_POINT ( 'NONE',  ( 9.499668754385636404, -7.473374494045003757, 0.07933194154488391880 ) ) ;
#168992 = CARTESIAN_POINT ( 'NONE',  ( 0.4148109920584437948, 0.8315006815404235585, 2.005833495578440928 ) ) ;
#168993 = CARTESIAN_POINT ( 'NONE',  ( 0.7785302072789467287, -0.4946362931835950327, -1.954778448132548752 ) ) ;
#168994 = CARTESIAN_POINT ( 'NONE',  ( 0.6823417656249917140, 5.342708333674749177, 1.181850606188765695 ) ) ;
#168995 = CARTESIAN_POINT ( 'NONE',  ( 4.600175520841607302, -1.926116679539988885, -0.04579137001822254638 ) ) ;
#168996 = CARTESIAN_POINT ( 'NONE',  ( -8.012344526598182026E-15, 11.79687500034140157, -1.575800808251669460 ) ) ;
#168997 = CARTESIAN_POINT ( 'NONE',  ( 0.6509960782678033686, 2.189857587618043055, 0.3722473809256007793 ) ) ;
#168999 = ORIENTED_EDGE ( 'NONE', *, *, #187563, .T. ) ;
#168998 = DIRECTION ( 'NONE',  ( -0.9999980456341537316, 0.000000000000000000, -0.001977050295958626257 ) ) ;
#169000 = CARTESIAN_POINT ( 'NONE',  ( 4.176167785551761824, 3.974543292672902961, -0.03298406423014330069 ) ) ;
#169001 = DIRECTION ( 'NONE',  ( -0.000000000000000000, -8.546850786086437571E-32, -1.000000000000000000 ) ) ;
#169002 = CARTESIAN_POINT ( 'NONE',  ( 2.517010073631369860, 6.088262185878572375, -0.7998128361456281477 ) ) ;
#169003 = CARTESIAN_POINT ( 'NONE',  ( -1.500000000000001110, 9.052083334016126415, 0.8660254037844418162 ) ) ;
#169004 = DIRECTION ( 'NONE',  ( 0.000000000000000000, 1.000000000000000000, -8.546850786086437571E-32 ) ) ;
#169005 = AXIS2_PLACEMENT_3D ( 'NONE', #60677, #7649, #44456 ) ;
#169006 = CARTESIAN_POINT ( 'NONE',  ( 4.475936636375839051, -1.689578365139619009, -0.4171736215478424881 ) ) ;
#169007 = CARTESIAN_POINT ( 'NONE',  ( 1.926150285298435572, 1.005797860886543660, 1.684270608208485065 ) ) ;
#169009 = CARTESIAN_POINT ( 'NONE',  ( 1.364683531249990311, 3.196875000341416140, 1.214306433183764966E-14 ) ) ;
#169008 = CARTESIAN_POINT ( 'NONE',  ( 5.555090253297246150, 7.504024600312024340, 1.599625672291267398 ) ) ;
#169010 = CARTESIAN_POINT ( 'NONE',  ( -5.906331710381417466, 6.003565991635761989, -0.1321356564752910190 ) ) ;
#169011 = CARTESIAN_POINT ( 'NONE',  ( 0.3970293196923400658, 0.3510089794473401081, 2.032437512258952417 ) ) ;
#169012 = CARTESIAN_POINT ( 'NONE',  ( -7.374745490829552885, 10.69128794168811680, -1.199719254218446718 ) ) ;
#169013 = CARTESIAN_POINT ( 'NONE',  ( -3.565431210269599749, 7.103494145382415859, 0.7216878364870317197 ) ) ;
#169014 = CARTESIAN_POINT ( 'NONE',  ( 5.331267653506235327, -1.592659417495114083, -1.236803018183525449 ) ) ;
#169015 = CARTESIAN_POINT ( 'NONE',  ( 1.165308694782108301, -2.046298710749935079, -0.9655196508330918803 ) ) ;
#169017 = VERTEX_POINT ( 'NONE', #28812 ) ;
#169016 = CARTESIAN_POINT ( 'NONE',  ( -6.663996196316808174, 7.733415969579778171, -1.199719254218446718 ) ) ;
#169018 = CARTESIAN_POINT ( 'NONE',  ( 1.499999999999987121, -0.4645833326505149907, 0.8660254037844524744 ) ) ;
#169019 = CARTESIAN_POINT ( 'NONE',  ( 1.317418832401914930, -1.826178791559311509, 0.4043020138455517554 ) ) ;
#169020 = CARTESIAN_POINT ( 'NONE',  ( 0.4571073982213811893, -1.631979074848688205, -0.5868837268243607408 ) ) ;
#169021 = CARTESIAN_POINT ( 'NONE',  ( 3.773127072069931032, 2.063069237518061705, -0.7396954945804237180 ) ) ;
#169022 = CARTESIAN_POINT ( 'NONE',  ( 6.053837855137599533, 0.6775820993057954933, -2.205875079116952797 ) ) ;
#169023 = CARTESIAN_POINT ( 'NONE',  ( 1.657177242756900926, -1.767118338917167852, -1.060216354352721435 ) ) ;
#169024 = CARTESIAN_POINT ( 'NONE',  ( 3.275267064432846098, 1.232403799581788251, 1.500778006584954749 ) ) ;
#169025 = CARTESIAN_POINT ( 'NONE',  ( -3.755245360860925086, 6.364574773437617239, -1.082531754730548412 ) ) ;
#169026 = CARTESIAN_POINT ( 'NONE',  ( 5.518772846390051612, 1.727975122137341613, 0.7167417953098526029 ) ) ;
#169027 = FILL_AREA_STYLE ('',( #154923 ) ) ;
#169028 = CARTESIAN_POINT ( 'NONE',  ( 5.085717018901939390, 5.105960408239938353, 0.000000000000000000 ) ) ;
#169029 = CARTESIAN_POINT ( 'NONE',  ( -1.360316468750072838, 1.661458333674769694, 0.7853790794158600486 ) ) ;
#169030 = CARTESIAN_POINT ( 'NONE',  ( 4.184220324914634581, 1.621181886760931778, 1.198861198883696799 ) ) ;
#169031 = CARTESIAN_POINT ( 'NONE',  ( -4.731432421044883263, 5.582721248382882528, -1.082531754730543971 ) ) ;
#169032 = CARTESIAN_POINT ( 'NONE',  ( -6.414942957921379474, 7.513130201443591005, -1.199719254218452047 ) ) ;
#169033 = CARTESIAN_POINT ( 'NONE',  ( 9.043452155515161905, 10.50944792197790889, 1.199719254218453823 ) ) ;
#169035 = CARTESIAN_POINT ( 'NONE',  ( -6.785280070212318826, -6.896483513897296191, 6.645879322773594389 ) ) ;
#169034 = CARTESIAN_POINT ( 'NONE',  ( 1.611646134362737959, -1.812087876328593916, 0.2219229778191167957 ) ) ;
#169036 = CARTESIAN_POINT ( 'NONE',  ( -4.111865726694519552, 8.019203457777400956, 0.000000000000000000 ) ) ;
#169037 = CARTESIAN_POINT ( 'NONE',  ( -5.143339171537844479, 7.093924681584510061, 1.599625672291263401 ) ) ;
#169038 = CARTESIAN_POINT ( 'NONE',  ( -10.81659190237994395, 5.544392656652913587, 6.534142543513654644 ) ) ;
#169039 = ORIENTED_EDGE ( 'NONE', *, *, #98945, .F. ) ;
#169040 = CARTESIAN_POINT ( 'NONE',  ( -6.251718229232867685, 6.466295153626015590, -0.7216878364870338292 ) ) ;
#169041 = CARTESIAN_POINT ( 'NONE',  ( -1.249999999999964695, 8.500000000000000000, 10.97907099895069294 ) ) ;
#169042 = CARTESIAN_POINT ( 'NONE',  ( -9.378489572351046633, 11.96465713920816043, -1.599625672291263179 ) ) ;
#169043 = CARTESIAN_POINT ( 'NONE',  ( 5.531901104011129000, -1.969946598288346618, 0.4446316349850876759 ) ) ;
#169045 = ORIENTED_EDGE ( 'NONE', *, *, #102286, .T. ) ;
#169044 = CARTESIAN_POINT ( 'NONE',  ( -0.1046615654881309365, -0.1561857951268459388, -2.086345279447648249 ) ) ;
#169046 = CARTESIAN_POINT ( 'NONE',  ( -6.611536185319534908, 7.742488966741438716, 1.199719254218452047 ) ) ;
#169047 = CARTESIAN_POINT ( 'NONE',  ( 4.819033534653518025, 7.709623992816043270, -1.199719254218452047 ) ) ;
#169048 = CARTESIAN_POINT ( 'NONE',  ( 5.313377624208335703, -0.3045090135303843981, 2.038146128872863283 ) ) ;
#169049 = CARTESIAN_POINT ( 'NONE',  ( 4.817029820108094995, 1.034167108704350024, -1.730865207599366240 ) ) ;
#169050 = VERTEX_POINT ( 'NONE', #111193 ) ;
#169051 = ORIENTED_EDGE ( 'NONE', *, *, #120432, .T. ) ;
#169052 = CARTESIAN_POINT ( 'NONE',  ( 3.594580577241007102, 7.345424419493749468, 0.3531702171868136841 ) ) ;
#169053 = CARTESIAN_POINT ( 'NONE',  ( 3.460355519985863548, 5.060167411448709629, 1.599625672291267398 ) ) ;
#169055 = VERTEX_POINT ( 'NONE', #114394 ) ;
#169054 = CARTESIAN_POINT ( 'NONE',  ( -7.957709816578236506, 8.248692638954882028, 0.7998128361456341429 ) ) ;
#169056 = CARTESIAN_POINT ( 'NONE',  ( 4.609415035364720303, 8.472105597856021575, 0.2450749143364742144 ) ) ;
#169057 = CARTESIAN_POINT ( 'NONE',  ( 3.884138610457484653, -0.1511163893381066714, 2.010518618204664154 ) ) ;
#169058 = CARTESIAN_POINT ( 'NONE',  ( 3.310337721246572773, 1.664907390794263531, 0.7863323413084821745 ) ) ;
#169059 = CARTESIAN_POINT ( 'NONE',  ( 1.255262969126037044E-15, -2.000000000000001776, -10.24999999999999822 ) ) ;
#169060 = CARTESIAN_POINT ( 'NONE',  ( 2.649405215588944262, -1.917952202864357414, 1.283049733485057908 ) ) ;
#169061 = CARTESIAN_POINT ( 'NONE',  ( 5.155843554946782703, 9.237177590738404831, -0.7998128361456481317 ) ) ;
#169062 = CARTESIAN_POINT ( 'NONE',  ( 4.850933092205481856, -1.739298515662604405, 1.283314429840809234 ) ) ;
#169063 = CARTESIAN_POINT ( 'NONE',  ( 8.782984583554449998, 9.141236857102018831, 1.040834085586084257E-14 ) ) ;
#169064 = CARTESIAN_POINT ( 'NONE',  ( 0.3978616433950994957, -0.6552777965449173569, -1.828281909955962181 ) ) ;
#169065 = CARTESIAN_POINT ( 'NONE',  ( -4.252453736180621391, 8.112946458852704268, -0.7998128361456281477 ) ) ;
#169066 = CARTESIAN_POINT ( 'NONE',  ( 6.890000000000007674, 7.629137130509070275, 2.600000000000001421 ) ) ;
#169067 = CARTESIAN_POINT ( 'NONE',  ( -0.001123102408844807139, -7.189630408304394926, -9.584291988782274174 ) ) ;
#169068 = CARTESIAN_POINT ( 'NONE',  ( 1.938157646728836614, 1.849873822469105145, 0.2772664081076986475 ) ) ;
#169069 = AXIS2_PLACEMENT_3D ( 'NONE', #90935, #57352, #126698 ) ;
#169070 = CARTESIAN_POINT ( 'NONE',  ( 6.737195113697223903, -1.761045485681483669, 0.8863934713586976155 ) ) ;
#169072 = DIRECTION ( 'NONE',  ( -0.9983585005135561241, 0.000000000000000000, 0.05727394217551147471 ) ) ;
#169071 = CARTESIAN_POINT ( 'NONE',  ( -1.500000000000001332, -1.318749999317178734, 0.000000000000000000 ) ) ;
#169073 = CARTESIAN_POINT ( 'NONE',  ( 1.207977004800918852, -0.5332226995428279714, 2.141375170867452660 ) ) ;
#169074 = VERTEX_POINT ( 'NONE', #209666 ) ;
#169075 = CARTESIAN_POINT ( 'NONE',  ( 4.989037339704528229, 4.922891105851139315, 1.040834085586084257E-14 ) ) ;
#169076 = CARTESIAN_POINT ( 'NONE',  ( 2.855963913973019963, 6.483708332943829866, 0.000000000000000000 ) ) ;
#169077 = CARTESIAN_POINT ( 'NONE',  ( -3.750802052474980108, 7.527686161196117887, 1.040834085586084257E-14 ) ) ;
#169078 = CARTESIAN_POINT ( 'NONE',  ( -8.064677165291199046, -5.223431457505083308, 7.446209719563363194 ) ) ;
#169079 = CARTESIAN_POINT ( 'NONE',  ( 5.752796013432011080, -1.554615333184097059, 1.212288997074702834 ) ) ;
#169080 = CARTESIAN_POINT ( 'NONE',  ( 0.6050338814152752542, -0.7811975584859867094, -2.171474816401474328 ) ) ;
#169081 = CARTESIAN_POINT ( 'NONE',  ( 0.5901948623465642640, 1.011764341257429978, -1.680720577067334354 ) ) ;
#169082 = CARTESIAN_POINT ( 'NONE',  ( 4.065324354713106381, 1.766439233411433163, 1.064669890786486661 ) ) ;
#169083 = CARTESIAN_POINT ( 'NONE',  ( 6.493992391265805075, 6.678671999339316656, 1.040834085586084257E-14 ) ) ;
#169084 = CARTESIAN_POINT ( 'NONE',  ( 7.367930134383754215, 7.560616343061329125, -0.7998128361456341429 ) ) ;
#169085 = ORIENTED_EDGE ( 'NONE', *, *, #127184, .F. ) ;
#169086 = CARTESIAN_POINT ( 'NONE',  ( 7.578644679914706472, 9.864838098032418401, 1.443375672974076540 ) ) ;
#169087 = CARTESIAN_POINT ( 'NONE',  ( -1.364683531250010295, 5.092708333674757171, 0.7879004041258379498 ) ) ;
#169088 = CARTESIAN_POINT ( 'NONE',  ( -4.952079582221279530, 4.885585162322970021, 0.5000114801232704576 ) ) ;
#169089 = CARTESIAN_POINT ( 'NONE',  ( 5.327991180046175224, 5.318337252916401248, -0.7216878364870207285 ) ) ;
#169090 = CARTESIAN_POINT ( 'NONE',  ( 6.795391773274086944, -1.942485666075419060, 0.9701230550103381312 ) ) ;
#169092 = CARTESIAN_POINT ( 'NONE',  ( 5.020983453748395497, -1.746657797055195305, 0.5827527221545365510 ) ) ;
#169091 = CARTESIAN_POINT ( 'NONE',  ( 11.78331023100045627, 11.37999999999998302, 1.799999999999999600 ) ) ;
#169093 = CARTESIAN_POINT ( 'NONE',  ( -4.845788168165207743, 6.628691488484695249, 1.364795842686959526 ) ) ;
#169094 = DIRECTION ( 'NONE',  ( 0.000000000000000000, -0.000000000000000000, 1.000000000000000000 ) ) ;
#169095 = CARTESIAN_POINT ( 'NONE',  ( 0.7900579835180140398, -1.855660487967484951, -0.2351621623290362506 ) ) ;
#169097 = EDGE_CURVE ( 'NONE', #134057, #89282, #146852, .T. ) ;
#169096 = CARTESIAN_POINT ( 'NONE',  ( -4.277165953568806245, 7.474871692096041187, 1.085114461911325101 ) ) ;
#169098 = CARTESIAN_POINT ( 'NONE',  ( -10.89523958697326833, -6.437359833193948333, 0.04208621775142193377 ) ) ;
#169099 = CARTESIAN_POINT ( 'NONE',  ( 5.612152705277200226, 7.484198595525810127, -1.333638438132278559 ) ) ;
#169100 = CIRCLE ( 'NONE', #58397, 1.250000000000000888 ) ;
#169101 = CARTESIAN_POINT ( 'NONE',  ( 0.7680391878876170475, 1.910087531778673187, -0.09433495293535018589 ) ) ;
#169102 = CARTESIAN_POINT ( 'NONE',  ( 1.498528727375374459, 1.449451107477307987, -1.015301706168385998 ) ) ;
#169103 = CARTESIAN_POINT ( 'NONE',  ( 6.059245300855401695, -1.699386736952392285, 1.078915776541150340 ) ) ;
#169105 = CARTESIAN_POINT ( 'NONE',  ( 3.989770193594462722, -1.910233455636681787, 0.1444642847954723808 ) ) ;
#169104 = CARTESIAN_POINT ( 'NONE',  ( -7.831806290188425557, 12.28885777186185990, -0.7998128361456281477 ) ) ;
#169106 = CARTESIAN_POINT ( 'NONE',  ( -0.1409997244345879697, 0.2375178066936211585, -2.034344168881811132 ) ) ;
#169107 = CARTESIAN_POINT ( 'NONE',  ( 4.984792273111487759, 1.884092017856910273, 0.5737924883163454393 ) ) ;
#169109 = ADVANCED_FACE ( 'NONE', ( #178274 ), #127470, .T. ) ;
#169108 = CARTESIAN_POINT ( 'NONE',  ( 6.135022435551370279, 1.886083186425246971, 0.7231739236989165320 ) ) ;
#169110 = CARTESIAN_POINT ( 'NONE',  ( 0.007601003541776819861, -8.259585062615352413, -10.93184718803891187 ) ) ;
#169111 = CARTESIAN_POINT ( 'NONE',  ( 4.364026845288040413, 0.8817440624687390427, 1.649792572839225091 ) ) ;
#169113 = ORIENTED_EDGE ( 'NONE', *, *, #92074, .F. ) ;
#169112 = CARTESIAN_POINT ( 'NONE',  ( 5.813083859329478464, 1.524454967706680319, 0.8070229810451818864 ) ) ;
#169115 = CARTESIAN_POINT ( 'NONE',  ( 3.063779527008311021, 5.557864633942907417, 1.082531754730546636 ) ) ;
#169114 = CARTESIAN_POINT ( 'NONE',  ( 3.703933201646680828, -0.6411959742554216302, 2.111683309420588905 ) ) ;
#169116 = CARTESIAN_POINT ( 'NONE',  ( -1.364683531249997417, 3.571875000341423245, 1.214306433183764966E-14 ) ) ;
#169117 = CARTESIAN_POINT ( 'NONE',  ( 0.3091261446717024630, -1.657722840873154135, 1.227268292441574538 ) ) ;
#169120 = EDGE_CURVE ( 'NONE', #138703, #170885, #202002, .T. ) ;
#169119 = AXIS2_PLACEMENT_3D ( 'NONE', #206387, #55880, #90535 ) ;
#169118 = CARTESIAN_POINT ( 'NONE',  ( 7.447506452608354088, 7.583179037664891098, 0.7998128361456341429 ) ) ;
#169121 = CARTESIAN_POINT ( 'NONE',  ( -8.748035429315585532, 11.22912730566677553, -1.599625672291263179 ) ) ;
#169122 = CARTESIAN_POINT ( 'NONE',  ( -7.090393287529871635, 15.44810098017736166, -9.636374456359583007 ) ) ;
#169123 = CARTESIAN_POINT ( 'NONE',  ( -3.418738334753848029, -0.02680128005874191088, -0.3660903872622625066 ) ) ;
#169124 = CARTESIAN_POINT ( 'NONE',  ( -1.499999999999960254, 7.064371086078064188, 10.89416074946470836 ) ) ;
#169125 = ORIENTED_EDGE ( 'NONE', *, *, #180163, .T. ) ;
#169126 = CARTESIAN_POINT ( 'NONE',  ( 3.684089399883890614, -1.230936008959164996, -1.664559344884769088 ) ) ;
#169127 = CARTESIAN_POINT ( 'NONE',  ( -1.001543065824772872E-14, 4.212500000000023448, 1.732050807568877637 ) ) ;
#169128 = CARTESIAN_POINT ( 'NONE',  ( 6.145923705696426431, 6.064665832934283962, 0.7998128361456341429 ) ) ;
#169129 = CARTESIAN_POINT ( 'NONE',  ( -6.253183873137761140, 7.001293123865100831, 0.9949814792902436089 ) ) ;
#169130 = CARTESIAN_POINT ( 'NONE',  ( 0.5924517288934522119, -1.120073279264972799, 1.680413856445305498 ) ) ;
#169131 = CARTESIAN_POINT ( 'NONE',  ( -0.9999999999999965583, 6.180000000000019256, 1.226552901175238481E-14 ) ) ;
#169133 = CARTESIAN_POINT ( 'NONE',  ( 7.863365906246055914, 10.19701286208565705, -1.443375672974057666 ) ) ;
#169132 = CARTESIAN_POINT ( 'NONE',  ( 0.1747926744264677035, 1.388892567315727744, -2.112808070315982167 ) ) ;
#169134 = CARTESIAN_POINT ( 'NONE',  ( 6.239611212763971793, -1.913511330438378177, -0.6350998681113121380 ) ) ;
#169135 = CARTESIAN_POINT ( 'NONE',  ( 5.454270856000166923, -1.210104932453776039, 1.485173795633880633 ) ) ;
#169136 = CARTESIAN_POINT ( 'NONE',  ( 6.539320575229292665, 2.014857154840712372, 2.506613887083661840 ) ) ;
#169137 = CARTESIAN_POINT ( 'NONE',  ( 4.195009555701286530, 1.760677850468267414, 1.304791629949946019 ) ) ;
#169138 = CARTESIAN_POINT ( 'NONE',  ( -0.7500000000000215383, 3.222916667349487341, 1.299038105676671107 ) ) ;
#169139 = CARTESIAN_POINT ( 'NONE',  ( 2.109489925670060551, 1.480643174185194200, 1.210387159491378650 ) ) ;
#169140 = CARTESIAN_POINT ( 'NONE',  ( -5.440899717785814715, 5.242137847038546461, 0.7998128361456341429 ) ) ;
#169142 = CARTESIAN_POINT ( 'NONE',  ( 3.917943204224906939, 5.594019709727598766, -1.443375672974051449 ) ) ;
#169141 = B_SPLINE_CURVE_WITH_KNOTS ( 'NONE', 3,
 ( #196138, #97585, #45633, #116001, #32557, #96528 ),
 .UNSPECIFIED., .F., .F.,
 ( 4, 2, 4 ),
 ( 0.001490700410107441247, 0.002078801942328945690, 0.002666903474550449699 ),
 .UNSPECIFIED. ) ;
#169144 = CARTESIAN_POINT ( 'NONE',  ( 1.405875298092047698, -1.122519365368032984, -1.674874950958963549 ) ) ;
#169143 = CARTESIAN_POINT ( 'NONE',  ( 3.469446951953614189E-15, 3.300000000000018030, 1.214306433183764966E-14 ) ) ;
#169145 = CARTESIAN_POINT ( 'NONE',  ( -1.364683531250014514, 11.40104166700806410, -0.7879004041258335089 ) ) ;
#169146 = VECTOR ( 'NONE', #208209, 1000.000000000000000 ) ;
#169148 = CARTESIAN_POINT ( 'NONE',  ( -5.306037014901836990, 7.283738832175834510, 1.599625672291263179 ) ) ;
#169147 = CARTESIAN_POINT ( 'NONE',  ( 6.427279137517246888, -1.429865906218323435, -1.660902671979214595 ) ) ;
#169150 = ORIENTED_EDGE ( 'NONE', *, *, #68660, .F. ) ;
#169149 = CARTESIAN_POINT ( 'NONE',  ( 2.854212618329458717, 0.5792176767629078071, 1.624745991979989812 ) ) ;
#169151 = CARTESIAN_POINT ( 'NONE',  ( -0.1399997263889594112, -0.002789056014654289761, -2.000146600338557956 ) ) ;
#169152 = CARTESIAN_POINT ( 'NONE',  ( 6.877010230629674759, 9.046264573866535486, 1.599625672291281386 ) ) ;
#169153 = CARTESIAN_POINT ( 'NONE',  ( 5.443762371086860341, 6.309809840144842141, 1.199719254218462483 ) ) ;
#169154 = CARTESIAN_POINT ( 'NONE',  ( 0.07735805125222164347, -0.0005418671161615787497, -2.088975025666544916 ) ) ;
#169155 = CARTESIAN_POINT ( 'NONE',  ( 1.785527960060459440, -1.848404783191982315, 0.6579185095809261252 ) ) ;
#169156 = PRESENTATION_STYLE_ASSIGNMENT (( #54352 ) ) ;
#169157 = CARTESIAN_POINT ( 'NONE',  ( 5.379888026524302980, 5.170957540566797128, -0.7998128361456211532 ) ) ;
#169158 = CARTESIAN_POINT ( 'NONE',  ( 0.07933194154487524519, -9.746166700180788567, 9.499668754385634628 ) ) ;
#169159 = VERTEX_POINT ( 'NONE', #62370 ) ;
#169160 = CARTESIAN_POINT ( 'NONE',  ( -2.331034670843834533E-15, -6.681160345272283863, 10.14529669463342998 ) ) ;
#169161 = ORIENTED_EDGE ( 'NONE', *, *, #21226, .F. ) ;
#169162 = CARTESIAN_POINT ( 'NONE',  ( 4.230988290566616072, 1.657980831523006460, 0.7301630082575115699 ) ) ;
#169163 = VERTEX_POINT ( 'NONE', #112260 ) ;
#169164 = CARTESIAN_POINT ( 'NONE',  ( 10.24048609702354717, 10.84165528948263457, -0.7998128361456281477 ) ) ;
#169165 = CARTESIAN_POINT ( 'NONE',  ( 5.083381250481017410, 4.895309311841474553, 0.7998128361456352531 ) ) ;
#169166 = CARTESIAN_POINT ( 'NONE',  ( 4.881432045509231266, 0.1721252788823707247, -1.803262557370821417 ) ) ;
#169167 = CARTESIAN_POINT ( 'NONE',  ( 7.634649897826745857, 8.079715433652276957, 0.7216878364870267237 ) ) ;
#169168 = CIRCLE ( 'NONE', #182918, 0.5000000000000008882 ) ;
#169169 = DIRECTION ( 'NONE',  ( 0.000000000000000000, 0.000000000000000000, 1.000000000000000000 ) ) ;
#169170 = CARTESIAN_POINT ( 'NONE',  ( 5.656792095876843618, 6.122768675584825182, -0.7810860850652520115 ) ) ;
#169172 = CARTESIAN_POINT ( 'NONE',  ( 9.459838494033030898, 12.05956421450382088, 1.599625672291281386 ) ) ;
#169171 = CARTESIAN_POINT ( 'NONE',  ( 4.650750022344506185, -0.4068995778509130190, -1.815856201304208550 ) ) ;
#169173 = CARTESIAN_POINT ( 'NONE',  ( 2.302218516519896507, 1.249579790052034456, -1.452036884154449314 ) ) ;
#169174 = DIRECTION ( 'NONE',  ( 0.000000000000000000, 0.000000000000000000, 1.000000000000000000 ) ) ;
#169175 = CARTESIAN_POINT ( 'NONE',  ( -10.97409330344778944, 4.894225957061862253, -4.351021568302368969 ) ) ;
#169176 = CARTESIAN_POINT ( 'NONE',  ( -7.013428937081434000, 5.939655416065874327, -2.436399677959149468 ) ) ;
#169177 = CARTESIAN_POINT ( 'NONE',  ( 6.346625304528514810, 6.577020074804287297, 0.000000000000000000 ) ) ;
#169178 = CARTESIAN_POINT ( 'NONE',  ( 5.477130870240836558, 9.333810415348903433, -0.7216878364870267237 ) ) ;
#169179 = CARTESIAN_POINT ( 'NONE',  ( -3.440018289565379028, 5.036440642624797626, 1.599625672291267398 ) ) ;
#169180 = CARTESIAN_POINT ( 'NONE',  ( 0.09294085500742563233, -0.4768749645070144982, -2.116232079886640971 ) ) ;
#169181 = CARTESIAN_POINT ( 'NONE',  ( -6.611536185319534908, 7.742488966741438716, 1.199719254218452047 ) ) ;
#169182 = CARTESIAN_POINT ( 'NONE',  ( 1.587951679898065294, -2.080713178594826296, -0.2033740637906420179 ) ) ;
#169183 = CARTESIAN_POINT ( 'NONE',  ( 6.391743074199808916, 6.421731439513382433, -0.7998128361456481317 ) ) ;
#169184 = CARTESIAN_POINT ( 'NONE',  ( 5.965835030274156736, 1.897794126051439045, -0.3298099971670089281 ) ) ;
#169185 = CARTESIAN_POINT ( 'NONE',  ( -5.253948220495577637, 6.088359997788290734, 1.199719254218450271 ) ) ;
#169186 = CARTESIAN_POINT ( 'NONE',  ( 2.608196206841297826, -0.6965810133783244540, -1.687657492251873226 ) ) ;
#169187 = EDGE_CURVE ( 'NONE', #105939, #36876, #34772, .T. ) ;
#169188 = CARTESIAN_POINT ( 'NONE',  ( -6.518203450479854943, 5.167241622962447600, 2.437504649502888920 ) ) ;
#169189 = CARTESIAN_POINT ( 'NONE',  ( 2.355592738034977263, -1.419685808644566949, -1.281520755053264571 ) ) ;
#169190 = CARTESIAN_POINT ( 'NONE',  ( 1.644903635585378554, -0.2856866470503526823, -1.948579891484893079 ) ) ;
#169191 = CARTESIAN_POINT ( 'NONE',  ( 4.071774441262452804, -1.115447612638842401, 1.589602391900000411 ) ) ;
#169192 = ORIENTED_EDGE ( 'NONE', *, *, #168663, .T. ) ;
#169193 = CARTESIAN_POINT ( 'NONE',  ( -6.291865805193673111, 9.498204651771386509, -1.199719254218452047 ) ) ;
#169195 = CARTESIAN_POINT ( 'NONE',  ( 4.025719079702368752, -0.3592959752154977204, 2.089770972018199835 ) ) ;
#169194 = CARTESIAN_POINT ( 'NONE',  ( 3.410758162289653672, 6.136912401716668519, -1.199719254218453823 ) ) ;
#169196 = CARTESIAN_POINT ( 'NONE',  ( 6.429544252029160134, -6.709867743870938206, 6.981856502303465106 ) ) ;
#169197 = CARTESIAN_POINT ( 'NONE',  ( 7.736899214892750010, 12.17813285068358020, 1.040834085586084257E-14 ) ) ;
#169198 = CARTESIAN_POINT ( 'NONE',  ( 5.834672162164848075, 6.194663582219344988, 0.9174233710642684114 ) ) ;
#169199 = CARTESIAN_POINT ( 'NONE',  ( -10.99126615174920651, -5.166862915010145052, 0.4382560683119391398 ) ) ;
#169200 = ORIENTED_EDGE ( 'NONE', *, *, #161158, .T. ) ;
#169201 = CARTESIAN_POINT ( 'NONE',  ( 5.338878628731272613, 9.450718510153643948, -0.7998128361456481317 ) ) ;
#169202 = CARTESIAN_POINT ( 'NONE',  ( 11.86685672517501899, 12.49081082140188670, -1.056525322636012065 ) ) ;
#169204 = ADVANCED_FACE ( 'NONE', ( #95968 ), #197688, .T. ) ;
#169203 = CARTESIAN_POINT ( 'NONE',  ( 3.422296110638740174, 1.157362003623555236, -1.411967061744797691 ) ) ;
#169205 = CARTESIAN_POINT ( 'NONE',  ( 1.284279953904121641, 3.077889714876734573, -0.7749999999999892530 ) ) ;
#169206 = CARTESIAN_POINT ( 'NONE',  ( -9.653042183249972652, 10.36423008998754192, -0.7216878364870267237 ) ) ;
#169207 = AXIS2_PLACEMENT_3D ( 'NONE', #116025, #65063, #132253 ) ;
#169208 = CARTESIAN_POINT ( 'NONE',  ( -5.274058703912462676, 7.771439464937274444, 1.305864451146660388 ) ) ;
#169209 = DIRECTION ( 'NONE',  ( -8.638326563840814399E-31, 0.000000000000000000, -1.000000000000000000 ) ) ;
#169210 = CARTESIAN_POINT ( 'NONE',  ( 4.838664814796108438, 0.3202261158844340594, 1.842872994462002367 ) ) ;
#169211 = CARTESIAN_POINT ( 'NONE',  ( 6.252281394196331554, 10.44607872653774372, 1.040834085586084257E-14 ) ) ;
#169212 = CARTESIAN_POINT ( 'NONE',  ( 2.174328269389655066, -1.185172859381509625, 1.518732482018339436 ) ) ;
#169213 = DIRECTION ( 'NONE',  ( 0.6507913734559658270, -0.7592566023652989049, 0.000000000000000000 ) ) ;
#169214 = CARTESIAN_POINT ( 'NONE',  ( 2.842405760359353106, 6.467890487061221272, -0.7998128361456291469 ) ) ;
#169215 = CARTESIAN_POINT ( 'NONE',  ( 0.6823417656249934904, 8.755208333674733723, 1.181850606188764807 ) ) ;
#169216 = CARTESIAN_POINT ( 'NONE',  ( -6.575868197828002693, 7.630599971342813426, 1.199719254218450271 ) ) ;
#169217 = CARTESIAN_POINT ( 'NONE',  ( 3.662674053986138656, 7.424870162959149589, 0.7998128361456321445 ) ) ;
#169218 = CARTESIAN_POINT ( 'NONE',  ( -5.438229012412903352, 6.477593614970734492, -1.082531754730549967 ) ) ;
#169219 = CARTESIAN_POINT ( 'NONE',  ( 0.9138395863287234189, -1.346417975848941406, -1.633941036375158973 ) ) ;
#169220 = CARTESIAN_POINT ( 'NONE',  ( 9.083072846151447166, 12.68433652289702884, 1.199719254218450271 ) ) ;
#169221 = CARTESIAN_POINT ( 'NONE',  ( -6.661184041420952440, 7.849261790823902629, 6.773376349083140013 ) ) ;
#169222 = CARTESIAN_POINT ( 'NONE',  ( 6.016483110937820733, 0.8336820848486149460, 1.895147399281302825 ) ) ;
#169224 = CARTESIAN_POINT ( 'NONE',  ( 4.037917249208685000, 7.776151245443112536, -0.4343759663945709892 ) ) ;
#169223 = CARTESIAN_POINT ( 'NONE',  ( 0.5031362391596030381, -1.832460416942282011, 0.1798594046882526221 ) ) ;
#169225 = CARTESIAN_POINT ( 'NONE',  ( 0.2460673368967214447, -2.230335335914147343, -0.5547215216719133535 ) ) ;
#169226 = CARTESIAN_POINT ( 'NONE',  ( 5.883875478650832491, 6.927238148923188454, -1.082531754730543083 ) ) ;
#169228 = FILL_AREA_STYLE_COLOUR ( '', #170789 ) ;
#169227 = CARTESIAN_POINT ( 'NONE',  ( 4.340018570150304456, 6.156717313299049366, -1.443375672974068769 ) ) ;
#169229 = CARTESIAN_POINT ( 'NONE',  ( 1.922231132759700589, 1.317440867170904362, -1.875679006090027690 ) ) ;
#169231 = EDGE_CURVE ( 'NONE', #176800, #137099, #166203, .T. ) ;
#169230 = CARTESIAN_POINT ( 'NONE',  ( -0.01492019832703625482, -9.953727901176275594, -9.579640682430666132 ) ) ;
#169232 = CARTESIAN_POINT ( 'NONE',  ( -6.557303570864871034, 7.679217583210999010, -1.199719254218452047 ) ) ;
#169233 = CARTESIAN_POINT ( 'NONE',  ( 6.404245030721173570, 1.437354257190478490, -1.306004427266238777 ) ) ;
#169234 = ORIENTED_EDGE ( 'NONE', *, *, #40097, .T. ) ;
#169235 = CARTESIAN_POINT ( 'NONE',  ( 9.395437264145964917, 10.06369101769952934, -0.7216878364870257245 ) ) ;
#169236 = ADVANCED_FACE ( 'NONE', ( #196642 ), #81819, .F. ) ;
#169237 = VERTEX_POINT ( 'NONE', #159874 ) ;
#169238 = CARTESIAN_POINT ( 'NONE',  ( 6.345967646908174054, -1.254484226688237447, -1.443505786478386899 ) ) ;
#169239 = CARTESIAN_POINT ( 'NONE',  ( 6.262907710099242742, -0.1037740067610822270, -2.014008436551452785 ) ) ;
#169241 = DIRECTION ( 'NONE',  ( 1.000000000000000000, 0.000000000000000000, 0.000000000000000000 ) ) ;
#169240 = CARTESIAN_POINT ( 'NONE',  ( -9.203287345578106127, 9.631590079462940324, 0.7998128361456462443 ) ) ;
#169242 = CARTESIAN_POINT ( 'NONE',  ( -9.587704862635016312, 4.026159954882873926, 6.671158199369250141 ) ) ;
#169244 = CARTESIAN_POINT ( 'NONE',  ( 1.217257651388839346, -1.727774110360464244, 0.3828142623626716867 ) ) ;
#169243 = CARTESIAN_POINT ( 'NONE',  ( 2.554727279587006183, -1.819456544085126026, -1.029573916123826427 ) ) ;
#169245 = CARTESIAN_POINT ( 'NONE',  ( -1.734723475976807094E-15, 2.999999999999988898, -6.938893903907228378E-15 ) ) ;
#169247 = CARTESIAN_POINT ( 'NONE',  ( 4.224787546089771695, 0.1105535957067731723, 2.289718640476182898 ) ) ;
#169246 = CARTESIAN_POINT ( 'NONE',  ( 2.925527285498711549, 6.635141943048991742, 0.7998128361456281477 ) ) ;
#169248 = CARTESIAN_POINT ( 'NONE',  ( 3.046520963529773862, -1.423092868940859956, -1.001465238821471315 ) ) ;
#169249 = CARTESIAN_POINT ( 'NONE',  ( 4.376584659113025744, 4.000436945253625254, 0.7998128361456341429 ) ) ;
#169250 = ADVANCED_FACE ( 'NONE', ( #11479 ), #100483, .T. ) ;
#169251 = MECHANICAL_DESIGN_GEOMETRIC_PRESENTATION_REPRESENTATION (  '', ( #68881 ), #124357 ) ;
#169252 = CARTESIAN_POINT ( 'NONE',  ( 3.716313722480235615, 7.557726119527409914, -0.5394532061484574870 ) ) ;
#169253 = CARTESIAN_POINT ( 'NONE',  ( 3.163173391212137808, -0.5009769021222918450, -1.659887746298273514 ) ) ;
#169254 = CARTESIAN_POINT ( 'NONE',  ( 3.754478802441584495, -2.168521383071635000, -0.1100146688530565936 ) ) ;
#169255 = CARTESIAN_POINT ( 'NONE',  ( 3.323720213644492993, 7.029424015893889433, 1.040834085586084257E-14 ) ) ;
#169256 = CARTESIAN_POINT ( 'NONE',  ( 4.171111447311355747, 1.799123655847803205, -0.9110083886025857058 ) ) ;
#169257 = CARTESIAN_POINT ( 'NONE',  ( 1.656250000000001554, -1.895863743164051485, 0.7852924748300756930 ) ) ;
#169258 = CARTESIAN_POINT ( 'NONE',  ( 1.499999999999989120, 2.785416667349484676, 0.8660254037844524744 ) ) ;
#169259 = CARTESIAN_POINT ( 'NONE',  ( 1.746969779936607292, -1.628684531152933657, 1.028491977540356705 ) ) ;
#169260 = CARTESIAN_POINT ( 'NONE',  ( 1.500000000000001332, 8.406250000682797818, 0.000000000000000000 ) ) ;
#169261 = CARTESIAN_POINT ( 'NONE',  ( 4.148835382215973588, 2.178989060337086503, 0.4312644480095380040 ) ) ;
#169262 = VERTEX_POINT ( 'NONE', #135907 ) ;
#169263 = CARTESIAN_POINT ( 'NONE',  ( -0.1106856583840877956, 1.350702755748961481, -2.249207804202685956 ) ) ;
#169264 = CARTESIAN_POINT ( 'NONE',  ( 0.7499999999999885647, 1.316666666666688190, -1.299038105676652899 ) ) ;
#169265 = CARTESIAN_POINT ( 'NONE',  ( 7.772902139336337335, 7.962807338847539107, 0.7998128361456341429 ) ) ;
#169266 = CARTESIAN_POINT ( 'NONE',  ( 3.999292125906899198, 6.649295999324608353, 1.082531754730558626 ) ) ;
#169267 = CARTESIAN_POINT ( 'NONE',  ( 0.000000000000000000, -1.946874999522044014, -3.793834371823813445 ) ) ;
#169268 = CARTESIAN_POINT ( 'NONE',  ( 1.102519259163890153, -0.9942956747860592914, 1.986404433118430291 ) ) ;
#169269 = CARTESIAN_POINT ( 'NONE',  ( 5.494571831323358246, 1.932540981948445147, 0.3370517209014682325 ) ) ;
#169270 = CARTESIAN_POINT ( 'NONE',  ( 7.456621297836067086, 10.68284669990868174, 1.082531754730558626 ) ) ;
#169271 = CARTESIAN_POINT ( 'NONE',  ( 0.000000000000000000, -4.000000000000003553, -5.799999999999999822 ) ) ;
#169272 = CARTESIAN_POINT ( 'NONE',  ( 6.608658273995139609, 1.683185115790312603, -1.511970481837302760 ) ) ;
#169273 = CARTESIAN_POINT ( 'NONE',  ( 5.740951700743842423, 5.662474837148078421, -0.7998128361456481317 ) ) ;
#169274 = CARTESIAN_POINT ( 'NONE',  ( -4.177320726786315497, 7.887641591310407208, -0.7216878364870458196 ) ) ;
#169275 = CARTESIAN_POINT ( 'NONE',  ( 3.648931631147700472, -0.3995851234466942792, -2.023444851274053491 ) ) ;
#169276 = CARTESIAN_POINT ( 'NONE',  ( -3.581325132304157943, 7.329963087663487364, -0.7998128361456281477 ) ) ;
#169277 = CARTESIAN_POINT ( 'NONE',  ( -1.500000000000013101, 3.660416667349488673, -0.8660254037844313801 ) ) ;
#169278 = CARTESIAN_POINT ( 'NONE',  ( -1.364683531250014514, -1.011458332991911568, -0.7879004041258359514 ) ) ;
#169279 = CARTESIAN_POINT ( 'NONE',  ( 4.850782132498069998, -1.503350029756752804, 1.112868480285071460 ) ) ;
#169280 = CARTESIAN_POINT ( 'NONE',  ( 4.096141260758720648, -0.2909454306243773325, 1.709365352543093186 ) ) ;
#169281 = CARTESIAN_POINT ( 'NONE',  ( 3.544249451937312667, -1.420498570261208959, 1.005328601869423633 ) ) ;
#169282 = CARTESIAN_POINT ( 'NONE',  ( 0.8379086502938500880, 0.9226890658239239595, -2.098657079483890353 ) ) ;
#169283 = CARTESIAN_POINT ( 'NONE',  ( -1.201851678989727383E-14, 3.384375000341421469, 1.575800808251672791 ) ) ;
#169284 = CARTESIAN_POINT ( 'NONE',  ( 5.653879428721274358, 0.8482012749469816093, 1.911158475179574046 ) ) ;
#169285 = CARTESIAN_POINT ( 'NONE',  ( 6.316353394666050391, 1.812894500769960837, 0.6965700268309078513 ) ) ;
#169286 = DIRECTION ( 'NONE',  ( -1.000000000000000000, 7.387867266669436732E-31, 0.000000000000000000 ) ) ;
#169287 = PRESENTATION_STYLE_ASSIGNMENT (( #172504 ) ) ;
#169288 = CARTESIAN_POINT ( 'NONE',  ( 2.022111496571117772, -1.799922141918413487, 0.9091460122201827643 ) ) ;
#169289 = CARTESIAN_POINT ( 'NONE',  ( 0.1292129718690297469, -2.001788180159810970, 0.8922102942980970619 ) ) ;
#169290 = CARTESIAN_POINT ( 'NONE',  ( 8.523031442321446605, 14.76712986476217715, -9.394111251778250349 ) ) ;
#169291 = CARTESIAN_POINT ( 'NONE',  ( -8.474009703741204547, 9.845098394908269768, -1.199719254218446718 ) ) ;
#169292 = CARTESIAN_POINT ( 'NONE',  ( 6.844168616800228477, 6.879284895888727824, -0.7998128361456281477 ) ) ;
#169293 = CARTESIAN_POINT ( 'NONE',  ( 2.807414684038778141, 1.817529592918063708, -1.092056846721880969 ) ) ;
#169294 = CARTESIAN_POINT ( 'NONE',  ( 1.364683531249986537, -1.136458332991912235, 0.7879004041258500513 ) ) ;
#169295 = CARTESIAN_POINT ( 'NONE',  ( 4.969292227364340953, 0.1756445257206709631, -1.817221496977147854 ) ) ;
#169296 = ADVANCED_FACE ( 'NONE', ( #21046 ), #184630, .T. ) ;
#169297 = ORIENTED_EDGE ( 'NONE', *, *, #12024, .F. ) ;
#169298 = CARTESIAN_POINT ( 'NONE',  ( -6.149505192250180663, 9.332117270003974951, -1.199719254218452047 ) ) ;
#169299 = CARTESIAN_POINT ( 'NONE',  ( 0.000000000000000000, 7.999999999999992895, -8.500000000000000000 ) ) ;
#169300 = CARTESIAN_POINT ( 'NONE',  ( 7.661766205054107992, 8.111351125417501251, -0.7216878364870317197 ) ) ;
#169301 = CARTESIAN_POINT ( 'NONE',  ( 3.475000000000000533, -4.010416665710750728, 2.006292185433948827 ) ) ;
#169302 = CARTESIAN_POINT ( 'NONE',  ( -6.723954117373590833, 9.932031339322813679, -1.199719254218440723 ) ) ;
#169303 = CARTESIAN_POINT ( 'NONE',  ( 2.215108757275308982, 1.619595947845490436, -1.206587912388109141 ) ) ;
#169304 = CARTESIAN_POINT ( 'NONE',  ( 0.1476710321905516377, -1.628112296142746995, -1.335496995165935674 ) ) ;
#169305 = CARTESIAN_POINT ( 'NONE',  ( 10.40318394038753702, 11.03146944007395724, -0.7998128361456281477 ) ) ;
#169306 = CARTESIAN_POINT ( 'NONE',  ( 3.766312297878508630, -0.7504043340197141809, -1.703115836376113634 ) ) ;
#169307 = CARTESIAN_POINT ( 'NONE',  ( 8.052653171512838881, 11.48218023581863001, -1.199719254218446718 ) ) ;
#169308 = LINE ( 'NONE', #185542, #19394 ) ;
#169309 = EDGE_LOOP ( 'NONE', ( #23311, #10938, #150687, #26930, #203145, #95490, #1804, #186469, #142613, #134076, #65242, #56993, #198336, #60845, #159755, #205108, #21021, #114919, #15006, #132790, #137445, #32134, #136043, #14804, #44784, #8974 ) ) ;
#169310 = CARTESIAN_POINT ( 'NONE',  ( -3.567766978690493307, 7.314145241780881435, 1.040834085586084257E-14 ) ) ;
#169311 = CARTESIAN_POINT ( 'NONE',  ( -7.995557903757128493, 10.35123685918189729, 1.599625672291295375 ) ) ;
#169312 = CARTESIAN_POINT ( 'NONE',  ( 4.881388680972560401, 1.702354803207173584, -0.6601141376258444771 ) ) ;
#169314 = CARTESIAN_POINT ( 'NONE',  ( -3.978769281187482854, 7.845005453061479450, 0.1301786893823601021 ) ) ;
#169313 = CARTESIAN_POINT ( 'NONE',  ( -7.761116589180078407, 8.019333873657032541, 0.000000000000000000 ) ) ;
#169315 = CARTESIAN_POINT ( 'NONE',  ( 5.120401779693986910, 7.917229619699595489, -1.217862772375446712 ) ) ;
#169316 = CARTESIAN_POINT ( 'NONE',  ( 1.282125424323858898, -1.693001012030776353, 0.3732380902255887367 ) ) ;
#169317 = CARTESIAN_POINT ( 'NONE',  ( 0.6908507670086707630, -0.6304954947415147837, 1.622297741125192427 ) ) ;
#169319 = CARTESIAN_POINT ( 'NONE',  ( 6.629573927402440781, 10.67832731537079383, 1.040834085586084257E-14 ) ) ;
#169318 = CARTESIAN_POINT ( 'NONE',  ( 5.039818274408326637, -1.629004898613298558, -1.634814698366208185 ) ) ;
#169320 = CARTESIAN_POINT ( 'NONE',  ( 6.349632722739280588, 6.936441728539081808, -0.8798346732450362806 ) ) ;
#169321 = CARTESIAN_POINT ( 'NONE',  ( 1.054063116485728813, 2.058546115662110765, -0.09824037785954514712 ) ) ;
#169322 = CARTESIAN_POINT ( 'NONE',  ( 6.006425746053997372, 6.966250444273174303, -1.199719254218445830 ) ) ;
#169323 = VECTOR ( 'NONE', #182802, 1000.000000000000114 ) ;
#169324 = CARTESIAN_POINT ( 'NONE',  ( 0.2630457479233569984, -2.015603748724136945, -0.05229424383911692592 ) ) ;
#169325 = DIRECTION ( 'NONE',  ( 0.000000000000000000, -1.000000000000000000, 0.000000000000000000 ) ) ;
#169326 = CARTESIAN_POINT ( 'NONE',  ( -5.427006627220116286, 9.553534508390610469, -0.7998128361456362523 ) ) ;
#169327 = CARTESIAN_POINT ( 'NONE',  ( 6.631728656526095556, -1.223761959379562114, -1.414937998750566361 ) ) ;
#169328 = B_SPLINE_CURVE_WITH_KNOTS ( 'NONE', 3,
 ( #52875, #103775, #153588, #167693, #36615, #168759 ),
 .UNSPECIFIED., .F., .F.,
 ( 4, 2, 4 ),
 ( 0.001616326159039268694, 0.001719602896561273769, 0.001822879634083278844 ),
 .UNSPECIFIED. ) ;
#169330 = CARTESIAN_POINT ( 'NONE',  ( -4.995253251992230581, 4.792493313604505367, 0.000000000000000000 ) ) ;
#169329 = CARTESIAN_POINT ( 'NONE',  ( 3.586107075002854305, 1.066394011600999780, 1.587261316105821551 ) ) ;
#169331 = CARTESIAN_POINT ( 'NONE',  ( 4.617920694193921705, -2.164688156338661962, 0.4286357439418769788 ) ) ;
#169332 = CARTESIAN_POINT ( 'NONE',  ( 1.224999999999992983, 1.458333334016138849, -0.7072540797572817173 ) ) ;
#169333 = CARTESIAN_POINT ( 'NONE',  ( -0.4500000000000545231, 4.000000000000003553, -0.8338124244296075682 ) ) ;
#169334 = CARTESIAN_POINT ( 'NONE',  ( 5.519577934094864524, 5.612131475965050242, 0.7216878364870328300 ) ) ;
#169335 = CARTESIAN_POINT ( 'NONE',  ( -4.787437638956935082, 6.678706226906775179, -1.443375672974066548 ) ) ;
#169336 = CARTESIAN_POINT ( 'NONE',  ( 5.936213163351176547, -1.177816969253571155, -1.763093882214488817 ) ) ;
#169337 = CARTESIAN_POINT ( 'NONE',  ( 3.698509654486553000, -2.304784958540738060, -0.1161927354758583580 ) ) ;
#169338 = CARTESIAN_POINT ( 'NONE',  ( 3.543363863352413823, 1.774678991803163575, -0.8365776047038612218 ) ) ;
#169339 =( NAMED_UNIT ( * ) SI_UNIT ( $, .STERADIAN. ) SOLID_ANGLE_UNIT ( ) );
#169340 = CARTESIAN_POINT ( 'NONE',  ( 0.5495624486224826022, 1.449728300881658383, 1.321815246172884040 ) ) ;
#169341 = FACE_OUTER_BOUND ( 'NONE', #71676, .T. ) ;
#169342 = FACE_OUTER_BOUND ( 'NONE', #114191, .T. ) ;
#169343 = ORIENTED_EDGE ( 'NONE', *, *, #91968, .T. ) ;
#169344 = CARTESIAN_POINT ( 'NONE',  ( 6.157435431667657610, 1.928259211291092123, -0.5899821858514133766 ) ) ;
#169345 = CARTESIAN_POINT ( 'NONE',  ( -7.537443334193545397, 10.88110209227943770, -1.199719254218446718 ) ) ;
#169346 = DIRECTION ( 'NONE',  ( 7.993605777301127091E-15, 0.000000000000000000, 1.000000000000000000 ) ) ;
#169347 = CARTESIAN_POINT ( 'NONE',  ( 2.922911270491454161, -1.500192211782652718, 1.569583652781519012 ) ) ;
#169348 = DIRECTION ( 'NONE',  ( 0.000000000000000000, 0.000000000000000000, 1.000000000000000000 ) ) ;
#169349 = CARTESIAN_POINT ( 'NONE',  ( 1.248456593208754795, 1.040400552670465162, -1.847740296886036582 ) ) ;
#169350 = CARTESIAN_POINT ( 'NONE',  ( -1.402160292154681736E-14, 1.868750000682816381, -1.732050807568863648 ) ) ;
#169351 = CARTESIAN_POINT ( 'NONE',  ( 8.757677159423465696, 12.30470822171437284, 1.199719254218450271 ) ) ;
#169352 = SURFACE_STYLE_FILL_AREA ( #135797 ) ;
#169353 = CARTESIAN_POINT ( 'NONE',  ( 5.966021608595377224, 7.209656400309186530, 1.216315744458285719 ) ) ;
#169354 = CARTESIAN_POINT ( 'NONE',  ( 0.7903930413690943846, -2.044920356511644499, -0.2547782948326294816 ) ) ;
#169356 = CARTESIAN_POINT ( 'NONE',  ( 0.3633518834214408688, 2.686172036145575426, 1.968336656323642853 ) ) ;
#169355 = CARTESIAN_POINT ( 'NONE',  ( -8.696665468161981494, 12.23352791524263239, -1.199719254218446718 ) ) ;
#169357 = CARTESIAN_POINT ( 'NONE',  ( -0.6823417656250212460, 1.551041667008083769, 1.181850606188755259 ) ) ;
#169358 = FACE_OUTER_BOUND ( 'NONE', #18527, .T. ) ;
#169359 = ORIENTED_EDGE ( 'NONE', *, *, #68413, .F. ) ;
#169360 = CARTESIAN_POINT ( 'NONE',  ( 4.055252259792781366, -1.662250449027093735, 0.9452659147194606426 ) ) ;
#169361 = PRESENTATION_LAYER_ASSIGNMENT (  '', '', ( #121051 ) ) ;
#169362 = CARTESIAN_POINT ( 'NONE',  ( 7.361151057576892143, 7.552707420120024828, 0.7998128361456291469 ) ) ;
#169363 = CARTESIAN_POINT ( 'NONE',  ( -4.762992037102518950, 4.451245552908022596, -0.7998128361456221525 ) ) ;
#169364 = CARTESIAN_POINT ( 'NONE',  ( -0.07045567476893913050, -1.776642250867260575, 0.3530574836328649324 ) ) ;
#169366 = CARTESIAN_POINT ( 'NONE',  ( 0.9541331885446997507, -1.212804274533643145, 1.482964625430952976 ) ) ;
#169365 = CARTESIAN_POINT ( 'NONE',  ( 1.441115678600851213, 8.287243072884326267, -3.161846531485696499 ) ) ;
#169367 = CARTESIAN_POINT ( 'NONE',  ( 1.627480586986803868, 0.1543294891723171747, -2.064685722993148342 ) ) ;
#169368 = CARTESIAN_POINT ( 'NONE',  ( -1.364683531250000748, 0.3218750003414205807, 0.000000000000000000 ) ) ;
#169369 = ADVANCED_FACE ( 'NONE', ( #17853 ), #133579, .T. ) ;
#169370 = CARTESIAN_POINT ( 'NONE',  ( 0.2156151883831447236, -1.933912933822299784, 0.3821239771369787097 ) ) ;
#169371 = CARTESIAN_POINT ( 'NONE',  ( 3.123480263227970344, -1.759325740769552393, 0.4874977319994436287 ) ) ;
#169373 = CARTESIAN_POINT ( 'NONE',  ( 5.685886686578042415, 7.314606927785019863, 1.221034997698521307 ) ) ;
#169372 = CARTESIAN_POINT ( 'NONE',  ( 6.445939570963194143, 0.8488519614954292969, -2.037301952897092594 ) ) ;
#169374 = CARTESIAN_POINT ( 'NONE',  ( -1.364683531250012516, 1.280208333674755172, 0.7879004041258379498 ) ) ;
#169375 = CARTESIAN_POINT ( 'NONE',  ( 4.316881300680885047, -1.530586319191833633, 1.382930202259499364 ) ) ;
#169376 = CARTESIAN_POINT ( 'NONE',  ( -4.876128802409253282, 8.840567369452784874, 0.7998128361456481317 ) ) ;
#169377 = CARTESIAN_POINT ( 'NONE',  ( 6.401421083946654100, 10.62007503124645957, -0.7998128361456291469 ) ) ;
#169378 = CARTESIAN_POINT ( 'NONE',  ( 5.605114358992041801, 6.317488171369740613, -1.123711807521186490 ) ) ;
#169379 = CARTESIAN_POINT ( 'NONE',  ( 6.491656622844908853, 6.468020902940851968, 0.7998128361456341429 ) ) ;
#169381 = CARTESIAN_POINT ( 'NONE',  ( 1.499999999999987121, 4.045833333333359150, -0.8660254037844323793 ) ) ;
#169380 = CARTESIAN_POINT ( 'NONE',  ( 4.858481695672255185, 0.8034365979220282616, 1.946882858121199211 ) ) ;
#169382 = CARTESIAN_POINT ( 'NONE',  ( 6.795378861676105053, -1.851214886592133846, 0.9271815693319698237 ) ) ;
#169383 = CARTESIAN_POINT ( 'NONE',  ( 0.6823417656249899377, 1.905208333674752952, 1.181850606188755259 ) ) ;
#169384 = CARTESIAN_POINT ( 'NONE',  ( 3.268983376858981327, -1.995845357749256976, -0.8305886511386084692 ) ) ;
#169385 = CARTESIAN_POINT ( 'NONE',  ( 4.125652552961744490, -0.3430436748357457710, 1.990152796604119034 ) ) ;
#169386 =( NAMED_UNIT ( * ) PLANE_ANGLE_UNIT ( ) SI_UNIT ( $, .RADIAN. ) );
#169387 = EDGE_CURVE ( 'NONE', #148587, #18521, #3669, .T. ) ;
#169390 = CARTESIAN_POINT ( 'NONE',  ( 5.721177635286841756, 6.737423998331861341, -1.082531754730543083 ) ) ;
#169389 = CARTESIAN_POINT ( 'NONE',  ( -3.285556943750000514, -2.938541666188710266, -1.896917185911906500 ) ) ;
#169388 = CARTESIAN_POINT ( 'NONE',  ( -1.225000000000010747, 1.500000000000008216, -8.673617379884035472E-15 ) ) ;
#169391 = CARTESIAN_POINT ( 'NONE',  ( -6.200875153403786477, 8.327716660428123419, -1.599625672291271394 ) ) ;
#169392 = CARTESIAN_POINT ( 'NONE',  ( 2.800017839408690090, -0.9981255096969069429, -1.752139039461996006 ) ) ;
#169393 = CARTESIAN_POINT ( 'NONE',  ( -7.883176251342026042, 11.28445716228600126, -1.199719254218446718 ) ) ;
#169395 = CARTESIAN_POINT ( 'NONE',  ( -10.91970695577495576, -5.907420853759283830, 8.456776945386934585E-15 ) ) ;
#169394 = CARTESIAN_POINT ( 'NONE',  ( -3.093231602212184850, 6.760520635889515795, -0.7998128361456281477 ) ) ;
#169396 = CARTESIAN_POINT ( 'NONE',  ( -0.6823417656250003738, 8.651041667008065872, 1.181850606188754593 ) ) ;
#169397 = CARTESIAN_POINT ( 'NONE',  ( 6.720655732516654268, 4.688933928088002467, 2.736284108207136079 ) ) ;
#169399 = CARTESIAN_POINT ( 'NONE',  ( 4.306267660493944049, 1.238306454277863677, -1.591331080693689781 ) ) ;
#169398 = CARTESIAN_POINT ( 'NONE',  ( -8.310784975052685652, 9.758632561392040827, -1.082531754730543083 ) ) ;
#169400 = CARTESIAN_POINT ( 'NONE',  ( -1.201851678989727383E-14, 4.587500000000025224, -1.732050807568863648 ) ) ;
#169401 = CARTESIAN_POINT ( 'NONE',  ( 0.6823417656249969321, 15.08854166700806410, -1.181850606188757036 ) ) ;
#169402 = CARTESIAN_POINT ( 'NONE',  ( 6.405283072077849305, 1.437190941405818156, 0.9532465752533066938 ) ) ;
#169403 = CARTESIAN_POINT ( 'NONE',  ( 6.170896192875352959, 7.228408975556602556, 1.199719254218453823 ) ) ;
#169405 = CARTESIAN_POINT ( 'NONE',  ( 0.04225267894259320672, -6.625438066542582938, 11.00000000000012257 ) ) ;
#169404 = CARTESIAN_POINT ( 'NONE',  ( 9.083599731475988648, 10.66024977721925104, 1.082531754730549967 ) ) ;
#169406 = AXIS2_PLACEMENT_3D ( 'NONE', #60412, #92946, #23638 ) ;
#169407 = CARTESIAN_POINT ( 'NONE',  ( -11.41492544888517990, 7.843637262818779377, 3.710592433486775921 ) ) ;
#169408 = CARTESIAN_POINT ( 'NONE',  ( 5.659403934932580427, 0.3656299861228041181, -1.834283699791404043 ) ) ;
#169409 =( BOUNDED_CURVE ( )  B_SPLINE_CURVE ( 2, ( #105013, #155885, #205677, #154818, #6403, #198482, #138575, #71400, #199550, #117315, #23731, #183311, #189441, #100990, #107191, #57314, #167080, #172136, #18671, #188365, #40005, #106115, #173216, #150838, #89836, #182237, #7473, #116249, #5318, #137512, #73554, #90898, #156959, #8551, #50127, #87341, #137172, #84133, #201057, #179779, #170717, #167522, #163529, #71056, #169651, #54842, #31398, #118829, #153409, #35375, #200001, #150219, #21236, #97472, #18046, #196031, #38592, #53775, #52698, #6060, #101449, #4978, #22303, #104669, #183765, #88414, #19119, #154482, #47666, #130039, #102519, #113777, #136099, #186960, #1791, #185883, #67848, #135044, #168582, #133995, #51651, #120993, #117774, #85198, #203196, #151283, #103594, #2854, #184815, #36445, #68923, #20182, #86269, #152340, #3918, #69987, #202115, #119908, #37518, #26595, #107930, #10336, #72131, #93761, #92696, #76410, #23383, #140392, #122061, #110056, #41817, #74296, #206411, #59098, #123148, #189105, #89495, #40738, #55904, #139307, #205336, #108990, #39654, #188025, #138238, #192280, #207478, #58035, #159800, #106844, #56974, #172875, #24446, #90559, #105763, #156621, #155549, #25528, #43940, #124199, #204252, #75359, #126319, #171788, #125258, #7128, #191218, #158742, #173954, #190163, #91636, #73201, #42881, #8211, #141471, #157688, #175009, #142520, #9286, #208529, #60165, #176068, #27666, #64439, #111121, #197620, #65470, #112195, #13545, #130583, #194433, #212801, #46074, #195509, #181379, #77481, #177124, #163016, #79616, #129529, #30890, #143600, #114327, #33003, #12471, #196573, #80695, #164083, #147833, #131621, #180323, #49264, #28741, #11403, #47146, #31945, #15664, #179267, #113262, #209592, #145735, #193366, #94826, #115385, #78546, #45011, #61238, #96968, #14598, #211735, #146786, #127394, #99081, #63373, #160877, #62306, #48215, #144664, #98029, #210678, #178200, #81751, #213851, #128465, #29817, #95901, #161954, #119647, #169396, #116438, #18859, #458, #202938, #134793, #167274, #84943, #152089, #1531, #67594, #182432, #133739, #199746, #17783 ),
 .UNSPECIFIED., .F., .T. ) 
 B_SPLINE_CURVE_WITH_KNOTS ( ( 3, 2, 2, 2, 2, 2, 2, 2, 2, 2, 2, 2, 2, 2, 2, 2, 2, 2, 2, 2, 2, 2, 2, 2, 2, 2, 2, 2, 2, 2, 2, 2, 2, 2, 2, 2, 2, 2, 2, 2, 2, 2, 2, 2, 2, 2, 2, 2, 2, 2, 2, 2, 2, 2, 2, 2, 2, 2, 2, 2, 2, 2, 2, 2, 2, 2, 2, 2, 2, 2, 2, 2, 2, 2, 2, 2, 2, 2, 2, 2, 2, 2, 2, 2, 2, 2, 2, 2, 2, 2, 2, 2, 2, 2, 2, 2, 2, 2, 2, 2, 2, 2, 2, 2, 2, 2, 2, 2, 2, 2, 2, 2, 2, 2, 2, 2, 2, 2, 2, 2, 2, 3 ),
 ( 0.2833317628822501488, 0.2857142857142856984, 0.2916666666666666852, 0.2976190476190476164, 0.3035714285714285476, 0.3095238095238095344, 0.3154761904761904656, 0.3214285714285714524, 0.3273809523809523836, 0.3333333333333333148, 0.3392857142857143016, 0.3452380952380952328, 0.3511904761904761640, 0.3571428571428571508, 0.3630952380952380820, 0.3690476190476190688, 0.3750000000000000000, 0.3809523809523809312, 0.3869047619047619180, 0.3928571428571428492, 0.3988095238095238360, 0.4047619047619047672, 0.4107142857142856984, 0.4166666666666666852, 0.4226190476190476164, 0.4285714285714285476, 0.4345238095238095344, 0.4404761904761904656, 0.4464285714285714524, 0.4523809523809523836, 0.4583333333333333148, 0.4642857142857143016, 0.4702380952380952328, 0.4761904761904761640, 0.4821428571428571508, 0.4880952380952380820, 0.4940476190476190688, 0.5000000000000000000, 0.5059523809523809312, 0.5119047619047618625, 0.5178571428571429047, 0.5238095238095238360, 0.5297619047619047672, 0.5357142857142856984, 0.5416666666666666297, 0.5476190476190476719, 0.5535714285714286031, 0.5595238095238095344, 0.5654761904761904656, 0.5714285714285713969, 0.5773809523809523281, 0.5833333333333333703, 0.5892857142857143016, 0.5952380952380952328, 0.6011904761904761640, 0.6071428571428570953, 0.6130952380952381375, 0.6190476190476190688, 0.6250000000000000000, 0.6309523809523809312, 0.6369047619047618625, 0.6428571428571430157, 0.6488095238095238360, 0.6547619047619047672, 0.6607142857142856984, 0.6666666666666665186, 0.6726190476190476719, 0.6785714285714286031, 0.6845238095238095344, 0.6904761904761904656, 0.6964285714285713969, 0.7023809523809523281, 0.7083333333333333703, 0.7142857142857143016, 0.7202380952380952328, 0.7261904761904760530, 0.7321428571428570953, 0.7380952380952381375, 0.7440476190476190688, 0.7500000000000000000, 0.7559523809523809312, 0.7619047619047618625, 0.7678571428571429047, 0.7738095238095238360, 0.7797619047619047672, 0.7857142857142856984, 0.7916666666666666297, 0.7976190476190476719, 0.8035714285714286031, 0.8095238095238095344, 0.8154761904761904656, 0.8214285714285713969, 0.8273809523809523281, 0.8333333333333333703, 0.8392857142857143016, 0.8452380952380952328, 0.8511904761904761640, 0.8571428571428570953, 0.8630952380952381375, 0.8690476190476190688, 0.8750000000000000000, 0.8809523809523809312, 0.8869047619047618625, 0.8928571428571429047, 0.8988095238095238360, 0.9047619047619047672, 0.9107142857142856984, 0.9166666666666666297, 0.9226190476190476719, 0.9285714285714286031, 0.9345238095238095344, 0.9404761904761904656, 0.9464285714285713969, 0.9523809523809523281, 0.9583333333333333703, 0.9642857142857143016, 0.9702380952380952328, 0.9761904761904761640, 0.9821428571428570953, 0.9880952380952381375, 0.9940476190476190688, 1.000000000000000000 ),
 .UNSPECIFIED. ) 
 CURVE ( )  GEOMETRIC_REPRESENTATION_ITEM ( )  RATIONAL_B_SPLINE_CURVE ( ( 0.9356780735513487990, 0.9463748142214183368, 1.000000000000000000, 0.8660254037844387076, 1.000000000000000000, 0.8660254037844387076, 1.000000000000000000, 0.8660254037844387076, 1.000000000000000000, 0.8660254037844387076, 1.000000000000000000, 0.8660254037844387076, 1.000000000000000000, 0.8660254037844387076, 1.000000000000000000, 0.8660254037844387076, 1.000000000000000000, 0.8660254037844387076, 1.000000000000000000, 0.8660254037844387076, 1.000000000000000000, 0.8660254037844387076, 1.000000000000000000, 0.8660254037844387076, 1.000000000000000000, 0.8660254037844387076, 1.000000000000000000, 0.8660254037844387076, 1.000000000000000000, 0.8660254037844387076, 1.000000000000000000, 0.8660254037844387076, 1.000000000000000000, 0.8660254037844387076, 1.000000000000000000, 0.8660254037844387076, 1.000000000000000000, 0.8660254037844387076, 1.000000000000000000, 0.8660254037844387076, 1.000000000000000000, 0.8660254037844387076, 1.000000000000000000, 0.8660254037844387076, 1.000000000000000000, 0.8660254037844387076, 1.000000000000000000, 0.8660254037844387076, 1.000000000000000000, 0.8660254037844387076, 1.000000000000000000, 0.8660254037844387076, 1.000000000000000000, 0.8660254037844387076, 1.000000000000000000, 0.8660254037844387076, 1.000000000000000000, 0.8660254037844387076, 1.000000000000000000, 0.8660254037844387076, 1.000000000000000000, 0.8660254037844387076, 1.000000000000000000, 0.8660254037844387076, 1.000000000000000000, 0.8660254037844387076, 1.000000000000000000, 0.8660254037844387076, 1.000000000000000000, 0.8660254037844387076, 1.000000000000000000, 0.8660254037844387076, 1.000000000000000000, 0.8660254037844387076, 1.000000000000000000, 0.8660254037844387076, 1.000000000000000000, 0.8660254037844387076, 1.000000000000000000, 0.8660254037844387076, 1.000000000000000000, 0.8660254037844387076, 1.000000000000000000, 0.8660254037844387076, 1.000000000000000000, 0.8660254037844387076, 1.000000000000000000, 0.8660254037844387076, 1.000000000000000000, 0.8660254037844387076, 1.000000000000000000, 0.8660254037844387076, 1.000000000000000000, 0.8660254037844387076, 1.000000000000000000, 0.8660254037844387076, 1.000000000000000000, 0.8660254037844387076, 1.000000000000000000, 0.8660254037844387076, 1.000000000000000000, 0.8660254037844387076, 1.000000000000000000, 0.8660254037844387076, 1.000000000000000000, 0.8660254037844387076, 1.000000000000000000, 0.8660254037844387076, 1.000000000000000000, 0.8660254037844387076, 1.000000000000000000, 0.8660254037844387076, 1.000000000000000000, 0.8660254037844387076, 1.000000000000000000, 0.8660254037844387076, 1.000000000000000000, 0.8660254037844387076, 1.000000000000000000, 0.8660254037844387076, 1.000000000000000000, 0.8660254037844387076, 1.000000000000000000, 0.8660254037844387076, 1.000000000000000000, 0.8660254037844387076, 1.000000000000000000, 0.8660254037844387076, 1.000000000000000000, 0.8660254037844387076, 1.000000000000000000, 0.8660254037844387076, 1.000000000000000000, 0.8660254037844387076, 1.000000000000000000, 0.8660254037844387076, 1.000000000000000000, 0.8660254037844387076, 1.000000000000000000, 0.8660254037844387076, 1.000000000000000000, 0.8660254037844387076, 1.000000000000000000, 0.8660254037844387076, 1.000000000000000000, 0.8660254037844387076, 1.000000000000000000, 0.8660254037844387076, 1.000000000000000000, 0.8660254037844387076, 1.000000000000000000, 0.8660254037844387076, 1.000000000000000000, 0.8660254037844387076, 1.000000000000000000, 0.8660254037844387076, 1.000000000000000000, 0.8660254037844387076, 1.000000000000000000, 0.8660254037844387076, 1.000000000000000000, 0.8660254037844387076, 1.000000000000000000, 0.8660254037844387076, 1.000000000000000000, 0.8660254037844387076, 1.000000000000000000, 0.8660254037844387076, 1.000000000000000000, 0.8660254037844387076, 1.000000000000000000, 0.8660254037844387076, 1.000000000000000000, 0.8660254037844387076, 1.000000000000000000, 0.8660254037844387076, 1.000000000000000000, 0.8660254037844387076, 1.000000000000000000, 0.8660254037844387076, 1.000000000000000000, 0.8660254037844387076, 1.000000000000000000, 0.8660254037844387076, 1.000000000000000000, 0.8660254037844387076, 1.000000000000000000, 0.8660254037844387076, 1.000000000000000000, 0.8660254037844387076, 1.000000000000000000, 0.8660254037844387076, 1.000000000000000000, 0.8660254037844387076, 1.000000000000000000, 0.8660254037844387076, 1.000000000000000000, 0.8660254037844387076, 1.000000000000000000, 0.8660254037844387076, 1.000000000000000000, 0.8660254037844387076, 1.000000000000000000, 0.8660254037844387076, 1.000000000000000000, 0.8660254037844387076, 1.000000000000000000, 0.8660254037844387076, 1.000000000000000000, 0.8660254037844387076, 1.000000000000000000, 0.8660254037844387076, 1.000000000000000000, 0.8660254037844387076, 1.000000000000000000, 0.8660254037844387076, 1.000000000000000000, 0.8660254037844387076, 1.000000000000000000, 0.8660254037844387076, 1.000000000000000000, 0.8660254037844387076, 1.000000000000000000, 0.8660254037844387076, 1.000000000000000000, 0.8660254037844387076, 1.000000000000000000, 0.8660254037844387076, 1.000000000000000000, 0.8660254037844387076, 1.000000000000000000, 0.8660254037844387076, 1.000000000000000000, 0.8660254037844387076, 1.000000000000000000, 0.8660254037844387076, 1.000000000000000000, 0.8660254037844387076, 1.000000000000000000, 0.8660254037844387076, 1.000000000000000000, 0.8660254037844387076, 1.000000000000000000 ) ) 
 REPRESENTATION_ITEM ( '' )  );
#169410 = CARTESIAN_POINT ( 'NONE',  ( 6.381113974719265336, -1.842344568942927419, -0.8120077521172417434 ) ) ;
#169411 = FACE_OUTER_BOUND ( 'NONE', #117025, .T. ) ;
#169412 = CARTESIAN_POINT ( 'NONE',  ( -4.650083499807250220, 5.295740330745369207, -7.499999999999997335 ) ) ;
#169413 = EDGE_LOOP ( 'NONE', ( #153050, #47562, #13220, #105015 ) ) ;
#169414 = FACE_OUTER_BOUND ( 'NONE', #163133, .T. ) ;
#169415 = CARTESIAN_POINT ( 'NONE',  ( 1.089470510105726708, -0.4871801946146369633, 1.956568126268923846 ) ) ;
#169416 = CARTESIAN_POINT ( 'NONE',  ( 0.9315677820061087910, -1.767094751418090803, 0.3981412331970111684 ) ) ;
#169417 = CARTESIAN_POINT ( 'NONE',  ( 3.702785349863636277, 7.334016984900627811, -0.7216878364870338292 ) ) ;
#169418 = DIRECTION ( 'NONE',  ( -0.000000000000000000, 1.000000000000000000, -0.000000000000000000 ) ) ;
#169419 = CARTESIAN_POINT ( 'NONE',  ( 7.741342523278692767, 11.01502146292508044, 1.082531754730558626 ) ) ;
#169420 = AXIS2_PLACEMENT_3D ( 'NONE', #1015, #48749, #84428 ) ;
#169421 = CARTESIAN_POINT ( 'NONE',  ( 6.479907352327590964, 9.647310113435821677, 1.199719254218462483 ) ) ;
#169423 = CARTESIAN_POINT ( 'NONE',  ( 5.853135685669797361, 0.1356727809044282473, -1.910850313501164743 ) ) ;
#169422 = CARTESIAN_POINT ( 'NONE',  ( -6.227272627378437342, 6.159572908229946187, -0.7998128361456291469 ) ) ;
#169424 = DIRECTION ( 'NONE',  ( -0.000000000000000000, -1.000000000000000000, -0.000000000000000000 ) ) ;
#169425 = CARTESIAN_POINT ( 'NONE',  ( -1.364683531250000748, -0.4281249996585800854, 0.000000000000000000 ) ) ;
#169427 = ORIENTED_EDGE ( 'NONE', *, *, #81943, .T. ) ;
#169426 = CARTESIAN_POINT ( 'NONE',  ( 2.223174002961016082, 5.537527403522402025, -0.7216878364870267237 ) ) ;
#169428 = CARTESIAN_POINT ( 'NONE',  ( -2.272963308585411735, 5.803540959991587478, 0.7998128361456341429 ) ) ;
#169429 = CARTESIAN_POINT ( 'NONE',  ( 4.399409362686744096, 1.734418756986338295, 1.290045131933370781 ) ) ;
#169430 = CARTESIAN_POINT ( 'NONE',  ( -7.444835747679825033, 7.858265591814152629, 0.000000000000000000 ) ) ;
#169431 = CARTESIAN_POINT ( 'NONE',  ( 6.373741612200171325, 7.569024981389272710, 1.082531754730549967 ) ) ;
#169432 = CARTESIAN_POINT ( 'NONE',  ( 0.2465380642357860586, 1.084720387836759947, -1.822023332652397354 ) ) ;
#169433 = CARTESIAN_POINT ( 'NONE',  ( 6.053692819838605743, 0.5272490726609193601, -1.747765065496959869 ) ) ;
#169434 = ADVANCED_FACE ( 'NONE', ( #124480 ), #86889, .F. ) ;
#169435 = CARTESIAN_POINT ( 'NONE',  ( 2.231653169902757750, -1.284661796483690832, -1.495404430405805174 ) ) ;
#169436 = CARTESIAN_POINT ( 'NONE',  ( 4.711142613322857109, 1.586760866459841379, -1.067142987418716604 ) ) ;
#169437 = ORIENTED_EDGE ( 'NONE', *, *, #74578, .T. ) ;
#169438 = CARTESIAN_POINT ( 'NONE',  ( 9.497255425109827343, -6.896119493545203483, -0.09872732973945687329 ) ) ;
#169439 = CARTESIAN_POINT ( 'NONE',  ( 5.670349227943210835, -0.8838483254627060859, -1.760150121488897490 ) ) ;
#169440 = CARTESIAN_POINT ( 'NONE',  ( 0.1814471035007196309, -0.9164790359779145801, 1.712077929913154328 ) ) ;
#169441 = ORIENTED_EDGE ( 'NONE', *, *, #19647, .F. ) ;
#169442 = CARTESIAN_POINT ( 'NONE',  ( -3.461074353238556167, 7.259946855412102273, 0.000000000000000000 ) ) ;
#169443 = CARTESIAN_POINT ( 'NONE',  ( -5.144392941742557568, 4.966489618313220333, -0.7998128361456362523 ) ) ;
#169445 = CARTESIAN_POINT ( 'NONE',  ( 6.224601922005513543, 7.395028676162137771, -1.082531754730548412 ) ) ;
#169444 = CARTESIAN_POINT ( 'NONE',  ( 8.284195553149872993, 9.623648552551724578, -1.199719254218445830 ) ) ;
#169447 = EDGE_LOOP ( 'NONE', ( #199509, #9353, #20459, #39414 ) ) ;
#169446 = CARTESIAN_POINT ( 'NONE',  ( 4.512308969215598431, -1.911949174345693336, -0.04343532550177275214 ) ) ;
#169448 = CARTESIAN_POINT ( 'NONE',  ( 0.3763673390903346516, 1.272619870141003418, 1.802674353332263335 ) ) ;
#169449 = CARTESIAN_POINT ( 'NONE',  ( 0.4032277238576422174, 3.019957635004400842, -0.4115402804778697243 ) ) ;
#169450 = CARTESIAN_POINT ( 'NONE',  ( 5.901044691261273734, -0.2977458250903759485, -1.990848032377992016 ) ) ;
#169451 = CARTESIAN_POINT ( 'NONE',  ( 0.07680821025391955381, 7.629137130509078268, -2.410791881123967251 ) ) ;
#169452 = CARTESIAN_POINT ( 'NONE',  ( 10.99943592164172657, -8.407420853759269619, -0.1113975120798811613 ) ) ;
#169453 = CARTESIAN_POINT ( 'NONE',  ( 6.778728372092623466, -7.783114986501003862, -6.734029298721178947 ) ) ;
#169454 = CARTESIAN_POINT ( 'NONE',  ( 2.857943571468853250, -0.6518772230660694333, 1.965110387975615991 ) ) ;
#169455 = CARTESIAN_POINT ( 'NONE',  ( -5.545448523189368650, 6.428443684264421698, -1.199719254218446718 ) ) ;
#169456 = CARTESIAN_POINT ( 'NONE',  ( -4.607477032339801326, 8.379641378740778634, 0.1280868206084313787 ) ) ;
#169458 = CARTESIAN_POINT ( 'NONE',  ( 0.9717996764858798375, 2.083101276202529384, -0.5774176476955604764 ) ) ;
#169457 = CARTESIAN_POINT ( 'NONE',  ( -4.172158584703340445, 5.890604320285754980, -1.599625672291256295 ) ) ;
#169459 = CARTESIAN_POINT ( 'NONE',  ( -10.81391327432222838, 6.436729623570534464, -5.219172391766678132 ) ) ;
#169460 = CARTESIAN_POINT ( 'NONE',  ( 3.445180431648323882, 6.073108699348104267, 1.082531754730549078 ) ) ;
#169461 = CARTESIAN_POINT ( 'NONE',  ( 7.986233326679963440, -6.863455982311493564, -7.564733433744406987 ) ) ;
#169462 = CIRCLE ( 'NONE', #38061, 0.08000000000000020983 ) ;
#169463 = CARTESIAN_POINT ( 'NONE',  ( 1.364683531250000303, 13.56770833367473017, -0.7879004041258355073 ) ) ;
#169465 = CARTESIAN_POINT ( 'NONE',  ( -6.791708605802965870, 6.888357893050385705, -0.7998128361456362523 ) ) ;
#169464 = CARTESIAN_POINT ( 'NONE',  ( 5.181758602633672162, 4.945385036406048762, -2.500000000000000444 ) ) ;
#169466 = CARTESIAN_POINT ( 'NONE',  ( 2.606657977298726614, 1.900416011228076130, 0.6748465934659984011 ) ) ;
#169467 = CARTESIAN_POINT ( 'NONE',  ( 5.396976841598324803, -0.7867719702298915374, -1.545497150229415251 ) ) ;
#169468 = CARTESIAN_POINT ( 'NONE',  ( -3.846762897975357198, 5.510976019103107859, -1.599625672291256295 ) ) ;
#169469 = CARTESIAN_POINT ( 'NONE',  ( 3.116144222688784549, 2.060704436481402890, -0.1983081510379124945 ) ) ;
#169470 = CARTESIAN_POINT ( 'NONE',  ( 5.079753589751704546, -0.7609352437839884686, 1.975942822842210234 ) ) ;
#169471 = CARTESIAN_POINT ( 'NONE',  ( 7.100719765255169236, 9.307259030929609267, -1.599625672291262513 ) ) ;
#169472 = CARTESIAN_POINT ( 'NONE',  ( -0.6823417656249969321, 5.217708333674756283, -1.181850606188749264 ) ) ;
#169473 = CARTESIAN_POINT ( 'NONE',  ( 3.028127619189690201, 1.049479266250245901, 1.666313143567710542 ) ) ;
#169474 = CARTESIAN_POINT ( 'NONE',  ( 0.7559434568639655794, 0.7726834774516875282, -1.749509110286852742 ) ) ;
#169475 = CARTESIAN_POINT ( 'NONE',  ( 4.488395308864603805, -0.4996631572763092222, -2.236994043316854697 ) ) ;
#169477 = EDGE_CURVE ( 'NONE', #6177, #181174, #31340, .T. ) ;
#169476 = CARTESIAN_POINT ( 'NONE',  ( 2.754317325142870754, 0.6151756178996542479, 1.719052816137212503 ) ) ;
#169478 = CARTESIAN_POINT ( 'NONE',  ( 5.448397627845284141, 7.449826213943242514, 1.599625672291268286 ) ) ;
#169479 = CARTESIAN_POINT ( 'NONE',  ( 5.788968402910812827, 6.816513227226497662, 1.082531754730558626 ) ) ;
#169480 = CARTESIAN_POINT ( 'NONE',  ( -7.718669524881690336, 7.899535955317097624, 0.7998128361456462443 ) ) ;
#169481 = CARTESIAN_POINT ( 'NONE',  ( 4.025643311844375738, -0.3400233446379635760, 1.984125136466656558 ) ) ;
#169482 = CARTESIAN_POINT ( 'NONE',  ( 2.711707638535421960, 0.5279276851305572116, -1.889291386287835550 ) ) ;
#169483 = CARTESIAN_POINT ( 'NONE',  ( -8.030507057996002729, 8.263346410617135263, 1.040834085586084257E-14 ) ) ;
#169484 = CARTESIAN_POINT ( 'NONE',  ( -6.196239896645333367, 7.187700286629718605, -1.199719254218446718 ) ) ;
#169486 = EDGE_CURVE ( 'NONE', #138513, #182199, #38030, .T. ) ;
#169485 = CARTESIAN_POINT ( 'NONE',  ( 10.95308175811721085, 13.79999999999999893, -1.800000000000001155 ) ) ;
#169488 = CARTESIAN_POINT ( 'NONE',  ( 4.153014383403249354, -1.471681513620528348, -0.9827620175600642050 ) ) ;
#169487 = CARTESIAN_POINT ( 'NONE',  ( 6.316366637557600860, 1.950215401406007354, 0.7537550503652605816 ) ) ;
#169489 = CARTESIAN_POINT ( 'NONE',  ( 1.499999999999990896, 3.306250000682818602, 1.214306433183764966E-14 ) ) ;
#169490 = CARTESIAN_POINT ( 'NONE',  ( 0.3577192552456122665, 2.167005522336755696, -0.3256184645209562190 ) ) ;
#169491 = CARTESIAN_POINT ( 'NONE',  ( 6.615217694991038400, -1.686041314625020160, 0.4309386324203681728 ) ) ;
#169492 = CARTESIAN_POINT ( 'NONE',  ( 7.233438648090761980, 8.397765496649418182, 1.199719254218462483 ) ) ;
#169493 = CARTESIAN_POINT ( 'NONE',  ( -11.33772463945036968, 10.90000000000000036, -3.680000000000001048 ) ) ;
#169494 = CARTESIAN_POINT ( 'NONE',  ( 0.5448069426677571991, 2.143542105210020754, -0.8297726512136813781 ) ) ;
#169495 = CARTESIAN_POINT ( 'NONE',  ( 0.09952931447375359952, -0.5783855404800625211, 2.113812074898171023 ) ) ;
#169496 = CARTESIAN_POINT ( 'NONE',  ( 6.679014442879065427, -0.8212242018711314318, -1.526972759001248514 ) ) ;
#169497 = CARTESIAN_POINT ( 'NONE',  ( 3.158999515626020216, -1.670948785577108797, 1.441709373268922123 ) ) ;
#169498 = CARTESIAN_POINT ( 'NONE',  ( 6.426262541905297887, 1.110578645885337501, 1.865513821534901417 ) ) ;
#169499 = DIRECTION ( 'NONE',  ( -5.551115123125765446E-17, 0.000000000000000000, 1.000000000000000000 ) ) ;
#169500 = CARTESIAN_POINT ( 'NONE',  ( 1.429080218188124585, -1.785550482114751203, 1.137718905448012352 ) ) ;
#169501 = CARTESIAN_POINT ( 'NONE',  ( 3.250000000000002665, 1.855058607017213327E-13, 2.052068128417948056 ) ) ;
#169502 = CARTESIAN_POINT ( 'NONE',  ( 6.727182134110196721, 7.629137130509074716, 2.889055895399252005 ) ) ;
#169503 = CARTESIAN_POINT ( 'NONE',  ( 5.280268953417031952, -1.070192140894361099, 1.601580209743416860 ) ) ;
#169504 = ORIENTED_EDGE ( 'NONE', *, *, #192353, .F. ) ;
#169506 = CARTESIAN_POINT ( 'NONE',  ( 0.6823417656249864960, -0.7614583329919113464, -1.181850606188749264 ) ) ;
#169505 = CARTESIAN_POINT ( 'NONE',  ( 1.031297522511119613, -2.069548003639944511, 0.9861895074133855132 ) ) ;
#169507 = CARTESIAN_POINT ( 'NONE',  ( 5.169736645512481132, 4.925780929386339935, 0.7998128361456341429 ) ) ;
#169508 = CARTESIAN_POINT ( 'NONE',  ( 6.830610463186557624, 6.863467050006115677, 1.040834085586084257E-14 ) ) ;
#169509 = CARTESIAN_POINT ( 'NONE',  ( 3.774281487401151214, 2.204430612424528757, -0.2728622730414613784 ) ) ;
#169510 = CARTESIAN_POINT ( 'NONE',  ( -6.561783159334130922, 9.638868871656395498, -1.082531754730538864 ) ) ;
#169511 = CARTESIAN_POINT ( 'NONE',  ( 11.33772463945037146, 13.39999999999998259, 3.599999999999999201 ) ) ;
#169512 = CARTESIAN_POINT ( 'NONE',  ( 6.209271165378815738, 7.306866450105836464, -1.082531754730543083 ) ) ;
#169513 = CARTESIAN_POINT ( 'NONE',  ( -9.137832345486311070, 9.763151945929928743, 1.040834085586084257E-14 ) ) ;
#169514 = EDGE_CURVE ( 'NONE', #60728, #2366, #191670, .T. ) ;
#169515 = CARTESIAN_POINT ( 'NONE',  ( 4.895902868310594513, 8.725987423088758632, 0.000000000000000000 ) ) ;
#169516 = ORIENTED_EDGE ( 'NONE', *, *, #79132, .T. ) ;
#169517 = CARTESIAN_POINT ( 'NONE',  ( 1.951796282902381163, -1.844710420878793444, -0.8146254186931353169 ) ) ;
#169519 = CARTESIAN_POINT ( 'NONE',  ( 6.443808500197930833, 1.419581301535753015, 1.496705048937081006 ) ) ;
#169518 = CARTESIAN_POINT ( 'NONE',  ( 9.250740883225924804, 9.686952540052077509, 1.040834085586084257E-14 ) ) ;
#169520 = SURFACE_SIDE_STYLE ('',( #198797 ) ) ;
#169521 = CARTESIAN_POINT ( 'NONE',  ( 7.173672674962134899, 7.541908673643526129, -0.7216878364870317197 ) ) ;
#169522 = CARTESIAN_POINT ( 'NONE',  ( -0.05938221139379848412, -1.422385081007140117, -1.168950373246782526 ) ) ;
#169523 = CARTESIAN_POINT ( 'NONE',  ( 10.55819884875827697, -6.268611901546719878, -1.734723475976807094E-15 ) ) ;
#169524 = CARTESIAN_POINT ( 'NONE',  ( 1.364683531249986537, 2.405208333674752286, -0.7879004041258239610 ) ) ;
#169525 = CARTESIAN_POINT ( 'NONE',  ( 2.864225066854100277, -1.223476834174407779, 1.278924851658661099 ) ) ;
#169526 = CARTESIAN_POINT ( 'NONE',  ( 1.565077508395201988, -1.076315722900993643, 1.704939445326451475 ) ) ;
#169527 = CARTESIAN_POINT ( 'NONE',  ( 0.4855842612344652975, -1.827229208960782447, -0.2260576252584786672 ) ) ;
#169528 = CARTESIAN_POINT ( 'NONE',  ( 5.302359097629713247, 1.737542498810572322, -1.495360377712177113 ) ) ;
#169529 = CARTESIAN_POINT ( 'NONE',  ( 3.661895226921571656, -1.235415792305821325, 1.365283978338522441 ) ) ;
#169530 = CARTESIAN_POINT ( 'NONE',  ( 7.934546212495622086, 10.28005655271014795, -1.599625672291262513 ) ) ;
#169531 = CARTESIAN_POINT ( 'NONE',  ( 3.592628304870106870, -0.3553021837224104584, -1.790491875447843384 ) ) ;
#169532 = CARTESIAN_POINT ( 'NONE',  ( 5.045546153961558922, -1.458558117013383892, 1.392544180963309230 ) ) ;
#169533 = CARTESIAN_POINT ( 'NONE',  ( -8.748035429315585532, 11.22912730566677553, -1.599625672291263179 ) ) ;
#169535 = CARTESIAN_POINT ( 'NONE',  ( -6.688968683495758683, 8.897159112202094988, -1.599625672291271394 ) ) ;
#169534 = CARTESIAN_POINT ( 'NONE',  ( 2.975713975707586556, 2.148818855599075928, -0.7084362298409478953 ) ) ;
#169536 = CARTESIAN_POINT ( 'NONE',  ( 6.809622064836790223, -0.4623527835773094119, 2.061910140347056331 ) ) ;
#169537 = CARTESIAN_POINT ( 'NONE',  ( 11.86145016429273191, 10.90000000000000036, -1.100000000000002087 ) ) ;
#169538 = CARTESIAN_POINT ( 'NONE',  ( 3.490741092712910998, 2.019281663078629219, 0.4563312328872348722 ) ) ;
#169539 = CARTESIAN_POINT ( 'NONE',  ( 4.216749469050096621, 4.878294787768598262, -1.199719254218452047 ) ) ;
#169540 = CARTESIAN_POINT ( 'NONE',  ( 1.360316468749997565, 2.067708333674723509, -0.7853790794159001276 ) ) ;
#169541 = CARTESIAN_POINT ( 'NONE',  ( 5.971359625099014856, -1.818578809777360972, -1.090262957368436147 ) ) ;
#169542 = APPLICATION_PROTOCOL_DEFINITION ( 'draft international standard', 'automotive_design', 1998, #51947 ) ;
#169543 = MANIFOLD_SOLID_BREP ( 'Sweep1[11]', #153736 ) ;
#169545 = CARTESIAN_POINT ( 'NONE',  ( 2.174328269389655066, -1.185172859381509625, 1.518732482018339436 ) ) ;
#169544 = CARTESIAN_POINT ( 'NONE',  ( -8.143643823302737061, 12.65266822716189843, 0.000000000000000000 ) ) ;
#169546 = DIRECTION ( 'NONE',  ( 0.000000000000000000, 0.000000000000000000, 1.000000000000000000 ) ) ;
#169547 = CARTESIAN_POINT ( 'NONE',  ( 0.2913706227113096459, -1.802261421121041707, 0.7947621968238273160 ) ) ;
#169548 = CARTESIAN_POINT ( 'NONE',  ( 4.624739795592929248, 6.488892076315451618, -1.443375672974068769 ) ) ;
#169549 = CARTESIAN_POINT ( 'NONE',  ( 5.830449476509543594, 6.014588727829297987, 0.4175459632603968352 ) ) ;
#169550 = CARTESIAN_POINT ( 'NONE',  ( -0.7500000000000179856, 11.07291666734946212, 1.299038105676658228 ) ) ;
#169551 = CARTESIAN_POINT ( 'NONE',  ( -4.497554271431319250, 6.270232621468402989, -1.599625672291256295 ) ) ;
#169552 = CARTESIAN_POINT ( 'NONE',  ( 0.6158632564332514603, 1.820540700843051418, 1.272696253368794439 ) ) ;
#169553 = CARTESIAN_POINT ( 'NONE',  ( 3.241344266390119078, -1.858123463236575290, 0.9911517508872002002 ) ) ;
#169554 = CARTESIAN_POINT ( 'NONE',  ( -4.329849954717889915, 6.144853928627882489, 1.599625672291270506 ) ) ;
#169555 = CARTESIAN_POINT ( 'NONE',  ( 7.450369105909416589, 8.650851030771185890, -1.199719254218441611 ) ) ;
#169556 = CARTESIAN_POINT ( 'NONE',  ( 1.064655064206044166, 1.412561167129450457, -1.211817338188374782 ) ) ;
#169557 = CARTESIAN_POINT ( 'NONE',  ( 7.637320603199683866, 7.804628880021436288, -0.7998128361456281477 ) ) ;
#169558 = CARTESIAN_POINT ( 'NONE',  ( 3.985207087413062066, 6.736826471035503694, -1.199719254218452047 ) ) ;
#169559 = CARTESIAN_POINT ( 'NONE',  ( -5.302647476720585118, 9.200522799567075083, 0.000000000000000000 ) ) ;
#169560 = CARTESIAN_POINT ( 'NONE',  ( -6.887178846062109727, 10.01849717283904262, -1.082531754730537976 ) ) ;
#169561 = CARTESIAN_POINT ( 'NONE',  ( 0.8266187642571948269, -0.9586779626098644869, -1.891633453305548773 ) ) ;
#169562 = CARTESIAN_POINT ( 'NONE',  ( -6.074935347375019390, 9.245119117649618801, 1.199719254218452047 ) ) ;
#169564 = CARTESIAN_POINT ( 'NONE',  ( 4.193769882565239193, -1.351282707657221582, -1.422545440481419510 ) ) ;
#169563 = CARTESIAN_POINT ( 'NONE',  ( -1.225000000000040057, 0.7708333333333476922, 0.7072540797572656190 ) ) ;
#169565 = CARTESIAN_POINT ( 'NONE',  ( 2.131903390035182255, -1.411712784473453830, -1.637176306262012826 ) ) ;
#169566 = CARTESIAN_POINT ( 'NONE',  ( 1.962219809069129184, -1.683971100191889336, -0.7449956418128443891 ) ) ;
#169568 = CARTESIAN_POINT ( 'NONE',  ( -5.762678113124475310, 6.090388861115007657, -0.6347866013659544393 ) ) ;
#169567 = CARTESIAN_POINT ( 'NONE',  ( -3.122120512896910505, 6.864500708346841229, 0.7998128361456352531 ) ) ;
#169569 = CARTESIAN_POINT ( 'NONE',  ( 3.521201755802486844, -1.038059167858174092, -1.396672450663126508 ) ) ;
#169570 = CARTESIAN_POINT ( 'NONE',  ( 4.026131012922935959, 7.773685636243294006, 0.3673651676878584849 ) ) ;
#169571 = CARTESIAN_POINT ( 'NONE',  ( 4.663641653420880218, 8.384739662392275861, -0.7216878364870207285 ) ) ;
#169572 = CARTESIAN_POINT ( 'NONE',  ( -9.997759874121660673, 5.662387697485826266, 5.943071269081472430 ) ) ;
#169573 = CARTESIAN_POINT ( 'NONE',  ( 0.3566080023540801336, 0.8287714912002723811, 1.996717379258300840 ) ) ;
#169574 = CARTESIAN_POINT ( 'NONE',  ( 3.356795910091507906, -0.8196482158769199389, 1.842165019812888271 ) ) ;
#169575 = CARTESIAN_POINT ( 'NONE',  ( -9.124274191872631334, 12.62844174295135069, -1.082531754730543083 ) ) ;
#169576 = CARTESIAN_POINT ( 'NONE',  ( 0.5499753625364013354, 0.6768306982547143136, -2.053065283773393368 ) ) ;
#169577 = CARTESIAN_POINT ( 'NONE',  ( 3.239098446765543482, -1.739280071990648935, 0.9281937050133574063 ) ) ;
#169578 = CARTESIAN_POINT ( 'NONE',  ( 6.509000000000011887, 3.696273625755361447, 2.514342382328867753 ) ) ;
#169579 = CARTESIAN_POINT ( 'NONE',  ( 2.331498104393217474, 0.9136196428927362279, -1.713718834741830177 ) ) ;
#169582 = VERTEX_POINT ( 'NONE', #213074 ) ;
#169581 = CARTESIAN_POINT ( 'NONE',  ( -5.153507786970276783, 6.145418851954329575, -1.082531754730549967 ) ) ;
#169580 = CARTESIAN_POINT ( 'NONE',  ( 6.433860211133586304, -1.853236450885078712, 0.4715264990977630077 ) ) ;
#169583 = CARTESIAN_POINT ( 'NONE',  ( -5.953438849732214599, 6.118302544208584770, 0.7216878364870257245 ) ) ;
#169584 = CARTESIAN_POINT ( 'NONE',  ( -0.1110810684432960160, 0.2482034880273851774, -1.831546034005934853 ) ) ;
#169585 = CARTESIAN_POINT ( 'NONE',  ( 3.711900195091365262, 7.552577004240394132, -0.7998128361456362523 ) ) ;
#169586 = CARTESIAN_POINT ( 'NONE',  ( -5.601453741101424022, 6.564059448486966986, -1.199719254218453823 ) ) ;
#169588 = ORIENTED_EDGE ( 'NONE', *, *, #186726, .F. ) ;
#169587 = CARTESIAN_POINT ( 'NONE',  ( -7.306918443122272677, 7.489436036589583345, 0.7998128361456341429 ) ) ;
#169589 = LINE ( 'NONE', #105691, #211602 ) ;
#169590 = CARTESIAN_POINT ( 'NONE',  ( 0.1830476545506658226, -2.141193618969746471, -0.5335393285625378290 ) ) ;
#169591 = CARTESIAN_POINT ( 'NONE',  ( -10.20548264327394428, 4.735695117630401185, 6.229399736498809403 ) ) ;
#169592 = CARTESIAN_POINT ( 'NONE',  ( 3.994932754639446859, 0.2835094185691371393, 1.941019531709553103 ) ) ;
#169593 =( BOUNDED_CURVE ( )  B_SPLINE_CURVE ( 3, ( #10843, #27104, #95347, #112700 ),
 .UNSPECIFIED., .F., .T. ) 
 B_SPLINE_CURVE_WITH_KNOTS ( ( 4, 4 ),
 ( 4.837716811552755125, 4.862957253161376059 ),
 .UNSPECIFIED. ) 
 CURVE ( )  GEOMETRIC_REPRESENTATION_ITEM ( )  RATIONAL_B_SPLINE_CURVE ( ( 1.000000000000000000, 0.9999469107135832147, 0.9999469107135832147, 1.000000000000000000 ) ) 
 REPRESENTATION_ITEM ( '' )  );
#169594 = CARTESIAN_POINT ( 'NONE',  ( 7.853197290813620945, 10.18514947741448573, 1.599625672291281386 ) ) ;
#169595 = CARTESIAN_POINT ( 'NONE',  ( 2.057267738415057057, -1.238319999287675666, 1.591319116112683396 ) ) ;
#169596 = VERTEX_POINT ( 'NONE', #214113 ) ;
#169597 = CARTESIAN_POINT ( 'NONE',  ( 2.800141503465008341, -1.047918259751862147, -1.839804015593812458 ) ) ;
#169598 = CARTESIAN_POINT ( 'NONE',  ( -1.500000000000013101, 1.952083334016152527, 0.8660254037844403729 ) ) ;
#169599 = CARTESIAN_POINT ( 'NONE',  ( -4.394814349124112951, 8.279033840620114049, -0.7998128361456281477 ) ) ;
#169600 = CARTESIAN_POINT ( 'NONE',  ( 3.433393508698717511, 0.8267853122289525736, -1.645126075773599039 ) ) ;
#169601 = ORIENTED_EDGE ( 'NONE', *, *, #70447, .T. ) ;
#169602 = APPLICATION_CONTEXT ( 'automotive_design' ) ;
#169603 = CARTESIAN_POINT ( 'NONE',  ( -9.657485491635913633, 10.16148791653038330, 1.040834085586084257E-14 ) ) ;
#169604 = FILL_AREA_STYLE_COLOUR ( '', #165857 ) ;
#169605 = CARTESIAN_POINT ( 'NONE',  ( 3.920270587443940080, -2.114697630030224929, 0.1593259359235904837 ) ) ;
#169606 = DIRECTION ( 'NONE',  ( -0.1674078377062480916, 2.168404344971017388E-14, 0.9858877298529068467 ) ) ;
#169607 = CARTESIAN_POINT ( 'NONE',  ( 7.311924916471702396, 7.425000578838787391, -0.7998128361456281477 ) ) ;
#169608 = CARTESIAN_POINT ( 'NONE',  ( 5.747358702077526971, -1.621750911093680081, -1.271367298817957181 ) ) ;
#169610 = CARTESIAN_POINT ( 'NONE',  ( 2.032514702046281485, -1.644074058028240692, 0.8291662819630771786 ) ) ;
#169609 = CARTESIAN_POINT ( 'NONE',  ( -7.739006755302186846, 7.923262724141010516, 0.7998128361456462443 ) ) ;
#169611 = CARTESIAN_POINT ( 'NONE',  ( 10.09812548408005384, 10.67556790771522124, -0.7998128361456281477 ) ) ;
#169612 = CARTESIAN_POINT ( 'NONE',  ( -1.364683531250010295, 5.738541667008088432, -0.7879004041258300672 ) ) ;
#169613 = DIRECTION ( 'NONE',  ( -0.000000000000000000, -1.000000000000000000, -0.000000000000000000 ) ) ;
#169614 = CARTESIAN_POINT ( 'NONE',  ( 10.99856159529785060, -8.101932402265175526, -0.2004767358929940846 ) ) ;
#169615 = CARTESIAN_POINT ( 'NONE',  ( 2.543839704335303153, -1.636039663378138886, -1.481301067789652537 ) ) ;
#169616 = CARTESIAN_POINT ( 'NONE',  ( 3.550319795034285519, 2.262578822424826441, 0.004170446471787879993 ) ) ;
#169617 = CARTESIAN_POINT ( 'NONE',  ( -8.026063749610063525, 8.466088584074293877, -0.7216878364870278340 ) ) ;
#169618 = CARTESIAN_POINT ( 'NONE',  ( 3.093827002871222920, 1.152939038403834493, 1.397299590375496336 ) ) ;
#169619 = CARTESIAN_POINT ( 'NONE',  ( 4.083139574666094340, 1.542046283821847830, 1.136513224425585555 ) ) ;
#169620 = CARTESIAN_POINT ( 'NONE',  ( 1.364683531249990311, 4.196875000341417028, 1.214306433183764966E-14 ) ) ;
#169621 = ADVANCED_FACE ( 'NONE', ( #197896 ), #161156, .T. ) ;
#169622 = CARTESIAN_POINT ( 'NONE',  ( 4.012542200100970291, 1.395003824703803685, -1.393317042198267020 ) ) ;
#169623 = CARTESIAN_POINT ( 'NONE',  ( 1.166875649673270399, -1.740261045891202230, -0.8264182621567657261 ) ) ;
#169624 = CARTESIAN_POINT ( 'NONE',  ( 5.348468966913380029, 0.5439794105128460400, 1.789823788735760646 ) ) ;
#169625 = CARTESIAN_POINT ( 'NONE',  ( 3.211855371912860413, -0.4501829054360923510, 2.263203710529379187 ) ) ;
#169626 = CARTESIAN_POINT ( 'NONE',  ( 4.439814405351947713, 1.214877501302736862, 1.409928613244580742 ) ) ;
#169627 = FACE_OUTER_BOUND ( 'NONE', #25069, .T. ) ;
#169628 = CARTESIAN_POINT ( 'NONE',  ( 11.04536101718726293, 10.19999999999999929, 1.099999999999996758 ) ) ;
#169630 = CARTESIAN_POINT ( 'NONE',  ( 1.576933964714849701, -2.000244969732989819, -0.6594162861879059312 ) ) ;
#169629 = CARTESIAN_POINT ( 'NONE',  ( -4.080641047588914994, 5.783833860318930320, -1.443375672974051449 ) ) ;
#169631 = CARTESIAN_POINT ( 'NONE',  ( 4.989037339704528229, 4.922891105851139315, 1.040834085586084257E-14 ) ) ;
#169633 = CARTESIAN_POINT ( 'NONE',  ( -8.482597663644387609, 13.04811437422715414, -0.7998128361456281477 ) ) ;
#169632 = DIRECTION ( 'NONE',  ( 0.7592566023653005702, -0.6507913734559639396, 0.000000000000000000 ) ) ;
#169634 = CARTESIAN_POINT ( 'NONE',  ( 2.935903058640790597, -2.042584291827519660, 0.5695675404085094318 ) ) ;
#169635 = DIRECTION ( 'NONE',  ( 0.7771862570881703514, 0.6292706268317952434, 0.000000000000000000 ) ) ;
#169636 = CARTESIAN_POINT ( 'NONE',  ( 0.6330766797960291070, 1.867852534778514428, 0.7690482435470397116 ) ) ;
#169637 = CARTESIAN_POINT ( 'NONE',  ( 0.6823417656249899377, 0.5927083336747518416, 1.181850606188755259 ) ) ;
#169638 = CARTESIAN_POINT ( 'NONE',  ( -4.284013352238265959, 5.060732334775157604, -1.082531754730544860 ) ) ;
#169639 = CARTESIAN_POINT ( 'NONE',  ( 6.335737856287750880, 6.286115675290828264, -0.7998128361456281477 ) ) ;
#169640 = ORIENTED_EDGE ( 'NONE', *, *, #22794, .F. ) ;
#169641 = CARTESIAN_POINT ( 'NONE',  ( 2.161604200734370096, 0.3718190433680613749, -2.129227089361292791 ) ) ;
#169642 = CARTESIAN_POINT ( 'NONE',  ( 5.694061328059478733, 5.745419092265336758, -0.7216878364870484841 ) ) ;
#169644 = CARTESIAN_POINT ( 'NONE',  ( 2.738383840280328663, 5.178236332760252303, 1.082531754730548412 ) ) ;
#169643 = CARTESIAN_POINT ( 'NONE',  ( 6.249382461256315580, 6.255644057745969988, -0.7998128361456481317 ) ) ;
#169645 = CARTESIAN_POINT ( 'NONE',  ( 0.000000000000000000, 0.000000000000000000, 0.000000000000000000 ) ) ;
#169646 = CARTESIAN_POINT ( 'NONE',  ( 6.385953923436008317, -2.015982004707029596, 0.05432014494890363698 ) ) ;
#169647 = CARTESIAN_POINT ( 'NONE',  ( -7.524412065904404479, 11.72230514362308185, 0.000000000000000000 ) ) ;
#169648 = CARTESIAN_POINT ( 'NONE',  ( -0.07626876867936756288, -1.353788312843669406, -1.724171373301164767 ) ) ;
#169649 = DIRECTION ( 'NONE',  ( -1.000000000000000000, -3.451266460341925773E-31, -8.638326563840809144E-31 ) ) ;
#169651 = CARTESIAN_POINT ( 'NONE',  ( 1.364683531249997417, 12.48437500034139980, 2.602085213965210642E-15 ) ) ;
#169650 = CARTESIAN_POINT ( 'NONE',  ( 0.2513181340676704512, -1.814898432050582766, 1.350810986113021750 ) ) ;
#169652 = CARTESIAN_POINT ( 'NONE',  ( -9.820183334999905256, 10.35130206712171130, 1.040834085586084257E-14 ) ) ;
#169653 = CARTESIAN_POINT ( 'NONE',  ( -4.948362878863562742, 5.835806782504650236, 1.082531754730558626 ) ) ;
#169654 = CARTESIAN_POINT ( 'NONE',  ( -1.402160292154681736E-14, 1.759375000341421469, -1.575800808251659024 ) ) ;
#169655 = CARTESIAN_POINT ( 'NONE',  ( 0.7500000000000006661, 9.333333333333332149, 1.299038105676657340 ) ) ;
#169656 = CARTESIAN_POINT ( 'NONE',  ( 1.499999999999993117, 9.854166666666671404, 0.8660254037844409281 ) ) ;
#169657 = CARTESIAN_POINT ( 'NONE',  ( 3.914446297384760243, 1.218041307117226690, -1.221573883832317575 ) ) ;
#169658 = CARTESIAN_POINT ( 'NONE',  ( 4.193214648376505593, 8.114110533073061404, 0.000000000000000000 ) ) ;
#169659 = CARTESIAN_POINT ( 'NONE',  ( 1.967667936517076166, 0.9046490693802499150, 1.520878277628298303 ) ) ;
#169660 = CARTESIAN_POINT ( 'NONE',  ( 2.596342214666306880, -1.033070880159161264, 1.727660946855133606 ) ) ;
#169661 = CARTESIAN_POINT ( 'NONE',  ( 10.01963921569910632, 11.64833282552586091, 1.199719254218450271 ) ) ;
#169662 = CARTESIAN_POINT ( 'NONE',  ( 5.385833121705805304, 1.478444731487274399, 1.638484004604986000 ) ) ;
#169663 = ORIENTED_EDGE ( 'NONE', *, *, #140883, .F. ) ;
#169664 = CARTESIAN_POINT ( 'NONE',  ( -6.774234028683526532, 7.932303117332766718, 1.199719254218452047 ) ) ;
#169666 = CARTESIAN_POINT ( 'NONE',  ( 3.550407796516129366, -1.352142120786763213, 1.496064415113136592 ) ) ;
#169665 = CARTESIAN_POINT ( 'NONE',  ( 4.301511568767760529, 1.893648340000140040, -0.9544086401246790752 ) ) ;
#169667 = ORIENTED_EDGE ( 'NONE', *, *, #69490, .F. ) ;
#169668 = CARTESIAN_POINT ( 'NONE',  ( 5.734172623936983904, 5.654565914206774124, 0.7998128361456352531 ) ) ;
#169669 = EDGE_LOOP ( 'NONE', ( #181631, #61969, #18821 ) ) ;
#169670 = CARTESIAN_POINT ( 'NONE',  ( 1.569004590881703853, 0.1408476687595125731, -1.865417194689425795 ) ) ;
#169671 = CARTESIAN_POINT ( 'NONE',  ( -10.91819195543077470, -9.943514287384804362, 0.1813054759508214986 ) ) ;
#169672 = CARTESIAN_POINT ( 'NONE',  ( 5.725234622465176670, 1.600757532941178063, 0.8479277756611166561 ) ) ;
#169673 = CARTESIAN_POINT ( 'NONE',  ( -4.507082409677585666, 8.222350002982272699, 0.3272366024553932107 ) ) ;
#169674 = CARTESIAN_POINT ( 'NONE',  ( -9.348596576284975868, 2.999985932080179829, -7.001940380475246251 ) ) ;
#169675 = LINE ( 'NONE', #35396, #7232 ) ;
#169676 = CARTESIAN_POINT ( 'NONE',  ( 1.364683531249990311, 3.446875000341416584, 1.214306433183764966E-14 ) ) ;
#169677 = CARTESIAN_POINT ( 'NONE',  ( 0.000000000000000000, 0.000000000000000000, 0.000000000000000000 ) ) ;
#169678 = CARTESIAN_POINT ( 'NONE',  ( 6.861835142292147083, 7.178098218861903135, 0.7216878364870328300 ) ) ;
#169679 = CARTESIAN_POINT ( 'NONE',  ( 1.838261372102001800, -1.052240823716396267, 1.655630454418555830 ) ) ;
#169680 = CARTESIAN_POINT ( 'NONE',  ( -2.862179826260718762, 6.353310540697199471, 0.000000000000000000 ) ) ;
#169681 = CARTESIAN_POINT ( 'NONE',  ( -4.274563570058511175, 8.209017608368725405, 0.000000000000000000 ) ) ;
#169682 = CARTESIAN_POINT ( 'NONE',  ( 4.693665235656380830, 1.977662049654808740, -0.7657889336421249693 ) ) ;
#169684 = CARTESIAN_POINT ( 'NONE',  ( -10.71026998871754721, 6.055660674263378951, 4.667787751035539223 ) ) ;
#169683 = CARTESIAN_POINT ( 'NONE',  ( 2.480760062148268386, 4.021557182957057996, -11.67105848277438973 ) ) ;
#169685 = CARTESIAN_POINT ( 'NONE',  ( 5.659438124648599633, 0.3871718161991606344, -1.932801920045317257 ) ) ;
#169686 = CARTESIAN_POINT ( 'NONE',  ( 0.6823417656249882723, 1.426041667008083547, -1.181850606188749264 ) ) ;
#169687 = CARTESIAN_POINT ( 'NONE',  ( 1.336190909427417139, -1.121870850062630653, -1.671457199112064806 ) ) ;
#169688 = ORIENTED_EDGE ( 'NONE', *, *, #74664, .T. ) ;
#169689 = CARTESIAN_POINT ( 'NONE',  ( 1.581820014152079956, -0.7095999980938502150, 1.994918640774499430 ) ) ;
#169690 = CARTESIAN_POINT ( 'NONE',  ( 10.93263675336509522, 8.268585769907408789, -4.963831765784436634 ) ) ;
#169691 = CARTESIAN_POINT ( 'NONE',  ( 2.260293373024503616, -2.069953001785612479, 0.04851313490940312168 ) ) ;
#169692 = ORIENTED_EDGE ( 'NONE', *, *, #35147, .F. ) ;
#169693 = CARTESIAN_POINT ( 'NONE',  ( 5.228604516725597229, 6.129068686715179126, -1.199719254218450271 ) ) ;
#169694 = CARTESIAN_POINT ( 'NONE',  ( 6.886615681098613884, 6.999082814228660077, 0.000000000000000000 ) ) ;
#169695 = EDGE_LOOP ( 'NONE', ( #19871, #103957, #81250, #175645 ) ) ;
#169697 = CARTESIAN_POINT ( 'NONE',  ( 5.005985031943777308, 6.863401842066294556, -1.599625672291256295 ) ) ;
#169696 = CARTESIAN_POINT ( 'NONE',  ( 4.365234240191905535, 2.027873629061471838, -0.5078740465511691893 ) ) ;
#169700 = ORIENTED_EDGE ( 'NONE', *, *, #175957, .F. ) ;
#169699 = CARTESIAN_POINT ( 'NONE',  ( 1.629273880293732768, -0.2214294203813528539, 1.797790724094426418 ) ) ;
#169698 = CARTESIAN_POINT ( 'NONE',  ( 3.100428009929767637, -0.5284298666012043899, -1.747434388548900541 ) ) ;
#169701 = CARTESIAN_POINT ( 'NONE',  ( 6.235036409211808461, 0.2120174297785166195, 2.196685143856290878 ) ) ;
#169702 = CARTESIAN_POINT ( 'NONE',  ( 4.524592175135637717, 1.360519573838222085, -1.737388959189073878 ) ) ;
#169703 = CARTESIAN_POINT ( 'NONE',  ( 6.771407655021410399, 9.987393799911945536, -1.199719254218441611 ) ) ;
#169704 = CARTESIAN_POINT ( 'NONE',  ( 0.6823417656249969321, 9.838541667008065872, -1.181850606188757036 ) ) ;
#169705 = ORIENTED_EDGE ( 'NONE', *, *, #56772, .T. ) ;
#169706 = CARTESIAN_POINT ( 'NONE',  ( 4.002528454542265024, -1.891902218777557598, -0.2775262981309714605 ) ) ;
#169707 = CARTESIAN_POINT ( 'NONE',  ( -3.273404022695637572, 5.906389562198459231, 1.199719254218462483 ) ) ;
#169708 = CARTESIAN_POINT ( 'NONE',  ( 8.097244055859613709, 10.46987070330147063, -1.599625672291262513 ) ) ;
#169709 = CARTESIAN_POINT ( 'NONE',  ( 6.092251258522619395, 1.023830597077223903, -1.799436568697235783 ) ) ;
#169710 = CARTESIAN_POINT ( 'NONE',  ( -1.360316468750014884, 0.1927083336747308917, 0.7853790794158901356 ) ) ;
#169711 = CARTESIAN_POINT ( 'NONE',  ( 6.233935805145816467, 2.167428969419796125, 0.3234103439683775894 ) ) ;
#169712 = CARTESIAN_POINT ( 'NONE',  ( 5.943507298343291723, 7.226397084328657350, -1.228854570503196575 ) ) ;
#169713 = CARTESIAN_POINT ( 'NONE',  ( -6.723453079147375000, 15.44785978006343896, -9.895885313386967752 ) ) ;
#169714 = VERTEX_POINT ( 'NONE', #33270 ) ;
#169715 = ORIENTED_EDGE ( 'NONE', *, *, #23547, .F. ) ;
#169716 = CARTESIAN_POINT ( 'NONE',  ( 6.142902043169038429, 7.013529245237516641, 0.9864344219776898237 ) ) ;
#169717 = CARTESIAN_POINT ( 'NONE',  ( 3.163207368312019430, 0.2779861718534247794, -1.849665920529340646 ) ) ;
#169718 = CARTESIAN_POINT ( 'NONE',  ( -3.285556943750000070, -0.8968749995220438587, 0.000000000000000000 ) ) ;
#169719 = CARTESIAN_POINT ( 'NONE',  ( 4.245111494854632461, 7.966730820723463502, 0.000000000000000000 ) ) ;
#169720 = CARTESIAN_POINT ( 'NONE',  ( -6.887178846062109727, 10.01849717283904262, -1.082531754730537976 ) ) ;
#169721 = CARTESIAN_POINT ( 'NONE',  ( 4.061549535745618833, 6.896169004081968090, -1.199719254218452047 ) ) ;
#169722 = CARTESIAN_POINT ( 'NONE',  ( 0.6902129346560643697, 1.017158767820530940, -1.686321398027894825 ) ) ;
#169724 = CARTESIAN_POINT ( 'NONE',  ( 0.9488424731869498086, -1.824129051820524205, -0.8596123018156722750 ) ) ;
#169723 = B_SPLINE_CURVE_WITH_KNOTS ( 'NONE', 3,
 ( #42200, #90946, #73604, #38981, #25913, #159125, #55231 ),
 .UNSPECIFIED., .F., .F.,
 ( 4, 3, 4 ),
 ( 0.0001126021369344370733, 0.001503110988946918273, 0.002006790696425522769 ),
 .UNSPECIFIED. ) ;
#169725 = CARTESIAN_POINT ( 'NONE',  ( -9.429859533504656000, 10.96025652963230534, -1.199719254218441611 ) ) ;
#169726 = CARTESIAN_POINT ( 'NONE',  ( 5.020262018810099924, 9.078999131912302900, 0.7998128361456331437 ) ) ;
#169727 = DIRECTION ( 'NONE',  ( 0.000000000000000000, -0.000000000000000000, 1.000000000000000000 ) ) ;
#169728 = CARTESIAN_POINT ( 'NONE',  ( 1.886939110189549185, 1.905679594745551819, -1.081921739459410059 ) ) ;
#169729 = CARTESIAN_POINT ( 'NONE',  ( 5.795480788678070816, 1.385457615097264394, 1.189071861804301466 ) ) ;
#169730 = CARTESIAN_POINT ( 'NONE',  ( -4.243865776277440993, 4.909930479533815451, -1.199719254218446718 ) ) ;
#169731 = CARTESIAN_POINT ( 'NONE',  ( 5.560252395380206103, 8.540692657035327429, 1.082531754730547524 ) ) ;
#169732 = CARTESIAN_POINT ( 'NONE',  ( 10.01963921569910632, 11.64833282552586091, 1.199719254218450271 ) ) ;
#169733 = CARTESIAN_POINT ( 'NONE',  ( 5.027376032568989572, 4.759693547618927489, 0.7998128361456341429 ) ) ;
#169734 = CARTESIAN_POINT ( 'NONE',  ( 5.063044020060520900, 4.871582543017558109, 0.7998128361456352531 ) ) ;
#169735 = ORIENTED_EDGE ( 'NONE', *, *, #40172, .T. ) ;
#169737 = CARTESIAN_POINT ( 'NONE',  ( 0.4342398884448725460, -1.078799894535716231, -1.699460183843485073 ) ) ;
#169736 = CARTESIAN_POINT ( 'NONE',  ( 4.106863108761789505, -0.3106082297497716471, 1.814695527881895476 ) ) ;
#169738 = CARTESIAN_POINT ( 'NONE',  ( 2.003655084434956102, 2.273349380270474729, 0.3377564834418695927 ) ) ;
#169740 = CARTESIAN_POINT ( 'NONE',  ( 0.2505320230819003680, -0.3960800208489853036, -1.824604621477694311 ) ) ;
#169739 = CARTESIAN_POINT ( 'NONE',  ( 4.555176424511575561, 4.416720038126027426, -0.7216878364870188411 ) ) ;
#169741 = CARTESIAN_POINT ( 'NONE',  ( 2.960183410750786059, -4.109567543049581495, -1.425552035297093623 ) ) ;
#169742 = CARTESIAN_POINT ( 'NONE',  ( -4.822949958159302497, 6.649860922651058992, -1.599625672291256295 ) ) ;
#169743 =( NAMED_UNIT ( * ) SI_UNIT ( $, .STERADIAN. ) SOLID_ANGLE_UNIT ( ) );
#169744 = CARTESIAN_POINT ( 'NONE',  ( 4.429883728109570207, -1.874397765517330061, 0.3784635845696313061 ) ) ;
#169745 = CARTESIAN_POINT ( 'NONE',  ( -9.982881178363895103, 10.54111621771303753, 1.040834085586084257E-14 ) ) ;
#169747 = EDGE_CURVE ( 'NONE', #15455, #29554, #57429, .T. ) ;
#169746 = CARTESIAN_POINT ( 'NONE',  ( 6.492781079782697695, 6.747302000852300807, 0.03582484399037785816 ) ) ;
#169748 = CARTESIAN_POINT ( 'NONE',  ( -3.122120512896910505, 6.864500708346841229, 0.7998128361456352531 ) ) ;
#169750 = CARTESIAN_POINT ( 'NONE',  ( 0.9009904985227291663, 1.526999960511504772, 1.080287613699250304 ) ) ;
#169749 = CARTESIAN_POINT ( 'NONE',  ( 3.052369502041663019, -1.581437162565798804, 1.367655637459828544 ) ) ;
#169751 = CARTESIAN_POINT ( 'NONE',  ( 8.948018195339340508, 9.541702104091804415, -0.7216878364870197293 ) ) ;
#169752 = CARTESIAN_POINT ( 'NONE',  ( 1.364683531249990311, 4.926041667008084879, 0.7879004041258499402 ) ) ;
#169753 = CARTESIAN_POINT ( 'NONE',  ( 3.368457041919175055, 0.03905506635776007096, -1.740168019110074793 ) ) ;
#169754 = AXIS2_PLACEMENT_3D ( 'NONE', #63403, #180352, #129556 ) ;
#169755 = CARTESIAN_POINT ( 'NONE',  ( 3.174580523894166006, 6.855427711185178019, 0.7998128361456341429 ) ) ;
#169756 = FACE_OUTER_BOUND ( 'NONE', #196878, .T. ) ;
#169757 = CARTESIAN_POINT ( 'NONE',  ( 4.230855031843249847, 0.08773280417345018234, 1.722775095924995004 ) ) ;
#169758 = CARTESIAN_POINT ( 'NONE',  ( 3.755584314896889264, 2.174856280799509545, -0.2696606696684644700 ) ) ;
#169759 = CARTESIAN_POINT ( 'NONE',  ( 5.883472226557855400, 2.040502603023553796, -0.8411249186189362348 ) ) ;
#169760 = DIRECTION ( 'NONE',  ( 0.000000000000000000, -1.000000000000000000, 0.000000000000000000 ) ) ;
#169761 = CARTESIAN_POINT ( 'NONE',  ( 3.292005203939939229, -1.454527599200394539, -1.611992012647659900 ) ) ;
#169762 = CARTESIAN_POINT ( 'NONE',  ( 1.664397423953474009, -1.292156093668932693, 1.290017532847971271 ) ) ;
#169763 = CARTESIAN_POINT ( 'NONE',  ( 0.4265131056294459433, -1.285834093136655643, 1.481649512794058321 ) ) ;
#169764 = CARTESIAN_POINT ( 'NONE',  ( 4.118443911689470660, 2.077242944681048975, 0.4093182092978660536 ) ) ;
#169765 = ORIENTED_EDGE ( 'NONE', *, *, #381, .T. ) ;
#169767 = CARTESIAN_POINT ( 'NONE',  ( 1.364683531249988535, 2.967708333674755394, -0.7879004041258239610 ) ) ;
#169766 = CARTESIAN_POINT ( 'NONE',  ( 4.898102649693969468, -0.7706710736265044437, -2.159050251936722731 ) ) ;
#169768 = CARTESIAN_POINT ( 'NONE',  ( 6.620655732516643965, 2.083750514537034970, 2.135603474206409835 ) ) ;
#169769 = CARTESIAN_POINT ( 'NONE',  ( 2.381428537494710618, 5.930083727052461562, 0.7998128361456462443 ) ) ;
#169770 = CARTESIAN_POINT ( 'NONE',  ( 0.8562900302464396818, 0.8558255631127342777, -1.940287777186230578 ) ) ;
#169771 = CARTESIAN_POINT ( 'NONE',  ( -4.107757355260591936, 7.736207981205250661, 1.040834085586084257E-14 ) ) ;
#169772 = CARTESIAN_POINT ( 'NONE',  ( 5.356880090730872013, 6.382686539675070492, 1.082531754730549078 ) ) ;
#169773 = CARTESIAN_POINT ( 'NONE',  ( -5.165293336682207581, 8.009630745229104676, 1.082531754730548412 ) ) ;
#169774 = EDGE_CURVE ( 'NONE', #95128, #19248, #104447, .T. ) ;
#169776 = CARTESIAN_POINT ( 'NONE',  ( 0.7500000000000006661, 11.61458333401613174, 1.299038105676657340 ) ) ;
#169775 = CARTESIAN_POINT ( 'NONE',  ( -10.99916818177030287, -10.00038292658551420, 0.1458870414460790577 ) ) ;
#169777 = ORIENTED_EDGE ( 'NONE', *, *, #38831, .F. ) ;
#169778 = CARTESIAN_POINT ( 'NONE',  ( 4.992814645674492624, -2.006446365708704160, 0.2004330516618065550 ) ) ;
#169780 = CARTESIAN_POINT ( 'NONE',  ( 4.768458259026512103, -0.8772815012083650110, -1.866809563962401164 ) ) ;
#169779 = CARTESIAN_POINT ( 'NONE',  ( 4.822949958159288286, 6.649860922651058992, -1.599625672291256295 ) ) ;
#169782 = CARTESIAN_POINT ( 'NONE',  ( 6.883263157960393563, 4.695771316066229772, 2.508818740863460572 ) ) ;
#169781 = CARTESIAN_POINT ( 'NONE',  ( 5.020262018810099924, 9.078999131912302900, 0.7998128361456331437 ) ) ;
#169783 = CARTESIAN_POINT ( 'NONE',  ( 7.364013710877980401, 8.620379413226322285, -1.199719254218452047 ) ) ;
#169784 = CARTESIAN_POINT ( 'NONE',  ( 1.642778471875001811, -2.092708332855373943, 2.845375778867859751 ) ) ;
#169785 = FACE_OUTER_BOUND ( 'NONE', #68443, .T. ) ;
#169786 = CARTESIAN_POINT ( 'NONE',  ( 0.6211766780156646739, -1.984520161701831986, 0.6578015034230285663 ) ) ;
#169787 = CARTESIAN_POINT ( 'NONE',  ( 4.940077362011475515, -1.704937458037486531, -1.076318853994034930 ) ) ;
#169788 = CARTESIAN_POINT ( 'NONE',  ( 2.858754248528099229, 0.2676582106064147593, -1.821554178878769470 ) ) ;
#169789 = CARTESIAN_POINT ( 'NONE',  ( 5.843727902690005749, 6.776436293681846301, -1.199719254218445830 ) ) ;
#169790 =( LENGTH_UNIT ( ) NAMED_UNIT ( * ) SI_UNIT ( .MILLI., .METRE. ) );
#169791 = CARTESIAN_POINT ( 'NONE',  ( 0.3051044079889728144, -0.4676614632079054701, 1.660094367756638434 ) ) ;
#169792 = CARTESIAN_POINT ( 'NONE',  ( 4.161989969715248705, 4.726297878971393196, -2.420000000000000373 ) ) ;
#169793 = CARTESIAN_POINT ( 'NONE',  ( 0.6164066528375180543, 0.1772060041554945342, 2.291936309153388862 ) ) ;
#169794 = CARTESIAN_POINT ( 'NONE',  ( -5.551173829791513192, 8.563787670477010394, 1.199719254218452047 ) ) ;
#169795 = CARTESIAN_POINT ( 'NONE',  ( 0.5974158272751062260, 1.880195615759198136, -1.258034406164424635 ) ) ;
#169796 = CARTESIAN_POINT ( 'NONE',  ( 2.666745002694201450, -1.451881433263510601, 1.525875076051644408 ) ) ;
#169797 = CARTESIAN_POINT ( 'NONE',  ( -4.797606254389363833, 6.690569611577942943, 1.599625672291263179 ) ) ;
#169798 = CARTESIAN_POINT ( 'NONE',  ( 8.274553823041976841, 8.548067636504127265, 1.040834085586084257E-14 ) ) ;
#169799 = CARTESIAN_POINT ( 'NONE',  ( 5.356880090730857802, 8.303424968277756335, 1.082531754730548412 ) ) ;
#169800 = CARTESIAN_POINT ( 'NONE',  ( 5.656250000000004441, -1.895863743163955339, 0.7852924748302813063 ) ) ;
#169801 = CARTESIAN_POINT ( 'NONE',  ( -5.391338639728555648, 9.441645512991978961, -0.7998128361456231517 ) ) ;
#169802 = CARTESIAN_POINT ( 'NONE',  ( 6.521108698048765362, 8.631046119188804155, -1.443375672974058777 ) ) ;
#169803 = CARTESIAN_POINT ( 'NONE',  ( 5.529887635128906354, 6.401445659467410287, 1.229860404580757072 ) ) ;
#169804 = CARTESIAN_POINT ( 'NONE',  ( -3.653032323878261600, 6.349289246911547835, -1.199719254218452047 ) ) ;
#169805 = CARTESIAN_POINT ( 'NONE',  ( 3.498459270752065198, -1.092227124545399164, 1.934249878339290740 ) ) ;
#169806 = CARTESIAN_POINT ( 'NONE',  ( 1.816621679704206516, 2.045545470589833492, 0.7867152234099920038 ) ) ;
#169807 = CARTESIAN_POINT ( 'NONE',  ( -5.280010757518168063, 8.247430752824802980, -1.199719254218446718 ) ) ;
#169808 = CARTESIAN_POINT ( 'NONE',  ( -4.664887371553763096, 7.600063145858131364, -1.199719254218453823 ) ) ;
#169809 = CARTESIAN_POINT ( 'NONE',  ( 5.705508943770692731, -1.545575431542939970, -1.208212526538715137 ) ) ;
#169810 = B_SPLINE_CURVE_WITH_KNOTS ( 'NONE', 3,
 ( #186223, #89829, #138568, #187296, #87671, #155877, #103934, #36775 ),
 .UNSPECIFIED., .F., .F.,
 ( 4, 2, 2, 4 ),
 ( 1.301042606982573158E-18, 0.0002224730689913829963, 0.0004449461379827646915, 0.0008898922759655280819 ),
 .UNSPECIFIED. ) ;
#169811 = PRESENTATION_LAYER_ASSIGNMENT (  '', '', ( #107226 ) ) ;
#169812 = CARTESIAN_POINT ( 'NONE',  ( -0.6823417656250212460, 1.801041667008083991, 1.181850606188755259 ) ) ;
#169813 = CARTESIAN_POINT ( 'NONE',  ( -5.167065940583949413, 5.200867483535597913, 0.000000000000000000 ) ) ;
#169814 = CARTESIAN_POINT ( 'NONE',  ( -5.910991785878175975, 6.958873840688411860, -1.082531754730544860 ) ) ;
#169815 = COLOUR_RGB ( '', 0.09019608, 0.27058824, 0.51372549) ;
#169816 = CARTESIAN_POINT ( 'NONE',  ( 4.570628194609677841, 0.8141925398062774821, 1.958264201954627026 ) ) ;
#169817 = CARTESIAN_POINT ( 'NONE',  ( -5.334207092333882017, 5.187939460669764635, 0.7998128361456281477 ) ) ;
#169818 = ORIENTED_EDGE ( 'NONE', *, *, #46527, .T. ) ;
#169820 = CARTESIAN_POINT ( 'NONE',  ( 6.069229152942410721, 0.1638285306290178100, -2.155560115052157055 ) ) ;
#169819 = CARTESIAN_POINT ( 'NONE',  ( -6.455090533882213322, 6.703562842383589349, -0.7216878364870338292 ) ) ;
#169821 = CARTESIAN_POINT ( 'NONE',  ( 5.307127064745490230, 8.279066444590018392, -1.199719254218452935 ) ) ;
#169822 = CARTESIAN_POINT ( 'NONE',  ( 5.354971380013192395, 0.3533838956982695567, -1.806849549699687696 ) ) ;
#169823 = PRESENTATION_LAYER_ASSIGNMENT (  '', '', ( #17652 ) ) ;
#169824 = CARTESIAN_POINT ( 'NONE',  ( 1.004302930252168075E-16, 6.999999999999999112, 1.500000000000005107 ) ) ;
#169825 = CARTESIAN_POINT ( 'NONE',  ( -1.364683531250012516, 2.342708333674752286, 0.7879004041258379498 ) ) ;
#169826 = CARTESIAN_POINT ( 'NONE',  ( 6.474529609311859168, -0.09325562727019585940, -1.737965710822095389 ) ) ;
#169827 = CARTESIAN_POINT ( 'NONE',  ( 11.43190902327452108, 12.44477871742131825, 3.649704988378163595 ) ) ;
#169828 = CARTESIAN_POINT ( 'NONE',  ( 0.007473969438204840048, 8.279395425053873936, 1.999986034896453324 ) ) ;
#169829 = DIRECTION ( 'NONE',  ( 1.000000000000000000, -0.000000000000000000, -0.000000000000000000 ) ) ;
#169830 = CARTESIAN_POINT ( 'NONE',  ( 4.768538688506021472, -1.414568798902924307, 1.634688457493836289 ) ) ;
#169831 = CARTESIAN_POINT ( 'NONE',  ( -4.894657149733403045, 5.669187081899118574, -1.199719254218446718 ) ) ;
#169832 = CARTESIAN_POINT ( 'NONE',  ( -6.683806541412768532, 8.820860269780128604, -1.443375672974058777 ) ) ;
#169833 = CARTESIAN_POINT ( 'NONE',  ( 4.803692121107413726, -0.5798474923815257753, 2.082409481564663434 ) ) ;
#169834 = CARTESIAN_POINT ( 'NONE',  ( 5.114510421747438862, 1.361449769532377729, -1.425934698893965402 ) ) ;
#169835 = CARTESIAN_POINT ( 'NONE',  ( 3.883936887208380373, -0.1284340723075507729, 1.729154583330833272 ) ) ;
#169836 = CARTESIAN_POINT ( 'NONE',  ( 0.9256184737543894370, -1.394389637717853514, -1.690728713229103342 ) ) ;
#169837 = CARTESIAN_POINT ( 'NONE',  ( 2.749405113950495583, -1.918974089273906003, 1.281321877411125909 ) ) ;
#169838 = CARTESIAN_POINT ( 'NONE',  ( 3.673166697908346379, 0.05419028943656278852, -2.060251915681856616 ) ) ;
#169839 = CARTESIAN_POINT ( 'NONE',  ( 5.583525073002030048, -0.8696438758921558598, 1.736526053206193243 ) ) ;
#169840 = CARTESIAN_POINT ( 'NONE',  ( -8.066738210006693777, 10.43428054980638997, 1.443375672974090751 ) ) ;
#169841 = CARTESIAN_POINT ( 'NONE',  ( -4.620296487206990932, 8.612372678375294299, 0.000000000000000000 ) ) ;
#169842 = FACE_OUTER_BOUND ( 'NONE', #28764, .T. ) ;
#169843 = CARTESIAN_POINT ( 'NONE',  ( -5.002032328799064231, 4.800402236545811441, -0.7998128361456362523 ) ) ;
#169844 = CARTESIAN_POINT ( 'NONE',  ( -5.870317324592805086, 9.792527945426188651, -0.7216878364870197293 ) ) ;
#169845 = CARTESIAN_POINT ( 'NONE',  ( 2.854729849855553780, 0.7423848465729752100, 2.078289375090878632 ) ) ;
#169846 = CARTESIAN_POINT ( 'NONE',  ( -1.642778471875000035, -2.705208332855375986, -2.845375778867859751 ) ) ;
#169847 = ORIENTED_EDGE ( 'NONE', *, *, #117853, .T. ) ;
#169848 = CARTESIAN_POINT ( 'NONE',  ( 1.147037741594110427, 1.644639672688326559, -0.8707446802224245719 ) ) ;
#169849 = CARTESIAN_POINT ( 'NONE',  ( -0.1288028175206725467, 0.2223783146117243037, -2.307352578052775272 ) ) ;
#169850 = CARTESIAN_POINT ( 'NONE',  ( -9.520891725235959058, -8.148349307653482754, 0.3199376857464493740 ) ) ;
#169852 = CARTESIAN_POINT ( 'NONE',  ( 6.825078400183572036, 7.051914997414900022, 2.742498282622223726 ) ) ;
#169851 = CARTESIAN_POINT ( 'NONE',  ( -6.434009798946909164, 6.877700593631734804, -0.7366733183416813713 ) ) ;
#169853 = CARTESIAN_POINT ( 'NONE',  ( 11.97929049433705373, 13.88000000000000078, 0.7046979865771783036 ) ) ;
#169854 = VERTEX_POINT ( 'NONE', #182714 ) ;
#169855 = CARTESIAN_POINT ( 'NONE',  ( 3.819256682291353400, -0.1532216265913727837, 2.055260608361098473 ) ) ;
#169856 = CARTESIAN_POINT ( 'NONE',  ( -1.360316468750007779, 0.1406250003413919702, -1.734723475976807094E-15 ) ) ;
#169857 = CARTESIAN_POINT ( 'NONE',  ( -5.555090253297260361, 7.504024600312024340, 1.599625672291269396 ) ) ;
#169858 = CARTESIAN_POINT ( 'NONE',  ( -4.450808633097256717, 7.987047222781189504, 2.500000000000000888 ) ) ;
#169859 = CARTESIAN_POINT ( 'NONE',  ( 3.765413976293345844, 5.416068943807445635, 1.599625672291267398 ) ) ;
#169860 = CARTESIAN_POINT ( 'NONE',  ( 2.360294219997323140, 0.8799647281299802781, 1.863710983410723943 ) ) ;
#169862 = CARTESIAN_POINT ( 'NONE',  ( -0.6823417656250003738, 13.90104166700806232, 1.181850606188754593 ) ) ;
#169861 = CARTESIAN_POINT ( 'NONE',  ( -1.500000000000015099, 12.47916666666666785, -0.8660254037844309360 ) ) ;
#169863 = CARTESIAN_POINT ( 'NONE',  ( 4.808338034340912337, 8.761478140039733020, 1.040834085586084257E-14 ) ) ;
#169864 = CARTESIAN_POINT ( 'NONE',  ( 5.690102719724574598, -0.9953569382129350274, 1.969734210959340093 ) ) ;
#169865 = CARTESIAN_POINT ( 'NONE',  ( 6.643838010208884981, 0.8751278368869718216, -2.086507859592637626 ) ) ;
#169866 = CARTESIAN_POINT ( 'NONE',  ( -5.314433026876900001, 6.262888621853549331, 1.082531754730548412 ) ) ;
#169867 = CARTESIAN_POINT ( 'NONE',  ( 1.253139057289072822, 0.1435168058863903473, -2.011451928166609893 ) ) ;
#169868 = EDGE_CURVE ( 'NONE', #39263, #145242, #149155, .T. ) ;
#169869 = CARTESIAN_POINT ( 'NONE',  ( 6.217437059193512638, 1.592560689453832001, 1.058264445519964125 ) ) ;
#169870 = SURFACE_STYLE_USAGE ( .BOTH. , #67012 ) ;
#169871 = AXIS2_PLACEMENT_3D ( 'NONE', #101408, #167481, #27360 ) ;
#169872 = CARTESIAN_POINT ( 'NONE',  ( 2.008475284031425723, 1.387998011844304491, -1.254312187223500796 ) ) ;
#169873 = CARTESIAN_POINT ( 'NONE',  ( 3.344935638061694139, -1.780668040901035143, -0.9463001528628791625 ) ) ;
#169875 = CARTESIAN_POINT ( 'NONE',  ( 6.639320575229257670, 0.5729255850590134758, 2.155858052613166986 ) ) ;
#169874 = CARTESIAN_POINT ( 'NONE',  ( -0.6823417656250003738, 1.217708333674752286, -1.181850606188749264 ) ) ;
#169877 = CARTESIAN_POINT ( 'NONE',  ( 4.986996339425863844, -0.2567466434181593371, -2.090293495131962942 ) ) ;
#169876 = CARTESIAN_POINT ( 'NONE',  ( -8.050844288416501016, 8.287073179441051707, 1.040834085586084257E-14 ) ) ;
#169878 = CARTESIAN_POINT ( 'NONE',  ( 5.933664784275179294, 10.07435934829639912, -0.7998128361456291469 ) ) ;
#169880 = CARTESIAN_POINT ( 'NONE',  ( -8.037286134802835491, 8.271255333558444889, -0.7998128361456291469 ) ) ;
#169879 = CARTESIAN_POINT ( 'NONE',  ( 4.492547798081839794, 6.334668079219206049, 1.599625672291262513 ) ) ;
#169881 = CARTESIAN_POINT ( 'NONE',  ( -0.2633404184769205236, -6.747343053191835693, -9.488968570712991379 ) ) ;
#169882 = CARTESIAN_POINT ( 'NONE',  ( 3.955335691828856692, -1.755346444749112722, 0.9990557238469994772 ) ) ;
#169883 = CARTESIAN_POINT ( 'NONE',  ( -1.364683531249997417, 5.009375000341425022, 1.214306433183764966E-14 ) ) ;
#169884 = EDGE_CURVE ( 'NONE', #45649, #1299, #79911, .T. ) ;
#169885 = CARTESIAN_POINT ( 'NONE',  ( 0.2509072133702301421, -0.4515964501156078392, -2.020277220192217449 ) ) ;
#169886 = CARTESIAN_POINT ( 'NONE',  ( 7.402388683381404988, 10.61957531637824204, -1.082531754730537976 ) ) ;
#169887 = CARTESIAN_POINT ( 'NONE',  ( 5.782550318682353918, -2.107506929020441788, -0.4798289361013233223 ) ) ;
#169888 = CARTESIAN_POINT ( 'NONE',  ( 5.365994935958575240, 9.482354201918870018, 0.7998128361456341429 ) ) ;
#169889 = CARTESIAN_POINT ( 'NONE',  ( -1.364683531250000748, -0.9281249996585805295, 0.000000000000000000 ) ) ;
#169891 = LINE ( 'NONE', #6310, #44970 ) ;
#169890 = CARTESIAN_POINT ( 'NONE',  ( 6.852720297064418986, 6.959538199522133262, 0.7998128361456331437 ) ) ;
#169892 = CARTESIAN_POINT ( 'NONE',  ( 6.575341312503417690, 10.61505593132193326, -0.7216878364870267237 ) ) ;
#169894 = CARTESIAN_POINT ( 'NONE',  ( 2.493766133720156652, 8.265889183060442846, 2.456386456769295901 ) ) ;
#169893 = CARTESIAN_POINT ( 'NONE',  ( 3.631445352573436480, 0.05657863903951602241, -2.170607583040237820 ) ) ;
#169896 = CARTESIAN_POINT ( 'NONE',  ( 1.997363575765517485, -1.840834563946552649, 0.04656924640939614363 ) ) ;
#169895 = CARTESIAN_POINT ( 'NONE',  ( -5.260200412422208593, 7.159986452624450770, -1.443375672974053447 ) ) ;
#169897 = CARTESIAN_POINT ( 'NONE',  ( 1.364683531249988535, 3.155208333674756283, -0.7879004041258239610 ) ) ;
#169898 = CARTESIAN_POINT ( 'NONE',  ( 2.823975127348025804, 1.215230906543849354, -1.823574674616668556 ) ) ;
#169899 = CARTESIAN_POINT ( 'NONE',  ( 6.983263157960387879, 4.689051080487334211, 2.716346346018564617 ) ) ;
#169900 = CARTESIAN_POINT ( 'NONE',  ( 4.610415411315283762, -0.9635332438130711497, -2.047219928730920291 ) ) ;
#169902 = CARTESIAN_POINT ( 'NONE',  ( -6.368579470117215813, 8.453095353268645695, 1.599625672291283607 ) ) ;
#169901 = B_SPLINE_CURVE_WITH_KNOTS ( 'NONE', 3,
 ( #132231, #100749, #49878, #2152 ),
 .UNSPECIFIED., .F., .F.,
 ( 4, 4 ),
 ( 0.002966363312150372029, 0.003746507044012918359 ),
 .UNSPECIFIED. ) ;
#169903 = CARTESIAN_POINT ( 'NONE',  ( -11.81900460097218186, 9.842428651258600780, 1.592493057836596115 ) ) ;
#169904 = CARTESIAN_POINT ( 'NONE',  ( 6.119462805442048570, 6.996221746119736018, -0.9567421715909133484 ) ) ;
#169905 = COLOUR_RGB ( '', 0.72549020, 0.75294118, 0.79215686) ;
#169906 = CARTESIAN_POINT ( 'NONE',  ( -1.402160292154681736E-14, 13.06249999999999822, 1.732050807568881190 ) ) ;
#169907 = CARTESIAN_POINT ( 'NONE',  ( -5.221298554594238084, 8.145246509451649075, 1.082531754730549967 ) ) ;
#169908 = CARTESIAN_POINT ( 'NONE',  ( 5.885648082108190238, 7.959951743916638733, 1.443375672974065660 ) ) ;
#169909 = CARTESIAN_POINT ( 'NONE',  ( 5.870295291196549137, -1.121585077578592049, 1.368893044642209178 ) ) ;
#169910 = CARTESIAN_POINT ( 'NONE',  ( 7.259501185113382604, 10.55683625168592243, -1.199719254218441611 ) ) ;
#169911 = CARTESIAN_POINT ( 'NONE',  ( 1.923017885777689839, 1.964713842245609410, 0.7587240108328905386 ) ) ;
#169914 = EDGE_CURVE ( 'NONE', #107037, #146253, #166353, .T. ) ;
#169913 = CARTESIAN_POINT ( 'NONE',  ( 1.499999999999987121, 2.004166666666684637, 0.8660254037844524744 ) ) ;
#169912 = CARTESIAN_POINT ( 'NONE',  ( -1.402160292154681736E-14, 12.42187500034139802, 1.575800808251682339 ) ) ;
#169915 = CARTESIAN_POINT ( 'NONE',  ( 1.926157630473192217, 1.009716079121532495, 1.690873403599216562 ) ) ;
#169916 = CARTESIAN_POINT ( 'NONE',  ( -3.902768115887413014, 5.646591783325653147, -1.599625672291283607 ) ) ;
#169917 = CARTESIAN_POINT ( 'NONE',  ( 0.3089402658475807195, -1.578002999302514642, 1.165503548361209063 ) ) ;
#169919 = ORIENTED_EDGE ( 'NONE', *, *, #205893, .T. ) ;
#169918 = CARTESIAN_POINT ( 'NONE',  ( 5.818593503215891971, -0.6604613111419742610, -1.687090931240011527 ) ) ;
#169920 = CARTESIAN_POINT ( 'NONE',  ( 5.165293337126522388, 8.969999960048859577, 1.040834085586084257E-14 ) ) ;
#169921 =( GEOMETRIC_REPRESENTATION_CONTEXT ( 3 ) GLOBAL_UNCERTAINTY_ASSIGNED_CONTEXT ( ( #20396 ) ) GLOBAL_UNIT_ASSIGNED_CONTEXT ( ( #111707, #25043, #61823 ) ) REPRESENTATION_CONTEXT ( 'NONE', 'WORKASPACE' ) );
#169922 = CARTESIAN_POINT ( 'NONE',  ( -0.6823417656250246877, -1.136458332991911790, 1.181850606188755259 ) ) ;
#169923 = CARTESIAN_POINT ( 'NONE',  ( 4.785944050937030347, -0.8815013282119156246, 1.649949660215948688 ) ) ;
#169924 = CARTESIAN_POINT ( 'NONE',  ( 6.016483110937820733, 0.8336820848486149460, 1.895147399281302603 ) ) ;
#169925 = CARTESIAN_POINT ( 'NONE',  ( 10.64229060209986599, 1.016282880930355681, 6.144329343916449027 ) ) ;
#169926 = CARTESIAN_POINT ( 'NONE',  ( -5.939880696118548187, 6.102484698325975288, 0.000000000000000000 ) ) ;
#169927 = CARTESIAN_POINT ( 'NONE',  ( 1.499999999999989120, 1.025000000000019007, 0.000000000000000000 ) ) ;
#169928 = CARTESIAN_POINT ( 'NONE',  ( 7.938462636001388795, 9.220293482545153907, -1.199719254218441611 ) ) ;
#169929 = CARTESIAN_POINT ( 'NONE',  ( -9.504429378379839477, 11.04725468198666150, 1.199719254218462483 ) ) ;
#169930 = CARTESIAN_POINT ( 'NONE',  ( 5.559725510055676168, 8.644040974110419384, 1.199719254218451159 ) ) ;
#169931 = EDGE_CURVE ( 'NONE', #12134, #94066, #34919, .T. ) ;
#169932 = CARTESIAN_POINT ( 'NONE',  ( 0.6823417656249882723, -0.6572916663252492686, 1.181850606188755259 ) ) ;
#169933 = CARTESIAN_POINT ( 'NONE',  ( -1.201851678989727383E-14, 0.9625000000000237810, 1.732050807568877637 ) ) ;
#169935 = CARTESIAN_POINT ( 'NONE',  ( 4.202137545231717120, 6.989912005157271402, 1.199719254218462483 ) ) ;
#169934 = CARTESIAN_POINT ( 'NONE',  ( 4.879329150013382410, -0.09822140645733207220, 1.959542894978071992 ) ) ;
#169936 = CARTESIAN_POINT ( 'NONE',  ( 2.952499795743710020, 1.423742661936340470, 1.427719607385954381 ) ) ;
#169937 = CARTESIAN_POINT ( 'NONE',  ( 2.378032431427847371, -1.910899176573145342, -0.1362895805000780836 ) ) ;
#169938 = CARTESIAN_POINT ( 'NONE',  ( 1.836970198721030181E-16, 13.49999999999999822, 1.500000000000000222 ) ) ;
#169939 = CARTESIAN_POINT ( 'NONE',  ( 0.8553300576445364012, 0.4222666777726029608, -2.150330908352434012 ) ) ;
#169940 = CARTESIAN_POINT ( 'NONE',  ( -11.87815913191726480, 9.796921793685831048, 1.708869976696563597 ) ) ;
#169941 = CARTESIAN_POINT ( 'NONE',  ( 2.600682448077856090, 1.504852936121018558, -1.110837741034584436 ) ) ;
#169942 = CARTESIAN_POINT ( 'NONE',  ( -1.201851678989727383E-14, 4.946875000341420581, -1.575800808251660134 ) ) ;
#169943 = CARTESIAN_POINT ( 'NONE',  ( 4.078389064453043389, 0.9529185939490876223, 1.773430079992607045 ) ) ;
#169944 = CARTESIAN_POINT ( 'NONE',  ( -9.345647958521597687, 9.797677461230342999, 0.7998128361456462443 ) ) ;
#169946 = CARTESIAN_POINT ( 'NONE',  ( 4.622735098982394319, 0.3634473554468270473, 2.085661844363582595 ) ) ;
#169945 = CARTESIAN_POINT ( 'NONE',  ( -6.263503779833496488, 6.409768619334935913, 0.7216878364870317197 ) ) ;
#169947 = CARTESIAN_POINT ( 'NONE',  ( 5.934052368846653991, 1.230181698326970885, 1.665117723180092213 ) ) ;
#169949 = CARTESIAN_POINT ( 'NONE',  ( 6.720655732516647163, 2.019696082639847567, 2.477441386028636394 ) ) ;
#169948 = CARTESIAN_POINT ( 'NONE',  ( 1.646151360528936625, 0.6591259108063004524, 1.984184313626126350 ) ) ;
#169951 = ORIENTED_EDGE ( 'NONE', *, *, #212216, .F. ) ;
#169950 = CARTESIAN_POINT ( 'NONE',  ( 5.965807262869926575, 1.798080572464531679, -0.3147057940002598864 ) ) ;
#169952 = CARTESIAN_POINT ( 'NONE',  ( 6.913768267964901071, 10.15348118167935709, -1.199719254218441611 ) ) ;
#169953 = DIRECTION ( 'NONE',  ( -1.544526636936600361E-14, -1.000000000000000000, -1.522060196430166414E-14 ) ) ;
#169954 = FACE_BOUND ( 'NONE', #139091, .T. ) ;
#169955 = CARTESIAN_POINT ( 'NONE',  ( -9.399990540229763880, 5.000000000000003553, 6.933248713717822476 ) ) ;
#169956 = CARTESIAN_POINT ( 'NONE',  ( 6.439759776366765998, 9.496508258194486629, 1.082531754730558626 ) ) ;
#169957 = CARTESIAN_POINT ( 'NONE',  ( -1.913201741516695087, 3.249623237789911023, 0.4478572873795984566 ) ) ;
#169958 = CARTESIAN_POINT ( 'NONE',  ( 0.1525891599635448848, 0.3075033511844190159, 1.785008687375288172 ) ) ;
#169959 = CARTESIAN_POINT ( 'NONE',  ( -8.681298431451969222, 9.022603012982438386, 1.040834085586084257E-14 ) ) ;
#169960 = VECTOR ( 'NONE', #47211, 1000.000000000000000 ) ;
#169961 = CARTESIAN_POINT ( 'NONE',  ( 4.924636110261782385, 6.768494766770632332, 1.599625672291267398 ) ) ;
#169962 = TOROIDAL_SURFACE ( 'NONE', #197639, 0.05000000000000000278, 0.05000000000000000278 ) ;
#169963 = CARTESIAN_POINT ( 'NONE',  ( 0.3891817118475826009, -6.836286050428183714, 10.85699613887008042 ) ) ;
#169964 = PLANE ( 'NONE',  #158453 ) ;
#169965 = CARTESIAN_POINT ( 'NONE',  ( 10.05978679165993483, 11.79913468076720306, 1.082531754730548412 ) ) ;
#169966 = EDGE_LOOP ( 'NONE', ( #14362, #186080, #112, #134029 ) ) ;
#169967 = CARTESIAN_POINT ( 'NONE',  ( 5.730092268227672037, 2.014234620932173758, 0.09611943034040781875 ) ) ;
#169968 = CARTESIAN_POINT ( 'NONE',  ( 0.4344390223590781641, -1.137927343861804053, -1.789123301873453364 ) ) ;
#169969 = CARTESIAN_POINT ( 'NONE',  ( -2.998506705650354487, 6.400614325406102978, -0.7302056868632772479 ) ) ;
#169970 = CARTESIAN_POINT ( 'NONE',  ( 2.273450361290503263, 5.679387915302107182, 0.4672911629945233347 ) ) ;
#169971 =( BOUNDED_CURVE ( )  B_SPLINE_CURVE ( 3, ( #169333, #35047, #104344, #133673 ),
 .UNSPECIFIED., .F., .T. ) 
 B_SPLINE_CURVE_WITH_KNOTS ( ( 4, 4 ),
 ( 1.570796326795096620, 3.141592653589643014 ),
 .UNSPECIFIED. ) 
 CURVE ( )  GEOMETRIC_REPRESENTATION_ITEM ( )  RATIONAL_B_SPLINE_CURVE ( ( 1.000000000000000000, 0.8047378541244475381, 0.8047378541244475381, 1.000000000000000000 ) ) 
 REPRESENTATION_ITEM ( '' )  );
#169972 = CARTESIAN_POINT ( 'NONE',  ( -5.938108093105513241, 6.030140318152288792, 0.7216878364870317197 ) ) ;
#169973 = CARTESIAN_POINT ( 'NONE',  ( 4.220665892555866883, 3.818531717603609987, -0.7998128361456211532 ) ) ;
#169974 = CARTESIAN_POINT ( 'NONE',  ( 3.678522182247864869, 1.252989934047860965, -1.519404455180313640 ) ) ;
#169975 = CARTESIAN_POINT ( 'NONE',  ( 4.569935513796226978, -0.9480243344661150040, 1.779636403143824985 ) ) ;
#169976 = CARTESIAN_POINT ( 'NONE',  ( -5.208303565944065738, 9.228104593576741621, -0.7998128361456231517 ) ) ;
#169977 = CARTESIAN_POINT ( 'NONE',  ( -9.481348452320373710, -9.006862915010128035, 0.5950054837411764552 ) ) ;
#169978 = CARTESIAN_POINT ( 'NONE',  ( 4.541096662771787251, -1.693051203114638525, -1.391418086139440957 ) ) ;
#169979 = DIRECTION ( 'NONE',  ( 0.000000000000000000, 1.000000000000000000, 0.000000000000000000 ) ) ;
#169980 = CARTESIAN_POINT ( 'NONE',  ( 2.766527970621732724, -1.329674337952547303, 1.394112488825666851 ) ) ;
#169981 = CARTESIAN_POINT ( 'NONE',  ( -7.694415870955439551, 8.935572256658169010, 1.199719254218462483 ) ) ;
#169982 = CARTESIAN_POINT ( 'NONE',  ( -0.02948999725182251466, 1.364966664109868555, -2.179895196203474050 ) ) ;
#169983 = CARTESIAN_POINT ( 'NONE',  ( 0.1331565106231363538, 7.629137130509071163, -2.545925718843544239 ) ) ;
#169984 = CARTESIAN_POINT ( 'NONE',  ( 5.605114358992040913, 6.317488171369740613, -1.123711807521186490 ) ) ;
#169985 = ORIENTED_EDGE ( 'NONE', *, *, #84896, .T. ) ;
#169986 = CARTESIAN_POINT ( 'NONE',  ( 5.573810548993915148, 5.675402860013913475, 0.000000000000000000 ) ) ;
#169987 = VERTEX_POINT ( 'NONE', #38618 ) ;
#169988 = CARTESIAN_POINT ( 'NONE',  ( 5.295741323871941297, -1.389945570378407380, -1.395530913269894091 ) ) ;
#169990 = CARTESIAN_POINT ( 'NONE',  ( 3.738934858379244552, 1.912307379442554689, 0.6292302551485791096 ) ) ;
#169989 = CARTESIAN_POINT ( 'NONE',  ( 0.08144728253534591622, -0.9147537949990096617, 1.713110483266879980 ) ) ;
#169991 = CARTESIAN_POINT ( 'NONE',  ( 5.835437120055854798, -1.464435618476932488, 1.771446943145409847 ) ) ;
#169992 = CARTESIAN_POINT ( 'NONE',  ( 4.030005733973434978, 1.030655172484344684, 1.549249419044882226 ) ) ;
#169993 = CARTESIAN_POINT ( 'NONE',  ( 5.826972158823246595, 10.02016096192762085, -0.7998128361456481317 ) ) ;
#169994 = CARTESIAN_POINT ( 'NONE',  ( 5.858512798400357546, 6.179092012920288646, 0.8810539604525641222 ) ) ;
#169995 = CARTESIAN_POINT ( 'NONE',  ( -6.368579470117215813, 8.453095353268645695, 1.599625672291283607 ) ) ;
#169996 = EDGE_CURVE ( 'NONE', #174410, #208229, #62396, .T. ) ;
#169997 = CARTESIAN_POINT ( 'NONE',  ( -3.499413046103020175, 7.096749297179887783, 0.7216878364870338292 ) ) ;
#169998 = CARTESIAN_POINT ( 'NONE',  ( 0.2049558871960316941, 1.909868400323280424, 1.074723926240577221 ) ) ;
#169999 = CARTESIAN_POINT ( 'NONE',  ( 5.124618876285529367, 7.962177208099690873, -1.082531754730549078 ) ) ;
#170000 = ORIENTED_EDGE ( 'NONE', *, *, #118916, .T. ) ;
#170001 = DIRECTION ( 'NONE',  ( -0.4999999999999997224, 0.000000000000000000, -0.8660254037844387076 ) ) ;
#170002 = CARTESIAN_POINT ( 'NONE',  ( -0.4350533241460393108, -6.938200158402035633, -9.251576347356897045 ) ) ;
#170003 = CARTESIAN_POINT ( 'NONE',  ( 0.01192831195480706721, -0.7772932952810689411, -1.650495136788888040 ) ) ;
#170004 = CARTESIAN_POINT ( 'NONE',  ( -4.412288926243578935, 7.235088616337731260, 1.199719254218464037 ) ) ;
#170005 = CARTESIAN_POINT ( 'NONE',  ( 2.689770611714628945, 1.466270380367465043, 0.9255270069659697896 ) ) ;
#170006 = FILL_AREA_STYLE_COLOUR ( '', #47275 ) ;
#170007 = CARTESIAN_POINT ( 'NONE',  ( 6.508999999999981689, 4.698440520552249922, 2.462686878797680556 ) ) ;
#170008 = CARTESIAN_POINT ( 'NONE',  ( -5.636439174979254396, 7.598931675607687453, -1.599625672291256295 ) ) ;
#170009 = DIRECTION ( 'NONE',  ( -0.000000000000000000, -1.000000000000000000, 0.000000000000000000 ) ) ;
#170010 = CARTESIAN_POINT ( 'NONE',  ( 0.5673436759025469733, 1.799520464221905369, 1.023488823764052480 ) ) ;
#170011 = CARTESIAN_POINT ( 'NONE',  ( 5.443921307256319508, 0.7362202147598860824, -1.670853202368662860 ) ) ;
#170012 = CARTESIAN_POINT ( 'NONE',  ( 3.362109073961421224, -1.959717995770013932, 0.09162775335717905645 ) ) ;
#170013 = CARTESIAN_POINT ( 'NONE',  ( -0.6125000000000401235, -0.3958333326505372729, 1.060881119635892933 ) ) ;
#170014 = CARTESIAN_POINT ( 'NONE',  ( -8.317037166979361018, 11.79062823052953668, 1.199719254218453823 ) ) ;
#170015 = CARTESIAN_POINT ( 'NONE',  ( 7.233438648090761980, 8.397765496649418182, 1.199719254218462483 ) ) ;
#170016 = CARTESIAN_POINT ( 'NONE',  ( 3.317144061745095129, 1.670432841370917298, -1.306055464808851818 ) ) ;
#170017 = CARTESIAN_POINT ( 'NONE',  ( 6.827182134110192813, 7.051736335826703339, 2.787205296604370108 ) ) ;
#170018 = CARTESIAN_POINT ( 'NONE',  ( -8.299562589859897699, 12.83457345481192036, -0.7998128361456281477 ) ) ;
#170019 = AXIS2_PLACEMENT_3D ( 'NONE', #124136, #56908, #186895 ) ;
#170020 = CARTESIAN_POINT ( 'NONE',  ( 1.340777958403309267, -2.018934908790828597, -0.4573474576154838989 ) ) ;
#170022 = CARTESIAN_POINT ( 'NONE',  ( 0.7500000000000006661, 14.86458333401613530, 1.299038105676657340 ) ) ;
#170021 = CYLINDRICAL_SURFACE ( 'NONE', #120457, 0.09999999999999961697 ) ;
#170024 = ORIENTED_EDGE ( 'NONE', *, *, #7830, .T. ) ;
#170023 = CARTESIAN_POINT ( 'NONE',  ( 5.039773670486915158, -2.109617592216144644, 0.6956167390435584741 ) ) ;
#170025 = CARTESIAN_POINT ( 'NONE',  ( 2.110373620506571957, 0.004507209458638748376, 2.298851035670963050 ) ) ;
#170026 = CARTESIAN_POINT ( 'NONE',  ( 8.758204044747998296, 11.24099069033793974, 1.443375672974076540 ) ) ;
#170028 = CARTESIAN_POINT ( 'NONE',  ( 3.285556943750000070, -3.434374999522042060, 0.000000000000000000 ) ) ;
#170027 = CARTESIAN_POINT ( 'NONE',  ( 5.695833931516881776, 9.659240330162777610, -0.7216878364870458196 ) ) ;
#170029 = FACE_OUTER_BOUND ( 'NONE', #89774, .T. ) ;
#170030 = FACE_OUTER_BOUND ( 'NONE', #121058, .T. ) ;
#170031 = CARTESIAN_POINT ( 'NONE',  ( -0.2959466228873294247, -9.091099919222520143, 9.630212118911225971 ) ) ;
#170032 = EDGE_CURVE ( 'NONE', #16921, #159827, #169675, .T. ) ;
#170033 = CARTESIAN_POINT ( 'NONE',  ( 2.672007700615218528, 1.902801012812182169, -0.1915479950082218386 ) ) ;
#170034 = CARTESIAN_POINT ( 'NONE',  ( -0.1609840471590594513, 6.431820245570142980, -3.209093660759736899 ) ) ;
#170035 = CARTESIAN_POINT ( 'NONE',  ( 4.629763539376270387, -1.062658783613348534, -1.358442396976522248 ) ) ;
#170036 = CARTESIAN_POINT ( 'NONE',  ( 2.641814858895009444, 2.006371511526034546, -0.2024640970367599380 ) ) ;
#170037 = CARTESIAN_POINT ( 'NONE',  ( 4.131641605347593504, 0.6128431504758731219, 2.215418681923121191 ) ) ;
#170038 = CARTESIAN_POINT ( 'NONE',  ( 3.497619258099498030, 1.781045823846095111, 1.394991416339389501 ) ) ;
#170039 = CARTESIAN_POINT ( 'NONE',  ( 6.147117739887063337, -1.780134362386740721, 1.125150951816885403 ) ) ;
#170040 = CARTESIAN_POINT ( 'NONE',  ( -4.502716413514296079, 8.267269892493059658, -0.7216878364870338292 ) ) ;
#170041 = CARTESIAN_POINT ( 'NONE',  ( 4.710057611840397840, -0.7560107150014344635, -1.600242281814190148 ) ) ;
#170043 = CARTESIAN_POINT ( 'NONE',  ( 0.2699993869635419208, 1.325028633338236839, 1.870336120953507875 ) ) ;
#170042 = CARTESIAN_POINT ( 'NONE',  ( 5.528692779322568640, 9.672168352510192690, 0.7998128361456341429 ) ) ;
#170044 = CARTESIAN_POINT ( 'NONE',  ( 5.085823778388903982, -1.827637283562512538, -0.2220107604927607503 ) ) ;
#170045 = CARTESIAN_POINT ( 'NONE',  ( -4.946027110887008860, 4.664786472323266153, -0.7998128361456221525 ) ) ;
#170046 = AXIS2_PLACEMENT_3D ( 'NONE', #63574, #162155, #193571 ) ;
#170047 = CARTESIAN_POINT ( 'NONE',  ( 5.894512528888635750, 1.793468170635740710, -1.259063434910556500 ) ) ;
#170048 = CARTESIAN_POINT ( 'NONE',  ( -4.956387674247580755, 7.940146832334256111, 1.199719254218452935 ) ) ;
#170049 = CARTESIAN_POINT ( 'NONE',  ( 1.360316468749973140, -0.2031249996586187434, -5.030698080332740574E-14 ) ) ;
#170050 = CARTESIAN_POINT ( 'NONE',  ( -9.367496996949647325, 15.51845925588232689, 7.500000000809292189 ) ) ;
#170051 = CARTESIAN_POINT ( 'NONE',  ( 5.635237798060349412, -0.04710594754482424346, -2.069988403558701062 ) ) ;
#170052 = CARTESIAN_POINT ( 'NONE',  ( 0.9718890779336667451, -0.9023411006064323558, 1.803417998987096427 ) ) ;
#170053 =( BOUNDED_CURVE ( )  B_SPLINE_CURVE ( 2, ( #208829, #75656, #91931, #89801, #107151, #123438, #205638 ),
 .UNSPECIFIED., .F., .T. ) 
 B_SPLINE_CURVE_WITH_KNOTS ( ( 3, 2, 2, 3 ),
 ( 0.08928571428571412116, 0.09523809523809514954, 0.1011904761904762057, 0.1071428571428572341 ),
 .UNSPECIFIED. ) 
 CURVE ( )  GEOMETRIC_REPRESENTATION_ITEM ( )  RATIONAL_B_SPLINE_CURVE ( ( 1.000000000000003775, 0.8660254037844349329, 1.000000000000000000, 0.8660254037844387076, 1.000000000000000000, 0.8660254037844364872, 1.000000000000002220 ) ) 
 REPRESENTATION_ITEM ( '' )  );
#170054 = CARTESIAN_POINT ( 'NONE',  ( 1.364683531249992088, 5.384375000341417916, 1.214306433183764966E-14 ) ) ;
#170055 = CARTESIAN_POINT ( 'NONE',  ( 4.793539397740587127, 1.428753304119126266, 1.292492988728560999 ) ) ;
#170056 = CARTESIAN_POINT ( 'NONE',  ( 1.364683531249997417, 11.23437500034139802, 2.602085213965210642E-15 ) ) ;
#170057 = CARTESIAN_POINT ( 'NONE',  ( 1.670502159040608170, 2.215024970770036017, -0.1695594764349258321 ) ) ;
#170059 = ORIENTED_EDGE ( 'NONE', *, *, #151561, .F. ) ;
#170058 = CARTESIAN_POINT ( 'NONE',  ( 4.858757509019057785, 5.629766575900002401, 7.500000000000000000 ) ) ;
#170061 = CARTESIAN_POINT ( 'NONE',  ( 0.3171178118501411514, 7.220087385434813321, -2.081545611384603145 ) ) ;
#170060 =( LENGTH_UNIT ( ) NAMED_UNIT ( * ) SI_UNIT ( .MILLI., .METRE. ) );
#170062 = CARTESIAN_POINT ( 'NONE',  ( 3.704402285031850539, 5.344888637335695414, -1.599625672291262513 ) ) ;
#170063 = CARTESIAN_POINT ( 'NONE',  ( -1.737499999999997824, -2.391666666666667052, 3.009438278150925683 ) ) ;
#170064 = CARTESIAN_POINT ( 'NONE',  ( 4.702146809683701356, 5.356480858934594025, -2.420000000000000373 ) ) ;
#170065 = CARTESIAN_POINT ( 'NONE',  ( 4.335344899790516848, 0.7389749068974335033, -1.575905762629246309 ) ) ;
#170067 = CARTESIAN_POINT ( 'NONE',  ( 2.435929278166943490, 1.204617592564939166, 1.548422000036096202 ) ) ;
#170066 = AXIS2_PLACEMENT_3D ( 'NONE', #136699, #25059, #56508 ) ;
#170069 = CARTESIAN_POINT ( 'NONE',  ( -1.364683531250012516, 2.342708333674752286, 0.7879004041258379498 ) ) ;
#170068 = CARTESIAN_POINT ( 'NONE',  ( 6.661133543015731462, 6.665743976473484267, -0.7998128361456281477 ) ) ;
#170070 = EDGE_CURVE ( 'NONE', #157226, #134989, #121020, .T. ) ;
#170071 = CARTESIAN_POINT ( 'NONE',  ( -4.446147712686649989, 7.104319146577407373, 1.107073289137233241 ) ) ;
#170072 = FACE_OUTER_BOUND ( 'NONE', #74228, .T. ) ;
#170073 = CARTESIAN_POINT ( 'NONE',  ( 0.1392228125525768467, -0.1412503886474673342, -2.030206775815279308 ) ) ;
#170074 = CARTESIAN_POINT ( 'NONE',  ( -7.472515219426274946, 11.86968485597268064, 0.000000000000000000 ) ) ;
#170075 = CARTESIAN_POINT ( 'NONE',  ( -3.701012746406287413, 6.301303389907177532, 1.082531754730560403 ) ) ;
#170076 = CARTESIAN_POINT ( 'NONE',  ( 1.569569324160888124, 0.1651462269399027738, -2.256556122256009100 ) ) ;
#170078 = ORIENTED_EDGE ( 'NONE', *, *, #26823, .T. ) ;
#170077 = CARTESIAN_POINT ( 'NONE',  ( -4.394814349124112951, 8.279033840620114049, -0.7998128361456281477 ) ) ;
#170079 = CARTESIAN_POINT ( 'NONE',  ( -0.7500000000000006661, -0.8604166659838472508, -1.299038105676652011 ) ) ;
#170080 = CARTESIAN_POINT ( 'NONE',  ( 1.598681293450100904, 1.532267803987485077, -1.072633048482305229 ) ) ;
#170081 = CARTESIAN_POINT ( 'NONE',  ( 0.4747597223977735315, -1.720734514737034093, -0.2143409017008046646 ) ) ;
#170083 = CARTESIAN_POINT ( 'NONE',  ( 3.966501855323391723, -2.045284974426237579, -0.7877190255709336508 ) ) ;
#170082 = CARTESIAN_POINT ( 'NONE',  ( 1.360316468749963592, 1.244791667008120051, 0.7853790794158760358 ) ) ;
#170084 = CARTESIAN_POINT ( 'NONE',  ( 5.930798096255836427, 2.221851032742766741, 0.6229754028606748761 ) ) ;
#170085 = CARTESIAN_POINT ( 'NONE',  ( 0.3739917644934092067, 1.186169308094830344, 1.685110605438163045 ) ) ;
#170086 = CARTESIAN_POINT ( 'NONE',  ( 3.960829289611409898, 0.2367351755836170912, -1.927401316828970979 ) ) ;
#170087 = CARTESIAN_POINT ( 'NONE',  ( -4.324687812634898876, 6.068555086205916105, 1.443375672974064550 ) ) ;
#170088 = CARTESIAN_POINT ( 'NONE',  ( 6.385527162356455122, 10.39360608948380538, 1.056142170575426150E-14 ) ) ;
#170089 = CARTESIAN_POINT ( 'NONE',  ( 4.584065335196271462, 5.481069324884694005, 1.082531754730549078 ) ) ;
#170090 = CARTESIAN_POINT ( 'NONE',  ( -4.757329562667670667E-14, 0.5781250003414448724, -1.570758158831812246 ) ) ;
#170091 = CARTESIAN_POINT ( 'NONE',  ( 3.076796235938107138, -0.8146265060355701859, 1.844709937164576097 ) ) ;
#170092 = CARTESIAN_POINT ( 'NONE',  ( -3.863710589770277259, 6.491117540498504646, 1.082531754730560403 ) ) ;
#170093 = CARTESIAN_POINT ( 'NONE',  ( -5.444481204339554736, 8.509589284108232121, 1.199719254218454489 ) ) ;
#170094 = CARTESIAN_POINT ( 'NONE',  ( 7.639129486296027061, 10.99973593639901814, 1.199719254218460707 ) ) ;
#170096 = CARTESIAN_POINT ( 'NONE',  ( 7.752014238602739730E-16, 3.000000000000000888, 6.329999999999995630 ) ) ;
#170095 = CARTESIAN_POINT ( 'NONE',  ( 0.7854531640391904102, 1.224056292049885419, 1.354719642434290439 ) ) ;
#170097 = CARTESIAN_POINT ( 'NONE',  ( -5.581116510680924847, 6.540332679663050541, -1.199719254218453823 ) ) ;
#170098 = CARTESIAN_POINT ( 'NONE',  ( -3.955946960137363799, 7.837298230127379917, 0.7998128361456350310 ) ) ;
#170099 = CARTESIAN_POINT ( 'NONE',  ( -11.66902918085182250, 4.335764935525111774, 5.185761432613135824 ) ) ;
#170100 = VERTEX_POINT ( 'NONE', #184838 ) ;
#170101 = CARTESIAN_POINT ( 'NONE',  ( 0.4444780689869810564, 2.156031605563761833, 0.1575401717312311101 ) ) ;
#170102 = CARTESIAN_POINT ( 'NONE',  ( -7.065207446052822249, 7.415365906582643163, -0.7216878364870338292 ) ) ;
#170103 = CARTESIAN_POINT ( 'NONE',  ( -3.195971524519394702, 4.751719416737803847, -1.599625672291262513 ) ) ;
#170104 = CARTESIAN_POINT ( 'NONE',  ( -4.173017639316489280, 7.592962374094866185, 0.9320401348096055694 ) ) ;
#170105 = CARTESIAN_POINT ( 'NONE',  ( 6.199869188016119637, 1.394352454258035001, 1.461346697781773507 ) ) ;
#170107 = ORIENTED_EDGE ( 'NONE', *, *, #137597, .F. ) ;
#170106 = CARTESIAN_POINT ( 'NONE',  ( 6.006509256357773552, -2.210310773855695743, -0.2204792344780072411 ) ) ;
#170108 = CARTESIAN_POINT ( 'NONE',  ( -8.072954122294394352, 8.383144328957069291, -0.7998128361456362523 ) ) ;
#170109 = CARTESIAN_POINT ( 'NONE',  ( 6.681470773436232413, 6.689470745297396270, -0.7998128361456281477 ) ) ;
#170110 = CARTESIAN_POINT ( 'NONE',  ( 5.577047029790810129, -0.04816181868504652158, -2.060495320025256483 ) ) ;
#170111 = CARTESIAN_POINT ( 'NONE',  ( 3.797500137148449362, 1.423962148579031917, -1.427936706820939872 ) ) ;
#170112 = ORIENTED_EDGE ( 'NONE', *, *, #161732, .T. ) ;
#170113 = FILL_AREA_STYLE ('',( #153884 ) ) ;
#170114 = CARTESIAN_POINT ( 'NONE',  ( 2.381428537494710618, 5.930083727052461562, 0.7998128361456462443 ) ) ;
#170115 = CIRCLE ( 'NONE', #97627, 0.04999999999999934358 ) ;
#170117 = ORIENTED_EDGE ( 'NONE', *, *, #91003, .T. ) ;
#170116 = CARTESIAN_POINT ( 'NONE',  ( -5.596483547390937119, 9.751257581923240991, 0.000000000000000000 ) ) ;
#170118 = CARTESIAN_POINT ( 'NONE',  ( 4.797842130449009090, 8.250315290282747682, 0.8618622828703215166 ) ) ;
#170119 = CARTESIAN_POINT ( 'NONE',  ( 4.200545946899570282, -1.388273439763810790, -1.462221600879671790 ) ) ;
#170120 = CARTESIAN_POINT ( 'NONE',  ( 3.240019139272034110, 0.4481936114588759845, 1.785621944311803100 ) ) ;
#170121 = CIRCLE ( 'NONE', #156380, 1.249999999999998890 ) ;
#170122 = DIRECTION ( 'NONE',  ( 0.000000000000000000, 8.546850786086437571E-32, 1.000000000000000000 ) ) ;
#170123 = CARTESIAN_POINT ( 'NONE',  ( 2.491230068042503465, -0.3961224009183231809, -2.273300736686647117 ) ) ;
#170124 = CARTESIAN_POINT ( 'NONE',  ( 3.250922972226694352, 7.014770244231638863, 0.7998128361456281477 ) ) ;
#170125 = EDGE_CURVE ( 'NONE', #96623, #58812, #183788, .T. ) ;
#170126 = CARTESIAN_POINT ( 'NONE',  ( 4.745497693432328745, -1.667575968047749546, -1.375352955852253922 ) ) ;
#170127 = CARTESIAN_POINT ( 'NONE',  ( 9.094822116668764167, 9.505047312402055582, 0.7998128361456462443 ) ) ;
#170129 = CARTESIAN_POINT ( 'NONE',  ( 2.800017839408690090, -0.9981255096969069429, -1.752139039461996006 ) ) ;
#170128 = CARTESIAN_POINT ( 'NONE',  ( 6.550350952284553330, -1.418464805562440922, 1.173678288350611609 ) ) ;
#170130 = CARTESIAN_POINT ( 'NONE',  ( -5.087333953625788219, 6.958308917361963886, 1.599625672291267398 ) ) ;
#170131 = CARTESIAN_POINT ( 'NONE',  ( 4.077728334586081083, 1.628699396557086398, -1.621930329367648138 ) ) ;
#170132 = CARTESIAN_POINT ( 'NONE',  ( -9.438074503189328723, 14.51398094803501060, -7.411038319754888803 ) ) ;
#170133 = CARTESIAN_POINT ( 'NONE',  ( 1.071256458935645988E-16, 3.599999999999999201, 1.600000000000005196 ) ) ;
#170134 = CARTESIAN_POINT ( 'NONE',  ( 2.764352523130030548, -1.291370965961564421, 1.353630663414123969 ) ) ;
#170135 = CARTESIAN_POINT ( 'NONE',  ( 0.6320224300673723539, 1.017306711037075262, -1.688479424803266404 ) ) ;
#170137 = CARTESIAN_POINT ( 'NONE',  ( -7.075376061485238566, 9.347967719856493218, 1.599625672291269396 ) ) ;
#170136 = CARTESIAN_POINT ( 'NONE',  ( -1.364683531249997417, 5.259375000341425022, 1.214306433183764966E-14 ) ) ;
#170138 = CARTESIAN_POINT ( 'NONE',  ( 1.735297346119796691, 0.2185962045802778420, 2.196029071591873993 ) ) ;
#170139 = VERTEX_POINT ( 'NONE', #167544 ) ;
#170140 = CARTESIAN_POINT ( 'NONE',  ( 1.316495309083404618E-15, 0.5000000000000000000, -10.75000000000000000 ) ) ;
#170141 = CARTESIAN_POINT ( 'NONE',  ( 4.273844736805816780, 6.009238164405336313, 1.599625672291267398 ) ) ;
#170142 = CARTESIAN_POINT ( 'NONE',  ( -3.761497552787613330, 6.475832013972435242, 1.199719254218464037 ) ) ;
#170143 = CARTESIAN_POINT ( 'NONE',  ( -7.747753938335002921, -5.575271019047995047, 7.808923410443626700 ) ) ;
#170144 = CARTESIAN_POINT ( 'NONE',  ( 6.561403051094389483, 0.3373947195176879021, -1.942235834477159084 ) ) ;
#170145 = CARTESIAN_POINT ( 'NONE',  ( 6.217413992247779575, -0.2892589651934658890, 2.289433544902704565 ) ) ;
#170147 = EDGE_CURVE ( 'NONE', #203624, #85209, #125015, .T. ) ;
#170146 = CARTESIAN_POINT ( 'NONE',  ( 0.2562055958934654210, -1.961350414083770977, -0.05204156388862594962 ) ) ;
#170148 = CARTESIAN_POINT ( 'NONE',  ( 3.678632908625163012, 1.312080992568062321, -1.591389186695492342 ) ) ;
#170149 = CARTESIAN_POINT ( 'NONE',  ( 4.853455804012203778, 8.606189504748821051, 0.7216878364870438212 ) ) ;
#170150 = CARTESIAN_POINT ( 'NONE',  ( 6.505933609711257226, 8.683618192786854095, -1.599625672291281386 ) ) ;
#170151 = CARTESIAN_POINT ( 'NONE',  ( 8.568389893712330618, 9.098802418860289620, 1.040834085586084257E-14 ) ) ;
#170152 = CARTESIAN_POINT ( 'NONE',  ( -0.6823417656250212460, 3.613541667008085767, 1.181850606188767472 ) ) ;
#170153 = DIRECTION ( 'NONE',  ( 0.000000000000000000, 1.000000000000000000, 0.000000000000000000 ) ) ;
#170154 = CARTESIAN_POINT ( 'NONE',  ( 5.463572716182829581, 6.436884926043849653, 1.082531754730560403 ) ) ;
#170155 = CARTESIAN_POINT ( 'NONE',  ( 6.549308719555964053, 1.892307808498715049, -1.064380946037797093 ) ) ;
#170156 = CARTESIAN_POINT ( 'NONE',  ( 5.231922985772964552, 1.814955821992572993, 0.3091130605668013231 ) ) ;
#170157 = DIRECTION ( 'NONE',  ( -0.8003905296791066215, 0.000000000000000000, 0.5994789404140892231 ) ) ;
#170158 = CARTESIAN_POINT ( 'NONE',  ( 6.058177568126345669, -1.550975213528119623, 1.548612826651605712 ) ) ;
#170159 = CARTESIAN_POINT ( 'NONE',  ( 0.2275331484566482099, -1.145445245298154946, -1.479381579510357758 ) ) ;
#170160 = CARTESIAN_POINT ( 'NONE',  ( -4.300870446666812619, 7.448604017583265957, 1.116033750828262949 ) ) ;
#170161 = CARTESIAN_POINT ( 'NONE',  ( 0.3029082221123034491, 2.721802924646587130, 2.050239952424178558 ) ) ;
#170162 = CARTESIAN_POINT ( 'NONE',  ( 6.225987253121650689, 7.022442755726078900, -1.008712875586889712 ) ) ;
#170163 = AXIS2_PLACEMENT_3D ( 'NONE', #127695, #130860, #47436 ) ;
#170164 = CARTESIAN_POINT ( 'NONE',  ( 11.33772463945036790, 13.50911576511426304, -3.600000000000000089 ) ) ;
#170165 = CARTESIAN_POINT ( 'NONE',  ( 2.289615904538056412, -0.7594197407109636311, 1.598781567136787318 ) ) ;
#170166 = CARTESIAN_POINT ( 'NONE',  ( 6.569000952640477564, -1.554625895936670554, 1.278542242695315689 ) ) ;
#170168 = CARTESIAN_POINT ( 'NONE',  ( 4.165583994951371771, 1.254247372560507223, 1.447964403467276506 ) ) ;
#170167 = CARTESIAN_POINT ( 'NONE',  ( -8.469039510030723861, 13.03229652834454733, 1.040834085586084257E-14 ) ) ;
#170169 = DIRECTION ( 'NONE',  ( 1.000000000000000000, -0.000000000000000000, -0.000000000000000000 ) ) ;
#170170 = CARTESIAN_POINT ( 'NONE',  ( 5.652785005015395825, -0.4769087673412530370, -1.910818445241519559 ) ) ;
#170171 = CARTESIAN_POINT ( 'NONE',  ( 0.2816890862925770511, 0.2015970107726860194, -2.110973810222869229 ) ) ;
#170172 = CARTESIAN_POINT ( 'NONE',  ( -0.4019237886466871523, 10.94866454968463110, -1.499999999999998668 ) ) ;
#170173 = CARTESIAN_POINT ( 'NONE',  ( 2.430351462470367707, 1.813921419787648315, 0.4566771774890953095 ) ) ;
#170175 = ORIENTED_EDGE ( 'NONE', *, *, #167966, .T. ) ;
#170174 = CARTESIAN_POINT ( 'NONE',  ( 6.182236774357948050, -0.9162642880373177423, 1.461205601097197659 ) ) ;
#170177 = CARTESIAN_POINT ( 'NONE',  ( 2.385871846325007706, 5.727341554113725586, -0.7216878364870267237 ) ) ;
#170176 = CARTESIAN_POINT ( 'NONE',  ( 3.246891520140795517, 0.5363302883765566076, 2.140594385818309409 ) ) ;
#170178 = CARTESIAN_POINT ( 'NONE',  ( 1.364683531249986537, 2.717708333674754062, -0.7879004041258239610 ) ) ;
#170179 = CARTESIAN_POINT ( 'NONE',  ( 0.3970293196923400658, 0.3510089794473401081, 2.032437512258952417 ) ) ;
#170180 = CARTESIAN_POINT ( 'NONE',  ( 8.111855979677986994, 8.358253485912799263, 1.040834085586084257E-14 ) ) ;
#170181 = CARTESIAN_POINT ( 'NONE',  ( -10.00321840878439339, 10.56484298653695397, 1.040834085586084257E-14 ) ) ;
#170182 = CARTESIAN_POINT ( 'NONE',  ( -6.723431022862452089, 15.44785976354745749, -9.895899930522206844 ) ) ;
#170183 = CARTESIAN_POINT ( 'NONE',  ( -3.405069135326500351, 7.124331091189553433, 1.040834085586084257E-14 ) ) ;
#170184 = AXIS2_PLACEMENT_3D ( 'NONE', #107337, #174429, #160285 ) ;
#170185 = CARTESIAN_POINT ( 'NONE',  ( -5.534896847468681713, 7.440644035717915550, -1.251640694545209209 ) ) ;
#170186 = EDGE_LOOP ( 'NONE', ( #172375, #79155, #192232, #198637 ) ) ;
#170187 = CARTESIAN_POINT ( 'NONE',  ( 2.664580169416390643, -0.7900844611210651180, -1.913877855911281234 ) ) ;
#170188 = CARTESIAN_POINT ( 'NONE',  ( -0.7499999999999972244, 4.608333333333352932, -1.299038105676652011 ) ) ;
#170189 = CARTESIAN_POINT ( 'NONE',  ( 5.823390672269506574, 6.752709524857930745, -1.199719254218446718 ) ) ;
#170190 = CARTESIAN_POINT ( 'NONE',  ( -6.019435214058361794, 7.168094078216475040, 1.196694171119830008 ) ) ;
#170192 = ADVANCED_FACE ( 'NONE', ( #37543 ), #153437, .F. ) ;
#170191 = CARTESIAN_POINT ( 'NONE',  ( 0.6100282365348074221, -0.7248652973187595938, 1.885305865817282323 ) ) ;
#170193 = CARTESIAN_POINT ( 'NONE',  ( 4.161989969715272686, 4.726297878971393196, 2.420000000000010587 ) ) ;
#170194 = CARTESIAN_POINT ( 'NONE',  ( -0.6823417656250212460, 4.051041667008085767, 1.181850606188767472 ) ) ;
#170195 = EDGE_LOOP ( 'NONE', ( #27972, #90581, #208703, #200502 ) ) ;
#170196 = EDGE_CURVE ( 'NONE', #131458, #113572, #114029, .T. ) ;
#170198 = CARTESIAN_POINT ( 'NONE',  ( 10.24960094225127172, 11.06021530882240356, -0.7216878364870257245 ) ) ;
#170197 = CARTESIAN_POINT ( 'NONE',  ( 0.07479286986305369589, 1.387406912293275729, -2.112587013352088317 ) ) ;
#170199 = CARTESIAN_POINT ( 'NONE',  ( 6.362657644764970755, -0.6818896071447738683, 1.897407954007489073 ) ) ;
#170200 = CARTESIAN_POINT ( 'NONE',  ( 6.069544675611900253, 1.326465198304109583, 1.382431045765440514 ) ) ;
#170201 = CARTESIAN_POINT ( 'NONE',  ( 6.639320575229286092, 2.965970653406803770, 2.456291990408800086 ) ) ;
#170202 = CARTESIAN_POINT ( 'NONE',  ( 4.142245973918059043, 0.5854081421233224836, 2.111838497463234710 ) ) ;
#170203 = CARTESIAN_POINT ( 'NONE',  ( 1.499999999999989120, 1.556250000682817047, 0.000000000000000000 ) ) ;
#170204 = CARTESIAN_POINT ( 'NONE',  ( 2.091926199050548441, 1.179367891222588005, 1.505316542580182437 ) ) ;
#170205 = CARTESIAN_POINT ( 'NONE',  ( -4.904298879841297421, 6.744767997946721216, 1.599625672291267398 ) ) ;
#170206 = CARTESIAN_POINT ( 'NONE',  ( 4.894130264408854458, 6.732904613275549899, -1.443375672974051449 ) ) ;
#170208 = CARTESIAN_POINT ( 'NONE',  ( 1.036732716359071604, -1.587823911754655315, 1.242746109592095527 ) ) ;
#170207 = CARTESIAN_POINT ( 'NONE',  ( 10.15205317230714144, 3.956598013261176217, -5.494609294606112471 ) ) ;
#170209 = CARTESIAN_POINT ( 'NONE',  ( -1.402160292154681736E-14, 11.23437500034139980, 1.575800808251682339 ) ) ;
#170211 = CARTESIAN_POINT ( 'NONE',  ( -4.630991987519598396, 7.560518531151607213, 1.199719254218452935 ) ) ;
#170210 = CARTESIAN_POINT ( 'NONE',  ( 6.532779862045914321, -1.958661757936002612, 0.9833580883553474372 ) ) ;
#170213 = ORIENTED_EDGE ( 'NONE', *, *, #128877, .F. ) ;
#170212 = CARTESIAN_POINT ( 'NONE',  ( 2.555303990735880770, 0.4627875540959677236, -1.661435987504814360 ) ) ;
#170214 = FACE_OUTER_BOUND ( 'NONE', #151593, .T. ) ;
#170215 = CARTESIAN_POINT ( 'NONE',  ( 5.770966940911189447, 9.884545197705074671, -0.7998128361456291469 ) ) ;
#170216 = CARTESIAN_POINT ( 'NONE',  ( 3.635557746758808495, 7.393234471193928847, -0.7998128361456291469 ) ) ;
#170217 = TOROIDAL_SURFACE ( 'NONE', #24860, 11.18000000000000149, 0.08000000000000000167 ) ;
#170218 = SURFACE_SIDE_STYLE ('',( #70556 ) ) ;
#170219 = CARTESIAN_POINT ( 'NONE',  ( 1.662477996687723669, -0.7030478115006146833, -1.831755296705489977 ) ) ;
#170220 =( LENGTH_UNIT ( ) NAMED_UNIT ( * ) SI_UNIT ( .MILLI., .METRE. ) );
#170221 = CARTESIAN_POINT ( 'NONE',  ( 5.867981556616276073, 5.740399992340775803, -0.7998128361456281477 ) ) ;
#170222 = CARTESIAN_POINT ( 'NONE',  ( 0.3769810270647828698, 3.049942316455306113, 0.4288785890452298522 ) ) ;
#170224 = VERTEX_POINT ( 'NONE', #74324 ) ;
#170223 = B_SPLINE_CURVE_WITH_KNOTS ( 'NONE', 3,
 ( #140088, #188808, #187729, #8987 ),
 .UNSPECIFIED., .F., .F.,
 ( 4, 4 ),
 ( 0.000000000000000000, 0.0004136821696107355730 ),
 .UNSPECIFIED. ) ;
#170225 = FACE_BOUND ( 'NONE', #188195, .T. ) ;
#170226 = VERTEX_POINT ( 'NONE', #170746 ) ;
#170227 = CARTESIAN_POINT ( 'NONE',  ( 4.494648839764849413, -1.758179434694202570, -0.4356380854809716041 ) ) ;
#170228 = ORIENTED_EDGE ( 'NONE', *, *, #163457, .F. ) ;
#170229 = CARTESIAN_POINT ( 'NONE',  ( 8.028399517586572998, 12.51821653715971472, -0.7998128361456352531 ) ) ;
#170230 = CARTESIAN_POINT ( 'NONE',  ( 5.259637247458703868, 5.100941308315409373, 0.000000000000000000 ) ) ;
#170231 = CARTESIAN_POINT ( 'NONE',  ( 5.057183878474817540, -1.550805960166462105, 0.9359391756664036111 ) ) ;
#170232 = CARTESIAN_POINT ( 'NONE',  ( 0.3046331935817621073, -6.606549254264995064, 9.611339018008543178 ) ) ;
#170233 = CARTESIAN_POINT ( 'NONE',  ( 5.085343294144599291, 4.914812813773358435, 0.1758235994440172922 ) ) ;
#170234 = CARTESIAN_POINT ( 'NONE',  ( 5.504159067553832330, 6.221818635116664886, 0.9641881782859774708 ) ) ;
#170236 = CARTESIAN_POINT ( 'NONE',  ( 0.6823417656249934904, 14.44270833367473195, 1.181850606188764807 ) ) ;
#170235 = CARTESIAN_POINT ( 'NONE',  ( 5.459367789976862895, 1.521435002614815790, 1.071484558867175529 ) ) ;
#170237 = CARTESIAN_POINT ( 'NONE',  ( 2.319824818950954270, 0.9007672528749611773, -1.690582045118453225 ) ) ;
#170238 = CARTESIAN_POINT ( 'NONE',  ( -10.96041802301306944, 4.843384909922287207, -4.379099270644332798 ) ) ;
#170239 = CARTESIAN_POINT ( 'NONE',  ( -1.500000000000011324, 5.660416667349481123, -0.8660254037844312691 ) ) ;
#170240 = CARTESIAN_POINT ( 'NONE',  ( 0.6823417656249882723, -1.157291666325249713, 1.181850606188755259 ) ) ;
#170241 = CARTESIAN_POINT ( 'NONE',  ( 5.816084710582486217, 9.729256562414162701, 1.040834085586084257E-14 ) ) ;
#170242 = CARTESIAN_POINT ( 'NONE',  ( -3.144601563365788444, 5.756120026313656268, -1.199719254218452935 ) ) ;
#170243 = CARTESIAN_POINT ( 'NONE',  ( 6.662120174140254925, -7.184999792969698262, -6.772456105771881951 ) ) ;
#170244 = CARTESIAN_POINT ( 'NONE',  ( 1.095779546523030668, -2.090823718873015657, 0.001679924440483454573 ) ) ;
#170245 = CARTESIAN_POINT ( 'NONE',  ( 5.773793314573267388, 7.829454515125894964, 1.599625672291268286 ) ) ;
#170246 = CARTESIAN_POINT ( 'NONE',  ( 6.581085459773934332, -0.09550846514571986745, -1.924131155975503216 ) ) ;
#170247 = CARTESIAN_POINT ( 'NONE',  ( -4.120788623549732854, 6.895004929861607401, -1.199719254218452047 ) ) ;
#170248 = CARTESIAN_POINT ( 'NONE',  ( 2.256629077056008015, -1.412982602626071449, 1.155960151518524937 ) ) ;
#170249 = CARTESIAN_POINT ( 'NONE',  ( -5.946383829923330921, 4.757679660048923509, 2.499999999998779199 ) ) ;
#170250 =( BOUNDED_SURFACE ( )  B_SPLINE_SURFACE ( 3, 2, ( 
 ( #37932, #104006, #170050 ),
 ( #68268, #5390, #149549 ),
 ( #49918, #133334, #165801 ),
 ( #190561, #23797, #137580 ),
 ( #90964, #89902, #157029 ),
 ( #139723, #122476, #42217 ),
 ( #174353, #8616, #138644 ),
 ( #22717, #203598, #171123 ),
 ( #188437, #155954, #40071 ),
 ( #74698, #55250, #140802 ),
 ( #187370, #106182, #58447 ),
 ( #41152, #108333, #121397 ),
 ( #205746, #88831, #206813 ),
 ( #141871, #107261, #92040 ) ),
 .UNSPECIFIED., .F., .F., .T. ) 
 B_SPLINE_SURFACE_WITH_KNOTS ( ( 4, 2, 2, 2, 2, 2, 4 ),
 ( 3, 3 ),
 ( 0.01742726433212075238, 0.02010289811550490524, 0.02144071500719698167, 0.02277853189888905810, 0.02411634879058113454, 0.02545416568227321097, 0.02812979946565736036 ),
 ( 0.000000000000000000, 1.000000000000000000 ),
 .UNSPECIFIED. ) 
 GEOMETRIC_REPRESENTATION_ITEM ( )  RATIONAL_B_SPLINE_SURFACE ( (
 ( 1.000000000000000000, 0.8509629433930189224, 1.000000000000000000),
 ( 1.000000000000000000, 0.8507262248946917405, 1.000000000000000000),
 ( 1.000000000000000000, 0.8494479596845089242, 1.000000000000000000),
 ( 1.000000000000000000, 0.8495361673793808688, 1.000000000000000000),
 ( 1.000000000000000000, 0.8498393499228069636, 1.000000000000000000),
 ( 1.000000000000000000, 0.8505768930579380438, 1.000000000000000000),
 ( 1.000000000000000000, 0.8510027784581069010, 1.000000000000000000),
 ( 1.000000000000000000, 0.8509174126978680253, 1.000000000000000000),
 ( 1.000000000000000000, 0.8504342006050041869, 1.000000000000000000),
 ( 1.000000000000000000, 0.8496654783626688134, 1.000000000000000000),
 ( 1.000000000000000000, 0.8493814140782459665, 1.000000000000000000),
 ( 1.000000000000000000, 0.8494163377631810397, 1.000000000000000000),
 ( 1.000000000000000000, 0.8508375213763882394, 1.000000000000000000),
 ( 1.000000000000000000, 0.8509612879365336946, 1.000000000000000000) ) ) 
 REPRESENTATION_ITEM ( '' )  SURFACE ( )  );
#170251 = CARTESIAN_POINT ( 'NONE',  ( 1.890998328602263800, 0.1897877418215961898, 1.960365536012158127 ) ) ;
#170252 = CARTESIAN_POINT ( 'NONE',  ( 3.280740747204694774, 1.754465757641409995, -0.8330476171748876224 ) ) ;
#170253 = VERTEX_POINT ( 'NONE', #139335 ) ;
#170254 = CARTESIAN_POINT ( 'NONE',  ( -3.673896439623302257, 4.156855427197417185, -0.9999999999999991118 ) ) ;
#170255 = CARTESIAN_POINT ( 'NONE',  ( -4.655245641445871385, 6.524482229810530498, 1.599625672291263179 ) ) ;
#170257 = CARTESIAN_POINT ( 'NONE',  ( 3.762070191281779774, 0.7111978290502696254, -1.997938288694045550 ) ) ;
#170256 = CARTESIAN_POINT ( 'NONE',  ( 6.318982112420993502, 9.529840343536603697, -1.199719254218452047 ) ) ;
#170258 = CARTESIAN_POINT ( 'NONE',  ( 6.524021554744638074, -6.747656629766706438, 6.895452369244322810 ) ) ;
#170259 = CARTESIAN_POINT ( 'NONE',  ( 9.260382613333817403, 10.76253345609967660, -1.199719254218446718 ) ) ;
#170260 = CARTESIAN_POINT ( 'NONE',  ( -5.960744811863571968, 6.983232364376142698, 1.199719254218452935 ) ) ;
#170261 = CARTESIAN_POINT ( 'NONE',  ( 4.053524740805938720, 3.831459740469437936, 1.214306433183764966E-14 ) ) ;
#170262 = VERTEX_POINT ( 'NONE', #109021 ) ;
#170263 = CARTESIAN_POINT ( 'NONE',  ( 7.212011367826596242, 7.378711115411311638, 0.000000000000000000 ) ) ;
#170264 = LINE ( 'NONE', #39206, #193017 ) ;
#170265 = CARTESIAN_POINT ( 'NONE',  ( 3.738726038629454074, 0.2694068579384528150, 1.805578518607708016 ) ) ;
#170266 = FACE_OUTER_BOUND ( 'NONE', #131292, .T. ) ;
#170267 = CARTESIAN_POINT ( 'NONE',  ( -2.117044542028253318, 5.621635732341564662, -0.7998128361456281477 ) ) ;
#170268 = TOROIDAL_SURFACE ( 'NONE', #80452, 11.70000000000000107, 0.2000000000000000111 ) ;
#170269 = CARTESIAN_POINT ( 'NONE',  ( -4.586029276033976920, 8.497253585842676316, 0.07182003436798957419 ) ) ;
#170270 = CARTESIAN_POINT ( 'NONE',  ( 6.925078400183550364, 4.698656493127392864, 2.418320467900983761 ) ) ;
#170271 = CARTESIAN_POINT ( 'NONE',  ( 4.240975883383619305, -1.627667033997456381, 0.9218181776217827528 ) ) ;
#170272 = CARTESIAN_POINT ( 'NONE',  ( 8.274553823041976841, 8.548067636504127265, 1.040834085586084257E-14 ) ) ;
#170273 = CARTESIAN_POINT ( 'NONE',  ( 1.717283182695702015, -0.2364092415704423800, 1.911874917900743931 ) ) ;
#170274 = CARTESIAN_POINT ( 'NONE',  ( 6.977413161700751765, -0.1449424838519241254, 1.929857014940839832 ) ) ;
#170275 = CARTESIAN_POINT ( 'NONE',  ( -1.402160292154681736E-14, 8.984375000341396245, 1.575800808251682339 ) ) ;
#170276 = CARTESIAN_POINT ( 'NONE',  ( -5.930802130974132780, 9.006687355190106103, -1.199719254218440723 ) ) ;
#170277 = CARTESIAN_POINT ( 'NONE',  ( 2.984766373302843778, 6.633977868828633717, -0.7998128361456291469 ) ) ;
#170278 = CARTESIAN_POINT ( 'NONE',  ( -3.797692425159308716, 7.444741906078900406, 0.000000000000000000 ) ) ;
#170279 = CARTESIAN_POINT ( 'NONE',  ( 1.757563674541680721, 2.025006261547353414, -0.6180173261674735130 ) ) ;
#170280 = CARTESIAN_POINT ( 'NONE',  ( 9.378489572351044856, 11.96465713920816043, -1.599625672291262513 ) ) ;
#170281 = CARTESIAN_POINT ( 'NONE',  ( -4.284013352238274841, 4.100363120473813794, -0.7216878364870207285 ) ) ;
#170282 = CARTESIAN_POINT ( 'NONE',  ( 5.383670357325340383, -1.967593191946028996, 0.6441560278484458335 ) ) ;
#170284 = CARTESIAN_POINT ( 'NONE',  ( 1.364683531249990311, 2.946875000341416140, 1.214306433183764966E-14 ) ) ;
#170283 = CARTESIAN_POINT ( 'NONE',  ( 0.9250624443557056154, -1.167992581197497604, -1.423340509374780405 ) ) ;
#170285 = CARTESIAN_POINT ( 'NONE',  ( 4.905072937705025282, -1.228516145343660826, -1.942733121961652376 ) ) ;
#170286 = CARTESIAN_POINT ( 'NONE',  ( 6.995644074971448134, 7.263932296995902149, -0.7216878364870257245 ) ) ;
#170288 = SURFACE_STYLE_FILL_AREA ( #104242 ) ;
#170287 = CARTESIAN_POINT ( 'NONE',  ( 4.800995793014950941, 5.734154859006458160, -1.082531754730548412 ) ) ;
#170289 = CARTESIAN_POINT ( 'NONE',  ( 1.412523707164672127, 1.536465969362065476, -1.701261851757162269 ) ) ;
#170290 = CARTESIAN_POINT ( 'NONE',  ( 3.172244755473273781, 6.644776614786712443, 0.000000000000000000 ) ) ;
#170291 = CARTESIAN_POINT ( 'NONE',  ( -4.925354943514475003, 8.968274210734028529, 0.000000000000000000 ) ) ;
#170292 = CARTESIAN_POINT ( 'NONE',  ( 6.035097030359367842, -1.408219244926838476, -1.337428300092268652 ) ) ;
#170293 = ORIENTED_EDGE ( 'NONE', *, *, #59579, .T. ) ;
#170294 = CARTESIAN_POINT ( 'NONE',  ( 7.687109908824030668, 10.95175007939464606, -1.082531754730543083 ) ) ;
#170295 = ORIENTED_EDGE ( 'NONE', *, *, #213625, .F. ) ;
#170296 = CARTESIAN_POINT ( 'NONE',  ( 5.976807594091997800, -1.347613670528555740, 1.357171208065083512 ) ) ;
#170297 = CARTESIAN_POINT ( 'NONE',  ( 6.122279814772175754, 1.995267444086584518, 0.2910868170948808786 ) ) ;
#170299 = DIRECTION ( 'NONE',  ( 0.9990890794760040050, 5.454924750823445190E-15, -0.04267330865764876885 ) ) ;
#170298 = CARTESIAN_POINT ( 'NONE',  ( -7.609150525767646833, 9.900428251527500834, -1.599625672291263179 ) ) ;
#170300 = CARTESIAN_POINT ( 'NONE',  ( -1.642778471875000035, -0.9552083328553742092, -2.845375778867859751 ) ) ;
#170302 = CARTESIAN_POINT ( 'NONE',  ( 0.9535335928906017999, 1.768114364327963539, -0.08115213312524624523 ) ) ;
#170301 = CARTESIAN_POINT ( 'NONE',  ( 2.589882131170073709, -2.085102945988726031, -0.1528390284690275547 ) ) ;
#170303 = CARTESIAN_POINT ( 'NONE',  ( 4.098537063712264228, 7.253343185014818673, 1.055677455976588686 ) ) ;
#170304 = CARTESIAN_POINT ( 'NONE',  ( 3.732637569912560682, 0.3354268113090127512, 2.267480163388153169 ) ) ;
#170305 = CARTESIAN_POINT ( 'NONE',  ( 3.661793474361102252, -1.167423004587186952, 1.290856655984705670 ) ) ;
#170306 = CARTESIAN_POINT ( 'NONE',  ( 8.191097360950562845, 12.70803068775103739, -0.7998128361456352531 ) ) ;
#170307 = CIRCLE ( 'NONE', #118583, 0.08000000000000004330 ) ;
#170308 = CARTESIAN_POINT ( 'NONE',  ( 1.224999999999968781, 0.6666666673495352802, 0.7072540797572596238 ) ) ;
#170309 = CARTESIAN_POINT ( 'NONE',  ( 2.108352191060134828, 0.6683163022180199642, -1.600079515618204606 ) ) ;
#170310 = CARTESIAN_POINT ( 'NONE',  ( 3.983024850003999973, 2.060528110339276520, 0.6844299113566986170 ) ) ;
#170311 = CARTESIAN_POINT ( 'NONE',  ( 3.499976210622149253, 7.235056012367825140, 0.7998128361456321445 ) ) ;
#170312 = CARTESIAN_POINT ( 'NONE',  ( 4.083220446344194343, 1.622485107653489633, 1.197306254465977826 ) ) ;
#170313 = CARTESIAN_POINT ( 'NONE',  ( 2.812500000000002665, 1.451031289061236684, 1.451031289061000873 ) ) ;
#170314 = CARTESIAN_POINT ( 'NONE',  ( 1.499999999999987121, 3.077083334016149863, -0.8660254037844262731 ) ) ;
#170315 = CARTESIAN_POINT ( 'NONE',  ( 0.8328817383555222609, 0.1387611642639074438, 1.921445197033289976 ) ) ;
#170316 = CARTESIAN_POINT ( 'NONE',  ( -1.500000000000008216, 8.281250000682797818, 3.469446951953614189E-15 ) ) ;
#170317 = CARTESIAN_POINT ( 'NONE',  ( 4.781579470667713494, 0.2167243770262658464, -2.210780252931910717 ) ) ;
#170318 = VERTEX_POINT ( 'NONE', #206439 ) ;
#170319 = CARTESIAN_POINT ( 'NONE',  ( -0.2108831679770926115, 5.723481173670196043, -2.491210874135452613 ) ) ;
#170320 = CARTESIAN_POINT ( 'NONE',  ( 0.7499999999999885647, -0.01666666666664401442, 1.299038105676657340 ) ) ;
#170321 = CARTESIAN_POINT ( 'NONE',  ( 7.962716289927667113, 8.184257181204083409, -0.7998128361456291469 ) ) ;
#170322 = CARTESIAN_POINT ( 'NONE',  ( 5.219525951136835928, 7.112532914458205013, -1.443375672974051449 ) ) ;
#170323 = CARTESIAN_POINT ( 'NONE',  ( 3.285556943750000514, -1.713541666188707735, 1.896917185911906722 ) ) ;
#170324 = EDGE_CURVE ( 'NONE', #127955, #91043, #127963, .T. ) ;
#170325 = CARTESIAN_POINT ( 'NONE',  ( 0.5049021242206577220, -2.205252279087748235, -0.2660074523756980058 ) ) ;
#170326 = CARTESIAN_POINT ( 'NONE',  ( 5.969191311310417802, 1.729517061547349632, 0.9261464158661563140 ) ) ;
#170327 = CARTESIAN_POINT ( 'NONE',  ( 10.39874063200158893, 11.23421161353111586, 0.000000000000000000 ) ) ;
#170328 = EDGE_CURVE ( 'NONE', #123959, #193266, #181328, .T. ) ;
#170329 = CARTESIAN_POINT ( 'NONE',  ( -1.272148008267886654, 3.977632425219428391, -0.4878157535072980000 ) ) ;
#170330 = CARTESIAN_POINT ( 'NONE',  ( 6.591137597455673180, 1.973280021476801149, -1.106527213950120547 ) ) ;
#170331 = AXIS2_PLACEMENT_3D ( 'NONE', #209533, #12407, #64377 ) ;
#170333 = CONICAL_SURFACE ( 'NONE', #184554, 1.376945625684933061, 0.7853981633974491672 ) ;
#170332 = CARTESIAN_POINT ( 'NONE',  ( -5.641601317062248988, 6.714861303728305586, -1.082531754730549967 ) ) ;
#170334 = CARTESIAN_POINT ( 'NONE',  ( 3.561030563730323006, 1.627881067681248073, -1.266672197246907494 ) ) ;
#170335 = CARTESIAN_POINT ( 'NONE',  ( -4.660252114795309097, 6.460046772059735432, -1.599625672291256295 ) ) ;
#170336 = CARTESIAN_POINT ( 'NONE',  ( 1.499999999999989120, 3.535416667349488229, 0.8660254037844524744 ) ) ;
#170337 = CARTESIAN_POINT ( 'NONE',  ( -1.364683531249997417, 4.821875000341417916, 1.214306433183764966E-14 ) ) ;
#170338 = CARTESIAN_POINT ( 'NONE',  ( 5.237510374101456812, -1.321932271818569093, -1.323673891312632245 ) ) ;
#170339 = CARTESIAN_POINT ( 'NONE',  ( 3.445721922217106936, -1.531427584095602867, -0.8135701209448819027 ) ) ;
#170340 = CARTESIAN_POINT ( 'NONE',  ( 2.981702274927648944, -1.715113757222336721, -0.2947475401101228853 ) ) ;
#170341 = CARTESIAN_POINT ( 'NONE',  ( 1.154322298621703435, 0.9348496236407450866, 2.093279060508267175 ) ) ;
#170342 = CARTESIAN_POINT ( 'NONE',  ( -0.6823417656250212460, 4.363541667008085767, 1.181850606188767472 ) ) ;
#170343 = CARTESIAN_POINT ( 'NONE',  ( 4.880461040030859010, -0.2572269614671355842, -2.074807210009928848 ) ) ;
#170344 = CARTESIAN_POINT ( 'NONE',  ( 0.1285073612291263989, -1.684675954457705682, 0.7431698939026829542 ) ) ;
#170346 = EDGE_LOOP ( 'NONE', ( #76981, #122233, #68684, #186752 ) ) ;
#170345 = PLANE ( 'NONE',  #36269 ) ;
#170347 = CARTESIAN_POINT ( 'NONE',  ( 0.8795299900376440938, -0.4926441280813895762, -1.955172062459666904 ) ) ;
#170348 = CARTESIAN_POINT ( 'NONE',  ( 0.9496594531581278309, -1.914679731917130479, 0.9119059213342151082 ) ) ;
#170349 = CARTESIAN_POINT ( 'NONE',  ( 0.000000000000000000, 4.518459255872631530, 0.000000000000000000 ) ) ;
#170350 = DIRECTION ( 'NONE',  ( 0.000000000000000000, 0.000000000000000000, 1.000000000000000000 ) ) ;
#170351 = CARTESIAN_POINT ( 'NONE',  ( -8.715193815486133033, 9.062147627688959872, 0.7998128361456462443 ) ) ;
#170352 = CARTESIAN_POINT ( 'NONE',  ( 6.307567778855705853, 8.381915046796901692, -1.599625672291262513 ) ) ;
#170353 = CARTESIAN_POINT ( 'NONE',  ( 2.385534290476189145, 0.1013982516714604792, -2.118174289320504666 ) ) ;
#170354 = DIRECTION ( 'NONE',  ( 1.000000000000000000, 1.725633230170963762E-31, 8.638326563840814399E-31 ) ) ;
#170355 = CARTESIAN_POINT ( 'NONE',  ( 4.635264976507449397, -1.668059998867366778, 0.7425182445051290436 ) ) ;
#170356 = ORIENTED_EDGE ( 'NONE', *, *, #173988, .T. ) ;
#170357 = CARTESIAN_POINT ( 'NONE',  ( -7.781453819600577582, 8.043060642480948985, 0.000000000000000000 ) ) ;
#170358 = CARTESIAN_POINT ( 'NONE',  ( -7.815970093360414158E-14, 8.210952333604092601, -2.038660652713623733 ) ) ;
#170359 = CARTESIAN_POINT ( 'NONE',  ( -1.737500000000000266, -4.214583332377418223, -3.009438278150923907 ) ) ;
#170360 = CARTESIAN_POINT ( 'NONE',  ( -6.235860587281615075, 9.362588887548838557, -1.199719254218440723 ) ) ;
#170361 = CARTESIAN_POINT ( 'NONE',  ( 2.443623115440888061, -1.883043647339300186, 0.7309814453849405869 ) ) ;
#170362 = CARTESIAN_POINT ( 'NONE',  ( 5.596761079150560647, -0.5311557606857522096, -2.141783596114990917 ) ) ;
#170363 = CIRCLE ( 'NONE', #35380, 2.750000000000000444 ) ;
#170364 = CARTESIAN_POINT ( 'NONE',  ( -5.632486471834530661, 5.535932070087196344, -0.7998128361456362523 ) ) ;
#170365 = ADVANCED_FACE ( 'NONE', ( #40771 ), #62595, .T. ) ;
#170366 = CARTESIAN_POINT ( 'NONE',  ( 3.977287768980780402, -0.1405865315737795385, 1.855722876009910038 ) ) ;
#170367 = CARTESIAN_POINT ( 'NONE',  ( 10.37606763316019531, 10.99983374830873650, 0.7998128361456462443 ) ) ;
#170368 = CARTESIAN_POINT ( 'NONE',  ( 11.41381675112453387, 10.19999999999998153, 3.704697986577180746 ) ) ;
#170369 = CARTESIAN_POINT ( 'NONE',  ( -3.228813138348844536, 6.918699094715619502, 0.7998128361456341429 ) ) ;
#170370 = CARTESIAN_POINT ( 'NONE',  ( -7.263417608619167076, 9.497073181520933716, -1.599625672291263179 ) ) ;
#170371 = CARTESIAN_POINT ( 'NONE',  ( 4.705575438601840688, -0.4840451379145363497, 1.760283039881085809 ) ) ;
#170373 = CARTESIAN_POINT ( 'NONE',  ( -4.475961918153980257, 7.265020140467052023, -1.287590260893024086 ) ) ;
#170372 = CARTESIAN_POINT ( 'NONE',  ( -3.923105346307911745, 5.670318552149568703, -1.599625672291283607 ) ) ;
#170374 = CARTESIAN_POINT ( 'NONE',  ( 1.364683531249986537, -0.3447916663252443836, -0.7879004041258309554 ) ) ;
#170375 = CARTESIAN_POINT ( 'NONE',  ( 0.5965333524920403141, 0.8982759108043871787, -1.482850294500896560 ) ) ;
#170376 = CARTESIAN_POINT ( 'NONE',  ( 6.714805130922314014, -0.1276373473727103192, 1.811824464382847832 ) ) ;
#170377 = CARTESIAN_POINT ( 'NONE',  ( 5.742881039954627731, 0.4445991233769739925, 2.264314392639497520 ) ) ;
#170378 = CARTESIAN_POINT ( 'NONE',  ( 4.634908411025333130, 6.500755460986618495, 1.599625672291268286 ) ) ;
#170379 = CARTESIAN_POINT ( 'NONE',  ( 1.317730169365991522, -2.011166735366700209, 0.4487503453191737934 ) ) ;
#170380 = CARTESIAN_POINT ( 'NONE',  ( 6.468148293998644327, 1.905381763673856810, 1.285138856061205148 ) ) ;
#170381 = CARTESIAN_POINT ( 'NONE',  ( -9.499679989893815346, -7.184999792974224420, -0.07801928546529064701 ) ) ;
#170382 = CARTESIAN_POINT ( 'NONE',  ( -6.611536185319534908, 7.742488966741438716, 1.199719254218452047 ) ) ;
#170383 = CARTESIAN_POINT ( 'NONE',  ( 5.366025703835962446, 0.9229158262306772498, 1.627043297953718382 ) ) ;
#170385 = CARTESIAN_POINT ( 'NONE',  ( -3.526002468005825286, 6.271364091718859335, -1.199719254218450271 ) ) ;
#170384 = CARTESIAN_POINT ( 'NONE',  ( 3.445477555875466891, -1.765175379189663607, 0.7362804355328657069 ) ) ;
#170386 = CARTESIAN_POINT ( 'NONE',  ( 4.987059637548557411, -0.2676712469649074055, -2.190530366034774801 ) ) ;
#170387 = CARTESIAN_POINT ( 'NONE',  ( -5.157946788997579689E-14, 2.000000000682813805, -1.414508159514627383 ) ) ;
#170388 = CARTESIAN_POINT ( 'NONE',  ( 6.075462232699536891, 6.260663157670513179, -0.7216878364870596974 ) ) ;
#170389 = CARTESIAN_POINT ( 'NONE',  ( 3.729901657090938460, 7.365652676665848553, 0.7216878364870257245 ) ) ;
#170390 = CARTESIAN_POINT ( 'NONE',  ( -4.299344108864953995, 7.069632989434141201, -1.082531754730551743 ) ) ;
#170391 = CARTESIAN_POINT ( 'NONE',  ( 5.742871283745087041, 2.043606947765171267, 0.5656136300068030920 ) ) ;
#170392 = ORIENTED_EDGE ( 'NONE', *, *, #208132, .F. ) ;
#170393 = CARTESIAN_POINT ( 'NONE',  ( 3.188805362043587888, -2.273175341261697291, -0.3962186847288259317 ) ) ;
#170395 = EDGE_CURVE ( 'NONE', #121330, #25653, #21135, .T. ) ;
#170394 = CARTESIAN_POINT ( 'NONE',  ( 4.176187491914356897, -1.006606191838583131, -1.683785057063936552 ) ) ;
#170396 = CARTESIAN_POINT ( 'NONE',  ( -5.041653019435350380, 6.975290837464928728, -1.599625672291271394 ) ) ;
#170397 = CARTESIAN_POINT ( 'NONE',  ( 0.9538670997781794059, -0.7113550649951918547, 1.828410001767373450 ) ) ;
#170398 = FACE_BOUND ( 'NONE', #145758, .T. ) ;
#170399 = CARTESIAN_POINT ( 'NONE',  ( -9.367496997601914899, 15.46908218389976497, 7.499999999994665600 ) ) ;
#170400 = EDGE_LOOP ( 'NONE', ( #93788, #22335, #5546, #130358 ) ) ;
#170401 = CARTESIAN_POINT ( 'NONE',  ( 6.333220217719927270, -1.622483202430196725, -1.197309987464048486 ) ) ;
#170402 = CARTESIAN_POINT ( 'NONE',  ( -9.671043645249580933, 10.17730576241299900, 0.7998128361456462443 ) ) ;
#170403 = CARTESIAN_POINT ( 'NONE',  ( 8.717716733090741243, 13.27471476138783224, 8.129441245349513068 ) ) ;
#170404 = CARTESIAN_POINT ( 'NONE',  ( 3.010768451359053355, 0.7272417100659108735, 2.045797318486474836 ) ) ;
#170405 = CARTESIAN_POINT ( 'NONE',  ( 4.030516805012513082, 7.924296382481737844, 0.000000000000000000 ) ) ;
#170406 = CARTESIAN_POINT ( 'NONE',  ( 0.8090202166558431163, -0.5209130535433897924, -2.055487714681260236 ) ) ;
#170407 = CARTESIAN_POINT ( 'NONE',  ( -1.500000000000013101, 1.202083334016148974, 0.8660254037844403729 ) ) ;
#170408 = CARTESIAN_POINT ( 'NONE',  ( 8.516493047678546091, 13.08765898893368629, -0.7998128361456352531 ) ) ;
#170409 = CARTESIAN_POINT ( 'NONE',  ( -1.834547262740437557, 2.517098059729869330, -2.498887020409608084 ) ) ;
#170410 = CARTESIAN_POINT ( 'NONE',  ( 5.853046489161108035, 7.294594176516559614, 1.271900669079442325 ) ) ;
#170411 = CARTESIAN_POINT ( 'NONE',  ( 0.4564140224992017658, 0.7863226074062683590, 1.905069713448727775 ) ) ;
#170413 = CARTESIAN_POINT ( 'NONE',  ( 1.500000000000001332, 8.406250000682797818, 0.000000000000000000 ) ) ;
#170412 = CARTESIAN_POINT ( 'NONE',  ( -9.236128959407555072, 11.79856975744075598, -1.599625672291263179 ) ) ;
#170414 = CARTESIAN_POINT ( 'NONE',  ( -1.364683531250014514, 1.988541667008086655, -0.7879004041258289570 ) ) ;
#170415 = CARTESIAN_POINT ( 'NONE',  ( -1.499999999999997780, 5.400000000000022560, 1.214306433183764966E-14 ) ) ;
#170416 = EDGE_CURVE ( 'NONE', #108753, #179933, #93796, .T. ) ;
#170417 = ORIENTED_EDGE ( 'NONE', *, *, #106933, .T. ) ;
#170418 = CARTESIAN_POINT ( 'NONE',  ( 3.229067839489424330, 1.729836904712976686, 0.8154208365811002057 ) ) ;
#170419 = AXIS2_PLACEMENT_3D ( 'NONE', #35232, #11793, #208917 ) ;
#170420 = CARTESIAN_POINT ( 'NONE',  ( 5.823074959372767090, -0.03971387110058427483, 1.769581062106811986 ) ) ;
#170421 = CARTESIAN_POINT ( 'NONE',  ( 5.040599249230596435, 9.102725900736217568, 0.7998128361456341429 ) ) ;
#170422 =( GEOMETRIC_REPRESENTATION_CONTEXT ( 3 ) GLOBAL_UNCERTAINTY_ASSIGNED_CONTEXT ( ( #105648 ) ) GLOBAL_UNIT_ASSIGNED_CONTEXT ( ( #70788, #169386, #54572 ) ) REPRESENTATION_CONTEXT ( 'NONE', 'WORKASPACE' ) );
#170423 = CARTESIAN_POINT ( 'NONE',  ( -2.916975605234527702, 6.554888639415577423, 1.040834085586084257E-14 ) ) ;
#170424 = CARTESIAN_POINT ( 'NONE',  ( 0.7030050633033817498, 1.597335618216610964, -0.8546489784103310505 ) ) ;
#170426 = CARTESIAN_POINT ( 'NONE',  ( 1.077184250232362306, 1.452872634298128629, 1.248800971253192005 ) ) ;
#170425 = FACE_OUTER_BOUND ( 'NONE', #30626, .T. ) ;
#170427 = CARTESIAN_POINT ( 'NONE',  ( 2.189971326302230903, -1.350648006375281929, -1.569233719104834890 ) ) ;
#170428 = CARTESIAN_POINT ( 'NONE',  ( -1.402160292154681736E-14, -0.1156249996585793222, 1.575800808251672791 ) ) ;
#170429 = CARTESIAN_POINT ( 'NONE',  ( 6.596569749568344854, -0.5012203084251048990, -1.802199723311518786 ) ) ;
#170430 = CARTESIAN_POINT ( 'NONE',  ( 2.402731849113007190, 1.466575434288765800, -1.087121784572639527 ) ) ;
#170432 = CARTESIAN_POINT ( 'NONE',  ( 5.916355900263067014, 7.140870225795406867, 1.119544393390920600 ) ) ;
#170431 = CARTESIAN_POINT ( 'NONE',  ( 0.2765547061623524483, 1.334074794448695034, 1.882843260577294009 ) ) ;
#170433 = CARTESIAN_POINT ( 'NONE',  ( -1.364683531250014514, 0.03020833367475737191, 0.7879004041258379498 ) ) ;
#170434 = CARTESIAN_POINT ( 'NONE',  ( 4.439923992641017669, 1.344862922493793578, 1.564070066283109295 ) ) ;
#170435 = CARTESIAN_POINT ( 'NONE',  ( -7.386494761346872551, 7.511998731193139989, -0.7998128361456291469 ) ) ;
#170436 = CARTESIAN_POINT ( 'NONE',  ( 9.074484886248265880, 9.481320543578137361, 0.7998128361456462443 ) ) ;
#170437 = CARTESIAN_POINT ( 'NONE',  ( 3.655894977179307226, 7.416961240017848844, -0.7998128361456291469 ) ) ;
#170438 = CARTESIAN_POINT ( 'NONE',  ( 4.632082037363250748, 8.555846143565791095, -0.7998128361456231517 ) ) ;
#170439 = CARTESIAN_POINT ( 'NONE',  ( 1.499999999999989120, 4.254166666666687746, 0.8660254037844524744 ) ) ;
#170440 = CARTESIAN_POINT ( 'NONE',  ( 6.689897370947560873, -1.349224794794257720, -1.570457413003906177 ) ) ;
#170441 = CARTESIAN_POINT ( 'NONE',  ( 0.6823417656249882723, 0.9885416670080832136, -1.181850606188749264 ) ) ;
#170442 = CARTESIAN_POINT ( 'NONE',  ( 3.392016793147753617, -0.8794390384766533897, 1.974801309016629869 ) ) ;
#170444 = EDGE_CURVE ( 'NONE', #40241, #113311, #78576, .T. ) ;
#170443 = CARTESIAN_POINT ( 'NONE',  ( 4.248697963213067474, 1.981114831247460017, 0.3918398546494082368 ) ) ;
#170445 = B_SPLINE_CURVE_WITH_KNOTS ( 'NONE', 3,
 ( #52251, #6678, #138852, #102069, #137785, #150834, #118378, #40278, #171327, #106388 ),
 .UNSPECIFIED., .F., .F.,
 ( 4, 2, 2, 2, 4 ),
 ( 0.000000000000000000, 0.0002334048330869039766, 0.0004668096661738078447, 0.0007002144992607117670, 0.0009336193323476156894 ),
 .UNSPECIFIED. ) ;
#170446 = CARTESIAN_POINT ( 'NONE',  ( 6.720655732516641834, 2.402268298795938950, 2.653651172607660591 ) ) ;
#170447 = EDGE_CURVE ( 'NONE', #156117, #182073, #29847, .T. ) ;
#170450 = CARTESIAN_POINT ( 'NONE',  ( 5.327991180490514012, 9.159814110640187579, 1.040834085586084257E-14 ) ) ;
#170449 = CARTESIAN_POINT ( 'NONE',  ( 1.001543065824772753E-15, -2.821874999522044458, 3.793834371823811669 ) ) ;
#170448 = CARTESIAN_POINT ( 'NONE',  ( -1.432719062495390716, -3.042800438942089514, 3.165902886691621010 ) ) ;
#170451 = CARTESIAN_POINT ( 'NONE',  ( -5.281783360975562225, 8.319775133516907673, 1.199719254218452935 ) ) ;
#170452 = CARTESIAN_POINT ( 'NONE',  ( 2.975796278104340331, -0.8128168404246680634, 1.845627246706407210 ) ) ;
#170453 = CARTESIAN_POINT ( 'NONE',  ( -7.497822643557261024, 8.706213491360317747, -1.199719254218446718 ) ) ;
#170455 = CARTESIAN_POINT ( 'NONE',  ( -1.123270288250343141, 3.096052654332833054, 0.7749999999993751887 ) ) ;
#170454 = CARTESIAN_POINT ( 'NONE',  ( -3.242371291962510504, 6.934516940598226320, 1.040834085586084257E-14 ) ) ;
#170456 = CARTESIAN_POINT ( 'NONE',  ( -3.725947703184500970, 7.355943492750648183, 0.6041107585062406304 ) ) ;
#170457 = CARTESIAN_POINT ( 'NONE',  ( 6.293217207623316156, -0.1008467329366956045, -1.909883259500498198 ) ) ;
#170458 = CARTESIAN_POINT ( 'NONE',  ( 6.720655732516667591, 2.416141799769660370, 2.554522868665403568 ) ) ;
#170460 = CARTESIAN_POINT ( 'NONE',  ( 4.025017672583341977, -1.753021876717888006, 0.9963191169995513352 ) ) ;
#170459 = CARTESIAN_POINT ( 'NONE',  ( -7.768458830506062007, 11.04665715469030296, 1.082531754730549967 ) ) ;
#170461 = CARTESIAN_POINT ( 'NONE',  ( 0.7499999999999920064, 5.233333333333353821, 1.299038105676669330 ) ) ;
#170462 = CARTESIAN_POINT ( 'NONE',  ( 1.364683531249996529, 8.463541667008065872, 0.7879004041258405033 ) ) ;
#170463 = CARTESIAN_POINT ( 'NONE',  ( 6.299779570463345912, -0.5759050694413189175, 1.625906498142214884 ) ) ;
#170464 = CARTESIAN_POINT ( 'NONE',  ( 5.417364897112183719, 8.477953592343014932, 1.199719254218451159 ) ) ;
#170465 = CARTESIAN_POINT ( 'NONE',  ( 8.080296364064698977, 12.37083682481011060, -0.7216878364870328300 ) ) ;
#170466 = CARTESIAN_POINT ( 'NONE',  ( 10.99962150373186986, -9.999999999999879208, -0.09125116240082961627 ) ) ;
#170467 = CARTESIAN_POINT ( 'NONE',  ( 5.167206475355686557, 0.1846639555213614448, -1.861428779493356167 ) ) ;
#170468 = CARTESIAN_POINT ( 'NONE',  ( 6.082294971626270197, 1.038730605371197324, 1.724430661308763213 ) ) ;
#170469 = CARTESIAN_POINT ( 'NONE',  ( 1.500000000000007105, 10.64264068711930733, 1.214306433183764966E-14 ) ) ;
#170470 = CARTESIAN_POINT ( 'NONE',  ( 2.448173108494243078, -0.8891298726186761536, 1.869765896676472083 ) ) ;
#170471 = CARTESIAN_POINT ( 'NONE',  ( -2.361527856944989345E-15, -9.448428148670510396, -9.261795338153651969 ) ) ;
#170472 = ORIENTED_EDGE ( 'NONE', *, *, #91659, .T. ) ;
#170473 = CARTESIAN_POINT ( 'NONE',  ( 1.177361486786612899, 1.528755565978222819, 1.314981834344926437 ) ) ;
#170474 = CARTESIAN_POINT ( 'NONE',  ( 1.406221933027915982, -1.803026290124358555, -0.1754379831288860880 ) ) ;
#170475 = CARTESIAN_POINT ( 'NONE',  ( 3.214691819771663628, 6.764574533126651801, -0.7216878364870338292 ) ) ;
#170476 = CYLINDRICAL_SURFACE ( 'NONE', #204376, 0.09999999999999982514 ) ;
#170477 = CARTESIAN_POINT ( 'NONE',  ( 9.219181267168295335, 9.858059021225592744, 1.040834085586084257E-14 ) ) ;
#170478 = CARTESIAN_POINT ( 'NONE',  ( 7.775764792637399836, 9.030479331953833011, -1.199719254218441611 ) ) ;
#170479 = CIRCLE ( 'NONE', #49435, 0.08000000000000014044 ) ;
#170481 = CARTESIAN_POINT ( 'NONE',  ( 6.468375100207775397, -1.879703733780390795, -0.3681822884963186215 ) ) ;
#170480 = CARTESIAN_POINT ( 'NONE',  ( -7.217017841176048165, 7.314275657660511243, 1.040834085586084257E-14 ) ) ;
#170482 = CIRCLE ( 'NONE', #187648, 2.021340551328831392 ) ;
#170483 = CARTESIAN_POINT ( 'NONE',  ( 0.4799999999999758349, 2.999999999999999112, 2.420000000000000373 ) ) ;
#170484 = DIRECTION ( 'NONE',  ( -0.000000000000000000, -0.000000000000000000, -1.000000000000000000 ) ) ;
#170485 = CARTESIAN_POINT ( 'NONE',  ( 1.364683531249988757, -0.8031249996585804185, 0.000000000000000000 ) ) ;
#170487 = VERTEX_POINT ( 'NONE', #161985 ) ;
#170486 = CARTESIAN_POINT ( 'NONE',  ( 3.714570900464274850, 6.317121236308204324, 1.082531754730558626 ) ) ;
#170488 = CARTESIAN_POINT ( 'NONE',  ( -4.796887421136680985, 4.490790167614548523, 1.214306433183764966E-14 ) ) ;
#170489 = CARTESIAN_POINT ( 'NONE',  ( -8.080296364064746939, 9.489729181906076505, 1.082531754730558626 ) ) ;
#170490 = CARTESIAN_POINT ( 'NONE',  ( 3.292016909520224743, -0.8776455207864016783, 1.975710135277891633 ) ) ;
#170491 = CARTESIAN_POINT ( 'NONE',  ( -5.641601317062233001, 9.595968946632336127, -0.7216878364870338292 ) ) ;
#170492 = CARTESIAN_POINT ( 'NONE',  ( 5.397554552016204710, 9.311247720745345902, 0.7216878364870317197 ) ) ;
#170493 = CARTESIAN_POINT ( 'NONE',  ( 1.055114822555893950, 0.4192091730233596381, 2.078585086915801128 ) ) ;
#170494 = CARTESIAN_POINT ( 'NONE',  ( 5.825187583072056974, -0.04236064406601056098, 1.825263316621673848 ) ) ;
#170495 = CIRCLE ( 'NONE', #39095, 1.250000000000000888 ) ;
#170496 = CARTESIAN_POINT ( 'NONE',  ( 1.757037784194936725, -1.688679813833958709, -1.016973138862599102 ) ) ;
#170497 = CARTESIAN_POINT ( 'NONE',  ( 4.482611839828003930, -1.244964735940889522, 1.451779576051547282 ) ) ;
#170498 = ORIENTED_EDGE ( 'NONE', *, *, #2927, .T. ) ;
#170499 = CARTESIAN_POINT ( 'NONE',  ( 0.000000000000000000, 15.50000000000019362, 0.000000000000000000 ) ) ;
#170500 = CARTESIAN_POINT ( 'NONE',  ( 4.562928411757408043, 1.523777916087779571, -1.247912438812292413 ) ) ;
#170501 = CARTESIAN_POINT ( 'NONE',  ( 6.620655732516682157, 0.004685112605702904456, 1.926407831898164114 ) ) ;
#170502 = VERTEX_POINT ( 'NONE', #11436 ) ;
#170503 = CARTESIAN_POINT ( 'NONE',  ( -6.120580001926503755, 6.105374521861167914, -0.7998128361456362523 ) ) ;
#170505 = DIRECTION ( 'NONE',  ( -5.578564026256490882E-16, -1.000000000000000000, -9.066213480720158442E-32 ) ) ;
#170504 = CARTESIAN_POINT ( 'NONE',  ( -5.483346782084204563, 5.361935765378481378, 0.000000000000000000 ) ) ;
#170507 = CARTESIAN_POINT ( 'NONE',  ( 5.031484404002867450, 8.884165881396448583, 0.7216878364870317197 ) ) ;
#170506 = CARTESIAN_POINT ( 'NONE',  ( 7.096803341749390981, 10.36702210109460154, -1.199719254218441611 ) ) ;
#170509 = VERTEX_POINT ( 'NONE', #45043 ) ;
#170508 = CARTESIAN_POINT ( 'NONE',  ( 5.320932177894995618, 1.445329238430465013, -1.252218921613167169 ) ) ;
#170510 = AXIS2_PLACEMENT_3D ( 'NONE', #174068, #109111, #108044 ) ;
#170511 = CARTESIAN_POINT ( 'NONE',  ( 0.4642757356001780966, 2.182421439735841684, -0.3260586787675948117 ) ) ;
#170512 = CARTESIAN_POINT ( 'NONE',  ( 0.4307572970102537813, 3.041534709929992975, -0.4240169840791682132 ) ) ;
#170513 = CARTESIAN_POINT ( 'NONE',  ( 5.865890606937535168, 0.5820329372835297832, -1.927131433562751406 ) ) ;
#170514 = CARTESIAN_POINT ( 'NONE',  ( -0.02338929933909470252, 2.896474228846234844, -2.200133910884606081 ) ) ;
#170515 = CARTESIAN_POINT ( 'NONE',  ( -5.070811854594947654, 7.957075094197910481, 1.225549284076495438 ) ) ;
#170516 = FACE_OUTER_BOUND ( 'NONE', #167511, .T. ) ;
#170517 = CARTESIAN_POINT ( 'NONE',  ( 3.051297593704501043, 1.777051743073382761, -1.062048545217339601 ) ) ;
#170518 = CARTESIAN_POINT ( 'NONE',  ( -5.228640796364566690, 9.251831362400652736, -0.7998128361456231517 ) ) ;
#170519 = CARTESIAN_POINT ( 'NONE',  ( -4.844715248835366417, 8.098060037232425401, 0.8884674472836263659 ) ) ;
#170521 = CARTESIAN_POINT ( 'NONE',  ( 0.6202742476981680797, -1.157488721396517040, -1.825510493854154426 ) ) ;
#170520 = CARTESIAN_POINT ( 'NONE',  ( -4.115063316947640715, 4.759660943649018705, 1.199719254218462483 ) ) ;
#170522 = CARTESIAN_POINT ( 'NONE',  ( -11.32603390678133159, 7.709074399366075525, 3.972318804447378504 ) ) ;
#170523 = CARTESIAN_POINT ( 'NONE',  ( 4.800995793014950941, 5.734154859006458160, -1.082531754730548412 ) ) ;
#170524 = CARTESIAN_POINT ( 'NONE',  ( 7.720982897393565914, -6.307829212974243482, -7.834948825496931057 ) ) ;
#170525 = CARTESIAN_POINT ( 'NONE',  ( 1.364683531249996529, 12.52604166700806054, 0.7879004041258405033 ) ) ;
#170527 = CARTESIAN_POINT ( 'NONE',  ( -4.471156797456668386, 8.438376373666578445, -0.7998128361456362523 ) ) ;
#170526 = CARTESIAN_POINT ( 'NONE',  ( 6.925078400183550364, 2.460400685555228950, 2.239421262742965268 ) ) ;
#170528 = CARTESIAN_POINT ( 'NONE',  ( 4.447759528527571504, -1.551977624003277212, -0.7738437340010505539 ) ) ;
#170529 = CARTESIAN_POINT ( 'NONE',  ( -4.090809663021341969, 5.795697244990093644, 1.599625672291267398 ) ) ;
#170530 = CARTESIAN_POINT ( 'NONE',  ( 3.485274717979901293, 0.04603381543630095940, 2.069897711131869933 ) ) ;
#170531 = CARTESIAN_POINT ( 'NONE',  ( 4.974263482967073990, -2.101360013415910721, -0.2580830166784564006 ) ) ;
#170532 = CARTESIAN_POINT ( 'NONE',  ( 6.805303039055573322, 10.02693841461847057, 1.199719254218460707 ) ) ;
#170533 = CARTESIAN_POINT ( 'NONE',  ( 1.364683531249988535, 4.113541667008088432, 0.7879004041258499402 ) ) ;
#170534 = CARTESIAN_POINT ( 'NONE',  ( 1.955843269872016066, -0.6684750375501640196, 1.852638994923772930 ) ) ;
#170535 = CARTESIAN_POINT ( 'NONE',  ( 1.283307755816986528, 0.1377011610334301639, -1.907463248872851569 ) ) ;
#170536 = CARTESIAN_POINT ( 'NONE',  ( 5.332074485713341971, 2.257618135992002895, 0.3962004586785839444 ) ) ;
#170537 = CARTESIAN_POINT ( 'NONE',  ( 1.892912435568369744, 1.589020553905008626, -0.8988452475950716725 ) ) ;
#170538 = CARTESIAN_POINT ( 'NONE',  ( 6.229045230835819069, 6.231917288922055320, -0.7998128361456481317 ) ) ;
#170539 = CARTESIAN_POINT ( 'NONE',  ( 5.870317324592803310, 7.871789516823500144, -1.443375672974057666 ) ) ;
#170540 = CARTESIAN_POINT ( 'NONE',  ( -6.184490626128011925, 10.36698949712469364, -0.7998128361456291469 ) ) ;
#170541 = EDGE_CURVE ( 'NONE', #188369, #117790, #70026, .T. ) ;
#170542 = CARTESIAN_POINT ( 'NONE',  ( 3.322524176979495980, -0.8198387518110359373, -1.838900561053190774 ) ) ;
#170543 = CARTESIAN_POINT ( 'NONE',  ( 3.748837004188230182, -0.3782986639458625899, -1.924763881548184230 ) ) ;
#170544 = CARTESIAN_POINT ( 'NONE',  ( -6.344325816190970357, 9.489131654609717970, 1.199719254218452047 ) ) ;
#170545 = CARTESIAN_POINT ( 'NONE',  ( -4.954615070790188369, 7.867802451642154082, -1.199719254218452047 ) ) ;
#170546 = CARTESIAN_POINT ( 'NONE',  ( 0.1753634416057497647, 0.0001173177735149660568, -2.144164757042036573 ) ) ;
#170548 = CARTESIAN_POINT ( 'NONE',  ( 4.416719503454580753, 1.618597840523916753, 0.7163212975811702465 ) ) ;
#170547 = CARTESIAN_POINT ( 'NONE',  ( 5.824191892830967276, 2.014527380540787505, 0.5587128073646082660 ) ) ;
#170549 = CARTESIAN_POINT ( 'NONE',  ( 0.000000000000000000, -9.999999999999994671, 0.000000000000000000 ) ) ;
#170550 = CARTESIAN_POINT ( 'NONE',  ( 0.4104466507391414387, 1.508250410577081979, -1.590083307377434974 ) ) ;
#170551 = CARTESIAN_POINT ( 'NONE',  ( 6.714805129994689814, -0.1247508129638870145, 1.711716247594262441 ) ) ;
#170552 = EDGE_CURVE ( 'NONE', #126346, #23033, #211334, .T. ) ;
#170553 = CARTESIAN_POINT ( 'NONE',  ( 5.601490020740366838, 9.686822124172440596, 1.040834085586084257E-14 ) ) ;
#170554 = CARTESIAN_POINT ( 'NONE',  ( 0.1331715793776600265, 2.877549198462618474, -2.442236402435117526 ) ) ;
#170555 = CARTESIAN_POINT ( 'NONE',  ( 6.609999999999973674, -0.005249217919313375023, 2.280159464062641916 ) ) ;
#170556 = CARTESIAN_POINT ( 'NONE',  ( -0.9311234436981496998, -1.284380368602565659, 3.475000000000000977 ) ) ;
#170557 = CARTESIAN_POINT ( 'NONE',  ( 1.981372325807278623, -0.1102420082176903682, -2.204251428397439483 ) ) ;
#170558 = AXIS2_PLACEMENT_3D ( 'NONE', #38330, #34059, #53512 ) ;
#170559 = CARTESIAN_POINT ( 'NONE',  ( 6.777770921962916972, -2.107754466287181661, 0.5206637005944132479 ) ) ;
#170560 = LINE ( 'NONE', #22143, #6072 ) ;
#170561 = CARTESIAN_POINT ( 'NONE',  ( 1.552129107922173068, 1.093532845977844170, 1.812997832068358850 ) ) ;
#170562 = CARTESIAN_POINT ( 'NONE',  ( 2.781250000000002665, 0.7852924748301273183, 1.895863743164028170 ) ) ;
#170563 = COLOUR_RGB ( '', 0.66274510, 0.83137255, 0.94901961) ;
#170564 = CARTESIAN_POINT ( 'NONE',  ( 6.727182134110194056, 3.682851444631680682, 2.702965647100654234 ) ) ;
#170565 = CARTESIAN_POINT ( 'NONE',  ( 4.893539313097565291, 1.427316681580325763, 1.293898783310668987 ) ) ;
#170566 = ORIENTED_EDGE ( 'NONE', *, *, #57726, .T. ) ;
#170568 = CARTESIAN_POINT ( 'NONE',  ( -1.500000000000011324, 5.670833333333358262, 0.8660254037844403729 ) ) ;
#170567 = CARTESIAN_POINT ( 'NONE',  ( 1.804612524702827514, 1.695363242818634930, -1.543121881923440020 ) ) ;
#170569 = CARTESIAN_POINT ( 'NONE',  ( 3.649115900372475796, 7.409052317076538330, 1.040834085586084257E-14 ) ) ;
#170570 = CARTESIAN_POINT ( 'NONE',  ( 6.993308306550549247, 7.053281200597435685, 1.040834085586084257E-14 ) ) ;
#170571 = EDGE_CURVE ( 'NONE', #138555, #184190, #41709, .T. ) ;
#170572 = CARTESIAN_POINT ( 'NONE',  ( 3.932468528151237042, -1.142516171320803853, -1.904832733444387971 ) ) ;
#170573 = CARTESIAN_POINT ( 'NONE',  ( -8.270110514656041190, 10.67154823856396817, 1.443375672974090751 ) ) ;
#170574 = CARTESIAN_POINT ( 'NONE',  ( 7.632877294813741109, 8.007371053478589573, 1.040834085586084257E-14 ) ) ;
#170575 = EDGE_CURVE ( 'NONE', #26370, #155330, #14188, .T. ) ;
#170576 = CARTESIAN_POINT ( 'NONE',  ( -6.982085920913410071, 11.08959130780024260, 0.7216878364870458196 ) ) ;
#170577 = CARTESIAN_POINT ( 'NONE',  ( 6.061904079085887354, 6.244845311787889486, 0.000000000000000000 ) ) ;
#170578 = CARTESIAN_POINT ( 'NONE',  ( 1.899064777474347654, -0.9530127170578571727, -1.777010740487514173 ) ) ;
#170580 = CARTESIAN_POINT ( 'NONE',  ( 6.426245203579573406, 1.057156898221789598, 1.771034054399809987 ) ) ;
#170579 = CARTESIAN_POINT ( 'NONE',  ( 7.914208982075123799, 10.25632978388623684, -1.599625672291262513 ) ) ;
#170581 = CARTESIAN_POINT ( 'NONE',  ( -10.99374989157288240, -6.893136995915043919, 0.3811408430856400575 ) ) ;
#170582 = CARTESIAN_POINT ( 'NONE',  ( 6.089020385868848528, 8.197219431637373432, -1.443375672974078761 ) ) ;
#170583 = CARTESIAN_POINT ( 'NONE',  ( 6.480030497237043718, -1.708793550445006248, -0.3294957622956768972 ) ) ;
#170584 = CARTESIAN_POINT ( 'NONE',  ( -0.6823417656250212460, 2.301041667008084435, 1.181850606188767472 ) ) ;
#170585 = CARTESIAN_POINT ( 'NONE',  ( 1.422737370818322633, -0.05026339470881428795, 1.769212045163440106 ) ) ;
#170586 = CARTESIAN_POINT ( 'NONE',  ( -0.1399997263889594112, -0.002789056014654289761, -2.000146600338557956 ) ) ;
#170587 = CARTESIAN_POINT ( 'NONE',  ( 6.356985390939413172, 0.2876776518413763917, -1.716344579348449084 ) ) ;
#170588 = CARTESIAN_POINT ( 'NONE',  ( 3.808379203468327034, 1.620604861375672945, -1.621544036339316985 ) ) ;
#170589 = CARTESIAN_POINT ( 'NONE',  ( 3.784953330938052751, 1.334695924059103644, 1.268461399425282687 ) ) ;
#170590 = CARTESIAN_POINT ( 'NONE',  ( 9.596473800374404561, 10.09030761005864285, 0.000000000000000000 ) ) ;
#170591 = CARTESIAN_POINT ( 'NONE',  ( 8.662992978453381454, 14.42103047445972308, -8.321347630537264450 ) ) ;
#170592 = CARTESIAN_POINT ( 'NONE',  ( 4.559475717982610199, 0.3993622990657343941, -1.781190812766835441 ) ) ;
#170593 = CARTESIAN_POINT ( 'NONE',  ( 4.535779832184696936, -1.617819081767550182, 1.203352566194588746 ) ) ;
#170594 = CARTESIAN_POINT ( 'NONE',  ( -8.317037166979361018, 11.79062823052953668, 1.199719254218453823 ) ) ;
#170596 = CARTESIAN_POINT ( 'NONE',  ( -8.093291352714894415, 8.406871097780989288, -0.7998128361456362523 ) ) ;
#170595 = CARTESIAN_POINT ( 'NONE',  ( 3.907294183660753539, 1.938944517003845736, 1.165763813888931688 ) ) ;
#170597 = CARTESIAN_POINT ( 'NONE',  ( 0.01252217983070766719, -0.9030397145437498718, -1.901010321977952389 ) ) ;
#170598 = CARTESIAN_POINT ( 'NONE',  ( -11.89829993707161648, 13.82919228251126142, -1.561606677374349772 ) ) ;
#170599 = CARTESIAN_POINT ( 'NONE',  ( 4.123533666479628046, 0.2564666318346648377, -2.054367117340555549 ) ) ;
#170600 = CARTESIAN_POINT ( 'NONE',  ( 2.354312230267378236, 5.898448035287240820, -0.7998128361456281477 ) ) ;
#170601 = CARTESIAN_POINT ( 'NONE',  ( -0.6801582343750368631, 2.130208333674714183, -1.178068619123862515 ) ) ;
#170602 = CARTESIAN_POINT ( 'NONE',  ( 5.461630201184114242, -1.671734486004393450, -1.304435072541964447 ) ) ;
#170603 = CONTEXT_DEPENDENT_SHAPE_REPRESENTATION ( #190160, #195953 ) ;
#170605 = CARTESIAN_POINT ( 'NONE',  ( 2.596214140771450296, -1.921342217666447860, -0.1417109463846803752 ) ) ;
#170604 = CARTESIAN_POINT ( 'NONE',  ( -9.073431116043565225, 11.60875560684942265, -1.599625672291263179 ) ) ;
#170606 = UNCERTAINTY_MEASURE_WITH_UNIT (LENGTH_MEASURE( 1.000000000000000082E-05 ), #138785, 'distance_accuracy_value', 'NONE');
#170607 = CARTESIAN_POINT ( 'NONE',  ( -5.002032328799064231, 4.800402236545811441, -0.7998128361456362523 ) ) ;
#170608 = CARTESIAN_POINT ( 'NONE',  ( 0.1390025477998011738, -0.1451226239368992033, -1.937570863154890688 ) ) ;
#170609 = CARTESIAN_POINT ( 'NONE',  ( 4.868786560638896255, 5.813244087901094481, 1.082531754730549078 ) ) ;
#170610 = CARTESIAN_POINT ( 'NONE',  ( 5.891550962509589873, 5.977563058329811163, 0.05700887847147687038 ) ) ;
#170611 = CARTESIAN_POINT ( 'NONE',  ( 1.177110729581195114, 3.245878374463980975, -0.7749999999999840350 ) ) ;
#170612 = CARTESIAN_POINT ( 'NONE',  ( -2.903417451620861289, 6.539070793532962611, 0.7998128361456341429 ) ) ;
#170613 = CARTESIAN_POINT ( 'NONE',  ( 0.05339833992625257070, 0.3882609103176749010, 2.187096328411592516 ) ) ;
#170614 = CARTESIAN_POINT ( 'NONE',  ( 2.889785439676189505, 1.488280975668257344, 1.490260817651526182 ) ) ;
#170615 = CARTESIAN_POINT ( 'NONE',  ( -3.332271893908731464, 7.109677319527304640, -0.7998128361456481317 ) ) ;
#170616 = CARTESIAN_POINT ( 'NONE',  ( 6.238723240582662477, 10.43026088065513513, -0.7998128361456291469 ) ) ;
#170617 = CARTESIAN_POINT ( 'NONE',  ( 0.5196754285911856508, 1.841638447829671899, -0.2671899778997516850 ) ) ;
#170618 = CARTESIAN_POINT ( 'NONE',  ( 5.601490020740366838, 9.686822124172440596, 1.040834085586084257E-14 ) ) ;
#170619 = DIRECTION ( 'NONE',  ( 0.000000000000000000, 1.000000000000000000, 0.000000000000000000 ) ) ;
#170620 = CARTESIAN_POINT ( 'NONE',  ( -5.316205630334251531, 9.216340645449683677, -0.7216878364870338292 ) ) ;
#170621 = B_SPLINE_CURVE_WITH_KNOTS ( 'NONE', 3,
 ( #45426, #162369, #161299, #145083, #96314, #208949 ),
 .UNSPECIFIED., .F., .F.,
 ( 4, 2, 4 ),
 ( 0.000000000000000000, 0.0003844267940947826553, 0.0007688535881895653106 ),
 .UNSPECIFIED. ) ;
#170622 = CARTESIAN_POINT ( 'NONE',  ( -7.646435448427427062, 10.90429654226522693, 1.082531754730549967 ) ) ;
#170623 = CARTESIAN_POINT ( 'NONE',  ( 0.8969213510382867405, -2.070190491330957006, -0.4589741369691033857 ) ) ;
#170624 = CARTESIAN_POINT ( 'NONE',  ( -6.912678218121246942, 9.158153569265168770, 1.599625672291269396 ) ) ;
#170626 = CARTESIAN_POINT ( 'NONE',  ( 2.945700582358207864, 1.385421296276163838, 1.389331660621349274 ) ) ;
#170625 = CARTESIAN_POINT ( 'NONE',  ( 0.6125000000000001554, 1.166666666666656083, -1.060881119635941339 ) ) ;
#170627 = CARTESIAN_POINT ( 'NONE',  ( 2.377987466095924152, 1.329388817951412394, 1.704534938537699995 ) ) ;
#170628 = CARTESIAN_POINT ( 'NONE',  ( 2.120424178990498731, 0.001545453418709194504, 1.841430844159386293 ) ) ;
#170630 = CARTESIAN_POINT ( 'NONE',  ( -5.402149754905330781, 6.322992007072439691, -1.066970298751448443 ) ) ;
#170629 = CARTESIAN_POINT ( 'NONE',  ( -3.851398154733808088, 6.650992392901508232, -1.199719254218450271 ) ) ;
#170631 = CARTESIAN_POINT ( 'NONE',  ( 3.890341755399207013, 1.468866505370895137, -0.9330376088199500151 ) ) ;
#170632 = CARTESIAN_POINT ( 'NONE',  ( 5.992340707560163793, 6.093411701682730275, 0.7216878364870317197 ) ) ;
#170633 = CARTESIAN_POINT ( 'NONE',  ( -10.50659947519749693, 5.359800460605414152, -5.105385958519358169 ) ) ;
#170634 = CARTESIAN_POINT ( 'NONE',  ( 1.182749364907993206, -2.109161078630458430, -0.4729781282231394490 ) ) ;
#170635 = VECTOR ( 'NONE', #89672, 1000.000000000000000 ) ;
#170636 = CARTESIAN_POINT ( 'NONE',  ( 3.321638586175166719, -1.528507173905558014, 1.314795459203411676 ) ) ;
#170637 = CARTESIAN_POINT ( 'NONE',  ( -8.961576348508637935, 12.43862759236002269, -1.082531754730543083 ) ) ;
#170639 = PRESENTATION_LAYER_ASSIGNMENT (  '', '', ( #163702 ) ) ;
#170638 = CARTESIAN_POINT ( 'NONE',  ( 0.4269344243218140544, 2.069031678568326704, 0.6260965431626740463 ) ) ;
#170640 = CARTESIAN_POINT ( 'NONE',  ( 1.903138372489954655, 1.638015138609005383, 1.096796735940619660 ) ) ;
#170641 = CARTESIAN_POINT ( 'NONE',  ( 6.609000000000047947, 0.5928748489389294996, 1.953858053793898542 ) ) ;
#170642 = CARTESIAN_POINT ( 'NONE',  ( 2.296341162515431744, 1.558512652156778699, -1.158513924970270059 ) ) ;
#170645 = EDGE_LOOP ( 'NONE', ( #121034, #43713, #106628, #73827 ) ) ;
#170644 = CARTESIAN_POINT ( 'NONE',  ( -4.909461021924285795, 6.821066840368686712, 1.443375672974058777 ) ) ;
#170643 = FILL_AREA_STYLE ('',( #124129 ) ) ;
#170646 = CARTESIAN_POINT ( 'NONE',  ( -3.973948422136970748, 6.690004688251493192, -1.082531754730546636 ) ) ;
#170647 = CARTESIAN_POINT ( 'NONE',  ( -0.2108831679771168421, 7.629137130509075604, -2.497154329497493386 ) ) ;
#170648 = CARTESIAN_POINT ( 'NONE',  ( 6.398522151006641678, 6.429640362454684954, 0.000000000000000000 ) ) ;
#170649 = CARTESIAN_POINT ( 'NONE',  ( -6.791708605802965870, 6.888357893050385705, -0.7998128361456362523 ) ) ;
#170650 = CARTESIAN_POINT ( 'NONE',  ( -7.293360289508603600, 7.473618190706972086, 0.000000000000000000 ) ) ;
#170651 = CARTESIAN_POINT ( 'NONE',  ( -1.291015824433223491, 4.080642823807198560, -0.4575187270168924458 ) ) ;
#170652 = CARTESIAN_POINT ( 'NONE',  ( 0.1654306582001447423, -1.972458130798220077, -0.9897840116655574061 ) ) ;
#170654 = EDGE_CURVE ( 'NONE', #106155, #173996, #126658, .T. ) ;
#170653 = CARTESIAN_POINT ( 'NONE',  ( 1.685698123273788651, -1.500000000000000000, -1.979500400907064916 ) ) ;
#170655 = CARTESIAN_POINT ( 'NONE',  ( 3.959774770350584561, -0.5736532364168048792, 1.875976257969473648 ) ) ;
#170656 = CARTESIAN_POINT ( 'NONE',  ( 8.606728586576791074, 8.935604860628076906, 0.7998128361456462443 ) ) ;
#170657 = CARTESIAN_POINT ( 'NONE',  ( 2.039685609654022347, -1.556907966322677472, 1.281362143053674130 ) ) ;
#170658 = ORIENTED_EDGE ( 'NONE', *, *, #195789, .F. ) ;
#170659 = CARTESIAN_POINT ( 'NONE',  ( 2.764987222883477980, -0.1607348756041589999, -2.111328481229361564 ) ) ;
#170660 = CARTESIAN_POINT ( 'NONE',  ( 0.7499999999999885647, 1.347916667349485786, -1.299038105676652899 ) ) ;
#170662 = CARTESIAN_POINT ( 'NONE',  ( -7.230575994789712801, 7.330093503543126054, 0.7998128361456341429 ) ) ;
#170661 = CARTESIAN_POINT ( 'NONE',  ( -15.75000000000000000, 10.90000000000000036, -1.100000000000002087 ) ) ;
#170663 = CARTESIAN_POINT ( 'NONE',  ( 2.853255899669316697, 1.832232481769331844, -0.1808706098178694266 ) ) ;
#170664 = ORIENTED_EDGE ( 'NONE', *, *, #144905, .T. ) ;
#170665 = CARTESIAN_POINT ( 'NONE',  ( -8.784793466650835825, 12.33634391347959713, 1.199719254218462483 ) ) ;
#170666 = CARTESIAN_POINT ( 'NONE',  ( -1.451998047840359130, 7.315968950356099398, 4.301760722582896435 ) ) ;
#170667 = CARTESIAN_POINT ( 'NONE',  ( 4.588201236890728119, 1.223260742344203900, 1.732012071221388450 ) ) ;
#170668 = CARTESIAN_POINT ( 'NONE',  ( 0.1812672858593766811, -0.8707521589867758260, 1.622202602641155345 ) ) ;
#170669 = CARTESIAN_POINT ( 'NONE',  ( 0.7499999999999902300, 5.597916667349482900, -1.299038105676658228 ) ) ;
#170670 = CARTESIAN_POINT ( 'NONE',  ( 6.100279051144945619, 9.204410428722734849, -1.199719254218440723 ) ) ;
#170671 = CARTESIAN_POINT ( 'NONE',  ( 4.305972304023081954, -2.055534471369814487, 0.1475827967423407050 ) ) ;
#170673 = CARTESIAN_POINT ( 'NONE',  ( 1.241482983173985533, 1.839155304979672501, 0.08999620058360720265 ) ) ;
#170672 = CARTESIAN_POINT ( 'NONE',  ( -7.549192604710863286, 7.701812881784464437, -0.7998128361456291469 ) ) ;
#170674 = CARTESIAN_POINT ( 'NONE',  ( 1.364683531249992088, 5.384375000341417916, 1.214306433183764966E-14 ) ) ;
#170675 =( BOUNDED_SURFACE ( )  B_SPLINE_SURFACE ( 3, 2, ( 
 ( #23870, #89977, #156027 ),
 ( #7617, #140878, #73701 ),
 ( #189582, #41229, #165613 ),
 ( #61721, #131053, #64904 ) ),
 .UNSPECIFIED., .F., .F., .T. ) 
 B_SPLINE_SURFACE_WITH_KNOTS ( ( 4, 4 ),
 ( 3, 3 ),
 ( 0.000000000000000000, 9.170893477921754312E-05 ),
 ( 0.000000000000000000, 1.000000000000000000 ),
 .UNSPECIFIED. ) 
 GEOMETRIC_REPRESENTATION_ITEM ( )  RATIONAL_B_SPLINE_SURFACE ( (
 ( 1.000000000000000000, 0.6787756258918323793, 1.000000000000000000),
 ( 1.000000000000000000, 0.6894756946172844181, 1.000000000000000000),
 ( 1.000000000000000000, 0.6998898451712581847, 1.000000000000000000),
 ( 1.000000000000000000, 0.7100530722070644840, 1.000000000000000000) ) ) 
 REPRESENTATION_ITEM ( '' )  SURFACE ( )  );
#170676 = LINE ( 'NONE', #138199, #28730 ) ;
#170677 = FACE_OUTER_BOUND ( 'NONE', #35761, .T. ) ;
#170678 = CARTESIAN_POINT ( 'NONE',  ( 0.9442952520863318044, 0.8911936224933308948, -2.019119535841918278 ) ) ;
#170679 = CARTESIAN_POINT ( 'NONE',  ( 3.585499571845919942, 2.047054288528706412, -0.9635960562263863327 ) ) ;
#170680 = CARTESIAN_POINT ( 'NONE',  ( -7.754900677336769022, 9.110100880723427608, 1.082531754730558626 ) ) ;
#170681 = CARTESIAN_POINT ( 'NONE',  ( 3.761794061002172729, 0.6050747832711267371, -1.707706662339498749 ) ) ;
#170682 = CARTESIAN_POINT ( 'NONE',  ( 3.854619899909034419, -1.789536248510626315, -0.6842995647342240417 ) ) ;
#170683 = CARTESIAN_POINT ( 'NONE',  ( 5.090316257491098284, 1.067296284200716983, -1.773933887923849984 ) ) ;
#170684 = CARTESIAN_POINT ( 'NONE',  ( -1.001543065824772872E-14, 4.384375000341417916, 1.575800808251672791 ) ) ;
#170685 = CARTESIAN_POINT ( 'NONE',  ( 3.326987498081665162, 0.04702425985559504501, 1.971060134238045602 ) ) ;
#170686 = CARTESIAN_POINT ( 'NONE',  ( 1.518447027862340093, 1.295632655171574665, -1.425748867336932513 ) ) ;
#170687 = CARTESIAN_POINT ( 'NONE',  ( 3.590566789841375339, -0.3639703897368729568, -1.834726254853453087 ) ) ;
#170688 = CARTESIAN_POINT ( 'NONE',  ( 3.018547437338540806, -1.137872740210974287, -2.007595131770247843 ) ) ;
#170689 = CARTESIAN_POINT ( 'NONE',  ( 3.596024570820981037, 0.8385914878215626755, -1.661501840750801540 ) ) ;
#170690 = CARTESIAN_POINT ( 'NONE',  ( -0.6823417656249969321, 4.217708333674755394, -1.181850606188749264 ) ) ;
#170691 = DIRECTION ( 'NONE',  ( -1.000000000000000000, 4.984021416236792516E-16, 0.000000000000000000 ) ) ;
#170692 = CARTESIAN_POINT ( 'NONE',  ( 1.453890484719716492, 0.6100395758942640523, -2.015780296659912985 ) ) ;
#170693 = CARTESIAN_POINT ( 'NONE',  ( 2.507895228403643539, 5.869702166538802501, -0.7216878364870267237 ) ) ;
#170695 = CARTESIAN_POINT ( 'NONE',  ( -11.01135777277262129, 0.000000000000000000, 1.399999999999998579 ) ) ;
#170694 = DIRECTION ( 'NONE',  ( -1.000000000000000000, 0.000000000000000000, 0.000000000000000000 ) ) ;
#170696 = CARTESIAN_POINT ( 'NONE',  ( -1.896098101912877310, 8.993996023093842496, -0.7749999999999996891 ) ) ;
#170697 = CARTESIAN_POINT ( 'NONE',  ( 3.551138032611600437, 0.3147205237276836653, 2.097014573754731881 ) ) ;
#170698 = CARTESIAN_POINT ( 'NONE',  ( 5.763039058787653879, 7.049721345481424706, -2.500000000000000000 ) ) ;
#170700 = EDGE_CURVE ( 'NONE', #7066, #123166, #196665, .T. ) ;
#170699 = CARTESIAN_POINT ( 'NONE',  ( 0.8967469923133252196, -1.971478154887895684, -0.4383870506769834141 ) ) ;
#170701 = CARTESIAN_POINT ( 'NONE',  ( -0.6823417656250212460, 0.8010416670080899859, 1.181850606188755259 ) ) ;
#170702 = CARTESIAN_POINT ( 'NONE',  ( -4.338245966692955591, 5.124003718305597310, 1.082531754730560403 ) ) ;
#170703 = CARTESIAN_POINT ( 'NONE',  ( 5.066996723205273057, 6.934582148538044777, 1.599625672291267398 ) ) ;
#170704 = ORIENTED_EDGE ( 'NONE', *, *, #7456, .F. ) ;
#170705 = CARTESIAN_POINT ( 'NONE',  ( 1.142116303652768172, 0.8771353898661786719, -1.975824051420910221 ) ) ;
#170706 = CARTESIAN_POINT ( 'NONE',  ( 6.890000000000025437, 2.478461836817289043, 2.104748632312344103 ) ) ;
#170709 = CARTESIAN_POINT ( 'NONE',  ( 2.385871846325007706, 5.727341554113725586, -0.7216878364870267237 ) ) ;
#170708 = CARTESIAN_POINT ( 'NONE',  ( -2.020417662918760016, 3.956598013261175772, 11.36521191596583336 ) ) ;
#170707 = CARTESIAN_POINT ( 'NONE',  ( 4.929271367020211514, 7.908511140569038922, 1.199719254218452047 ) ) ;
#170710 = CARTESIAN_POINT ( 'NONE',  ( 9.151390499099949949, 12.66007743471656788, -1.082531754730543971 ) ) ;
#170711 = CARTESIAN_POINT ( 'NONE',  ( 6.087125082597877324, 1.679220375458953862, 1.116214469231976869 ) ) ;
#170712 = CARTESIAN_POINT ( 'NONE',  ( -6.710922849084449915, 10.77323439066645783, 0.000000000000000000 ) ) ;
#170713 = EDGE_CURVE ( 'NONE', #71097, #147625, #145694, .T. ) ;
#170714 = CARTESIAN_POINT ( 'NONE',  ( 6.321832389622432657, 1.203313566387714584, -1.709558936785739780 ) ) ;
#170715 = FACE_BOUND ( 'NONE', #27774, .T. ) ;
#170717 = CARTESIAN_POINT ( 'NONE',  ( -0.6823417656250039265, 12.56770833367473017, -1.181850606188755259 ) ) ;
#170716 = CARTESIAN_POINT ( 'NONE',  ( 6.631704542599726082, -1.407888343591977121, -1.640466528430361670 ) ) ;
#170718 = CARTESIAN_POINT ( 'NONE',  ( -9.158696461231359720, 10.64389961198009615, 1.199719254218462483 ) ) ;
#170719 = CARTESIAN_POINT ( 'NONE',  ( -4.867013957181525186, 8.622007350113015889, 0.7216878364870458196 ) ) ;
#170720 = CARTESIAN_POINT ( 'NONE',  ( 1.364683531249986537, 1.967708333674750731, -0.7879004041258239610 ) ) ;
#170721 = B_SPLINE_CURVE_WITH_KNOTS ( 'NONE', 3,
 ( #72358, #204480, #156849, #188249, #39890, #106000, #157919, #108154 ),
 .UNSPECIFIED., .F., .F.,
 ( 4, 2, 2, 4 ),
 ( 1.734723475976789761E-18, 0.0004365159022975801891, 0.0006547738534463698771, 0.0008730318045951596193 ),
 .UNSPECIFIED. ) ;
#170722 = CARTESIAN_POINT ( 'NONE',  ( 0.6311622855796304998, 3.199999999999987743, -0.4000000000000236144 ) ) ;
#170723 = CARTESIAN_POINT ( 'NONE',  ( 0.7500000000000006661, 9.916666666666671404, -1.299038105676657340 ) ) ;
#170724 = CARTESIAN_POINT ( 'NONE',  ( 2.894803161253765467, 1.479297447286776590, -0.8868043451095276586 ) ) ;
#170725 = CARTESIAN_POINT ( 'NONE',  ( 5.228604516725597229, 6.129068686715179126, -1.199719254218450271 ) ) ;
#170726 = CARTESIAN_POINT ( 'NONE',  ( 2.090717947541526289, 1.542569122296926221, -0.8672550169683733712 ) ) ;
#170727 = AXIS2_PLACEMENT_3D ( 'NONE', #153148, #207224, #108736 ) ;
#170728 = CARTESIAN_POINT ( 'NONE',  ( 5.491335294905154818, 1.948586811899848614, -1.035780281143129811 ) ) ;
#170729 = STYLED_ITEM ( 'NONE', ( #144626 ), #55927 ) ;
#170730 = EDGE_LOOP ( 'NONE', ( #166934, #178844, #128123, #64486, #21952 ) ) ;
#170731 = CARTESIAN_POINT ( 'NONE',  ( 4.201429114599513959, 1.802380596022877368, -0.9117778440167979559 ) ) ;
#170732 = CARTESIAN_POINT ( 'NONE',  ( -7.262327558775498737, 8.501745569106741840, 1.199719254218452047 ) ) ;
#170734 = CARTESIAN_POINT ( 'NONE',  ( 3.638296137631126914, 0.7283958097016438593, 1.880429543521966007 ) ) ;
#170733 = CARTESIAN_POINT ( 'NONE',  ( 4.213620120093874988, 1.703795446819071691, 1.262174061880352083 ) ) ;
#170736 = ORIENTED_EDGE ( 'NONE', *, *, #108972, .T. ) ;
#170735 = CARTESIAN_POINT ( 'NONE',  ( 4.025510356283497515, -0.3035946714039591265, 1.785781755087331391 ) ) ;
#170737 = CARTESIAN_POINT ( 'NONE',  ( 5.248941747146098180, 6.152795455539095570, -1.199719254218452047 ) ) ;
#170738 = ORIENTED_EDGE ( 'NONE', *, *, #100013, .F. ) ;
#170739 = CARTESIAN_POINT ( 'NONE',  ( 0.9009904985227291663, 1.526999960511504772, 1.080287613699250304 ) ) ;
#170740 = EDGE_CURVE ( 'NONE', #22081, #118779, #130611, .T. ) ;
#170742 = AXIS2_PLACEMENT_3D ( 'NONE', #87792, #54229, #43075 ) ;
#170741 = CARTESIAN_POINT ( 'NONE',  ( 2.460826785407678408, 8.202405370174465915, -2.499999999999995559 ) ) ;
#170743 = CARTESIAN_POINT ( 'NONE',  ( 6.639320575229251453, 0.008029245381881154262, 1.796863947021019481 ) ) ;
#170744 = CARTESIAN_POINT ( 'NONE',  ( -4.613852347352193739, 4.277249248199312071, 1.214306433183764966E-14 ) ) ;
#170745 = CARTESIAN_POINT ( 'NONE',  ( -10.37923916842784422, 4.890109552615133026, -5.358306740738790097 ) ) ;
#170746 = CARTESIAN_POINT ( 'NONE',  ( 1.499999999999990896, 4.056250000682819490, 1.214306433183764966E-14 ) ) ;
#170747 = CARTESIAN_POINT ( 'NONE',  ( -0.6823417656249969321, 3.530208333674754506, -1.181850606188749264 ) ) ;
#170748 = CARTESIAN_POINT ( 'NONE',  ( 0.03522015555855115276, -0.09184495783944729430, 1.910282976853895587 ) ) ;
#170749 = ORIENTED_EDGE ( 'NONE', *, *, #135163, .T. ) ;
#170750 = CARTESIAN_POINT ( 'NONE',  ( 7.688882512725796481, 8.142986817701137525, 0.000000000000000000 ) ) ;
#170751 = CARTESIAN_POINT ( 'NONE',  ( -3.472296738875691346, 6.104744391113324120, 1.082531754730549967 ) ) ;
#170752 = CARTESIAN_POINT ( 'NONE',  ( -4.450819567036169211, 8.414649604842665553, -0.7998128361456362523 ) ) ;
#170753 = CARTESIAN_POINT ( 'NONE',  ( 3.814780496183818315, -0.6684712460508880350, -2.012520831323429515 ) ) ;
#170754 = CARTESIAN_POINT ( 'NONE',  ( -10.99878419127389684, 6.872217442641685103, 3.961452310287494338 ) ) ;
#170755 = CARTESIAN_POINT ( 'NONE',  ( 5.905538618093676639, -0.4813517389176332206, 1.911553968036589390 ) ) ;
#170756 = CARTESIAN_POINT ( 'NONE',  ( -1.201851678989727383E-14, 1.571875000341420581, 1.575800808251672791 ) ) ;
#170757 = CARTESIAN_POINT ( 'NONE',  ( 0.8791531640492165067, -1.821740142837099174, -0.8571184184497283587 ) ) ;
#170758 = ORIENTED_EDGE ( 'NONE', *, *, #208798, .T. ) ;
#170759 = CARTESIAN_POINT ( 'NONE',  ( -0.1408020194050146334, -0.005144001661238749128, -2.100147592658160089 ) ) ;
#170760 = CARTESIAN_POINT ( 'NONE',  ( 11.08329605692676623, 7.955792042383879270, 4.620896497113651691 ) ) ;
#170761 = CARTESIAN_POINT ( 'NONE',  ( 1.539598694730393680, 1.913698299121506352, -0.7905179490511196061 ) ) ;
#170762 = ORIENTED_EDGE ( 'NONE', *, *, #59714, .T. ) ;
#170763 = CARTESIAN_POINT ( 'NONE',  ( 6.852720297064418986, 6.959538199522133262, 0.7998128361456331437 ) ) ;
#170764 = CARTESIAN_POINT ( 'NONE',  ( 6.062430963966053632, 7.101866208495718702, -1.199719254218452047 ) ) ;
#170765 = VERTEX_POINT ( 'NONE', #113291 ) ;
#170767 = CARTESIAN_POINT ( 'NONE',  ( 6.179819089730593795, 6.104210447640811665, 1.040834085586084257E-14 ) ) ;
#170766 = CARTESIAN_POINT ( 'NONE',  ( 4.523432754507224374, -1.286067535266706807, -1.648171318802932106 ) ) ;
#170770 = ORIENTED_EDGE ( 'NONE', *, *, #42883, .F. ) ;
#170769 = CARTESIAN_POINT ( 'NONE',  ( 1.805022944457121081, 1.575911691392884117, -0.8931387472532796856 ) ) ;
#170768 = CARTESIAN_POINT ( 'NONE',  ( 3.065264358586119009, 0.2694654384877669395, -1.805464241506696155 ) ) ;
#170771 = B_SPLINE_CURVE_WITH_KNOTS ( 'NONE', 3,
 ( #164050, #130547, #97992, #81716, #31914, #13509 ),
 .UNSPECIFIED., .F., .F.,
 ( 4, 2, 4 ),
 ( 0.000000000000000000, 0.0003172254002810696557, 0.0006344508005621393113 ),
 .UNSPECIFIED. ) ;
#170772 = CARTESIAN_POINT ( 'NONE',  ( 6.604147088760183415, -2.206502607372296421, 0.04933187264975073122 ) ) ;
#170773 = CARTESIAN_POINT ( 'NONE',  ( 3.768774344222697970, -1.483932802477351487, 1.633493490917396151 ) ) ;
#170774 = CARTESIAN_POINT ( 'NONE',  ( 6.096362627639171805, 10.26417349888772179, -0.7998128361456291469 ) ) ;
#170775 = CARTESIAN_POINT ( 'NONE',  ( 1.364683531249996529, 8.776041667008067648, 0.7879004041258403923 ) ) ;
#170776 = CARTESIAN_POINT ( 'NONE',  ( 3.246637215680724164, 1.866209232881730573, 0.4165188312477489663 ) ) ;
#170777 = CARTESIAN_POINT ( 'NONE',  ( 7.235247531187115833, 11.59287255302699648, -0.7998128361456291469 ) ) ;
#170778 = CARTESIAN_POINT ( 'NONE',  ( 6.689897370947560873, -1.349224794794257720, -1.570457413003906177 ) ) ;
#170779 = CARTESIAN_POINT ( 'NONE',  ( -9.356506676016417501, 15.43424542432546787, 7.432410969269082734 ) ) ;
#170780 = CARTESIAN_POINT ( 'NONE',  ( 5.741772062182810998, 2.188963553168365994, 0.1087695542012837302 ) ) ;
#170781 = CARTESIAN_POINT ( 'NONE',  ( 5.038060948978250408, 7.997685013099862239, -1.157798351953726490 ) ) ;
#170782 = CARTESIAN_POINT ( 'NONE',  ( -5.580126084947876208, 15.44693018518439054, -10.58314212524266296 ) ) ;
#170783 = VERTEX_POINT ( 'NONE', #81780 ) ;
#170784 = ORIENTED_EDGE ( 'NONE', *, *, #40036, .F. ) ;
#170785 = DIRECTION ( 'NONE',  ( -0.000000000000000000, -1.000000000000000000, -0.000000000000000000 ) ) ;
#170786 = CARTESIAN_POINT ( 'NONE',  ( 3.409304255485625657, -0.3681080166235695117, 1.833790788056933962 ) ) ;
#170787 = CARTESIAN_POINT ( 'NONE',  ( 3.285556943750000514, -1.451041666188708890, 1.896917185911906722 ) ) ;
#170788 = DIRECTION ( 'NONE',  ( 1.000000000000000000, 0.000000000000000000, -3.491481338843133355E-15 ) ) ;
#170789 = COLOUR_RGB ( '', 0.08235294, 0.09019608, 0.10196078) ;
#170790 = CARTESIAN_POINT ( 'NONE',  ( -8.514157279702036618, 9.035531035848267223, -0.7216878364870278340 ) ) ;
#170791 = CARTESIAN_POINT ( 'NONE',  ( 4.004454267989866700, 5.765225627445230927, 1.599625672291262513 ) ) ;
#170792 = CARTESIAN_POINT ( 'NONE',  ( 6.438344962566215024, -1.112565956905732456, 1.745730973219234539 ) ) ;
#170793 = CARTESIAN_POINT ( 'NONE',  ( 0.9664229901367871189, -1.967894173845800898, -0.4390061282484733485 ) ) ;
#170794 = VECTOR ( 'NONE', #167163, 1000.000000000000114 ) ;
#170795 = CARTESIAN_POINT ( 'NONE',  ( -8.136864746495904299, 12.64475930422059768, -0.7998128361456281477 ) ) ;
#170796 = CARTESIAN_POINT ( 'NONE',  ( 2.911969131885072670, 6.619324097166378706, 0.000000000000000000 ) ) ;
#170797 = PRESENTATION_STYLE_ASSIGNMENT (( #104749 ) ) ;
#170798 = B_SPLINE_CURVE_WITH_KNOTS ( 'NONE', 3,
 ( #196980, #214252, #130990, #98423, #146133, #65883, #50735, #198041, #47565, #164488, #31300, #82158, #115794, #178618, #213215, #195928, #162367, #66952, #1957, #81101, #48620, #166625, #129940, #149304, #96312, #114735, #150386, #194851, #163432, #17145, #84302, #180733, #32359, #33416, #148249, #133091, #13947, #112606, #147190, #18217, #132031, #49671, #97375, #199089, #15012, #179679, #181783, #116861, #34480, #99495, #68018, #165552, #30228, #80030, #212146, #63782, #117939, #151454, #186059, #119007, #20358, #155716, #72302, #7299, #103771, #71230, #203363, #87519, #201231, #3026, #69094, #183933, #102697, #169822, #101623, #105942, #52872, #5153, #152508, #187133, #188198, #202294, #53946, #120083, #4092, #138408, #89664, #153584, #37694, #137345, #21409, #122239, #135216, #85372, #38762, #55015, #121164, #35545, #86443, #104843, #170888, #70163, #184985, #167688, #22481, #134159, #19290, #36611, #88592, #168755, #136274, #154649, #6231, #204427, #56082, #200167, #39834, #51821, #171966, #23557, #175182, #123309, #41986, #43056, #40912, #45185, #140569, #158916, #91805, #126495, #127575, #206581, #109169, #143777, #108095, #174124, #60334, #24625, #192458, #8381, #90732, #61412, #74464, #156795, #44112, #59268, #191390, #189273, #25697, #193543, #157863, #58210, #176241, #161048, #124369, #77655, #9456, #73377, #11583, #75528, #111299, #26768, #92870, #190327, #95002, #205511, #141639, #10512, #207648, #209772, #57142, #177303, #110233, #76586, #107018, #125424, #142697, #208707, #27843, #93940, #159981, #139482, #28917, #173042, #195683, #31060, #63545, #196743, #128636, #132839, #214016, #114496, #181543, #163189, #64609, #62474, #198843, #162123, #115547, #194602, #97136, #98196, #78714, #14773, #131786, #625, #148005, #80864, #129701, #149049, #50490, #180493, #130749, #211908, #49427, #197790, #48383, #47320, #33170, #113433, #13712, #146954, #144842, #99252, #66692, #210848, #32111, #145898, #116611, #46246, #165300, #82976, #179440, #182604, #212969, #164244, #15832, #81918, #16895, #34228, #65638, #79785, #178376, #100301, #12644, #96070, #112363, #29985, #204161, #37429, #167440, #117689, #86186, #186873, #22214, #51564, #185796, #170628, #88327, #134960, #166367, #102430, #154391, #168499, #20098, #199917, #169566, #19032, #5969, #85112, #72039, #138152, #151198, #69901, #103506, #120900, #55816, #121972, #184728, #187937, #4892, #183681, #21148, #39567, #87252, #2769, #136012, #68840, #202025, #153317, #150133, #36352, #200968, #133911, #38505, #17958, #52615, #152255, #84045, #118744, #3828, #67760, #53685, #1706, #35286, #119816, #203105, #101362, #70970, #137080, #54750, #104583, #205245, #171696, #105669, #73114, #23295, #56886, #155454, #7037, #139214, #123061, #189015, #89405, #179575, #96207, #66838, #147086, #113571, #162258, #1850, #31194, #33305, #213108, #178507, #30118, #112497, #79921, #67911, #198984, #134056, #46378, #97269, #13845, #65774, #64740, #148146, #196877, #163324, #146029, #132982, #130883, #14904, #212038, #63681, #80998, #99390, #48514, #129835, #195817, #47456, #114634, #180627, #32250, #98320, #164385, #15969, #82053, #131922, #214148, #197932, #50628, #34371, #49559, #115685, #181678, #166516, #165442, #116754, #182753, #17039, #83116, #149197, #100445, #772, #18107, #84194 ),
 .UNSPECIFIED., .F., .F.,
 ( 4, 1, 1, 1, 1, 1, 1, 1, 1, 1, 1, 1, 1, 1, 1, 1, 1, 1, 1, 1, 1, 1, 1, 1, 1, 1, 1, 1, 1, 1, 1, 1, 1, 1, 1, 1, 1, 1, 1, 1, 1, 1, 1, 1, 1, 1, 1, 1, 1, 1, 1, 1, 1, 1, 1, 1, 1, 1, 1, 1, 1, 1, 1, 1, 1, 1, 1, 1, 1, 1, 1, 1, 1, 1, 1, 1, 1, 1, 1, 1, 1, 1, 1, 1, 1, 1, 1, 1, 1, 1, 1, 1, 1, 1, 1, 1, 1, 1, 1, 1, 1, 1, 1, 1, 1, 1, 1, 1, 1, 1, 1, 1, 1, 1, 1, 1, 1, 1, 1, 1, 1, 1, 1, 1, 1, 1, 1, 1, 1, 1, 1, 1, 1, 1, 1, 1, 1, 1, 1, 1, 1, 1, 1, 1, 1, 1, 1, 1, 1, 1, 1, 1, 1, 1, 1, 1, 1, 1, 1, 1, 1, 1, 1, 1, 1, 1, 1, 1, 1, 1, 1, 1, 1, 1, 1, 1, 1, 1, 1, 1, 1, 1, 1, 1, 1, 1, 1, 1, 1, 1, 1, 1, 1, 1, 1, 1, 1, 1, 1, 1, 1, 1, 1, 1, 1, 1, 1, 1, 1, 1, 1, 1, 1, 1, 1, 1, 1, 1, 1, 1, 1, 1, 1, 1, 1, 1, 1, 1, 1, 1, 1, 1, 1, 1, 1, 1, 1, 1, 1, 1, 1, 1, 1, 1, 1, 1, 1, 1, 1, 1, 1, 1, 1, 1, 1, 1, 1, 1, 1, 1, 1, 1, 1, 1, 1, 1, 1, 1, 1, 1, 1, 1, 1, 1, 1, 1, 1, 1, 1, 1, 1, 1, 1, 1, 1, 1, 1, 1, 1, 1, 1, 1, 1, 1, 1, 1, 1, 1, 1, 1, 1, 1, 1, 1, 1, 1, 1, 1, 1, 1, 1, 1, 1, 1, 1, 1, 1, 1, 1, 1, 1, 1, 1, 1, 1, 1, 1, 1, 1, 1, 1, 1, 1, 1, 1, 1, 1, 1, 1, 1, 1, 1, 1, 1, 1, 1, 1, 1, 1, 1, 1, 1, 1, 1, 1, 1, 1, 1, 1, 1, 1, 1, 1, 1, 1, 1, 1, 1, 1, 1, 1, 1, 1, 1, 1, 1, 1, 1, 1, 1, 1, 1, 1, 1, 4 ),
 ( 0.000000000000000000, 0.002600209826155936224, 0.005208878553436857226, 0.007813350965615119270, 0.01041570154746907992, 0.01302155883015148306, 0.01562460066207539862, 0.01822947720112986364, 0.02083337797298438765, 0.02343721533725894035, 0.02604213897589890969, 0.02864525980212044229, 0.03125073504456635232, 0.03385369766904555017, 0.03645898980682723417, 0.03906240375024701977, 0.04166680464497042602, 0.04427120869897264999, 0.04687461886132015393, 0.04947991130494613921, 0.05208287402783655373, 0.05468834688957619622, 0.05729146186993632622, 0.05989639238693608009, 0.06250023923939096449, 0.06510408216679804128, 0.06770901469741306966, 0.07031212675311915294, 0.07291759917081726272, 0.07552056149378454097, 0.07812585104223603027, 0.08072926279340975064, 0.08333366149866272554, 0.08593806365491549193, 0.08854147146176674643, 0.09114676191340240208, 0.09374972248801059782, 0.09635519323906190092, 0.09895830628708340848, 0.1015632345865536273, 0.1041670796237980645, 0.1067709202568039306, 0.1093758509056654005, 0.1119789607794838548, 0.1145844312107493490, 0.1171873915655986947, 0.1197926790194954738, 0.1223960889855860712, 0.1250004854864837645, 0.1276048858798866925, 0.1302082914968497596, 0.1328135800830011481, 0.1354165386474412147, 0.1380220074263333041, 0.1406251186789811980, 0.1432300448973659046, 0.1458338882574615747, 0.1484377267335943440, 0.1510426556371624596, 0.1536457634674935069, 0.1562512320483212536, 0.1588541905735017246, 0.1614594760690261366, 0.1640628843880489185, 0.1666672788216651824, 0.1692716775892487424, 0.1718750811543677814, 0.1744803680111783883, 0.1770833247038955116, 0.1796887916465979840, 0.1822919012421508056, 0.1848968255159594287, 0.1875006673364670307, 0.1901045037933276616, 0.1927094310880738681, 0.1953125370132051675, 0.1979180038795354257, 0.2005209607134520455, 0.2031262443867272172, 0.2057296511966431873, 0.2083340436999963075, 0.2109384409787386505, 0.2135418426300015604, 0.2161471278935624962, 0.2187500828529475860, 0.2213555480953768861, 0.2239586561720615654, 0.2265635786377499516, 0.2291674190561798496, 0.2317712536313151217, 0.2343761794536610432, 0.2369792836118274071, 0.2395847488995502261, 0.2421877041805577391, 0.2447929861676560459, 0.2473963916063780244, 0.2500007823164346887, 0.2526051782432667259, 0.2552085781186103075, 0.2578138619249652486, 0.2604168152893601151, 0.2630222789673848927, 0.2656253856633817301, 0.2682303064573571261, 0.2708341456111751366, 0.2734379784420828963, 0.2760429029284052760, 0.2786460054577940548, 0.2812514693027542978, 0.2838544231691620401, 0.2864597036061101165, 0.2890631078115080133, 0.2916674968651886135, 0.2942718915769991783, 0.2968752898143142138, 0.2994805722994643427, 0.3020835242071668869, 0.3046889864566129091, 0.3072920919100609050, 0.3098970111686871198, 0.3125008491953192857, 0.3151046804194536644, 0.3177096037060897493, 0.3203127047448455222, 0.3229181672828482230, 0.3255211198729257016, 0.3281263988957095479, 0.3307298020056156362, 0.3333341895397992083, 0.3359385831734401084, 0.3385419799105768290, 0.3411472612104861635, 0.3437502117997557338, 0.3463556727564109927, 0.3489587771054129539, 0.3515636949650152721, 0.3541675320018531359, 0.3567713617566292128, 0.3593762839798815834, 0.3619793836661120978, 0.3645848450329270407, 0.3671877964849088460, 0.3697930742294792128, 0.3723964763816929868, 0.3750008625332226786, 0.3776052552255140804, 0.3802086506002868016, 0.3828139308508870520, 0.3854168802599494681, 0.3880223400595693151, 0.3906254434421968513, 0.3932303600390676390, 0.3958341962234732669, 0.3984380246462727593, 0.4010429459424146859, 0.4036460444141952153, 0.4062515047455624306, 0.4088544551976535102, 0.4114597317999305615, 0.4140631331322238151, 0.4166675180379114662, 0.4192719099256467796, 0.4218753040758395079, 0.4244805834130354061, 0.4270835317800880659, 0.4296889905584002634, 0.4322920931126992272, 0.4348970085831024290, 0.4375008440524135733, 0.4401046712805898320, 0.4427095917858701601, 0.4453126891812490551, 0.4479181486128839262, 0.4505210982032648026, 0.4531263737991432228, 0.4557297744492659897, 0.4583341582458977381, 0.4609385494658484461, 0.4635419425292200413, 0.4661472210888942258, 0.4687501685521111572, 0.4713556264448209299, 0.4739587283088163017, 0.4765636427889929916, 0.4791674776805284197, 0.4817713038514113699, 0.4843762237020596273, 0.4869793201590638665, 0.4895847788266616818, 0.4921877276934932821, 0.4947930024188478271, 0.4973964025245324327, 0.5000007853488734888, 0.5026051760377950872, 0.5052085681520839255, 0.5078138460701020485, 0.5104167927676396266, 0.5130222499104345468, 0.5156253512221359303, 0.5182302648483090302, 0.5208340992993732987, 0.5234379245502747136, 0.5260428438825063280, 0.5286459395391455152, 0.5312513975783873521, 0.5338543458598166147, 0.5364596198505067193, 0.5390630195494738874, 0.5416674015382738627, 0.5442717918329101900, 0.5468751831358398263, 0.5494804605480556603, 0.5520834066180569932, 0.5546888631466128095, 0.5572919640440190392, 0.5598968769523987588, 0.5625007111002878757, 0.5651045355685063720, 0.5677094545185276120, 0.5703125495128006373, 0.5729180070593572482, 0.5755209548935220631, 0.5781262282853970591, 0.5807296277153600750, 0.5833340090053582561, 0.5859383990424469335, 0.5885417896717308750, 0.5911470667139914204, 0.5937500122945923442, 0.5963554683445766447, 0.5989585689656815592, 0.6015634812924701702, 0.6041673152744758690, 0.6067711390973024033, 0.6093760578013157625, 0.6119791522712144660, 0.6145846094607528842, 0.6171875569857874222, 0.6197928299146914233, 0.6223962292133623508, 0.6250006099412922511, 0.6276049998575695676, 0.6302083899509167697, 0.6328136667590675835, 0.6354166119884008257, 0.6380220676954796444, 0.6406251681782773044, 0.6432300800596744139, 0.6458339140130902045, 0.6484377373278128465, 0.6510426559220214848, 0.6536457500055372627, 0.6562512069737248543, 0.6588541543277639523, 0.6614594269295416273, 0.6640628262346358612, 0.6666672065372305500, 0.6692715964694370134, 0.6718749861645568755, 0.6744802628744462902, 0.6770832078906477980, 0.6796886633904898334, 0.6822917638729786294, 0.6848966754451861760, 0.6875005095073121186, 0.6901043324512210475, 0.6927092510718347862, 0.6953123449069624762, 0.6979178017894718256, 0.7005207491106575368, 0.7031260215211581066, 0.7057294209703992571, 0.7083338009843969107, 0.7109381910692819107, 0.7135415805038890502, 0.7161468572513741693, 0.7187498021925872171, 0.7213552576208688283, 0.7239583582410578089, 0.7265632696402853918, 0.7291671039484327599, 0.7317709266588259265, 0.7343758454420658000, 0.7369789391668094547, 0.7395843960993241373, 0.7421873435258099505, 0.7447926158808931829, 0.7473960156120186271, 0.7500003954741673029, 0.7526047858484943287, 0.7552081751603144655, 0.7578134520812660480, 0.7604163970856469001, 0.7630218525780576577, 0.7656249534739711926, 0.7682298648364407345, 0.7708336995279378989, 0.7734375221421257995, 0.7760424412242287184, 0.7786455349766069345, 0.7812509920948264019, 0.7838539397647821261, 0.7864592122003229990, 0.7890626123510894319, 0.7916669921981516200, 0.7942713829987035901, 0.7968747723254782089, 0.7994800495557851105, 0.8020829947615083499, 0.8046884504537559213, 0.8072915517634385862, 0.8098964632253897733, 0.8125002984375870874, 0.8151041210928977598, 0.8177090406101226172, 0.8203121345281733090, 0.8229175919678175521, 0.8255205400194353116, 0.8281258126713292311, 0.8307292133795166622, 0.8333335933482756142, 0.8359379847118599827, 0.8385413741913512187, 0.8411466518669262760, 0.8437495974121898001, 0.8463550534400045011, 0.8489581553015269622, 0.8515630669992224622, 0.8541669028694969246, 0.8567707257032814994, 0.8593756457919137226, 0.8619787400136992295, 0.8645841979105142183, 0.8671871464820134490, 0.8697924194861808012, 0.8723958208895988831, 0.8750002011168627192, 0.8776045931803160283, 0.8802079829503125508, 0.8828132612070975771, 0.8854162072301272612, 0.8880216637292678294, 0.8906247662807315058, 0.8932296783504612980, 0.8958335150162225480, 0.8984373381658604663, 0.9010422589622166800, 0.9036453536258294283, 0.9062508121155921081, 0.9088537613452241093, 0.9114590348376164775, 0.9140624370741091687, 0.9166668176967164294, 0.9192712105969091940, 0.9218746007952320909, 0.9244798797692056480, 0.9270828264082496828, 0.9296882835145078294, 0.9322913868941045124, 0.9348962994721256026, 0.9375001370706889103, 0.9401039606740361210, 0.9427088823143441321, 0.9453119775565693717, 0.9479174367776000976, 0.9505203868030935865, 0.9531256609099927335, 0.9557290641454977420, 0.9583334452981105978, 0.9609378390199675435, 0.9635412300619400350, 0.9661465102466426647, 0.9687494557931184413, 0.9713549143510965544, 0.9739580252604012056, 0.9765629275426017664, 0.9791667581373608709, 0.9817706348486141543, 0.9843755007711335603, 0.9869785191422796311, 0.9895843624858681187, 0.9921867025132995455, 0.9947911529560371502, 0.9973998138561904758, 1.000000000000000000 ),
 .UNSPECIFIED. ) ;
#170799 = CARTESIAN_POINT ( 'NONE',  ( 1.289316216709124996, 1.661312375189183399, 1.429258102917586815 ) ) ;
#170800 = CARTESIAN_POINT ( 'NONE',  ( 4.670415550810885996, -1.190324863180821646, 1.384379922071424351 ) ) ;
#170801 = CARTESIAN_POINT ( 'NONE',  ( -3.924195396151603177, 6.665646164563756138, 1.199719254218464037 ) ) ;
#170802 = CARTESIAN_POINT ( 'NONE',  ( 4.719646871332936477, 8.520355426614829142, -0.7216878364870357165 ) ) ;
#170803 = CARTESIAN_POINT ( 'NONE',  ( 3.728129053633592704, 4.412200653069714207, -1.082531754730543083 ) ) ;
#170804 = CARTESIAN_POINT ( 'NONE',  ( -6.642568916052639771, 6.714361588341672515, 0.000000000000000000 ) ) ;
#170805 = CARTESIAN_POINT ( 'NONE',  ( 2.869522067586683711, 6.499526178826442013, 0.7998128361456362523 ) ) ;
#170806 = CARTESIAN_POINT ( 'NONE',  ( 4.228163802615382494, 6.026220084508304708, -1.599625672291269396 ) ) ;
#170807 = ORIENTED_EDGE ( 'NONE', *, *, #183332, .T. ) ;
#170809 = CARTESIAN_POINT ( 'NONE',  ( 5.924093355334532518, -1.997480882691978987, 0.2508417921044738819 ) ) ;
#170808 = CARTESIAN_POINT ( 'NONE',  ( 3.878315922200573862, -0.1843894689829879696, -1.832007427040844183 ) ) ;
#170810 = CARTESIAN_POINT ( 'NONE',  ( 1.617049182541079544, 0.6662764605713987764, -2.199669867806148371 ) ) ;
#170812 = CARTESIAN_POINT ( 'NONE',  ( 6.965691013979927959, -0.4331334938386353084, 1.920344510276907890 ) ) ;
#170811 = CARTESIAN_POINT ( 'NONE',  ( 4.202664430556254160, 5.926194473780837413, 1.443375672974062551 ) ) ;
#170813 = CARTESIAN_POINT ( 'NONE',  ( -4.446184310277715213, 7.274633231044262516, -1.199719254218452047 ) ) ;
#170814 = CARTESIAN_POINT ( 'NONE',  ( 4.787437623848783907, 6.678706240755900581, -1.249999999999999334 ) ) ;
#170815 = CARTESIAN_POINT ( 'NONE',  ( 3.673993457511487204, 1.897360377298975553, -0.2389773157873422427 ) ) ;
#170816 = CARTESIAN_POINT ( 'NONE',  ( -10.47097470845587175, 11.11055866948701443, 1.040834085586084257E-14 ) ) ;
#170817 = CARTESIAN_POINT ( 'NONE',  ( 6.438112759045284683, 6.782534085545247393, 0.3978009605737874432 ) ) ;
#170818 = CARTESIAN_POINT ( 'NONE',  ( -7.770231434407805615, 8.237893892996801526, 0.000000000000000000 ) ) ;
#170820 = CARTESIAN_POINT ( 'NONE',  ( 1.692057038649401601, -1.861345348035767344, -0.1864469194169729449 ) ) ;
#170819 = CARTESIAN_POINT ( 'NONE',  ( 2.894169963053084160, -0.6095376172369629808, -1.999899515593931199 ) ) ;
#170821 = CARTESIAN_POINT ( 'NONE',  ( 2.249374845261054467, -1.976652949091894707, -0.3960421909960794018 ) ) ;
#170822 = CARTESIAN_POINT ( 'NONE',  ( 7.429504990608736037, 11.61158022244479682, -0.7216878364870267237 ) ) ;
#170823 = CARTESIAN_POINT ( 'NONE',  ( 1.364683531249990311, 4.196875000341417028, 1.214306433183764966E-14 ) ) ;
#170824 = CARTESIAN_POINT ( 'NONE',  ( 3.596946774904510757, -0.5014486528964605672, 1.666646126512297821 ) ) ;
#170825 = CARTESIAN_POINT ( 'NONE',  ( 3.659811400685081040, 6.357198169852855685, -1.199719254218446718 ) ) ;
#170826 = DIRECTION ( 'NONE',  ( 0.000000000000000000, 0.000000000000000000, 1.000000000000000000 ) ) ;
#170827 = CARTESIAN_POINT ( 'NONE',  ( 3.932037377198682737, 0.9205326289291086983, -1.458499330894097668 ) ) ;
#170828 = CARTESIAN_POINT ( 'NONE',  ( 3.333693798916517625, 0.9835563995168915552, -1.958507884819527867 ) ) ;
#170829 = CARTESIAN_POINT ( 'NONE',  ( 6.691986956589398794, -0.9478133180038283978, 1.990996264204819122 ) ) ;
#170830 = CARTESIAN_POINT ( 'NONE',  ( -11.66942904513850543, 4.336835040752899495, -5.185078083676367910 ) ) ;
#170831 = CARTESIAN_POINT ( 'NONE',  ( 4.118177926953592305, 2.155335829443456142, -0.2601999948229383741 ) ) ;
#170832 = CARTESIAN_POINT ( 'NONE',  ( 1.699542765152612711, -0.6164703606487754728, 1.718597393154073671 ) ) ;
#170833 = DIRECTION ( 'NONE',  ( -8.881784197001252323E-16, 0.000000000000000000, 1.000000000000000000 ) ) ;
#170834 = CARTESIAN_POINT ( 'NONE',  ( 4.733676700703519202, 0.6609272643324247687, -2.011644693266708916 ) ) ;
#170835 = CARTESIAN_POINT ( 'NONE',  ( 6.539320575229251808, 0.004279804010676873348, 1.996977849922920267 ) ) ;
#170836 = EDGE_LOOP ( 'NONE', ( #49925, #191678, #173728, #91417 ) ) ;
#170838 = CARTESIAN_POINT ( 'NONE',  ( 1.364683531249988757, 2.196875000341415252, 1.214306433183764966E-14 ) ) ;
#170837 = CARTESIAN_POINT ( 'NONE',  ( 4.845436733290686249, 0.7204735554154987343, -2.176297985750157427 ) ) ;
#170839 = CARTESIAN_POINT ( 'NONE',  ( 6.720655732516610747, 3.700489942686377098, 2.440724243369211788 ) ) ;
#170840 = CARTESIAN_POINT ( 'NONE',  ( 9.890836756369282057, 11.49806328964105617, -1.199719254218440723 ) ) ;
#170841 = EDGE_CURVE ( 'NONE', #193389, #94238, #47095, .T. ) ;
#170842 = CARTESIAN_POINT ( 'NONE',  ( 0.6805317496583452863, 1.048634805427307359, 1.842989218901350812 ) ) ;
#170843 = CARTESIAN_POINT ( 'NONE',  ( -6.127922243696855453, 7.211959374810172463, 1.082531754730549967 ) ) ;
#170844 = CARTESIAN_POINT ( 'NONE',  ( 2.738383840280328663, 5.178236332760252303, 1.082531754730548412 ) ) ;
#170845 = CARTESIAN_POINT ( 'NONE',  ( -5.219525951136845698, 8.072902128759544382, -1.082531754730543971 ) ) ;
#170846 = CARTESIAN_POINT ( 'NONE',  ( -10.91877484692252942, -9.999999999999991118, 0.1449562030364423548 ) ) ;
#170847 = VERTEX_POINT ( 'NONE', #213879 ) ;
#170848 = CARTESIAN_POINT ( 'NONE',  ( 4.852185490356213826, 0.1948433276699329531, -2.006959737079899497 ) ) ;
#170850 = CARTESIAN_POINT ( 'NONE',  ( 2.764570516439817549, -0.7852151221510113022, -1.907448154738192514 ) ) ;
#170849 = CARTESIAN_POINT ( 'NONE',  ( 5.983225862332436584, 5.874851682342960402, 0.7998128361456341429 ) ) ;
#170852 = CARTESIAN_POINT ( 'NONE',  ( -0.2411972340276230808, 7.629137130509075604, -2.500476664557866435 ) ) ;
#170851 = CARTESIAN_POINT ( 'NONE',  ( 1.347111479062088405E-15, 6.999999999999999112, 11.00000000000000000 ) ) ;
#170853 = CARTESIAN_POINT ( 'NONE',  ( 5.525830126021535449, 8.604496359403894346, -1.199719254218452047 ) ) ;
#170854 = CARTESIAN_POINT ( 'NONE',  ( 1.001543065824772753E-15, -0.3718749995220430038, 3.793834371823811669 ) ) ;
#170855 = CYLINDRICAL_SURFACE ( 'NONE', #68301, 0.3999999999999996891 ) ;
#170856 = CARTESIAN_POINT ( 'NONE',  ( 5.771465802492605768, 1.302860414194568550, 1.761948869136241047 ) ) ;
#170857 = CARTESIAN_POINT ( 'NONE',  ( 3.920546200773936896, -1.392545040883992336, -1.458557299768625581 ) ) ;
#170858 = CARTESIAN_POINT ( 'NONE',  ( 3.614658571667620279, -0.1319153736358945894, 1.836568937333193485 ) ) ;
#170859 = CARTESIAN_POINT ( 'NONE',  ( 4.821896187954575197, 8.777295985922343391, 0.7998128361456462443 ) ) ;
#170860 = CARTESIAN_POINT ( 'NONE',  ( 2.218750000000001332, -0.7852924748298697466, 1.895863743164134974 ) ) ;
#170861 = CARTESIAN_POINT ( 'NONE',  ( 1.148929321228649991, -1.355925326379325391, -1.065857193176344309 ) ) ;
#170862 = CARTESIAN_POINT ( 'NONE',  ( -4.302014814237876017, 3.913438792899272212, 0.7998128361456341429 ) ) ;
#170863 =( BOUNDED_SURFACE ( )  B_SPLINE_SURFACE ( 3, 3, ( 
 ( #127605, #111329, #179468, #177332, #28946, #191422, #13742, #95030, #161080, #141671 ),
 ( #194634, #31093, #79815, #12670, #126528, #62501, #97165, #144869, #210876, #128666 ),
 ( #46276, #112392, #207682, #59302, #43088, #10542, #109201, #26796, #92901, #158947 ),
 ( #142729, #148032, #213000, #199949, #36388, #102466, #67792, #115575, #214042, #181571 ),
 ( #130776, #15864, #16924, #14802, #65668, #48414, #196771, #81949, #183710, #101396 ),
 ( #80893, #50519, #131816, #134992, #146983, #167470, #85144, #197825, #201002, #83004 ),
 ( #149080, #99283, #19066, #64637, #658, #165331, #49457, #66725, #2800, #164274 ) ),
 .UNSPECIFIED., .T., .F., .T. ) 
 B_SPLINE_SURFACE_WITH_KNOTS ( ( 4, 3, 4 ),
 ( 4, 1, 1, 1, 1, 1, 1, 4 ),
 ( 0.000000000000000000, 0.5000000000000000000, 1.000000000000000000 ),
 ( 0.000000000000000000, 0.09790276019723312406, 0.1918320694002237370, 0.2608036337010187777, 0.3626611837559554630, 0.5214803378330250538, 0.7337833476510040587, 1.000000000000000000 ),
 .UNSPECIFIED. ) 
 GEOMETRIC_REPRESENTATION_ITEM ( )  RATIONAL_B_SPLINE_SURFACE ( (
 ( 1.000000000000000444, 1.000000000000000444, 1.000000000000000000, 1.000000000000000444, 1.000000000000000222, 1.000000000000000222, 1.000000000000000444, 1.000000000000000000, 1.000000000000000222, 1.000000000000000222),
 ( 0.3333333333333334814, 0.3333333333333334814, 0.3333333333333334814, 0.3333333333333334259, 0.3333333333333333703, 0.3333333333333334259, 0.3333333333333335369, 0.3333333333333333703, 0.3333333333333334259, 0.3333333333333334259),
 ( 0.3333333333333334814, 0.3333333333333334814, 0.3333333333333334814, 0.3333333333333334259, 0.3333333333333333703, 0.3333333333333334259, 0.3333333333333335369, 0.3333333333333333703, 0.3333333333333334259, 0.3333333333333334259),
 ( 1.000000000000000444, 1.000000000000000444, 1.000000000000000000, 1.000000000000000444, 1.000000000000000222, 1.000000000000000222, 1.000000000000000444, 1.000000000000000000, 1.000000000000000222, 1.000000000000000222),
 ( 0.3333333333333334814, 0.3333333333333334814, 0.3333333333333334814, 0.3333333333333334259, 0.3333333333333333703, 0.3333333333333334259, 0.3333333333333335369, 0.3333333333333333703, 0.3333333333333334259, 0.3333333333333334259),
 ( 0.3333333333333334814, 0.3333333333333334814, 0.3333333333333334814, 0.3333333333333334259, 0.3333333333333333703, 0.3333333333333334259, 0.3333333333333335369, 0.3333333333333333703, 0.3333333333333334259, 0.3333333333333334259),
 ( 1.000000000000000444, 1.000000000000000444, 1.000000000000000000, 1.000000000000000444, 1.000000000000000222, 1.000000000000000222, 1.000000000000000444, 1.000000000000000000, 1.000000000000000222, 1.000000000000000222) ) ) 
 REPRESENTATION_ITEM ( '' )  SURFACE ( )  );
#170864 = CARTESIAN_POINT ( 'NONE',  ( 0.9151166212276349299, -1.463470719828030120, -1.772635753884302057 ) ) ;
#170865 = CARTESIAN_POINT ( 'NONE',  ( -5.391338639728555648, 9.441645512991978961, -0.7998128361456231517 ) ) ;
#170866 = CARTESIAN_POINT ( 'NONE',  ( 0.4568015506021270156, 0.8674211623492070755, 2.089700042804636837 ) ) ;
#170867 = CARTESIAN_POINT ( 'NONE',  ( 2.737057789242686390, 0.2582918889518608374, 2.090101187703028884 ) ) ;
#170868 = CARTESIAN_POINT ( 'NONE',  ( -5.041653019435350380, 6.975290837464928728, -1.599625672291271394 ) ) ;
#170869 = CARTESIAN_POINT ( 'NONE',  ( 7.938462636001388795, 9.220293482545153907, -1.199719254218441611 ) ) ;
#170870 = CARTESIAN_POINT ( 'NONE',  ( 4.678972410047582464, 8.472901888448573615, -0.7216878364870357165 ) ) ;
#170871 = CARTESIAN_POINT ( 'NONE',  ( -5.442708600882160574, 8.437244903416123876, -1.199719254218446718 ) ) ;
#170872 = CARTESIAN_POINT ( 'NONE',  ( 7.605760987142057061, 7.975735361194951523, -0.7216878364870267237 ) ) ;
#170873 = CARTESIAN_POINT ( 'NONE',  ( 4.344452866495080556, 7.409550296852231099, 1.129427019999120985 ) ) ;
#170874 = CARTESIAN_POINT ( 'NONE',  ( -5.168682875307782254, 7.053215992657626110, -1.599625672291256295 ) ) ;
#170875 = CARTESIAN_POINT ( 'NONE',  ( 4.043395766388809598, 0.1113883285390921962, 2.218758960698932192 ) ) ;
#170876 = CARTESIAN_POINT ( 'NONE',  ( 2.800927341068761844, 1.851789894747071008, 1.171597702228709181 ) ) ;
#170877 = CARTESIAN_POINT ( 'NONE',  ( -7.237355071596549116, 7.338002426484427687, 1.040834085586084257E-14 ) ) ;
#170878 = CARTESIAN_POINT ( 'NONE',  ( -5.309953438407606363, 6.223975762010839574, 1.199719254218452935 ) ) ;
#170879 = CARTESIAN_POINT ( 'NONE',  ( 5.160583804383015227, -0.6592509027269661814, -1.847929681152965520 ) ) ;
#170880 = CARTESIAN_POINT ( 'NONE',  ( -1.364683531250000748, 1.509375000341421691, 0.000000000000000000 ) ) ;
#170881 = CARTESIAN_POINT ( 'NONE',  ( -3.363831509966360489, 6.938570838353784076, -0.7216878364870458196 ) ) ;
#170882 = CARTESIAN_POINT ( 'NONE',  ( -6.561783159334141580, 7.718130443053708767, -1.082531754730544860 ) ) ;
#170883 = CARTESIAN_POINT ( 'NONE',  ( 4.430007776716601953, -2.079114408633813582, 0.4165480963118637914 ) ) ;
#170884 = CARTESIAN_POINT ( 'NONE',  ( -4.496464221587651799, 5.274905009054215554, 1.199719254218452935 ) ) ;
#170885 = VERTEX_POINT ( 'NONE', #67620 ) ;
#170886 = CARTESIAN_POINT ( 'NONE',  ( 6.016527291255574283, 1.455332790597754000, -1.598591904487467463 ) ) ;
#170887 = CARTESIAN_POINT ( 'NONE',  ( 5.361359679200154105, 8.342337828120466980, 1.199719254218462483 ) ) ;
#170888 = CARTESIAN_POINT ( 'NONE',  ( 4.880324068823122197, -0.2306306682541107433, -1.826696389425507938 ) ) ;
#170889 = B_SPLINE_CURVE_WITH_KNOTS ( 'NONE', 3,
 ( #124613, #28085, #159152, #94181 ),
 .UNSPECIFIED., .F., .F.,
 ( 4, 4 ),
 ( 0.003642155973307022437, 0.004387807266393894436 ),
 .UNSPECIFIED. ) ;
#170890 = CARTESIAN_POINT ( 'NONE',  ( -5.897748123441601820, 6.008673066555767051, -0.2037434952626964724 ) ) ;
#170891 = CARTESIAN_POINT ( 'NONE',  ( -1.364683531250014514, 1.301041667008083325, -0.7879004041258289570 ) ) ;
#170892 = CARTESIAN_POINT ( 'NONE',  ( 0.4150587399484934603, -0.9287321991380654840, -1.471733822881353015 ) ) ;
#170893 = CARTESIAN_POINT ( 'NONE',  ( 6.827182134110246103, 6.039869998172250121, 2.305852349323509021 ) ) ;
#170894 = CARTESIAN_POINT ( 'NONE',  ( -0.3562281372919119393, 7.169715878026186928, 1.968597608854712133 ) ) ;
#170895 = CARTESIAN_POINT ( 'NONE',  ( -0.3282377607281367626, 1.698664549684633096, -1.225000000000013411 ) ) ;
#170896 = CARTESIAN_POINT ( 'NONE',  ( 3.924826023212550030, 2.051882857192890430, 0.6804245187241527715 ) ) ;
#170897 = CARTESIAN_POINT ( 'NONE',  ( -3.574546055497324737, 7.322054164722185732, 0.7998128361456341429 ) ) ;
#170898 = CARTESIAN_POINT ( 'NONE',  ( -6.846504384776758378, 9.010674420371453053, -1.443375672974058777 ) ) ;
#170899 = CARTESIAN_POINT ( 'NONE',  ( 3.133815226704575796, -1.450665623810345473, -1.602838778681405785 ) ) ;
#170900 = CARTESIAN_POINT ( 'NONE',  ( 5.272717044759430927, -1.855309747074182836, -0.6666870051924634888 ) ) ;
#170901 = CARTESIAN_POINT ( 'NONE',  ( 4.165211049733441584, -0.5436426828948260903, -1.646488866570811060 ) ) ;
#170902 = CARTESIAN_POINT ( 'NONE',  ( 0.6092356648998223934, -0.3158941238240610128, 2.168550393043596536 ) ) ;
#170903 = CARTESIAN_POINT ( 'NONE',  ( 0.7280630558558630616, -2.190032360377992315, 0.7273814547973026512 ) ) ;
#170904 = CARTESIAN_POINT ( 'NONE',  ( 3.339188440279222458, -1.819168825518402199, 0.9681599264559497264 ) ) ;
#170905 = CARTESIAN_POINT ( 'NONE',  ( 5.337426827915986216, 0.7834791095375337466, -1.777179163755914448 ) ) ;
#170906 = CARTESIAN_POINT ( 'NONE',  ( -7.605760987142072160, 10.85684300409898384, 1.082531754730549967 ) ) ;
#170907 = CARTESIAN_POINT ( 'NONE',  ( -5.550083779947821760, 7.568460058062819407, -1.599625672291271394 ) ) ;
#170908 = CARTESIAN_POINT ( 'NONE',  ( -1.284279953904152949, 2.952889714876734573, 0.7750000000000152323 ) ) ;
#170910 = ORIENTED_EDGE ( 'NONE', *, *, #174500, .T. ) ;
#170909 = CARTESIAN_POINT ( 'NONE',  ( 1.409462824231155764E-15, 1.016282880930358123, -12.28865868783309878 ) ) ;
#170911 = CARTESIAN_POINT ( 'NONE',  ( -7.117667457050096402, 10.28740055232499984, 1.082531754730549967 ) ) ;
#170912 = CARTESIAN_POINT ( 'NONE',  ( 3.645738483435243982, -1.669485028154977790, -1.443228448415982079 ) ) ;
#170913 = CARTESIAN_POINT ( 'NONE',  ( -3.285556943749998737, -3.667708332855377673, 1.896917185911908499 ) ) ;
#170914 = VERTEX_POINT ( 'NONE', #34089 ) ;
#170915 = CARTESIAN_POINT ( 'NONE',  ( 0.6724161089360582988, 1.288989887148813018, -1.342485977130857711 ) ) ;
#170916 = CARTESIAN_POINT ( 'NONE',  ( 4.435735274902380176, 7.313263296268260660, -1.222879399185505367 ) ) ;
#170918 = CARTESIAN_POINT ( 'NONE',  ( 6.925078400183548588, 2.417948008941684268, 2.525058136801380027 ) ) ;
#170917 = CARTESIAN_POINT ( 'NONE',  ( -6.258858270227934284, 6.997355405945988593, -0.9884160956115575214 ) ) ;
#170919 = CARTESIAN_POINT ( 'NONE',  ( 6.351489326974223637, 1.835832825663574752, -0.1405570519043483624 ) ) ;
#170920 = VERTEX_POINT ( 'NONE', #153176 ) ;
#170921 = CARTESIAN_POINT ( 'NONE',  ( 2.518495319897054330, 1.347246837915631490, -1.559621528479130825 ) ) ;
#170922 = CARTESIAN_POINT ( 'NONE',  ( -0.6801582343750143256, 0.3489583336747370534, -1.178068619123865846 ) ) ;
#170923 = CARTESIAN_POINT ( 'NONE',  ( -5.831978632172702071, 9.955725504176825780, 0.7998128361456481317 ) ) ;
#170924 = SURFACE_STYLE_USAGE ( .BOTH. , #188235 ) ;
#170925 = FILL_AREA_STYLE ('',( #23598 ) ) ;
#170926 = CARTESIAN_POINT ( 'NONE',  ( 3.323720213644492993, 7.029424015893889433, 1.040834085586084257E-14 ) ) ;
#170927 = CARTESIAN_POINT ( 'NONE',  ( 0.9013288230189763217, 1.684346374898238352, 1.187240197102001904 ) ) ;
#170929 = CARTESIAN_POINT ( 'NONE',  ( -1.364683531250010295, 13.38020833367473017, 0.7879004041258445001 ) ) ;
#170928 = CARTESIAN_POINT ( 'NONE',  ( -1.500000000000008216, 12.49999999999999645, 3.469446951953614189E-15 ) ) ;
#170930 = CARTESIAN_POINT ( 'NONE',  ( 4.632082037363250748, 8.555846143565791095, -0.7998128361456231517 ) ) ;
#170931 =( NAMED_UNIT ( * ) PLANE_ANGLE_UNIT ( ) SI_UNIT ( $, .RADIAN. ) );
#170932 = CARTESIAN_POINT ( 'NONE',  ( 5.356176587289051660, 2.204499490778097481, -0.1052899746726426722 ) ) ;
#170933 = CARTESIAN_POINT ( 'NONE',  ( 0.5093243970649004027, 1.880507610096779025, 1.065828983023514809 ) ) ;
#170934 = CARTESIAN_POINT ( 'NONE',  ( -4.772106882330234612, 6.590544000850479200, -1.443375672974053447 ) ) ;
#170935 = CARTESIAN_POINT ( 'NONE',  ( 0.6680393924826667496, 1.910109291395128972, -0.09634788558426229943 ) ) ;
#170936 = CARTESIAN_POINT ( 'NONE',  ( 0.7433754753295095385, 0.3886281223182270761, -1.978556061772406505 ) ) ;
#170937 = CARTESIAN_POINT ( 'NONE',  ( 6.739811759324814133, 8.956476034002680109, -1.443375672974078761 ) ) ;
#170938 = CARTESIAN_POINT ( 'NONE',  ( 0.07999999999999327094, 7.849261790823902629, 9.579665964948873125 ) ) ;
#170939 = CARTESIAN_POINT ( 'NONE',  ( -0.3549189177861599154, 6.558674322353176933, 3.205845166494230902 ) ) ;
#170941 = EDGE_LOOP ( 'NONE', ( #52632, #18983, #202061, #68582 ) ) ;
#170940 = CYLINDRICAL_SURFACE ( 'NONE', #16322, 0.3999999999999996336 ) ;
#170942 = TOROIDAL_SURFACE ( 'NONE', #60237, 10.89999999999920632, 0.2000000000000000111 ) ;
#170943 = CARTESIAN_POINT ( 'NONE',  ( 1.586564105604048480, -0.2713065988851799393, -1.850747533123621391 ) ) ;
#170944 = CARTESIAN_POINT ( 'NONE',  ( 2.483611571103708116, -0.6279893487078171965, 1.916353726171161620 ) ) ;
#170946 = DIRECTION ( 'NONE',  ( -1.224646799147343346E-16, 0.000000000000000000, -1.000000000000000000 ) ) ;
#170945 = CARTESIAN_POINT ( 'NONE',  ( 1.364683531249986537, 0.6552083336747522857, -0.7879004041258239610 ) ) ;
#170948 = CARTESIAN_POINT ( 'NONE',  ( 4.863951442137788739, 2.083289488599335826, -0.3080729427491457062 ) ) ;
#170947 = CARTESIAN_POINT ( 'NONE',  ( -9.040589502214116280, 9.441775928871617651, 0.7998128361456462443 ) ) ;
#170949 = AXIS2_PLACEMENT_3D ( 'NONE', #55902, #203194, #3916 ) ;
#170950 = CARTESIAN_POINT ( 'NONE',  ( 6.760712154708803823, 11.03924794713562818, 1.040834085586084257E-14 ) ) ;
#170952 = CARTESIAN_POINT ( 'NONE',  ( -8.050844288416501016, 8.287073179441051707, 1.040834085586084257E-14 ) ) ;
#170951 = CARTESIAN_POINT ( 'NONE',  ( 3.549202351727371862, 7.362762853649070571, -0.7998128361456362523 ) ) ;
#170953 = CARTESIAN_POINT ( 'NONE',  ( 4.037319642967612587, 7.289149851185872997, 0.9744337199438335428 ) ) ;
#170954 = CARTESIAN_POINT ( 'NONE',  ( 4.429947715222688487, -1.979980911821906497, 0.3981057063161990706 ) ) ;
#170955 = CARTESIAN_POINT ( 'NONE',  ( 1.364683531249990311, 4.384375000341417028, 1.214306433183764966E-14 ) ) ;
#170956 = CARTESIAN_POINT ( 'NONE',  ( 5.969198602517502117, 1.817331191306554850, 0.9757160385870704555 ) ) ;
#170957 = CARTESIAN_POINT ( 'NONE',  ( 10.08690309888728187, 10.87040115823107911, -0.7216878364870257245 ) ) ;
#170958 = CARTESIAN_POINT ( 'NONE',  ( 5.026735257907362531, 2.066873009482797841, 0.6328083787210944111 ) ) ;
#170959 = CARTESIAN_POINT ( 'NONE',  ( 5.203297092594585393, 9.292540051327542017, 0.7998128361456341429 ) ) ;
#170960 = CARTESIAN_POINT ( 'NONE',  ( 1.364683531249986537, -0.7822916663252464931, -0.7879004041258309554 ) ) ;
#170962 = CARTESIAN_POINT ( 'NONE',  ( -0.2108831679770960255, -0.001785917861228669690, -1.896958272444612792 ) ) ;
#170961 = CARTESIAN_POINT ( 'NONE',  ( 4.355912491740495440, 8.303924683664389406, 0.000000000000000000 ) ) ;
#170963 = CARTESIAN_POINT ( 'NONE',  ( 8.066738210006692000, 8.513542121203711233, 0.7216878364870458196 ) ) ;
#170965 = CARTESIAN_POINT ( 'NONE',  ( -5.395781948114519722, 5.397426482329451325, 0.000000000000000000 ) ) ;
#170964 = CARTESIAN_POINT ( 'NONE',  ( 1.416727708472965253, 0.8794254021464522619, 1.985261695379604507 ) ) ;
#170967 = CARTESIAN_POINT ( 'NONE',  ( 1.522747961674526085, -1.733470594775164075, 0.6210259959333885860 ) ) ;
#170966 = CARTESIAN_POINT ( 'NONE',  ( -5.748293942514186128, 6.769059690097084747, -1.082531754730544860 ) ) ;
#170968 = EDGE_CURVE ( 'NONE', #150426, #134733, #16754, .T. ) ;
#170969 = CARTESIAN_POINT ( 'NONE',  ( -1.364683531249997417, 2.759375000341422801, 1.214306433183764966E-14 ) ) ;
#170970 = CARTESIAN_POINT ( 'NONE',  ( 2.876726420669137863, -0.1638259704515396820, -2.185508879517850112 ) ) ;
#170971 = CARTESIAN_POINT ( 'NONE',  ( 6.983263157960363898, 2.958708369276577432, 2.506372104999963657 ) ) ;
#170972 = CARTESIAN_POINT ( 'NONE',  ( 3.977597974223236132, 2.131470459685447238, -0.7591987100158004154 ) ) ;
#170973 = CARTESIAN_POINT ( 'NONE',  ( -7.054319997812058318, 7.124461507069184130, 1.040834085586084257E-14 ) ) ;
#170974 = CARTESIAN_POINT ( 'NONE',  ( -1.873515663034567291, 3.299988112486733627, 0.3999999999999993006 ) ) ;
#170975 = CARTESIAN_POINT ( 'NONE',  ( 6.381672224870991172, 6.819330018336470012, -0.5576268912585117254 ) ) ;
#170976 = CARTESIAN_POINT ( 'NONE',  ( 1.499999999999997113, 14.14583333333333037, -0.8660254037844378194 ) ) ;
#170977 = CARTESIAN_POINT ( 'NONE',  ( 5.804299160426222848, 7.865044668620976509, -1.443375672974078761 ) ) ;
#170978 = CARTESIAN_POINT ( 'NONE',  ( 5.430809967973590169, 0.1307738731834498513, 1.764929826691101100 ) ) ;
#170979 = CARTESIAN_POINT ( 'NONE',  ( 8.718056468787178659, 10.12981962079525289, 1.199719254218462483 ) ) ;
#170980 = CARTESIAN_POINT ( 'NONE',  ( 1.571456177274520805, 0.1552745290232947217, -2.100303177343607608 ) ) ;
#170982 = CARTESIAN_POINT ( 'NONE',  ( 0.7499999999999885647, 2.566666666666689522, -1.299038105676658228 ) ) ;
#170981 = CARTESIAN_POINT ( 'NONE',  ( 1.364683531249996529, 11.46354166700806410, 0.7879004041258405033 ) ) ;
#170983 = CARTESIAN_POINT ( 'NONE',  ( 1.205442482676940541, -1.550459043822360661, -1.214442484561629509 ) ) ;
#170984 = CARTESIAN_POINT ( 'NONE',  ( -2.972980823146582186, 6.690504403638126263, 0.000000000000000000 ) ) ;
#170985 = CARTESIAN_POINT ( 'NONE',  ( 0.3792546940144908563, -0.1001052471676349837, 1.959448305358338693 ) ) ;
#170987 = ORIENTED_EDGE ( 'NONE', *, *, #139910, .T. ) ;
#170986 = CARTESIAN_POINT ( 'NONE',  ( 5.484552789610383172, -1.142847587564936207, 1.405643779654427661 ) ) ;
#170988 = CARTESIAN_POINT ( 'NONE',  ( 6.399085315970131305, 8.488685506763726352, -1.443375672974057666 ) ) ;
#170989 = CARTESIAN_POINT ( 'NONE',  ( 0.6823417656249882723, -0.01145833299191073573, -1.181850606188749264 ) ) ;
#170990 = CARTESIAN_POINT ( 'NONE',  ( 4.680451076648031616, -1.814532364864028136, -0.4542276060127621862 ) ) ;
#170991 = CARTESIAN_POINT ( 'NONE',  ( 2.367870383881045981, 5.914265881169853856, 0.000000000000000000 ) ) ;
#170992 = ORIENTED_EDGE ( 'NONE', *, *, #108550, .T. ) ;
#170993 = CARTESIAN_POINT ( 'NONE',  ( 5.418829850390409320, -1.503349927839289002, 1.423607673449282851 ) ) ;
#170994 = CARTESIAN_POINT ( 'NONE',  ( -1.225000000000028066, 2.020833333333377446, 0.7072540797572697269 ) ) ;
#170995 = ADVANCED_FACE ( 'NONE', ( #70825 ), #82837, .F. ) ;
#170996 = CARTESIAN_POINT ( 'NONE',  ( -4.448483798615272100, 8.203998508444197313, 0.000000000000000000 ) ) ;
#170997 = PRESENTATION_LAYER_ASSIGNMENT (  '', '', ( #87974 ) ) ;
#170998 = CARTESIAN_POINT ( 'NONE',  ( 1.499999999999987121, -0.9958333333333134751, 0.8660254037844524744 ) ) ;
#170999 = CARTESIAN_POINT ( 'NONE',  ( 6.805303039055573322, 10.02693841461847057, 1.199719254218460707 ) ) ;
#171000 = CARTESIAN_POINT ( 'NONE',  ( -9.073431116043565225, 11.60875560684942265, -1.599625672291263179 ) ) ;
#171001 = CARTESIAN_POINT ( 'NONE',  ( 6.692885107001518286, 7.837396042037102717, -1.199719254218452047 ) ) ;
#171002 = CARTESIAN_POINT ( 'NONE',  ( 1.364683531249986537, -0.3447916663252443836, -0.7879004041258309554 ) ) ;
#171004 = AXIS2_PLACEMENT_3D ( 'NONE', #22675, #90923, #158056 ) ;
#171003 = CARTESIAN_POINT ( 'NONE',  ( -1.500000000000001332, 1.150000000000019007, 0.000000000000000000 ) ) ;
#171006 = CARTESIAN_POINT ( 'NONE',  ( 6.308621549060418054, 6.254479983525607523, 0.7998128361456341429 ) ) ;
#171005 = CARTESIAN_POINT ( 'NONE',  ( 5.564887814092526419, 1.486691789297951871, -1.280227714881218892 ) ) ;
#171007 = CARTESIAN_POINT ( 'NONE',  ( 2.284529629648517801, -1.956262009633228605, 0.4871271731112236658 ) ) ;
#171008 = CARTESIAN_POINT ( 'NONE',  ( -4.650083499807267984, 5.295740330745369207, 2.420000000000010587 ) ) ;
#171009 = CARTESIAN_POINT ( 'NONE',  ( 0.6268464039562298140, 0.1668571106153530770, 2.185281662807083691 ) ) ;
#171010 = CARTESIAN_POINT ( 'NONE',  ( -11.89317557362571698, 9.837241561624070485, 1.599935658896036283 ) ) ;
#171011 = CARTESIAN_POINT ( 'NONE',  ( 2.495189509527053762, 1.443206194050347557, 1.189963633554675937 ) ) ;
#171012 = CARTESIAN_POINT ( 'NONE',  ( -1.364683531250012516, 4.738541667008091096, -0.7879004041258300672 ) ) ;
#171013 = CARTESIAN_POINT ( 'NONE',  ( 3.814701174604028466, -0.6354162253871125099, -1.910337659313849024 ) ) ;
#171014 = CARTESIAN_POINT ( 'NONE',  ( -7.133561379084627063, 11.47423870890741782, 0.7998128361456481317 ) ) ;
#171016 = CARTESIAN_POINT ( 'NONE',  ( 4.939118062403117904, -1.789252976562827779, -1.131630611658622332 ) ) ;
#171015 = CARTESIAN_POINT ( 'NONE',  ( -3.768803514918943609, 7.340761834139994058, 0.7216878364870317197 ) ) ;
#171017 = CARTESIAN_POINT ( 'NONE',  ( -0.07933543236768950124, -9.910877263631634904, -9.499668725233682665 ) ) ;
#171018 = CARTESIAN_POINT ( 'NONE',  ( 5.652806998763869828, -0.4994405740583847675, -2.009109930559597856 ) ) ;
#171020 = CARTESIAN_POINT ( 'NONE',  ( 6.720655732516679137, 7.052218778754904882, 2.671889809988809983 ) ) ;
#171019 = CARTESIAN_POINT ( 'NONE',  ( 0.7496951219271037470, 2.088183804393455301, -0.1063107438588738879 ) ) ;
#171022 = ORIENTED_EDGE ( 'NONE', *, *, #68712, .T. ) ;
#171021 = CARTESIAN_POINT ( 'NONE',  ( 0.1469036390603413456, -1.327996847208750442, -1.100432056080926202 ) ) ;
#171023 = CARTESIAN_POINT ( 'NONE',  ( 8.260995669428309540, 8.532249790621511565, 0.7998128361456481317 ) ) ;
#171024 = LINE ( 'NONE', #138543, #144281 ) ;
#171025 = SURFACE_STYLE_USAGE ( .BOTH. , #5290 ) ;
#171026 = CARTESIAN_POINT ( 'NONE',  ( -10.96276904610368597, 4.385383195573210102, 6.374211443005175504 ) ) ;
#171027 = CARTESIAN_POINT ( 'NONE',  ( 6.710922848640084482, 9.812865175846695820, -1.082531754730537976 ) ) ;
#171028 = CARTESIAN_POINT ( 'NONE',  ( 0.6823417656249969321, 13.33854166700806942, -1.181850606188757036 ) ) ;
#171029 = CARTESIAN_POINT ( 'NONE',  ( 6.516268831907007453, -1.911747763583053317, 0.05203757306279645223 ) ) ;
#171030 = CARTESIAN_POINT ( 'NONE',  ( -6.333630315878337136, 10.54098580183340772, 0.000000000000000000 ) ) ;
#171031 = CARTESIAN_POINT ( 'NONE',  ( 5.681030059326015014, 6.586622143090519188, -1.199719254218445830 ) ) ;
#171032 = CARTESIAN_POINT ( 'NONE',  ( -9.469892045836674654, -6.532648833121171172, 0.4294077647110563500 ) ) ;
#171033 = CARTESIAN_POINT ( 'NONE',  ( -1.000000000000017097, 9.200000000000018829, 0.4000000000000144551 ) ) ;
#171034 = CARTESIAN_POINT ( 'NONE',  ( 3.602716132929354664, 5.226254793216122074, 1.599625672291267398 ) ) ;
#171035 = EDGE_LOOP ( 'NONE', ( #136964, #100848 ) ) ;
#171036 = CARTESIAN_POINT ( 'NONE',  ( 6.099232498865051255, -0.2440123228986730841, 2.001514574626765075 ) ) ;
#171037 = CARTESIAN_POINT ( 'NONE',  ( 0.8035760164417544704, 1.868272328500224289, -1.003034915376184388 ) ) ;
#171038 = DIRECTION ( 'NONE',  ( -1.000000000000000000, 0.000000000000000000, 0.000000000000000000 ) ) ;
#171039 = CARTESIAN_POINT ( 'NONE',  ( -0.1399997263889612154, 1.357298622859518078, -2.254419820505838334 ) ) ;
#171040 = CARTESIAN_POINT ( 'NONE',  ( -5.477130870240893401, 6.452702772444876445, 1.082531754730548412 ) ) ;
#171041 = CARTESIAN_POINT ( 'NONE',  ( 8.866669273657322492, 12.32790267170016207, -1.082531754730543083 ) ) ;
#171042 = CARTESIAN_POINT ( 'NONE',  ( 3.854321288642187149, -1.967005588004781202, -0.1009957709416451771 ) ) ;
#171043 = CARTESIAN_POINT ( 'NONE',  ( 4.112907772398490813, 0.1017678201147946826, 2.013986186455194449 ) ) ;
#171044 = CARTESIAN_POINT ( 'NONE',  ( -6.368579470117215813, 8.453095353268645695, 1.599625672291283607 ) ) ;
#171045 = CARTESIAN_POINT ( 'NONE',  ( 6.727182134110222478, 4.688348259194305534, 2.751590707055273199 ) ) ;
#171046 = CARTESIAN_POINT ( 'NONE',  ( 4.716832014018703667, -0.1092502567305031480, 2.188841582221649595 ) ) ;
#171047 = CARTESIAN_POINT ( 'NONE',  ( -1.333477130265052990, 8.249568609204949610, -9.911050286642563378 ) ) ;
#171048 = CARTESIAN_POINT ( 'NONE',  ( 2.977471715415116460, 1.829795069231574534, -0.6025905002205227401 ) ) ;
#171049 = CARTESIAN_POINT ( 'NONE',  ( -5.994676475536691029, 10.14553965476814845, 0.7998128361456481317 ) ) ;
#171050 = CARTESIAN_POINT ( 'NONE',  ( -0.02968770228140016343, 1.391517546076680434, -2.083419219542380407 ) ) ;
#171051 = CARTESIAN_POINT ( 'NONE',  ( 0.000000000000000000, 3.481540744127368914, 0.000000000000000000 ) ) ;
#171052 = CARTESIAN_POINT ( 'NONE',  ( -8.804383207025272995, 15.51845922978708181, -8.203328898748138087 ) ) ;
#171053 = CARTESIAN_POINT ( 'NONE',  ( 4.855228407469603269, 7.718164671139588151, -1.082531754730548412 ) ) ;
#171054 = CARTESIAN_POINT ( 'NONE',  ( 6.173040012923759257, 6.096301524699504704, -0.7998128361456281477 ) ) ;
#171055 = ORIENTED_EDGE ( 'NONE', *, *, #150437, .F. ) ;
#171056 = CARTESIAN_POINT ( 'NONE',  ( 3.594320121398666856, 7.207474218358159490, -1.734723475976807094E-15 ) ) ;
#171057 = ORIENTED_EDGE ( 'NONE', *, *, #136186, .F. ) ;
#171058 = CARTESIAN_POINT ( 'NONE',  ( 5.559413648769178096, 1.607788300429791262, 1.137107417019854072 ) ) ;
#171060 = CARTESIAN_POINT ( 'NONE',  ( 3.897138702661524956, -0.1997049427340416294, -2.003176435020975088 ) ) ;
#171059 = CARTESIAN_POINT ( 'NONE',  ( 0.4330194205178988232, -1.374205638499223614, -1.372529395279479703 ) ) ;
#171061 = CARTESIAN_POINT ( 'NONE',  ( 5.536544918007444416, 2.217299919257350371, -0.6050018498083614693 ) ) ;
#171062 = CARTESIAN_POINT ( 'NONE',  ( 3.590524784426767813, 1.814595775041549564, 0.4119230038364861679 ) ) ;
#171063 = CARTESIAN_POINT ( 'NONE',  ( 0.000000000000000000, -0.1968749995220437643, -3.793834371823813001 ) ) ;
#171064 = CARTESIAN_POINT ( 'NONE',  ( -10.72111444838896155, -6.105866302529358691, 1.138412281109779656E-15 ) ) ;
#171065 = CARTESIAN_POINT ( 'NONE',  ( 10.10176665042273392, 1.000000000000000888, 6.279211784079129721 ) ) ;
#171066 = CARTESIAN_POINT ( 'NONE',  ( -5.357443255694392725, 9.402100898285455699, 0.000000000000000000 ) ) ;
#171067 = CARTESIAN_POINT ( 'NONE',  ( -4.421367491832313590, 6.251624388594711590, 1.443375672974065660 ) ) ;
#171068 = CARTESIAN_POINT ( 'NONE',  ( 5.935123052105460317, -1.514893180500265002, -1.441204661170019108 ) ) ;
#171069 = CARTESIAN_POINT ( 'NONE',  ( 5.178851490740196795, 7.065079377328788546, 1.443375672974062551 ) ) ;
#171070 = VERTEX_POINT ( 'NONE', #136941 ) ;
#171071 = PRESENTATION_STYLE_ASSIGNMENT (( #137530 ) ) ;
#171072 = CARTESIAN_POINT ( 'NONE',  ( -11.04536101718726293, 12.69999999999999929, 1.099999999999996758 ) ) ;
#171073 = CARTESIAN_POINT ( 'NONE',  ( 0.8205984872286451459, 1.685833220154912881, 0.7012733028506010768 ) ) ;
#171074 = CARTESIAN_POINT ( 'NONE',  ( -5.087333953625788219, 6.958308917361963886, 1.599625672291267398 ) ) ;
#171075 = CARTESIAN_POINT ( 'NONE',  ( 3.094086244858067047, -0.3350832708051197373, 1.701246549458427015 ) ) ;
#171076 = CARTESIAN_POINT ( 'NONE',  ( -1.743066579297358008E-15, 1.875000000682791379, 1.224999999999958566 ) ) ;
#171077 = CARTESIAN_POINT ( 'NONE',  ( 6.609000000000047947, 0.5928748489389294996, 1.953858053793898542 ) ) ;
#171078 = CARTESIAN_POINT ( 'NONE',  ( -7.040761844198392794, 7.108643661186573759, -0.7998128361456291469 ) ) ;
#171079 = CARTESIAN_POINT ( 'NONE',  ( -4.326460414921602826, 8.061637894134911164, 8.322892513849239118E-08 ) ) ;
#171080 = CARTESIAN_POINT ( 'NONE',  ( 0.2509399751232620490, -0.4509356589572112162, -2.027996233343106081 ) ) ;
#171081 = CARTESIAN_POINT ( 'NONE',  ( 6.041596546049881944, -1.325759876995153075, -1.255439798616593716 ) ) ;
#171082 = CARTESIAN_POINT ( 'NONE',  ( 3.907043859180459933, -1.606318986283064021, 1.125903821926607318 ) ) ;
#171083 = CARTESIAN_POINT ( 'NONE',  ( -1.225000000000045386, -0.9374999993171719836, -5.551115123125782702E-14 ) ) ;
#171084 = CARTESIAN_POINT ( 'NONE',  ( -7.991641480251377772, 11.41099992934688956, 1.199719254218453823 ) ) ;
#171085 = CARTESIAN_POINT ( 'NONE',  ( 8.274553823041976841, 8.548067636504127265, 1.040834085586084257E-14 ) ) ;
#171086 = EDGE_CURVE ( 'NONE', #31644, #95942, #117539, .T. ) ;
#171087 = CARTESIAN_POINT ( 'NONE',  ( 4.178469031319306914, 1.000645923475869559, 1.869553197578948334 ) ) ;
#171088 = CARTESIAN_POINT ( 'NONE',  ( -4.791166081694341550, 4.882818525799564213, 0.4357780244859492669 ) ) ;
#171089 = CIRCLE ( 'NONE', #133100, 11.92000000000000171 ) ;
#171090 = CARTESIAN_POINT ( 'NONE',  ( -8.272446282632566650, 12.80293776304669962, 0.7998128361456481317 ) ) ;
#171091 = CARTESIAN_POINT ( 'NONE',  ( 2.061466481998303735, 1.718891244229248105, 1.153550331455879707 ) ) ;
#171093 = CARTESIAN_POINT ( 'NONE',  ( -1.364683531250014514, -0.6989583329919100141, -0.7879004041258359514 ) ) ;
#171092 =( NAMED_UNIT ( * ) PLANE_ANGLE_UNIT ( ) SI_UNIT ( $, .RADIAN. ) );
#171094 = VERTEX_POINT ( 'NONE', #133765 ) ;
#171097 = ORIENTED_EDGE ( 'NONE', *, *, #95578, .F. ) ;
#171096 = CARTESIAN_POINT ( 'NONE',  ( 4.407017973072342443, -0.4864924038828158381, -2.167217472756521879 ) ) ;
#171095 = AXIS2_PLACEMENT_3D ( 'NONE', #117292, #34894, #184349 ) ;
#171098 = CARTESIAN_POINT ( 'NONE',  ( 2.145563594533715257, 0.9871410470321148045, 2.076082784368099787 ) ) ;
#171100 = CARTESIAN_POINT ( 'NONE',  ( 6.631690664033638605, 1.975529463507015526, -0.5929735606366983713 ) ) ;
#171099 = CARTESIAN_POINT ( 'NONE',  ( 9.002250809793993724, 11.52571191622492464, -1.443375672974057666 ) ) ;
#171102 = CARTESIAN_POINT ( 'NONE',  ( 3.475000000000000533, -0.2041666666666657748, 2.006292185433948827 ) ) ;
#171101 = CARTESIAN_POINT ( 'NONE',  ( 7.702440666339465558, 8.158804663583751449, -0.7216878364870317197 ) ) ;
#171103 = CARTESIAN_POINT ( 'NONE',  ( -10.91005274787796786, -6.893137084989842123, 0.4659925305415812957 ) ) ;
#171104 = ORIENTED_EDGE ( 'NONE', *, *, #9331, .F. ) ;
#171105 = CARTESIAN_POINT ( 'NONE',  ( 5.346851039111033543, 6.199209027673978412, -2.420000000000000373 ) ) ;
#171106 = CARTESIAN_POINT ( 'NONE',  ( 3.445477555875466891, -1.765175379189663607, 0.7362804355328657069 ) ) ;
#171107 = CARTESIAN_POINT ( 'NONE',  ( 1.737500000000001155, -1.283333333333334325, 3.009438278150922130 ) ) ;
#171108 = CARTESIAN_POINT ( 'NONE',  ( 3.873808679987042147, 0.9582704680195216485, 1.433834079761304281 ) ) ;
#171109 = CARTESIAN_POINT ( 'NONE',  ( 2.764861550476094276, -0.1531697945360478708, -2.010801143277194392 ) ) ;
#171110 = CARTESIAN_POINT ( 'NONE',  ( 3.815287691547566418, 1.229174737571071541, -1.942296044024049761 ) ) ;
#171111 = CIRCLE ( 'NONE', #22345, 10.24999999999998934 ) ;
#171112 = CARTESIAN_POINT ( 'NONE',  ( 3.550319795034285519, 2.262578822424826441, 0.004170446471787879993 ) ) ;
#171113 = CARTESIAN_POINT ( 'NONE',  ( 0.01274299142895937362, -0.9473294304004549193, -1.991142614049784099 ) ) ;
#171114 = CARTESIAN_POINT ( 'NONE',  ( -6.129694847154222970, 7.284303755502281597, -1.082531754730549967 ) ) ;
#171115 = CARTESIAN_POINT ( 'NONE',  ( 5.149538872483485186, 0.5550977867328189541, -1.680460614999980340 ) ) ;
#171117 = CARTESIAN_POINT ( 'NONE',  ( 1.183963288966838334, -1.026766722195756376, 2.049517438521175183 ) ) ;
#171116 = CARTESIAN_POINT ( 'NONE',  ( 6.200875153403774043, 8.327716660428123419, -1.599625672291283607 ) ) ;
#171118 = CARTESIAN_POINT ( 'NONE',  ( 5.665905727187005247, -1.164751086281138770, 1.425882759469448979 ) ) ;
#171119 = CARTESIAN_POINT ( 'NONE',  ( -4.457933580795036654, 4.095344020549286590, -0.7998128361456221525 ) ) ;
#171120 = CARTESIAN_POINT ( 'NONE',  ( 5.226606370275341362, 0.1587857941063846590, 2.185760735149797185 ) ) ;
#171121 = CARTESIAN_POINT ( 'NONE',  ( -4.685224601974262271, 7.623789914682047808, -1.199719254218453823 ) ) ;
#171122 = CARTESIAN_POINT ( 'NONE',  ( -4.471491734408701291, 4.111161866431900513, 1.214306433183764966E-14 ) ) ;
#171123 = CARTESIAN_POINT ( 'NONE',  ( -4.767792892813339733, 15.51850240610817444, 11.02130865604331689 ) ) ;
#171124 = CARTESIAN_POINT ( 'NONE',  ( 6.373496627357888578, -0.2573980274669443458, 2.054251119134167691 ) ) ;
#171125 = CARTESIAN_POINT ( 'NONE',  ( 0.6027503803631119039, 1.865048444749048739, 0.7672877736318934883 ) ) ;
#171126 = CARTESIAN_POINT ( 'NONE',  ( -1.001543065824772872E-14, 5.571875000341416140, 1.575800808251672791 ) ) ;
#171127 = CARTESIAN_POINT ( 'NONE',  ( 3.791558849520747287, 1.396117892292214613, 1.327735796816224223 ) ) ;
#171128 = CARTESIAN_POINT ( 'NONE',  ( 0.6823417656249934904, 9.692708333674735499, 1.181850606188764807 ) ) ;
#171129 = VECTOR ( 'NONE', #37541, 1000.000000000000114 ) ;
#171130 = CARTESIAN_POINT ( 'NONE',  ( 1.564984312397620814, 0.7026195195478746047, 2.107413697313319290 ) ) ;
#171132 = ORIENTED_EDGE ( 'NONE', *, *, #15624, .F. ) ;
#171131 = DIRECTION ( 'NONE',  ( 5.551115123125764213E-17, 0.000000000000000000, -1.000000000000000000 ) ) ;
#171134 = CARTESIAN_POINT ( 'NONE',  ( -7.451274665340259951, -7.616254850791390751, 6.794158526849257029 ) ) ;
#171133 = CARTESIAN_POINT ( 'NONE',  ( -11.89942855770814134, 9.799999999999998934, -0.7000000000000009548 ) ) ;
#171135 = CARTESIAN_POINT ( 'NONE',  ( 3.297657676621871925, 4.870353260857385180, 1.599625672291267398 ) ) ;
#171136 = CARTESIAN_POINT ( 'NONE',  ( -1.814759087649988833, 3.975067388631688292, -0.4606438099578630818 ) ) ;
#171137 = CARTESIAN_POINT ( 'NONE',  ( -1.772826578343109416, 3.949999999999995293, -0.4000000000000270561 ) ) ;
#171138 = CARTESIAN_POINT ( 'NONE',  ( 3.939498435241196805, 2.812004590916141300, -0.7749999999999935829 ) ) ;
#171139 = CARTESIAN_POINT ( 'NONE',  ( 2.717183929654675811, -1.705535211757349456, -0.9694657131227711888 ) ) ;
#171141 = CARTESIAN_POINT ( 'NONE',  ( -1.364683531250014514, 2.051041667008086655, -0.7879004041258289570 ) ) ;
#171140 = CARTESIAN_POINT ( 'NONE',  ( 5.392392409933256303, 7.314210449720692786, 1.599625672291267398 ) ) ;
#171142 = FACE_OUTER_BOUND ( 'NONE', #203656, .T. ) ;
#171143 = CARTESIAN_POINT ( 'NONE',  ( 0.2739786698724961944, -2.023204396000506833, 0.4007670430965051822 ) ) ;
#171144 = CARTESIAN_POINT ( 'NONE',  ( -9.182950115157607840, 9.607863310639020327, 0.7998128361456462443 ) ) ;
#171145 = CARTESIAN_POINT ( 'NONE',  ( -3.741687207247254676, 7.309126141856352454, 1.040834085586084257E-14 ) ) ;
#171146 = AXIS2_PLACEMENT_3D ( 'NONE', #15039, #36636, #148279 ) ;
#171147 = CARTESIAN_POINT ( 'NONE',  ( 6.702040708066513197, -2.161345696851162845, 0.04751196314212167288 ) ) ;
#171149 = VERTEX_POINT ( 'NONE', #53539 ) ;
#171148 = CARTESIAN_POINT ( 'NONE',  ( -5.799137018343247796, 7.788745826199009237, -1.599625672291256295 ) ) ;
#171151 = EDGE_CURVE ( 'NONE', #183115, #199688, #69542, .T. ) ;
#171150 = CARTESIAN_POINT ( 'NONE',  ( 0.6823417656249917140, 5.342708333674749177, 1.181850606188765695 ) ) ;
#171152 = CARTESIAN_POINT ( 'NONE',  ( 1.053721402318724021, 1.868689351376726204, -0.08586956420430363890 ) ) ;
#171153 = CARTESIAN_POINT ( 'NONE',  ( 0.7911957196942709380, 1.314039333434241508, -1.131676627359794240 ) ) ;
#171155 = CARTESIAN_POINT ( 'NONE',  ( 4.687173145698103838, 1.624054394666199830, 1.471728111018810070 ) ) ;
#171154 = CARTESIAN_POINT ( 'NONE',  ( 1.360316468750000896, 2.515625000341401130, -3.469446951953614189E-15 ) ) ;
#171156 = CARTESIAN_POINT ( 'NONE',  ( 5.298025090176222029, -0.8365315220497183679, 2.150796518170698057 ) ) ;
#171157 = CARTESIAN_POINT ( 'NONE',  ( 6.802032647988246694, -2.060431444914239130, 0.04577141437269586360 ) ) ;
#171158 = CARTESIAN_POINT ( 'NONE',  ( 2.062350447250702157, -1.775486198902403778, -0.7870378659600388849 ) ) ;
#171159 = CARTESIAN_POINT ( 'NONE',  ( -5.761852095683518193, 6.784877535461274256, 1.082531754730546636 ) ) ;
#171160 = CIRCLE ( 'NONE', #95110, 10.91999999999999105 ) ;
#171161 = CYLINDRICAL_SURFACE ( 'NONE', #85642, 0.3999999999999993006 ) ;
#171162 = CARTESIAN_POINT ( 'NONE',  ( 4.204437034013637664, 6.958908068774287692, -1.082531754730548412 ) ) ;
#171163 = CARTESIAN_POINT ( 'NONE',  ( 1.360316468749971586, 0.008342803999308550170, 0.2745256636459995070 ) ) ;
#171164 = CARTESIAN_POINT ( 'NONE',  ( 3.779922787921150995, 1.701948043757589124, -1.081065327119046016 ) ) ;
#171165 = CARTESIAN_POINT ( 'NONE',  ( -5.111060722227552588, 6.025620933095978238, 1.082531754730546636 ) ) ;
#171166 = CARTESIAN_POINT ( 'NONE',  ( -6.818824913030298696, 6.919993584815607335, 0.7998128361456341429 ) ) ;
#171167 = CARTESIAN_POINT ( 'NONE',  ( 10.08456733046637765, 10.65975006183261087, 0.000000000000000000 ) ) ;
#171169 = CARTESIAN_POINT ( 'NONE',  ( 7.882977371601994854, -5.341768514962173420, -7.624693973552353121 ) ) ;
#171168 = CARTESIAN_POINT ( 'NONE',  ( 0.6623940301842005107, -1.324425631624454036, 1.256838194884236204 ) ) ;
#171170 = CARTESIAN_POINT ( 'NONE',  ( -6.784929528996132220, 6.880448970109080520, 0.000000000000000000 ) ) ;
#171171 = LINE ( 'NONE', #184210, #37065 ) ;
#171172 = CARTESIAN_POINT ( 'NONE',  ( -10.14895191633106819, 2.999999999999999112, 7.601392964450658596 ) ) ;
#171173 = ORIENTED_EDGE ( 'NONE', *, *, #41132, .F. ) ;
#171174 = CARTESIAN_POINT ( 'NONE',  ( 5.190332118341006051, -2.045072267241864861, -0.2543341860123843334 ) ) ;
#171175 = CARTESIAN_POINT ( 'NONE',  ( -7.390603132780803719, 7.794994207765291172, -0.7216878364870338292 ) ) ;
#171176 = CARTESIAN_POINT ( 'NONE',  ( -2.788906526875773208E-15, 11.71875000068279604, -1.499999999999998446 ) ) ;
#171177 = CARTESIAN_POINT ( 'NONE',  ( -3.632695093457760649, 6.325562478087638496, -1.199719254218452047 ) ) ;
#171178 = CARTESIAN_POINT ( 'NONE',  ( -10.32183501870554387, 10.93656236477829502, 0.7998128361456462443 ) ) ;
#171179 = CARTESIAN_POINT ( 'NONE',  ( 5.215492487644303843, 1.652332223238074604, 1.161132580238199541 ) ) ;
#171181 = ORIENTED_EDGE ( 'NONE', *, *, #161821, .F. ) ;
#171180 = CARTESIAN_POINT ( 'NONE',  ( 6.199871938995108245, 1.529590366309235172, 1.610960538716522006 ) ) ;
#171182 = CARTESIAN_POINT ( 'NONE',  ( -2.993318053567081360, 6.714231172462041819, 0.000000000000000000 ) ) ;
#171183 = CARTESIAN_POINT ( 'NONE',  ( 6.114890974963323345, 7.092793211334054604, 1.199719254218462483 ) ) ;
#171184 = CARTESIAN_POINT ( 'NONE',  ( 5.330957127283824981, 0.1492067265368417217, 2.055538663769764796 ) ) ;
#171185 = CARTESIAN_POINT ( 'NONE',  ( 3.727185537919291747, 2.006959858346604619, 0.1948421285040344286 ) ) ;
#171186 = ORIENTED_EDGE ( 'NONE', *, *, #64855, .T. ) ;
#171187 = FACE_OUTER_BOUND ( 'NONE', #196760, .T. ) ;
#171188 = CARTESIAN_POINT ( 'NONE',  ( 3.704402285031850539, 5.344888637335695414, -1.599625672291262513 ) ) ;
#171190 = ORIENTED_EDGE ( 'NONE', *, *, #111491, .F. ) ;
#171189 = CARTESIAN_POINT ( 'NONE',  ( -5.769876891067536206, 8.889217585290882795, 1.199719254218454489 ) ) ;
#171191 = CARTESIAN_POINT ( 'NONE',  ( 5.535985025370705692, 7.434063834270491000, -1.247683609459742549 ) ) ;
#171192 = CARTESIAN_POINT ( 'NONE',  ( 4.288435361214689046, -1.930121902525683053, 0.5825675424541224556 ) ) ;
#171193 = CARTESIAN_POINT ( 'NONE',  ( 3.679498877186979211, -0.9061679144062879665, 1.602619060095414216 ) ) ;
#171194 = DIRECTION ( 'NONE',  ( 1.276756478318932585E-15, -1.000000000000000000, 1.665334536937738262E-16 ) ) ;
#171195 = CARTESIAN_POINT ( 'NONE',  ( 1.963905137100800724, 0.3917726540721230832, -2.274054798471192296 ) ) ;
#171196 = CARTESIAN_POINT ( 'NONE',  ( 4.061549535745618833, 6.896169004081968090, -1.199719254218452047 ) ) ;
#171197 = CARTESIAN_POINT ( 'NONE',  ( 4.112696061561730509, 1.531809107248631507, -1.525399859652858847 ) ) ;
#171198 = CARTESIAN_POINT ( 'NONE',  ( 6.611572464958476836, 10.86525164242692298, 0.7998128361456462443 ) ) ;
#171199 = CARTESIAN_POINT ( 'NONE',  ( -5.762378981008047241, 6.681529218386182301, 1.199719254218450271 ) ) ;
#171200 = CARTESIAN_POINT ( 'NONE',  ( 3.163697234774452305, -0.6641558444393131921, -2.200356767709225725 ) ) ;
#171201 = CARTESIAN_POINT ( 'NONE',  ( 1.499999999999978906, 4.077083334016147198, -0.8660254037844369313 ) ) ;
#171202 = CARTESIAN_POINT ( 'NONE',  ( 2.483090063216564669, 1.711211315118581711, -0.7561169667836544761 ) ) ;
#171203 = CARTESIAN_POINT ( 'NONE',  ( 6.789933821422706295, -0.8420773930338676383, 1.780570074765168043 ) ) ;
#171205 = CARTESIAN_POINT ( 'NONE',  ( -7.533490631048818109, 8.818102486758951031, -1.199719254218452047 ) ) ;
#171204 = CARTESIAN_POINT ( 'NONE',  ( -1.001543065824772872E-14, 5.071875000341421469, 1.575800808251672791 ) ) ;
#171207 = CARTESIAN_POINT ( 'NONE',  ( 1.612255294781844706, -2.189918024983358080, 0.2725913246661854084 ) ) ;
#171206 = CARTESIAN_POINT ( 'NONE',  ( -4.238895582566952314, 8.097128612970093897, 1.040834085586084257E-14 ) ) ;
#171208 = CARTESIAN_POINT ( 'NONE',  ( -4.009193028827814587, 7.297902834095492786, -0.7581239365674132813 ) ) ;
#171209 = CARTESIAN_POINT ( 'NONE',  ( 4.320244504248938355, 8.192035688265757898, 1.040834085586084257E-14 ) ) ;
#171210 = CARTESIAN_POINT ( 'NONE',  ( -4.786191920824102830, 5.542644314838231168, 1.199719254218462483 ) ) ;
#171211 = CARTESIAN_POINT ( 'NONE',  ( -7.873959529867724072, -5.295524846228480520, 7.681496476274701557 ) ) ;
#171212 = CARTESIAN_POINT ( 'NONE',  ( 6.244996228834688523, -1.665663155820007013, 1.054347381401467887 ) ) ;
#171213 = CARTESIAN_POINT ( 'NONE',  ( 5.883493432195608719, 2.134490442297873880, -0.8776364701479767438 ) ) ;
#171214 = CARTESIAN_POINT ( 'NONE',  ( 0.1390251588108057101, -0.1389306544097475005, -1.930426113910483688 ) ) ;
#171215 = CARTESIAN_POINT ( 'NONE',  ( 2.553648762129530958, 1.591643574212991297, 1.311770128662164137 ) ) ;
#171216 = CARTESIAN_POINT ( 'NONE',  ( 6.968527767744104651, 8.192665819532020777, 1.082531754730558626 ) ) ;
#171217 = CARTESIAN_POINT ( 'NONE',  ( 6.210516883511641772, 9.403297576475722508, 1.199719254218452047 ) ) ;
#171218 = CARTESIAN_POINT ( 'NONE',  ( 6.710922848640084482, 9.812865175846695820, -1.082531754730537976 ) ) ;
#171219 = CARTESIAN_POINT ( 'NONE',  ( -1.364683531250012516, 3.301041667008084879, -0.7879004041258289570 ) ) ;
#171220 = CARTESIAN_POINT ( 'NONE',  ( -1.500000000000022204, 8.627523663848661428, 2.580000000000011173 ) ) ;
#171221 = CARTESIAN_POINT ( 'NONE',  ( 4.975479186090857375, 5.867442474269873642, 1.082531754730560403 ) ) ;
#171222 = CARTESIAN_POINT ( 'NONE',  ( 5.916515574059204141, 0.8745146271147998807, 1.987442084954823773 ) ) ;
#171224 = CARTESIAN_POINT ( 'NONE',  ( 4.686955257832659427, 1.367739038236553517, 1.232883728221023212 ) ) ;
#171223 = CARTESIAN_POINT ( 'NONE',  ( 3.469446951953614189E-15, 0.2401923788623722134, 6.938893903907228378E-15 ) ) ;
#171225 = ADVANCED_FACE ( 'NONE', ( #102284 ), #181405, .F. ) ;
#171226 = CARTESIAN_POINT ( 'NONE',  ( 9.567202289542830584, -7.627132808484214266, -0.008219159353554262443 ) ) ;
#171227 = CARTESIAN_POINT ( 'NONE',  ( 4.580108180932601414, 8.499999999999996447, -0.1719113009628105149 ) ) ;
#171228 = CARTESIAN_POINT ( 'NONE',  ( -11.88168509644349058, 9.719999999999982876, 1.685788023084328513 ) ) ;
#171229 = CARTESIAN_POINT ( 'NONE',  ( -4.103288207896339301, 7.680416417065718093, 0.7589585138018557497 ) ) ;
#171230 = CARTESIAN_POINT ( 'NONE',  ( -0.3639057010162629613, 2.808035090322519522, 2.035120794639562636 ) ) ;
#171231 = CARTESIAN_POINT ( 'NONE',  ( 6.270956187569860063, 6.991113019333711875, 0.9580997929081371822 ) ) ;
#171232 = CARTESIAN_POINT ( 'NONE',  ( -0.09332341176954483952, -0.4182270256129701491, -1.872751671355552983 ) ) ;
#171233 = CARTESIAN_POINT ( 'NONE',  ( 1.604008636410862554, -0.6330215999658711512, -1.652955932040809595 ) ) ;
#171234 = CARTESIAN_POINT ( 'NONE',  ( 6.340495571224031401, 1.157139813629002756, -1.647119299906736556 ) ) ;
#171236 = CARTESIAN_POINT ( 'NONE',  ( 2.829585337313187399, 0.6869450147981278620, -1.788391637942953860 ) ) ;
#171235 = CARTESIAN_POINT ( 'NONE',  ( -9.561524646135538319, 12.17819805862340310, -1.599625672291263179 ) ) ;
#171237 = DIRECTION ( 'NONE',  ( -0.000000000000000000, -1.000000000000000000, -0.000000000000000000 ) ) ;
#171238 = CARTESIAN_POINT ( 'NONE',  ( 4.334397697284593676, -1.135867708366841367, 1.608802569665278348 ) ) ;
#171239 = CARTESIAN_POINT ( 'NONE',  ( 0.2992908618118708675, -0.2657624787030036240, -2.103842954668332599 ) ) ;
#171240 = CARTESIAN_POINT ( 'NONE',  ( -3.810004860640155311, 4.403759411290286252, 1.199719254218462483 ) ) ;
#171241 = CARTESIAN_POINT ( 'NONE',  ( 3.203821283898714345, -1.868584281295191607, 0.09040415888627445495 ) ) ;
#171243 = ORIENTED_EDGE ( 'NONE', *, *, #156087, .F. ) ;
#171242 = CARTESIAN_POINT ( 'NONE',  ( 5.971300253285758863, 0.1196647562241616447, -1.720808320142935610 ) ) ;
#171245 = CARTESIAN_POINT ( 'NONE',  ( 3.009546912553647147, 5.494593250412460606, -1.082531754730543083 ) ) ;
#171244 = CARTESIAN_POINT ( 'NONE',  ( 2.895379187063460424, 1.892502543702856865, -1.135010264495312837 ) ) ;
#171246 = CARTESIAN_POINT ( 'NONE',  ( -0.6823417656250212460, 3.613541667008085767, 1.181850606188767472 ) ) ;
#171247 = CARTESIAN_POINT ( 'NONE',  ( 1.293506021254931193, -1.865543137965872678, 0.8802379953135958113 ) ) ;
#171248 = CARTESIAN_POINT ( 'NONE',  ( 6.425674737872927089, 9.584038729905381970, -1.199719254218440723 ) ) ;
#171250 = CARTESIAN_POINT ( 'NONE',  ( -8.859363311525973117, 12.42334206583395328, -1.199719254218446718 ) ) ;
#171249 = CIRCLE ( 'NONE', #101992, 7.750000000000000888 ) ;
#171251 = DIRECTION ( 'NONE',  ( 0.000000000000000000, 0.000000000000000000, 1.000000000000000000 ) ) ;
#171252 = CARTESIAN_POINT ( 'NONE',  ( -5.590039407536138150, 5.416134151747256986, 0.000000000000000000 ) ) ;
#171253 = CARTESIAN_POINT ( 'NONE',  ( -7.768428355091604232, -6.306978362809940286, -7.788485247870016615 ) ) ;
#171254 =( BOUNDED_CURVE ( )  B_SPLINE_CURVE ( 2, ( #141244, #157465, #176902, #56748, #108767, #90322, #61014, #24220, #205106 ),
 .UNSPECIFIED., .F., .T. ) 
 B_SPLINE_CURVE_WITH_KNOTS ( ( 3, 2, 2, 2, 3 ),
 ( 0.5781250000000001110, 0.5833333333333333703, 0.5937500000000000000, 0.6041666666666666297, 0.6093749999999997780 ),
 .UNSPECIFIED. ) 
 CURVE ( )  GEOMETRIC_REPRESENTATION_ITEM ( )  RATIONAL_B_SPLINE_CURVE ( ( 0.9330127018922192983, 0.9330127018922207416, 1.000000000000000000, 0.8660254037844387076, 1.000000000000000000, 0.8660254037844387076, 1.000000000000000000, 0.9330127018922221849, 0.9330127018922194093 ) ) 
 REPRESENTATION_ITEM ( '' )  );
#171255 = ORIENTED_EDGE ( 'NONE', *, *, #88039, .T. ) ;
#171256 = CARTESIAN_POINT ( 'NONE',  ( 2.647004975520852454, -0.3514972095969396970, -2.040143077068845123 ) ) ;
#171258 = CARTESIAN_POINT ( 'NONE',  ( 0.7499999999999920064, 4.483333333333352932, 1.299038105676669330 ) ) ;
#171257 = AXIS2_PLACEMENT_3D ( 'NONE', #119168, #169979, #184096 ) ;
#171259 = CARTESIAN_POINT ( 'NONE',  ( 4.202137545231717120, 6.989912005157271402, 1.199719254218462483 ) ) ;
#171260 = CARTESIAN_POINT ( 'NONE',  ( -6.601093878019091754, 6.767222581227101408, 0.2246719935465150975 ) ) ;
#171261 = CARTESIAN_POINT ( 'NONE',  ( 0.8737014391667098367, 0.3917534382160395290, -1.981132022265948756 ) ) ;
#171262 = B_SPLINE_CURVE_WITH_KNOTS ( 'NONE', 3,
 ( #110304, #143850, #45252, #98257, #81987, #49495, #181611, #64674, #164314, #1781, #65708 ),
 .UNSPECIFIED., .F., .F.,
 ( 4, 1, 1, 1, 1, 1, 1, 1, 4 ),
 ( 0.000000000000000000, 0.2254494161556361009, 0.3971188491599597081, 0.5240836380151728813, 0.6154273167216615104, 0.6803253696226415626, 0.7282602231486813293, 0.7688932809586735972, 1.000000000000000000 ),
 .UNSPECIFIED. ) ;
#171263 = CARTESIAN_POINT ( 'NONE',  ( -1.001543065824772872E-14, 4.321875000341417916, 1.575800808251672791 ) ) ;
#171264 = ORIENTED_EDGE ( 'NONE', *, *, #138892, .T. ) ;
#171266 = CARTESIAN_POINT ( 'NONE',  ( 9.463228032658635769, 11.10314946193233965, -1.082531754730543083 ) ) ;
#171265 = CARTESIAN_POINT ( 'NONE',  ( 0.07459516483343267557, 2.058153987855536382, -2.173125978204577535 ) ) ;
#171267 = CARTESIAN_POINT ( 'NONE',  ( 5.255232437486731634, -2.000551055875991580, -0.2495666058281582056 ) ) ;
#171268 = CARTESIAN_POINT ( 'NONE',  ( 6.210162240821837543, 1.096913934394160517, -1.570407731631766390 ) ) ;
#171269 = LINE ( 'NONE', #25013, #34430 ) ;
#171270 = CARTESIAN_POINT ( 'NONE',  ( 3.737968522918270864, 2.181131050170285857, 0.2133239450496857148 ) ) ;
#171271 =( BOUNDED_CURVE ( )  B_SPLINE_CURVE ( 2, ( #188391, #206771, #139681, #109359, #190518, #159098, #41109 ),
 .UNSPECIFIED., .F., .T. ) 
 B_SPLINE_CURVE_WITH_KNOTS ( ( 3, 2, 2, 3 ),
 ( 0.01785714285714263064, 0.02380952380952366942, 0.02976190476190470821, 0.03571428571428574700 ),
 .UNSPECIFIED. ) 
 CURVE ( )  GEOMETRIC_REPRESENTATION_ITEM ( )  RATIONAL_B_SPLINE_CURVE ( ( 1.000000000000005107, 0.8660254037844337116, 1.000000000000000000, 0.8660254037844387076, 1.000000000000000000, 0.8660254037844379305, 1.000000000000000666 ) ) 
 REPRESENTATION_ITEM ( '' )  );
#171272 = CARTESIAN_POINT ( 'NONE',  ( -1.402160292154681736E-14, 1.618750000682814827, -1.732050807568863648 ) ) ;
#171273 = CARTESIAN_POINT ( 'NONE',  ( 2.162237915172473546, 1.912057200688283665, 0.04323261116381121871 ) ) ;
#171274 = CARTESIAN_POINT ( 'NONE',  ( -5.904739593951539689, 6.847616600153594746, 1.199719254218450271 ) ) ;
#171275 = CARTESIAN_POINT ( 'NONE',  ( 4.568734577680873876, 6.353276312092901890, -1.443375672974051449 ) ) ;
#171277 = CARTESIAN_POINT ( 'NONE',  ( 0.5269705342763851830, -1.727990693721896287, 1.039014695730144933 ) ) ;
#171276 = DIRECTION ( 'NONE',  ( -0.5265943820692667865, 0.4485553919953594315, -0.7221470882617865295 ) ) ;
#171278 = CARTESIAN_POINT ( 'NONE',  ( 1.364683531249996529, 10.77604166700806765, 0.7879004041258405033 ) ) ;
#171280 = CARTESIAN_POINT ( 'NONE',  ( -4.606738333593328072, 8.596554832492683929, 0.7998128361456281477 ) ) ;
#171279 = CARTESIAN_POINT ( 'NONE',  ( 6.620655732516649294, -0.002413161512292843602, 2.173887093218459743 ) ) ;
#171282 = ORIENTED_EDGE ( 'NONE', *, *, #154124, .T. ) ;
#171281 = CARTESIAN_POINT ( 'NONE',  ( 2.696000938853719830, -1.719994558248700844, -0.1292177092697097962 ) ) ;
#171283 = PRESENTATION_STYLE_ASSIGNMENT (( #119403 ) ) ;
#171284 = CARTESIAN_POINT ( 'NONE',  ( 8.457588896826466751, 8.761608555919362828, 1.040834085586084257E-14 ) ) ;
#171285 = CARTESIAN_POINT ( 'NONE',  ( 5.281064527722868718, 6.119995689553514140, 1.199719254218462483 ) ) ;
#171286 = FILL_AREA_STYLE_COLOUR ( '', #71373 ) ;
#171287 = CARTESIAN_POINT ( 'NONE',  ( 1.464175926609780964E-14, -2.493749999044085452, -3.475000000000000533 ) ) ;
#171288 =( BOUNDED_CURVE ( )  B_SPLINE_CURVE ( 2, ( #186648, #171473, #38274, #73976, #119590, #106527, #140071, #206095, #88093, #155231, #187712, #123886, #8970, #157375, #104351, #20924, #136853, #87020, #6812, #170396, #189852, #91318, #172553, #72890, #153092, #4667, #173641, #202877, #75044, #120670, #185573, #37203, #71811, #54525, #103277, #203942, #39341, #208224, #177891, #175760, #181842, #12168, #198100, #11091, #110809, #210363, #95597, #77168, #176814, #128159, #28429, #160560, #78240, #26278, #190908, #59856, #132091 ),
 .UNSPECIFIED., .F., .T. ) 
 B_SPLINE_CURVE_WITH_KNOTS ( ( 3, 2, 2, 2, 2, 2, 2, 2, 2, 2, 2, 2, 2, 2, 2, 2, 2, 2, 2, 2, 2, 2, 2, 2, 2, 2, 2, 2, 3 ),
 ( 0.2844739210328576795, 0.2916666666666666852, 0.2999999999999999889, 0.3083333333333333481, 0.3166666666666666519, 0.3250000000000000111, 0.3333333333333333148, 0.3416666666666666741, 0.3499999999999999778, 0.3583333333333333370, 0.3666666666666666408, 0.3750000000000000000, 0.3833333333333333592, 0.3916666666666666630, 0.4000000000000000222, 0.4083333333333333259, 0.4166666666666666852, 0.4249999999999999889, 0.4333333333333333481, 0.4416666666666666519, 0.4500000000000000111, 0.4583333333333333148, 0.4666666666666666741, 0.4749999999999999778, 0.4833333333333333370, 0.4916666666666666408, 0.5000000000000000000, 0.5083333333333333037, 0.5119843065236711066 ),
 .UNSPECIFIED. ) 
 CURVE ( )  GEOMETRIC_REPRESENTATION_ITEM ( )  RATIONAL_B_SPLINE_CURVE ( ( 0.9683452906431710971, 0.8843625769635039546, 1.000000000000000000, 0.8660254037844387076, 1.000000000000000000, 0.8660254037844387076, 1.000000000000000000, 0.8660254037844387076, 1.000000000000000000, 0.8660254037844387076, 1.000000000000000000, 0.8660254037844387076, 1.000000000000000000, 0.8660254037844387076, 1.000000000000000000, 0.8660254037844387076, 1.000000000000000000, 0.8660254037844387076, 1.000000000000000000, 0.8660254037844387076, 1.000000000000000000, 0.8660254037844387076, 1.000000000000000000, 0.8660254037844387076, 1.000000000000000000, 0.8660254037844387076, 1.000000000000000000, 0.8660254037844387076, 1.000000000000000000, 0.8660254037844387076, 1.000000000000000000, 0.8660254037844387076, 1.000000000000000000, 0.8660254037844387076, 1.000000000000000000, 0.8660254037844387076, 1.000000000000000000, 0.8660254037844387076, 1.000000000000000000, 0.8660254037844387076, 1.000000000000000000, 0.8660254037844387076, 1.000000000000000000, 0.8660254037844387076, 1.000000000000000000, 0.8660254037844387076, 1.000000000000000000, 0.8660254037844387076, 1.000000000000000000, 0.8660254037844387076, 1.000000000000000000, 0.8660254037844387076, 1.000000000000000000, 0.8660254037844387076, 1.000000000000000000, 0.9413034809236788814, 0.9340388220506692374 ) ) 
 REPRESENTATION_ITEM ( '' )  );
#171289 = CARTESIAN_POINT ( 'NONE',  ( 0.000000000000000000, 0.000000000000000000, 2.000000000000000000 ) ) ;
#171290 = CARTESIAN_POINT ( 'NONE',  ( 4.821896187954575197, 8.777295985922343391, 0.7998128361456462443 ) ) ;
#171291 = CARTESIAN_POINT ( 'NONE',  ( -4.874313559192080092, 4.961021341527962036, 0.5169845646830675268 ) ) ;
#171292 = DIRECTION ( 'NONE',  ( -0.2275915169919967007, 0.8825604524983418075, -0.4114476261679050340 ) ) ;
#171293 = EDGE_LOOP ( 'NONE', ( #11079, #165940, #155902, #139887 ) ) ;
#171294 = CARTESIAN_POINT ( 'NONE',  ( 2.877393275988342047, 0.2635569349610377143, -1.792047384982973890 ) ) ;
#171295 = VECTOR ( 'NONE', #88960, 1000.000000000000000 ) ;
#171296 = VERTEX_POINT ( 'NONE', #132696 ) ;
#171297 = CARTESIAN_POINT ( 'NONE',  ( 9.999301985278609806, 11.62460605670194447, 1.199719254218452047 ) ) ;
#171298 = CARTESIAN_POINT ( 'NONE',  ( 4.329849954717849947, 6.144853928627882489, 1.599625672291262513 ) ) ;
#171299 = CARTESIAN_POINT ( 'NONE',  ( 3.668453237830204827, 0.6552377326864079476, 1.688991677562341920 ) ) ;
#171300 = CARTESIAN_POINT ( 'NONE',  ( 7.661766205054107992, 8.111351125417501251, -0.7216878364870317197 ) ) ;
#171301 = CARTESIAN_POINT ( 'NONE',  ( 5.094532678321557206, 4.917790403868676385, -0.1305349544365452807 ) ) ;
#171302 = CARTESIAN_POINT ( 'NONE',  ( 5.804557637360799660, 6.030435022130575362, 0.4940411958238543066 ) ) ;
#171304 = CARTESIAN_POINT ( 'NONE',  ( -1.364683531250014514, 14.08854166700806942, -0.7879004041258335089 ) ) ;
#171303 = CARTESIAN_POINT ( 'NONE',  ( 5.564867526603252124, 1.409050971242819417, -1.215897700512589052 ) ) ;
#171305 = CARTESIAN_POINT ( 'NONE',  ( 3.040549542926245241, -1.448533627684518654, 1.253585735969472648 ) ) ;
#171306 = CARTESIAN_POINT ( 'NONE',  ( -11.19349454483825212, 5.612381422204108183, 3.868266946477203927 ) ) ;
#171307 = CARTESIAN_POINT ( 'NONE',  ( -6.329176825324663191, 6.889957431341297678, 0.7450545735031323114 ) ) ;
#171308 = CARTESIAN_POINT ( 'NONE',  ( 6.925078400183548588, 2.417948008941684268, 2.525058136801380027 ) ) ;
#171309 = CARTESIAN_POINT ( 'NONE',  ( 6.100805936469477331, 9.101062111647635788, -1.082531754730537088 ) ) ;
#171310 = CARTESIAN_POINT ( 'NONE',  ( -4.009460741339347045, 5.700790169694431420, -1.599625672291256295 ) ) ;
#171311 = CARTESIAN_POINT ( 'NONE',  ( -9.499700864329913230, -7.154544010627095219, -0.07538891330674860058 ) ) ;
#171312 = CARTESIAN_POINT ( 'NONE',  ( 1.394599547902091174, 1.708230453586807585, -1.204993862942314031 ) ) ;
#171313 = CARTESIAN_POINT ( 'NONE',  ( 5.825163275726873202, 6.825053905550038991, 1.199719254218452047 ) ) ;
#171314 = CARTESIAN_POINT ( 'NONE',  ( 6.352563997503644977, 0.6048113787208497794, 1.829064924511276002 ) ) ;
#171315 = CARTESIAN_POINT ( 'NONE',  ( -3.958090780185743451, 6.705190779270287393, -1.199719254218452047 ) ) ;
#171316 = CARTESIAN_POINT ( 'NONE',  ( 1.940199132888191791, 1.805219978825555627, 0.2711003711317952480 ) ) ;
#171317 = CARTESIAN_POINT ( 'NONE',  ( 1.408750476333323176, 7.229967155398369982, -4.273289540531086672 ) ) ;
#171318 = CARTESIAN_POINT ( 'NONE',  ( 0.9141475326900462273, -1.912571728325639153, 0.002704284578637640348 ) ) ;
#171319 = CARTESIAN_POINT ( 'NONE',  ( 1.293335457286367784, -1.782033794834203766, 0.8390149815750718165 ) ) ;
#171320 = CARTESIAN_POINT ( 'NONE',  ( 4.159667821157567502, 0.9185609468507827113, 1.711114809252372915 ) ) ;
#171321 = ORIENTED_EDGE ( 'NONE', *, *, #76523, .T. ) ;
#171322 = LINE ( 'NONE', #157231, #33237 ) ;
#171324 = CARTESIAN_POINT ( 'NONE',  ( 6.737149535461696814, -0.09068363363158969681, -1.858830251952103385 ) ) ;
#171323 = CARTESIAN_POINT ( 'NONE',  ( -3.305155586681401303, 7.078041627762083898, 0.7998128361456352531 ) ) ;
#171326 = CARTESIAN_POINT ( 'NONE',  ( 3.990573222356631256, -1.218298518170106925, 1.735533685479621502 ) ) ;
#171325 = CARTESIAN_POINT ( 'NONE',  ( 3.237364818613055473, 6.998952398349030268, -1.734723475976807094E-15 ) ) ;
#171327 = CARTESIAN_POINT ( 'NONE',  ( -2.722740351562989813E-16, -7.550885189219943783, 9.573337995800487832 ) ) ;
#171328 = CARTESIAN_POINT ( 'NONE',  ( 9.582915646760733708, 10.07448976417602893, 0.7998128361456462443 ) ) ;
#171329 = CARTESIAN_POINT ( 'NONE',  ( -5.586841817283045408, 8.675676665875643678, 1.199719254218454489 ) ) ;
#171330 = CARTESIAN_POINT ( 'NONE',  ( -11.00605293250196226, 9.990747386415566922, -1.443095658425808114 ) ) ;
#171331 = ORIENTED_EDGE ( 'NONE', *, *, #113687, .F. ) ;
#171332 = CARTESIAN_POINT ( 'NONE',  ( 5.176180785367283654, 9.260904359562321275, -0.7998128361456481317 ) ) ;
#171333 = CARTESIAN_POINT ( 'NONE',  ( 3.913815762669449416, 7.330443837381343641, -0.8582294057540799104 ) ) ;
#171334 = CARTESIAN_POINT ( 'NONE',  ( 4.353998665852670591, 1.825246345946249571, -0.04724550102237072557 ) ) ;
#171335 = CARTESIAN_POINT ( 'NONE',  ( -0.4019237886466933696, 13.08258545099817027, 1.500000000000005995 ) ) ;
#171336 = CARTESIAN_POINT ( 'NONE',  ( -10.30383355670593737, 11.12348669235284504, -0.7216878364870267237 ) ) ;
#171337 =( BOUNDED_SURFACE ( )  B_SPLINE_SURFACE ( 3, 2, ( 
 ( #46485, #163434, #81103 ),
 ( #126743, #176479, #147191 ),
 ( #213216, #211086, #144022 ),
 ( #95250, #30229, #195929 ),
 ( #13949, #160226, #64846 ),
 ( #29159, #80032, #111542 ),
 ( #164490, #130992, #47567 ),
 ( #113678, #212148, #62709 ),
 ( #192702, #210016, #28090 ),
 ( #127826, #78961, #128870 ) ),
 .UNSPECIFIED., .F., .F., .T. ) 
 B_SPLINE_SURFACE_WITH_KNOTS ( ( 4, 2, 2, 2, 4 ),
 ( 3, 3 ),
 ( 0.001823084239704076889, 0.002278855299642388362, 0.002734626359580699835, 0.003190397419519010874, 0.003646168479457322347 ),
 ( 0.000000000000000000, 1.000000000000000000 ),
 .UNSPECIFIED. ) 
 GEOMETRIC_REPRESENTATION_ITEM ( )  RATIONAL_B_SPLINE_SURFACE ( (
 ( 1.000000000000000000, 0.8275596917163435817, 1.000000000000000000),
 ( 1.000000000000000000, 0.8320789365404243076, 1.000000000000000000),
 ( 1.000000000000000000, 0.8266768160090710582, 1.000000000000000000),
 ( 1.000000000000000000, 0.7938580293400921972, 1.000000000000000000),
 ( 1.000000000000000000, 0.7658694575135178706, 1.000000000000000000),
 ( 1.000000000000000000, 0.6964599583665085358, 1.000000000000000000),
 ( 1.000000000000000000, 0.6553951921932222868, 1.000000000000000000),
 ( 1.000000000000000000, 0.5911026409457650344, 1.000000000000000000),
 ( 1.000000000000000000, 0.5677445233671155611, 1.000000000000000000),
 ( 1.000000000000000000, 0.5613739026647618369, 1.000000000000000000) ) ) 
 REPRESENTATION_ITEM ( '' )  SURFACE ( )  );
#171338 = CARTESIAN_POINT ( 'NONE',  ( -4.688377817131518910, 8.372325690950924937, 0.6434091164432588217 ) ) ;
#171339 = DIRECTION ( 'NONE',  ( 1.000000000000000000, 0.000000000000000000, 0.000000000000000000 ) ) ;
#171340 = CARTESIAN_POINT ( 'NONE',  ( 5.032044620589739559, 0.9611010790777809731, -1.604743002217932313 ) ) ;
#171341 = CARTESIAN_POINT ( 'NONE',  ( 7.995557903757111617, 10.35123685918189729, 1.599625672291281386 ) ) ;
#171342 = CARTESIAN_POINT ( 'NONE',  ( 1.629391185616009707, -1.814203104720218951, 0.6484763462606003559 ) ) ;
#171343 = CARTESIAN_POINT ( 'NONE',  ( 6.596542563702321615, 1.939940506139478327, 0.2910815776849539627 ) ) ;
#171344 = EDGE_CURVE ( 'NONE', #175693, #65271, #198703, .T. ) ;
#171345 = CARTESIAN_POINT ( 'NONE',  ( -1.364683531250010295, 8.442708333674730170, 0.7879004041258445001 ) ) ;
#171346 = CARTESIAN_POINT ( 'NONE',  ( -5.280010757518168063, 8.247430752824802980, -1.199719254218446718 ) ) ;
#171347 = CARTESIAN_POINT ( 'NONE',  ( 3.497113557321089861, 6.167384019261527683, -1.199719254218446718 ) ) ;
#171348 = ADVANCED_FACE ( 'NONE', ( #35140 ), #1560, .F. ) ;
#171349 = CARTESIAN_POINT ( 'NONE',  ( -3.621436428181653788, 7.239109909604962922, 0.7216878364870338292 ) ) ;
#171350 = VECTOR ( 'NONE', #165844, 1000.000000000000000 ) ;
#171351 = CARTESIAN_POINT ( 'NONE',  ( 6.421125127611838401, -1.890376142121247494, 0.9539971363903186896 ) ) ;
#171352 = CARTESIAN_POINT ( 'NONE',  ( 8.920375002787457319, 12.49452237230570084, 1.199719254218450271 ) ) ;
#171353 = CARTESIAN_POINT ( 'NONE',  ( -1.288108131580338211, -0.9841229182759280159, 3.227445187970915619 ) ) ;
#171354 = CARTESIAN_POINT ( 'NONE',  ( 5.084861876562203342, 1.979495018489594305, 0.6061691862097525751 ) ) ;
#171356 = CARTESIAN_POINT ( 'NONE',  ( 1.364683531249988535, 2.426041667008088432, 0.7879004041258500513 ) ) ;
#171355 = CARTESIAN_POINT ( 'NONE',  ( 0.2922019606856861018, 1.531309713818730822, -1.022077305420886040 ) ) ;
#171357 = CARTESIAN_POINT ( 'NONE',  ( 4.975319123388493914, -2.281077821084981583, -0.2834334243917625562 ) ) ;
#171358 = CARTESIAN_POINT ( 'NONE',  ( 7.321039761699430493, 7.643560598178549270, -0.7216878364870257245 ) ) ;
#171360 = CARTESIAN_POINT ( 'NONE',  ( 7.462104991928526054, -5.166862915010159263, 8.081892667527535323 ) ) ;
#171359 = CARTESIAN_POINT ( 'NONE',  ( 2.943528747942701695, 6.448217615992859919, 0.000000000000000000 ) ) ;
#171361 = CARTESIAN_POINT ( 'NONE',  ( 0.8500709472824579116, 2.289359419033740295, -0.1177234237379476411 ) ) ;
#171362 = CARTESIAN_POINT ( 'NONE',  ( 10.91944002402979130, -9.900000000000005684, -0.1105873483556608222 ) ) ;
#171363 = CARTESIAN_POINT ( 'NONE',  ( -6.261886844665283114, 8.398896966899865646, 1.599625672291269396 ) ) ;
#171364 = CARTESIAN_POINT ( 'NONE',  ( 5.331954954513311584, 1.913531179151845674, 0.3301462080481341599 ) ) ;
#171365 = EDGE_LOOP ( 'NONE', ( #136158, #135527, #52491, #62872 ) ) ;
#171367 = EDGE_CURVE ( 'NONE', #188409, #130695, #7392, .T. ) ;
#171366 = CARTESIAN_POINT ( 'NONE',  ( 8.310784975052673218, 10.71900177569337487, -1.443375672974063439 ) ) ;
#171368 = ORIENTED_EDGE ( 'NONE', *, *, #56480, .T. ) ;
#171369 = CARTESIAN_POINT ( 'NONE',  ( 5.836178160628028522, -1.067892152678026951, -1.586260290404594597 ) ) ;
#171370 = CARTESIAN_POINT ( 'NONE',  ( 5.823453932400854960, -1.463924103857511039, -1.387103351090559933 ) ) ;
#171372 = CARTESIAN_POINT ( 'NONE',  ( -1.271070482942027180, 8.436788551174039696, -10.93994114196923384 ) ) ;
#171371 = CARTESIAN_POINT ( 'NONE',  ( -7.506410603460441422, 11.90922947067921278, -0.7998128361456291469 ) ) ;
#171373 = CARTESIAN_POINT ( 'NONE',  ( 3.285556943750000514, -2.151041666188709733, 1.896917185911906500 ) ) ;
#171375 = CARTESIAN_POINT ( 'NONE',  ( 1.480939207288126669, 1.637052324538622816, -0.6731226676765161843 ) ) ;
#171374 = CARTESIAN_POINT ( 'NONE',  ( 2.449268230884271702, 0.5568478702235891697, -2.015041263885499756 ) ) ;
#171376 = CARTESIAN_POINT ( 'NONE',  ( -0.4294077647110545737, -6.532648833121157850, -9.469892045836658667 ) ) ;
#171377 = B_SPLINE_CURVE_WITH_KNOTS ( 'NONE', 3,
 ( #145795, #82871, #97031, #160943, #78609, #194497 ),
 .UNSPECIFIED., .F., .F.,
 ( 4, 2, 4 ),
 ( 0.000000000000000000, 0.002110194456903486098, 0.004220388913806971329 ),
 .UNSPECIFIED. ) ;
#171379 = CARTESIAN_POINT ( 'NONE',  ( 4.453268702153020620, 0.5046191974597475927, -2.235886964606835559 ) ) ;
#171378 = CARTESIAN_POINT ( 'NONE',  ( 4.435452530326143616, 5.203724702582467998, -1.199719254218452047 ) ) ;
#171380 = CARTESIAN_POINT ( 'NONE',  ( 2.255425419672125287, 0.7431408456733903378, 1.573829366573131328 ) ) ;
#171381 = CARTESIAN_POINT ( 'NONE',  ( 3.517450787741589036, 6.191110788085444128, -1.199719254218446718 ) ) ;
#171382 = CARTESIAN_POINT ( 'NONE',  ( -4.880762754383670021, 4.880089465954365657, -0.6148759978819359207 ) ) ;
#171383 = CARTESIAN_POINT ( 'NONE',  ( 2.090756734626127766, 1.002568922338117563, -1.414341044747928766 ) ) ;
#171384 = CARTESIAN_POINT ( 'NONE',  ( -0.6801582343750229853, 1.380208333674720622, -1.178068619123855409 ) ) ;
#171385 = CARTESIAN_POINT ( 'NONE',  ( 1.697469458906812667, -1.344883679737416404, -1.286638954052413908 ) ) ;
#171386 = CARTESIAN_POINT ( 'NONE',  ( 2.119799831544411095, 0.3726140298815834861, -2.138824928699584405 ) ) ;
#171387 = CARTESIAN_POINT ( 'NONE',  ( 5.392392409933256303, 7.314210449720692786, 1.599625672291267398 ) ) ;
#171388 = CARTESIAN_POINT ( 'NONE',  ( 4.469935555517978720, -0.9463019959239076240, 1.780667052345537238 ) ) ;
#171389 = CARTESIAN_POINT ( 'NONE',  ( 2.656250000000001332, -1.895863743164027504, 0.7852924748301256530 ) ) ;
#171390 = CARTESIAN_POINT ( 'NONE',  ( 0.7499999999999885647, 3.347916667349487341, -1.299038105676658228 ) ) ;
#171391 = CARTESIAN_POINT ( 'NONE',  ( 0.9735099972556484627, 1.857407184102148001, -0.5107058244425541904 ) ) ;
#171392 = CARTESIAN_POINT ( 'NONE',  ( -0.6823417656250039265, 13.81770833367473195, -1.181850606188755259 ) ) ;
#171393 = CARTESIAN_POINT ( 'NONE',  ( 4.922253396635227318, -2.210645704158546554, 0.2187456033138199529 ) ) ;
#171394 = ORIENTED_EDGE ( 'NONE', *, *, #138645, .T. ) ;
#171395 = CARTESIAN_POINT ( 'NONE',  ( -0.2110808730066960626, 4.094899759311981136, -2.352064028521171135 ) ) ;
#171396 = CARTESIAN_POINT ( 'NONE',  ( 0.7499999999999885647, 0.5666666666666875241, -1.299038105676652899 ) ) ;
#171398 = ADVANCED_FACE ( 'NONE', ( #134820 ), #118603, .T. ) ;
#171397 = CARTESIAN_POINT ( 'NONE',  ( 6.479907352327590964, 9.647310113435821677, 1.199719254218462483 ) ) ;
#171399 = CARTESIAN_POINT ( 'NONE',  ( -1.364683531250014514, -0.7197916663252461600, 0.7879004041258379498 ) ) ;
#171400 = CARTESIAN_POINT ( 'NONE',  ( 0.1357878378635381522, -0.1024811726445598314, 2.219055157331132566 ) ) ;
#171401 = CARTESIAN_POINT ( 'NONE',  ( 5.266048140081638351, -1.952571265509401854, 0.1905133553196102503 ) ) ;
#171402 = CARTESIAN_POINT ( 'NONE',  ( 8.920901888111986366, 12.39117405523060889, 1.082531754730546636 ) ) ;
#171403 = FACE_OUTER_BOUND ( 'NONE', #139372, .T. ) ;
#171404 = CARTESIAN_POINT ( 'NONE',  ( 6.919229411136463170, -0.1667645622517479609, 2.226262756130835463 ) ) ;
#171405 = CIRCLE ( 'NONE', #19094, 0.5000000000000015543 ) ;
#171406 = CARTESIAN_POINT ( 'NONE',  ( -4.014622883422329203, 6.737458226417744278, -1.082531754730546636 ) ) ;
#171407 = CARTESIAN_POINT ( 'NONE',  ( 3.051292873657907023, 1.770411945740796966, -1.058192539780268282 ) ) ;
#171408 = CARTESIAN_POINT ( 'NONE',  ( -6.501298352952815662, 7.543601818988450169, -1.199719254218446718 ) ) ;
#171409 = VECTOR ( 'NONE', #127732, 1000.000000000000000 ) ;
#171411 = EDGE_CURVE ( 'NONE', #43349, #56038, #152116, .T. ) ;
#171410 = CARTESIAN_POINT ( 'NONE',  ( -1.201851678989727383E-14, 2.993750000682821266, 1.732050807568877637 ) ) ;
#171412 = CARTESIAN_POINT ( 'NONE',  ( 0.6823417656249864960, -1.073958332991911568, -1.181850606188749264 ) ) ;
#171413 = CARTESIAN_POINT ( 'NONE',  ( 4.516781199771729760, 1.709404882366181377, 0.7599583452636837766 ) ) ;
#171414 = CARTESIAN_POINT ( 'NONE',  ( 3.515997504735939305, -1.600726479906929844, 0.6675610986628178756 ) ) ;
#171415 = CARTESIAN_POINT ( 'NONE',  ( 3.878220372009810291, -0.1751146298830832670, -1.731616844506628006 ) ) ;
#171416 = CARTESIAN_POINT ( 'NONE',  ( 0.4336627441306003528, -1.626622142924066594, -1.615526755278140492 ) ) ;
#171417 = CARTESIAN_POINT ( 'NONE',  ( -1.201851678989727383E-14, 4.009375000341416140, -1.575800808251660134 ) ) ;
#171418 = CARTESIAN_POINT ( 'NONE',  ( 4.985920054561153059, -2.075123007882358817, -0.2543892858761549469 ) ) ;
#171419 = CARTESIAN_POINT ( 'NONE',  ( 5.349535142863500070, 1.939630122921351729, -0.09734604192479337503 ) ) ;
#171420 = EDGE_CURVE ( 'NONE', #126440, #94296, #114281, .T. ) ;
#171422 = ORIENTED_EDGE ( 'NONE', *, *, #162356, .T. ) ;
#171421 = CARTESIAN_POINT ( 'NONE',  ( 8.874816357151750879, 14.67092918096089527, 8.013384896292299331 ) ) ;
#171423 =( LENGTH_UNIT ( ) NAMED_UNIT ( * ) SI_UNIT ( .MILLI., .METRE. ) );
#171424 = CARTESIAN_POINT ( 'NONE',  ( 0.8971115437808926396, -0.9091470795906559932, -1.799921601489597123 ) ) ;
#171425 = CARTESIAN_POINT ( 'NONE',  ( 0.9144942500491148873, -2.120778211678171488, 0.005759991200282587286 ) ) ;
#171426 = CARTESIAN_POINT ( 'NONE',  ( 6.293592298849589817, 1.492257802130890765, -1.356297202127904944 ) ) ;
#171427 = CARTESIAN_POINT ( 'NONE',  ( -7.985916173649233230, 9.275655943134292869, -1.199719254218446718 ) ) ;
#171428 = CARTESIAN_POINT ( 'NONE',  ( 5.035963992472171746, 7.962709526937818083, 1.199719254218462483 ) ) ;
#171429 = CARTESIAN_POINT ( 'NONE',  ( 2.754661888675050019, 2.104750880745378083, 0.2572054321872129790 ) ) ;
#171430 = ADVANCED_BREP_SHAPE_REPRESENTATION ( '', ( #87643, #200407 ), #135205 ) ;
#171431 = CARTESIAN_POINT ( 'NONE',  ( 4.107882937833263526, -1.820653182827164596, 0.1363937739093170898 ) ) ;
#171432 = ORIENTED_EDGE ( 'NONE', *, *, #194419, .T. ) ;
#171433 = CARTESIAN_POINT ( 'NONE',  ( -7.957709816578236506, 8.248692638954882028, 0.7998128361456341429 ) ) ;
#171434 = DIRECTION ( 'NONE',  ( 0.000000000000000000, 0.000000000000000000, -1.000000000000000000 ) ) ;
#171435 = CARTESIAN_POINT ( 'NONE',  ( -3.285556943749998737, -0.5177083328553757635, 1.896917185911908499 ) ) ;
#171436 = CARTESIAN_POINT ( 'NONE',  ( -5.669280788808708671, 9.765911353585494226, 0.7998128361456481317 ) ) ;
#171437 = CARTESIAN_POINT ( 'NONE',  ( 2.285421205933793942, 0.09476354472776055138, -2.017669629103500117 ) ) ;
#171438 = CARTESIAN_POINT ( 'NONE',  ( 5.421004802376033993, 2.037064969303593820, 0.8491359902737596332 ) ) ;
#171439 = CARTESIAN_POINT ( 'NONE',  ( -5.957882158562513908, 5.915560371269843465, -0.7998128361456362523 ) ) ;
#171440 = CARTESIAN_POINT ( 'NONE',  ( 3.186215892106421421, 1.037744835847534741, -1.544512256342661427 ) ) ;
#171441 = CARTESIAN_POINT ( 'NONE',  ( 8.380911511541880188, 12.92948053010758258, 0.7998128361456462443 ) ) ;
#171442 = CARTESIAN_POINT ( 'NONE',  ( 10.51595811585101004, 12.48659653991854945, -3.553980774159643197 ) ) ;
#171443 = VERTEX_POINT ( 'NONE', #91404 ) ;
#171444 = CARTESIAN_POINT ( 'NONE',  ( -4.711622075948912247, 5.455646162483875017, -1.199719254218446718 ) ) ;
#171445 = CARTESIAN_POINT ( 'NONE',  ( -9.345647958521597687, 9.797677461230342999, 0.7998128361456462443 ) ) ;
#171446 = CARTESIAN_POINT ( 'NONE',  ( 4.564971734551386717, -1.632036996880025903, -0.8184370388232551363 ) ) ;
#171447 = VECTOR ( 'NONE', #59968, 1000.000000000000000 ) ;
#171449 = CARTESIAN_POINT ( 'NONE',  ( -4.432925279414208219, 7.308574008990986748, -1.253226476263115341 ) ) ;
#171448 = CARTESIAN_POINT ( 'NONE',  ( -3.492107083971660586, 6.231819477012331632, 1.199719254218452935 ) ) ;
#171450 = CARTESIAN_POINT ( 'NONE',  ( 6.480989489388473856, 6.848452138476523565, -0.6157061703677743081 ) ) ;
#171451 = CARTESIAN_POINT ( 'NONE',  ( 1.000851265249177890, 1.706856028473648257, 0.3036596661522768525 ) ) ;
#171452 = CARTESIAN_POINT ( 'NONE',  ( 0.3393031230796061948, 1.735299727462248587, 0.1329522994921657764 ) ) ;
#171453 = CARTESIAN_POINT ( 'NONE',  ( 5.760475268203285815, 0.9300522481428794563, 2.112166060234192511 ) ) ;
#171454 = CARTESIAN_POINT ( 'NONE',  ( 5.228604516725597229, 6.129068686715179126, -1.199719254218450271 ) ) ;
#171455 = CARTESIAN_POINT ( 'NONE',  ( 0.7552377862659557239, -1.739527406477459515, -1.104632168941059867 ) ) ;
#171456 = CARTESIAN_POINT ( 'NONE',  ( 6.440286661691305703, 7.472421512516709718, 1.199719254218462483 ) ) ;
#171457 = CARTESIAN_POINT ( 'NONE',  ( 5.185072832991014735, -1.223605693886620438, -1.945460884747321151 ) ) ;
#171458 = CARTESIAN_POINT ( 'NONE',  ( 11.00006988736402036, -9.999999999999994671, -0.09199170129443705324 ) ) ;
#171459 = CARTESIAN_POINT ( 'NONE',  ( -6.394605727500880299, 7.489403432619674561, -1.199719254218452047 ) ) ;
#171460 = CARTESIAN_POINT ( 'NONE',  ( 5.893391625361731556, 1.417579469995243091, 1.220656814419220249 ) ) ;
#171461 = PRESENTATION_LAYER_ASSIGNMENT (  '', '', ( #50392 ) ) ;
#171463 = CARTESIAN_POINT ( 'NONE',  ( -4.981695098378565945, 4.776675467721892332, -0.7998128361456362523 ) ) ;
#171462 = CARTESIAN_POINT ( 'NONE',  ( 2.988426722125224977, -1.135634098421594240, 1.538566774472991616 ) ) ;
#171464 = CARTESIAN_POINT ( 'NONE',  ( 5.215527394842717435, -0.3265260713646127022, 2.182469266582609091 ) ) ;
#171465 = CARTESIAN_POINT ( 'NONE',  ( 4.206348283080693307, 1.299600563804912623, -1.671539989125019332 ) ) ;
#171466 = CARTESIAN_POINT ( 'NONE',  ( -1.352083138863443345E-14, 1.500000000682843115, -1.414508159514601626 ) ) ;
#171467 = CARTESIAN_POINT ( 'NONE',  ( 6.883263157960399781, 2.970623603138924818, 2.399364662246627589 ) ) ;
#171468 = CARTESIAN_POINT ( 'NONE',  ( 4.706088717274895750, 6.583799151611112954, 1.443375672974065660 ) ) ;
#171469 = CARTESIAN_POINT ( 'NONE',  ( -4.733205024502264102, 7.575804057677677505, 1.082531754730549967 ) ) ;
#171470 = CARTESIAN_POINT ( 'NONE',  ( 5.567072742743464531, -1.671543079161823542, 1.304629437388994395 ) ) ;
#171471 = CARTESIAN_POINT ( 'NONE',  ( 2.731810774274369802, -2.153386645068070759, 0.8298372035008163561 ) ) ;
#171472 = CARTESIAN_POINT ( 'NONE',  ( 3.473055881322492322, 1.772541284497713976, 0.8411618914155660764 ) ) ;
#171473 = CARTESIAN_POINT ( 'NONE',  ( -4.718311597035095062, 6.762783142908123324, 1.537733183400904702 ) ) ;
#171474 = CARTESIAN_POINT ( 'NONE',  ( 1.006607400890747295, 0.5640878064397096825, 1.878940696355746454 ) ) ;
#171475 = CARTESIAN_POINT ( 'NONE',  ( 0.000000000000000000, -0.5000000000000004441, 3.599999999999999201 ) ) ;
#171476 = CARTESIAN_POINT ( 'NONE',  ( 4.577813143269636065, 5.369812084349879555, -1.199719254218450271 ) ) ;
#171477 = EDGE_LOOP ( 'NONE', ( #120534, #140973, #128265, #62987, #19771 ) ) ;
#171478 = CARTESIAN_POINT ( 'NONE',  ( 6.139861302770143858, 2.010801613648224961, -0.1531635369260639090 ) ) ;
#171479 = CARTESIAN_POINT ( 'NONE',  ( -8.727698198895085469, 11.20540053684285553, -1.599625672291263179 ) ) ;
#171480 = DIRECTION ( 'NONE',  ( -0.000000000000000000, -8.546850786086437571E-32, -1.000000000000000000 ) ) ;
#171481 = CARTESIAN_POINT ( 'NONE',  ( 3.292005203939939229, -1.454527599200394539, -1.611992012647659900 ) ) ;
#171482 = DIRECTION ( 'NONE',  ( -1.000000000000000000, 1.014813233446432150E-15, 1.972152263052529514E-31 ) ) ;
#171483 = CARTESIAN_POINT ( 'NONE',  ( 0.2992908618118708675, -0.2657624787030036240, -2.103842954668332599 ) ) ;
#171484 = CARTESIAN_POINT ( 'NONE',  ( 1.499999999999989120, 1.806250000682817269, 0.000000000000000000 ) ) ;
#171485 = FILL_AREA_STYLE_COLOUR ( '', #13601 ) ;
#171486 = FACE_OUTER_BOUND ( 'NONE', #152359, .T. ) ;
#171487 = CARTESIAN_POINT ( 'NONE',  ( 5.917965873332177829, 7.245500866451762612, 1.242176317587460943 ) ) ;
#171488 = CARTESIAN_POINT ( 'NONE',  ( 1.001328657153805146, 1.683097017759589420, 1.188813969666648873 ) ) ;
#171490 = FACE_OUTER_BOUND ( 'NONE', #181274, .T. ) ;
#171489 = CARTESIAN_POINT ( 'NONE',  ( -7.980945979938748103, 12.46285407657057220, 0.000000000000000000 ) ) ;
#171491 = CARTESIAN_POINT ( 'NONE',  ( 0.6823417656249882723, 1.176041667008083325, -1.181850606188749264 ) ) ;
#171492 = DIRECTION ( 'NONE',  ( 0.000000000000000000, -1.496258514059622730E-16, 1.000000000000000000 ) ) ;
#171493 = ORIENTED_EDGE ( 'NONE', *, *, #110609, .F. ) ;
#171494 = CARTESIAN_POINT ( 'NONE',  ( 3.000541214264150547, -1.884352459892328024, -0.3246530749497905655 ) ) ;
#171495 = CARTESIAN_POINT ( 'NONE',  ( 5.524192064727496465, 1.051792464684684347, -1.423223091708211818 ) ) ;
#171496 = CARTESIAN_POINT ( 'NONE',  ( 5.200434439293556643, 8.224868058221247225, -1.199719254218452047 ) ) ;
#171497 = CARTESIAN_POINT ( 'NONE',  ( -4.765854690403601879, 5.518917546014321829, 1.199719254218462483 ) ) ;
#171498 = CARTESIAN_POINT ( 'NONE',  ( 0.6151243592659773052, 1.481389731780102137, 1.042453732408530342 ) ) ;
#171499 = CARTESIAN_POINT ( 'NONE',  ( 0.4092221944725178417, -1.818073194988058194, 0.6039046695034550050 ) ) ;
#171500 = CARTESIAN_POINT ( 'NONE',  ( 2.014207461368537455, 2.064961549741591185, -0.1501100615294431728 ) ) ;
#171501 = CARTESIAN_POINT ( 'NONE',  ( 0.6823417656249882723, -0.01145833299191073573, -1.181850606188749264 ) ) ;
#171502 = CARTESIAN_POINT ( 'NONE',  ( 6.280143113937574739, -0.9989825818290422044, 1.581392243879369053 ) ) ;
#171503 = CARTESIAN_POINT ( 'NONE',  ( 2.332394550857110893, 1.770734860448031300, 0.4440693575865002907 ) ) ;
#171505 = CARTESIAN_POINT ( 'NONE',  ( 5.840936731490688594, 7.196517624969346549, 1.161314407385056313 ) ) ;
#171504 = CARTESIAN_POINT ( 'NONE',  ( 5.215527394842717435, -0.3265260713646127022, 2.182469266582609091 ) ) ;
#171506 = CARTESIAN_POINT ( 'NONE',  ( 1.364683531249986537, -0.3447916663252443836, -0.7879004041258309554 ) ) ;
#171507 = CARTESIAN_POINT ( 'NONE',  ( 3.982923569253065121, 1.957725435881779941, 0.6497275974019289801 ) ) ;
#171508 = CARTESIAN_POINT ( 'NONE',  ( -6.714312387265696458, 8.856450423275211037, 1.599625672291283607 ) ) ;
#171509 = CARTESIAN_POINT ( 'NONE',  ( 10.06423010004587759, 10.63602329300870153, 0.000000000000000000 ) ) ;
#171510 = CARTESIAN_POINT ( 'NONE',  ( 3.818592820543299293, 7.606775390609172405, -0.7998128361456221525 ) ) ;
#171511 = CARTESIAN_POINT ( 'NONE',  ( 0.6851285477917113953, -0.2638797801631336259, -2.145333599305146333 ) ) ;
#171512 = CARTESIAN_POINT ( 'NONE',  ( 6.584440175795505112, 1.195396180001909059, -1.690200020538407566 ) ) ;
#171513 = CARTESIAN_POINT ( 'NONE',  ( -1.364683531250014514, 1.801041667008085767, -0.7879004041258289570 ) ) ;
#171514 = CARTESIAN_POINT ( 'NONE',  ( 4.165412764819938829, 0.2691229397190370576, -2.144731622849817221 ) ) ;
#171515 = CARTESIAN_POINT ( 'NONE',  ( 4.055335607603890224, -1.756228124781366917, 0.9972510931155349478 ) ) ;
#171516 = SURFACE_SIDE_STYLE ('',( #7938 ) ) ;
#171517 = EDGE_CURVE ( 'NONE', #51191, #72609, #28136, .T. ) ;
#171520 = CARTESIAN_POINT ( 'NONE',  ( 7.293923454472091450, 7.611924906413328529, 0.7216878364870317197 ) ) ;
#171519 = CARTESIAN_POINT ( 'NONE',  ( 0.000000000000000000, -2.996874999522043392, -3.793834371823813001 ) ) ;
#171518 = FACE_OUTER_BOUND ( 'NONE', #148138, .T. ) ;
#171521 = CARTESIAN_POINT ( 'NONE',  ( -7.228432174741334038, 8.462200954400218578, -1.199719254218452047 ) ) ;
#171522 = CARTESIAN_POINT ( 'NONE',  ( 2.184780103950241248, 1.616692242240840960, -1.205043568535242304 ) ) ;
#171524 = CARTESIAN_POINT ( 'NONE',  ( -4.227109282828894088, 7.477533499778591164, -0.9684700126486052163 ) ) ;
#171523 = CARTESIAN_POINT ( 'NONE',  ( -5.115504031057831469, 4.862509545855891346, 0.7998128361456341429 ) ) ;
#171525 = LINE ( 'NONE', #141214, #70506 ) ;
#171526 = CARTESIAN_POINT ( 'NONE',  ( 5.554919272666569263, 0.3793472168572444292, 1.874222000232607765 ) ) ;
#171527 = CARTESIAN_POINT ( 'NONE',  ( -1.499999999999997780, 4.431250000682819490, 1.214306433183764966E-14 ) ) ;
#171528 = CARTESIAN_POINT ( 'NONE',  ( 3.972175818679561043, 7.578029521860726092, -0.7216878364870197293 ) ) ;
#171530 = CARTESIAN_POINT ( 'NONE',  ( 4.376577478760902196, -0.4445230835841383898, -1.966641233467445016 ) ) ;
#171529 = CARTESIAN_POINT ( 'NONE',  ( -7.334597914868722590, 11.50085530074811935, -0.7216878364870267237 ) ) ;
#171531 = CARTESIAN_POINT ( 'NONE',  ( 1.499999999999989120, 4.504166666666688634, 0.8660254037844524744 ) ) ;
#171532 = CARTESIAN_POINT ( 'NONE',  ( 1.364683531250000303, 8.505208333674730170, -0.7879004041258355073 ) ) ;
#171533 = CARTESIAN_POINT ( 'NONE',  ( 6.018504615762162224, 1.154743246034171555, -1.281328459571188239 ) ) ;
#171534 = CARTESIAN_POINT ( 'NONE',  ( 4.929271367020211514, 7.908511140569038922, 1.199719254218452047 ) ) ;
#171535 = CARTESIAN_POINT ( 'NONE',  ( 7.890482213473377193, 11.18901776815221716, -1.082531754730543083 ) ) ;
#171536 = CARTESIAN_POINT ( 'NONE',  ( -11.44779965693221335, 10.99686076798700007, -3.599999932276613190 ) ) ;
#171537 = CARTESIAN_POINT ( 'NONE',  ( 4.481629103029507455, 1.220264704679861811, 1.417821649906551906 ) ) ;
#171538 = CARTESIAN_POINT ( 'NONE',  ( 0.000000000000000000, 4.500000000000003553, 0.000000000000000000 ) ) ;
#171539 = CARTESIAN_POINT ( 'NONE',  ( 2.184514099445804547, 1.195434181571125132, -1.690031224328606196 ) ) ;
#171540 = CARTESIAN_POINT ( 'NONE',  ( 3.834746474454188013E-15, 12.34375000068279959, 1.500000000000001554 ) ) ;
#171541 = VERTEX_POINT ( 'NONE', #205105 ) ;
#171542 = CARTESIAN_POINT ( 'NONE',  ( 3.054329744828568227, 6.785411478933790264, 0.000000000000000000 ) ) ;
#171543 = CARTESIAN_POINT ( 'NONE',  ( 0.3687678296072604556, -0.2496303596870551866, -2.000855358883571800 ) ) ;
#171544 = CARTESIAN_POINT ( 'NONE',  ( 3.716343503477301802, 7.349834830783237294, -1.734723475976807094E-15 ) ) ;
#171545 = CARTESIAN_POINT ( 'NONE',  ( 9.427850895902817996, 13.54474674066948481, 7.423989997610750180 ) ) ;
#171546 = CARTESIAN_POINT ( 'NONE',  ( 8.066738210006686671, 9.473911335505048825, 1.082531754730558626 ) ) ;
#171547 = EDGE_CURVE ( 'NONE', #108528, #132409, #41584, .T. ) ;
#171548 = AXIS2_PLACEMENT_3D ( 'NONE', #182373, #167215, #134739 ) ;
#171549 = CARTESIAN_POINT ( 'NONE',  ( 8.426556166093362776, 9.789735934319136135, -1.199719254218446718 ) ) ;
#171551 = CARTESIAN_POINT ( 'NONE',  ( 6.521099267210373363, -1.708630446951715731, 0.8662611975780337703 ) ) ;
#171550 = CARTESIAN_POINT ( 'NONE',  ( -7.203459687562382641, 7.298457811777897319, -0.7998128361456291469 ) ) ;
#171552 = DIRECTION ( 'NONE',  ( 0.000000000000000000, 0.000000000000000000, 1.000000000000000000 ) ) ;
#171553 = AXIS2_PLACEMENT_3D ( 'NONE', #9383, #57072, #108023 ) ;
#171554 = CARTESIAN_POINT ( 'NONE',  ( -0.6823417656250003738, -0.4697916663252491021, -1.181850606188749264 ) ) ;
#171556 = ORIENTED_EDGE ( 'NONE', *, *, #132492, .F. ) ;
#171555 = CARTESIAN_POINT ( 'NONE',  ( 4.690757960648231695, 5.535267711253469614, 1.082531754730560403 ) ) ;
#171557 = CARTESIAN_POINT ( 'NONE',  ( -7.375272376154093479, 9.627570410311676596, -1.443375672974059665 ) ) ;
#171558 = CARTESIAN_POINT ( 'NONE',  ( 3.502937704049162715, 1.705309618848281250, -1.328393843302432931 ) ) ;
#171559 = CARTESIAN_POINT ( 'NONE',  ( -5.614485009834902840, 9.564333254867113610, 0.7216878364870267237 ) ) ;
#171560 = CARTESIAN_POINT ( 'NONE',  ( 6.549997609177859559, 6.814287763561861944, 0.000000000000000000 ) ) ;
#171561 = CARTESIAN_POINT ( 'NONE',  ( 0.5805319366703353134, 1.050441701016216145, 1.842106252469346339 ) ) ;
#171562 = CARTESIAN_POINT ( 'NONE',  ( 5.684540951402929920, -1.781552174421060064, -0.3977488440568625605 ) ) ;
#171563 = CARTESIAN_POINT ( 'NONE',  ( 1.827351761895773530, -1.857630472158870116, 0.6603073207397982536 ) ) ;
#171564 = CARTESIAN_POINT ( 'NONE',  ( 5.097880177178074845, 1.288836597028759634, 1.412999258680311510 ) ) ;
#171565 = EDGE_LOOP ( 'NONE', ( #81874, #45460 ) ) ;
#171566 = CARTESIAN_POINT ( 'NONE',  ( -5.601522619460554075, 14.48156018096324971, -10.62176275871059694 ) ) ;
#171567 = CARTESIAN_POINT ( 'NONE',  ( 4.457443581450992731, 1.580467340599530424, 1.175029403372893855 ) ) ;
#171568 = CARTESIAN_POINT ( 'NONE',  ( 0.5857530202744161141, -1.927162159831939503, -0.2386530530817491391 ) ) ;
#171569 = ORIENTED_EDGE ( 'NONE', *, *, #29580, .T. ) ;
#171570 = CARTESIAN_POINT ( 'NONE',  ( -4.450819567036169211, 8.414649604842665553, -0.7998128361456362523 ) ) ;
#171572 = CARTESIAN_POINT ( 'NONE',  ( 6.663994888585881959, -7.154544010627095219, -6.770610912236887380 ) ) ;
#171571 = CARTESIAN_POINT ( 'NONE',  ( -5.496904935697871863, 5.377753611261092637, 0.7998128361456281477 ) ) ;
#171574 = CARTESIAN_POINT ( 'NONE',  ( 5.682275777458841048, 8.683053269460405232, 1.082531754730547524 ) ) ;
#171573 = CARTESIAN_POINT ( 'NONE',  ( 6.598014311344812199, 10.84943379654430906, 1.040834085586084257E-14 ) ) ;
#171576 = VERTEX_POINT ( 'NONE', #174791 ) ;
#171575 = CARTESIAN_POINT ( 'NONE',  ( 5.074826771331380826, -1.382354945563003312, 1.321565576914075502 ) ) ;
#171577 = EDGE_CURVE ( 'NONE', #212297, #74385, #69697, .T. ) ;
#171578 = CARTESIAN_POINT ( 'NONE',  ( 0.7630613749609324037, -1.597064910551798667, 1.523150255686569476 ) ) ;
#171579 = EDGE_CURVE ( 'NONE', #57507, #195170, #1932, .T. ) ;
#171580 = CARTESIAN_POINT ( 'NONE',  ( 7.446209719563361418, -5.223431457505083308, 8.064677165291199046 ) ) ;
#171581 = CARTESIAN_POINT ( 'NONE',  ( 0.02974158317493520720, -1.875378228685410376, 0.3729384364157954379 ) ) ;
#171582 = CARTESIAN_POINT ( 'NONE',  ( -0.02338929933904005179, 0.7691289590099622542, -1.796825425911799723 ) ) ;
#171583 = CARTESIAN_POINT ( 'NONE',  ( -0.06840433871349645145, 15.50637188434422420, 11.99962847080720074 ) ) ;
#171584 = CARTESIAN_POINT ( 'NONE',  ( -6.524021554744627416, -6.747656629766783709, -6.895452369244214452 ) ) ;
#171585 = CARTESIAN_POINT ( 'NONE',  ( 2.084514231050747401, 1.193861083872927109, -1.691280048542340486 ) ) ;
#171586 = CARTESIAN_POINT ( 'NONE',  ( -6.358937740009323214, 7.377514437221045718, -1.199719254218446718 ) ) ;
#171587 = VECTOR ( 'NONE', #101196, 1000.000000000000000 ) ;
#171588 = CARTESIAN_POINT ( 'NONE',  ( -4.606532530031762995, 8.380852375923623754, -0.1178885281021696541 ) ) ;
#171590 = CARTESIAN_POINT ( 'NONE',  ( 0.4796413896344040029, 2.016494124141111399, -0.7793912508547717888 ) ) ;
#171589 = CARTESIAN_POINT ( 'NONE',  ( -3.418627288940168096, 7.140148937072163804, -0.7998128361456281477 ) ) ;
#171591 = CARTESIAN_POINT ( 'NONE',  ( 5.248414862265931902, 5.295774558831261913, 0.000000000000000000 ) ) ;
#171592 = CARTESIAN_POINT ( 'NONE',  ( -4.741649638052999549, 5.202212439478444139, 1.069586989871945670 ) ) ;
#171593 = CARTESIAN_POINT ( 'NONE',  ( 0.6823417656249934904, 12.50520833367473017, 1.181850606188764807 ) ) ;
#171595 = CARTESIAN_POINT ( 'NONE',  ( -6.200875153403786477, 8.327716660428123419, -1.599625672291271394 ) ) ;
#171594 = CARTESIAN_POINT ( 'NONE',  ( 3.231779075379134003, 6.036511184309971689, 7.500000000000000000 ) ) ;
#171596 = CARTESIAN_POINT ( 'NONE',  ( 4.693871744853702843, 1.512258256419211078, 0.8485452647231973566 ) ) ;
#171597 = AXIS2_PLACEMENT_3D ( 'NONE', #50931, #186241, #37876 ) ;
#171598 = B_SPLINE_CURVE_WITH_KNOTS ( 'NONE', 3,
 ( #172090, #152627, #4214, #123429, #153705, #189391, #55134, #89793, #187255, #41034 ),
 .UNSPECIFIED., .F., .F.,
 ( 4, 1, 1, 1, 1, 1, 1, 4 ),
 ( 0.000000000000000000, 0.09705918685507786137, 0.1907419858981972138, 0.2602182418918835838, 0.3625179829595637226, 0.5215049497019805802, 0.7338397267804015467, 1.000000000000000000 ),
 .UNSPECIFIED. ) ;
#171599 = CARTESIAN_POINT ( 'NONE',  ( -3.602716132929368875, 5.226254793216122074, 1.599625672291267398 ) ) ;
#171600 = CARTESIAN_POINT ( 'NONE',  ( 2.711853232431875593, 0.5564382603544039130, -1.993978196652478996 ) ) ;
#171601 = CARTESIAN_POINT ( 'NONE',  ( 4.693022120063472080, 1.842747525957793009, 1.042402977009656340 ) ) ;
#171602 = CARTESIAN_POINT ( 'NONE',  ( 6.856673000209174695, 9.022537805042615489, 1.599625672291281386 ) ) ;
#171603 = CARTESIAN_POINT ( 'NONE',  ( 0.09924927195300653482, -9.920000000000094076, 10.99955234463956089 ) ) ;
#171604 = CARTESIAN_POINT ( 'NONE',  ( 2.131642331222316500, 1.886095724437972798, -0.5669754052412961931 ) ) ;
#171605 = CARTESIAN_POINT ( 'NONE',  ( 6.114657076318319007, 6.015903114251479167, -0.04046911893108330605 ) ) ;
#171606 = CARTESIAN_POINT ( 'NONE',  ( -0.4000000000000001332, 2.999999999999999112, -2.420000000000000373 ) ) ;
#171607 = CARTESIAN_POINT ( 'NONE',  ( 5.068466688948791266, -2.157128183272677191, -0.7757897288535390290 ) ) ;
#171608 = CARTESIAN_POINT ( 'NONE',  ( 1.347985785199314668, 1.823511463271022093, 0.09156768404049858701 ) ) ;
#171609 = VECTOR ( 'NONE', #32281, 1000.000000000000000 ) ;
#171610 = CARTESIAN_POINT ( 'NONE',  ( 4.030516805012513082, 7.924296382481737844, 0.000000000000000000 ) ) ;
#171612 = EDGE_CURVE ( 'NONE', #11745, #21505, #22068, .T. ) ;
#171611 = CARTESIAN_POINT ( 'NONE',  ( 4.297571505407542958, 7.957657823043374989, -0.7216878364870197293 ) ) ;
#171613 = CARTESIAN_POINT ( 'NONE',  ( -8.206763054973658100, 8.468978407091068306, 0.7998128361456602331 ) ) ;
#171614 = CARTESIAN_POINT ( 'NONE',  ( 2.988542084594744797, -1.195720007494217585, 1.619529446093708636 ) ) ;
#171615 = CARTESIAN_POINT ( 'NONE',  ( 2.869914117416060062, -1.941089286637355693, 0.2830422620509198128 ) ) ;
#171616 = CARTESIAN_POINT ( 'NONE',  ( -7.995557903757128493, 10.35123685918189729, 1.599625672291295375 ) ) ;
#171617 = CARTESIAN_POINT ( 'NONE',  ( -6.226218857173722476, 8.287007971501239467, 1.599625672291283607 ) ) ;
#171618 = DIRECTION ( 'NONE',  ( 0.6507913734559658270, 0.7592566023652989049, 0.000000000000000000 ) ) ;
#171620 = CARTESIAN_POINT ( 'NONE',  ( 4.504631171302628800, 1.367295333670435653, -1.123774403194759408 ) ) ;
#171619 = CARTESIAN_POINT ( 'NONE',  ( 5.947236541613409422, 0.6080794538029854479, -2.000250932508009782 ) ) ;
#171621 = CARTESIAN_POINT ( 'NONE',  ( -1.201851678989727383E-14, 3.368750000682815049, -1.732050807568863648 ) ) ;
#171622 = CARTESIAN_POINT ( 'NONE',  ( 0.9553299046189435151, 0.4242123182428610972, -2.149831459026855907 ) ) ;
#171623 = CARTESIAN_POINT ( 'NONE',  ( 5.701030997009290502, -0.4167664840721523878, 1.689554919747728423 ) ) ;
#171624 = CARTESIAN_POINT ( 'NONE',  ( 7.588813295347141441, 9.876701482703580837, -1.599625672291262513 ) ) ;
#171625 = DIRECTION ( 'NONE',  ( -1.000000000000000000, 6.308085367188389255E-16, 0.000000000000000000 ) ) ;
#171626 = CARTESIAN_POINT ( 'NONE',  ( 0.1405533004714097089, -0.003749010675423158478, -2.279853246149381452 ) ) ;
#171627 = EDGE_CURVE ( 'NONE', #211313, #160372, #173503, .T. ) ;
#171628 = CARTESIAN_POINT ( 'NONE',  ( 5.413366682498521598, 0.5056653987138818307, 1.658472451074376242 ) ) ;
#171629 = CARTESIAN_POINT ( 'NONE',  ( 1.893488989520499377, 1.919108310403025985, -1.089527612406354873 ) ) ;
#171630 = CARTESIAN_POINT ( 'NONE',  ( 5.529782829607038153, 2.093976201882574273, -0.5736635526294631138 ) ) ;
#171631 = CARTESIAN_POINT ( 'NONE',  ( 1.095081093118466908, 1.870138624552514006, 0.9927810678921239473 ) ) ;
#171632 = CARTESIAN_POINT ( 'NONE',  ( 2.937500000000001776, 1.451031289060998430, -1.451031289061236018 ) ) ;
#171633 = CARTESIAN_POINT ( 'NONE',  ( 6.727182134110201162, 1.237345558575110083, 2.302850971298702198 ) ) ;
#171634 = CARTESIAN_POINT ( 'NONE',  ( 4.612281621929555264, -0.8233390244782293754, -1.741700550419862825 ) ) ;
#171635 = CARTESIAN_POINT ( 'NONE',  ( 0.7686061912218185022, 2.218469807834182017, -0.1147041126551024554 ) ) ;
#171636 = ORIENTED_EDGE ( 'NONE', *, *, #82182, .T. ) ;
#171638 = CARTESIAN_POINT ( 'NONE',  ( 1.499999999999990896, 3.775000000000021227, 1.214306433183764966E-14 ) ) ;
#171637 = CARTESIAN_POINT ( 'NONE',  ( 1.294905083876269236, 1.870644729521577565, -1.324771388537665961 ) ) ;
#171639 = CARTESIAN_POINT ( 'NONE',  ( 5.359550796103802028, 5.147230771742885125, -0.7998128361456231517 ) ) ;
#171640 = CARTESIAN_POINT ( 'NONE',  ( 6.331821432781979730, 7.345878745455822312, -1.199719254218445830 ) ) ;
#171641 = CARTESIAN_POINT ( 'NONE',  ( 4.266425542637849233, 2.220793247050854902, -0.05466516159106404871 ) ) ;
#171642 = CARTESIAN_POINT ( 'NONE',  ( -9.178506806771670412, 9.810605484096178941, 1.040834085586084257E-14 ) ) ;
#171643 = CARTESIAN_POINT ( 'NONE',  ( 7.348156068926750883, 8.635565504245116486, -1.082531754730537976 ) ) ;
#171644 = CARTESIAN_POINT ( 'NONE',  ( -8.798878505144649864, 11.28844422746735532, -1.443375672974058777 ) ) ;
#171645 = CARTESIAN_POINT ( 'NONE',  ( 6.319508997745523438, 9.426492026461511742, -1.082531754730548412 ) ) ;
#171646 = ORIENTED_EDGE ( 'NONE', *, *, #184187, .F. ) ;
#171647 = CARTESIAN_POINT ( 'NONE',  ( 2.285779929129946098, 1.617817622347239803, -1.203354541732377658 ) ) ;
#171649 = CARTESIAN_POINT ( 'NONE',  ( 6.303195905902406970, -1.744534168554587872, 1.100284471152054300 ) ) ;
#171648 = CARTESIAN_POINT ( 'NONE',  ( 6.564118927310645724, 10.80988918183778225, -0.7998128361456291469 ) ) ;
#171650 = CARTESIAN_POINT ( 'NONE',  ( 5.519577934094840543, 9.453608333170423705, 0.7216878364870317197 ) ) ;
#171651 = CARTESIAN_POINT ( 'NONE',  ( 6.304260172732157663, 1.282988983046409848, -1.176258868317042294 ) ) ;
#171652 = ADVANCED_FACE ( 'NONE', ( #156390 ), #190991, .T. ) ;
#171653 = CARTESIAN_POINT ( 'NONE',  ( -0.6823417656250003738, 2.217708333674753174, -1.181850606188749264 ) ) ;
#171654 = CARTESIAN_POINT ( 'NONE',  ( 1.141466271755723794, 0.7239738643088615699, -1.615086939138086652 ) ) ;
#171655 = CARTESIAN_POINT ( 'NONE',  ( 0.1588275700346117869, 1.163271727376416376, 1.646837250247008777 ) ) ;
#171656 = CARTESIAN_POINT ( 'NONE',  ( 0.1691535571452691677, 1.059206136818511501, 1.505872603892892458 ) ) ;
#171657 = CARTESIAN_POINT ( 'NONE',  ( 4.511445251964079084, -2.248337965441957742, 0.4463705457610280258 ) ) ;
#171658 = CARTESIAN_POINT ( 'NONE',  ( 3.116968920156853340, -1.774181764490849522, 0.4917334186493869108 ) ) ;
#171659 = EDGE_CURVE ( 'NONE', #181928, #188409, #35070, .T. ) ;
#171660 = CARTESIAN_POINT ( 'NONE',  ( 8.422639742587595180, 10.84949900448412130, -1.599625672291268286 ) ) ;
#171661 = CARTESIAN_POINT ( 'NONE',  ( 11.18117232051588594, 8.274016526874332200, -4.422333253022389776 ) ) ;
#171662 = CARTESIAN_POINT ( 'NONE',  ( 2.678497062878131718, -1.746332412481563567, -0.5319975912557314279 ) ) ;
#171663 = CARTESIAN_POINT ( 'NONE',  ( 3.885388821667290493, -0.6351983117205138862, -1.913803978180687482 ) ) ;
#171664 = CARTESIAN_POINT ( 'NONE',  ( -8.292783513053063160, 12.82666453187061073, 0.7998128361456481317 ) ) ;
#171666 = DIRECTION ( 'NONE',  ( -0.000000000000000000, -1.000000000000000000, 0.000000000000000000 ) ) ;
#171665 = CARTESIAN_POINT ( 'NONE',  ( 3.837032359523879332, 0.3291597691741187104, 2.238327980419333674 ) ) ;
#171667 = CARTESIAN_POINT ( 'NONE',  ( 5.350649881110917327, 0.6085095821539068250, 2.016136239840255140 ) ) ;
#171668 = CARTESIAN_POINT ( 'NONE',  ( 3.947765587739564097, 1.497496809916948779, 1.429883829622953462 ) ) ;
#171669 = CARTESIAN_POINT ( 'NONE',  ( 3.837121167867449945, 4.435395103055503441, 1.199719254218464037 ) ) ;
#171670 = CARTESIAN_POINT ( 'NONE',  ( -0.6801582343750316451, 0.2135416670080853008, 1.178068619123807004 ) ) ;
#171671 = CARTESIAN_POINT ( 'NONE',  ( 5.760427271636393343, 2.118038551301495875, 0.1041057254967461404 ) ) ;
#171673 = CIRCLE ( 'NONE', #5586, 3.150000000000000799 ) ;
#171672 = SHAPE_DEFINITION_REPRESENTATION ( #213239, #203468 ) ;
#171675 = CARTESIAN_POINT ( 'NONE',  ( 1.312975575179779586, 1.698600376263710743, 0.9089255565387382996 ) ) ;
#171674 = CARTESIAN_POINT ( 'NONE',  ( -9.124801077197171040, 10.60435499727357289, -1.199719254218441611 ) ) ;
#171676 = CARTESIAN_POINT ( 'NONE',  ( -4.736594563127865420, 6.619389305106191834, -1.599625672291271394 ) ) ;
#171677 = CARTESIAN_POINT ( 'NONE',  ( 9.908311333488716954, 10.45411806535867782, 0.7998128361456462443 ) ) ;
#171678 = CARTESIAN_POINT ( 'NONE',  ( 3.214691819771663628, 6.764574533126651801, -0.7216878364870338292 ) ) ;
#171679 = CARTESIAN_POINT ( 'NONE',  ( 5.244386534325491844, 6.400378350754194479, 1.153371672928265479 ) ) ;
#171680 = CARTESIAN_POINT ( 'NONE',  ( -2.788906526875773208E-15, 10.96875000068279427, -1.499999999999998446 ) ) ;
#171681 = CARTESIAN_POINT ( 'NONE',  ( -3.928111819657352566, 5.605883094398769195, 1.599625672291267398 ) ) ;
#171682 = CARTESIAN_POINT ( 'NONE',  ( 0.5807245924134795123, 1.101748585799481095, 1.928910967146231004 ) ) ;
#171683 = CARTESIAN_POINT ( 'NONE',  ( 2.151528103076968179, -1.690815887601760270, -1.255243123012689921 ) ) ;
#171684 = CARTESIAN_POINT ( 'NONE',  ( -5.178288325776719603, 5.006034233019745372, 0.000000000000000000 ) ) ;
#171685 = CARTESIAN_POINT ( 'NONE',  ( 6.577677080924314801, 10.82570702772039262, 1.040834085586084257E-14 ) ) ;
#171686 = CARTESIAN_POINT ( 'NONE',  ( 6.930517489306616596, -1.145039166549733922, 1.467359839328785664 ) ) ;
#171687 = CARTESIAN_POINT ( 'NONE',  ( 6.479907352327590964, 9.647310113435821677, 1.199719254218462483 ) ) ;
#171688 = CARTESIAN_POINT ( 'NONE',  ( 11.94980361058169116, 10.19999999999999929, 1.099999999999994982 ) ) ;
#171689 = CARTESIAN_POINT ( 'NONE',  ( -7.770231434407805615, 8.237893892996801526, 0.000000000000000000 ) ) ;
#171690 = CARTESIAN_POINT ( 'NONE',  ( -8.839552966430012759, 10.37552855133225904, -1.082531754730543971 ) ) ;
#171691 = CARTESIAN_POINT ( 'NONE',  ( -1.822139829856989079, 2.508700120398218214, 2.498486944294419754 ) ) ;
#171692 = CARTESIAN_POINT ( 'NONE',  ( -6.291865805193673111, 9.498204651771386509, -1.199719254218452047 ) ) ;
#171694 = CARTESIAN_POINT ( 'NONE',  ( 3.437899435096212208, 1.242623406730450908, 1.518177208742684803 ) ) ;
#171693 = CARTESIAN_POINT ( 'NONE',  ( -1.360316468750058627, 2.692708333674814991, 0.7853790794158641564 ) ) ;
#171695 = CARTESIAN_POINT ( 'NONE',  ( 2.694378501574711926, -2.155843008138720762, -0.1600555415394027403 ) ) ;
#171696 = CARTESIAN_POINT ( 'NONE',  ( 1.135996871135702024, 0.3593859243370273182, 1.805655672011026391 ) ) ;
#171698 = CARTESIAN_POINT ( 'NONE',  ( -6.041716223103725802, 6.056113169402001617, -0.5645603026655892087 ) ) ;
#171697 = CARTESIAN_POINT ( 'NONE',  ( -5.957882158562513908, 5.915560371269843465, -0.7998128361456362523 ) ) ;
#171699 = CARTESIAN_POINT ( 'NONE',  ( 3.609068157710407565, -1.714216318138677808, 0.2993142247325294991 ) ) ;
#171700 = CARTESIAN_POINT ( 'NONE',  ( 4.989037340148863464, 8.764367963574922982, -0.7216878364870257245 ) ) ;
#171701 = CARTESIAN_POINT ( 'NONE',  ( -11.80098439192703097, 4.809115636342174760, 4.927210371565812430 ) ) ;
#171702 = CARTESIAN_POINT ( 'NONE',  ( 8.829384350997564468, 11.32403438096243775, 1.599625672291281386 ) ) ;
#171703 = CARTESIAN_POINT ( 'NONE',  ( 1.094844843509492183, -0.5259716649698794599, -2.096624219460433647 ) ) ;
#171704 = AXIS2_PLACEMENT_3D ( 'NONE', #160598, #97756, #31678 ) ;
#171705 = CARTESIAN_POINT ( 'NONE',  ( 3.901720107437017582, 0.2930258228103881923, 1.994564303527603499 ) ) ;
#171706 = CARTESIAN_POINT ( 'NONE',  ( -0.09196683552162310260, -9.918146503183461249, -10.99961570984661563 ) ) ;
#171707 = CARTESIAN_POINT ( 'NONE',  ( 0.5851287433712646369, -0.2658872486876809327, -2.145209338178376335 ) ) ;
#171708 = CARTESIAN_POINT ( 'NONE',  ( 2.535955197907293179, 0.9309914139831111379, -1.737806310995954728 ) ) ;
#171709 = CIRCLE ( 'NONE', #150858, 2.000000000000006217 ) ;
#171710 = CARTESIAN_POINT ( 'NONE',  ( 6.509000000000048303, 2.074227158855263209, 2.209070705210983032 ) ) ;
#171711 = CARTESIAN_POINT ( 'NONE',  ( 2.313922598539425390, 1.266723153581908567, -1.472183398282415956 ) ) ;
#171713 = CARTESIAN_POINT ( 'NONE',  ( -4.990809943606286048, 5.955604701363006015, -1.082531754730549967 ) ) ;
#171712 = CARTESIAN_POINT ( 'NONE',  ( 0.2331563151865486683, 0.005903526429595904942, -1.945944850731482934 ) ) ;
#171714 = CARTESIAN_POINT ( 'NONE',  ( -5.275531169048922386, 5.327410250078064458, -0.7216878364870338292 ) ) ;
#171715 = CARTESIAN_POINT ( 'NONE',  ( -0.1108833634137010304, 6.948331553507800962, -2.491992042620773340 ) ) ;
#171716 = CARTESIAN_POINT ( 'NONE',  ( 4.213551878797002992, 8.137837301896977849, 0.000000000000000000 ) ) ;
#171717 = CARTESIAN_POINT ( 'NONE',  ( -6.656127069666307072, 6.730179434224282886, 0.7998128361456341429 ) ) ;
#171718 = CARTESIAN_POINT ( 'NONE',  ( -6.607619761813764647, 8.802252036906432764, 1.599625672291269396 ) ) ;
#171719 = CARTESIAN_POINT ( 'NONE',  ( -1.286956418854606543, 4.047654341997520611, 0.4592741676706140197 ) ) ;
#171720 = CARTESIAN_POINT ( 'NONE',  ( 5.333197341169245043, 0.1633263742753125747, 2.301865194068336784 ) ) ;
#171721 = DIRECTION ( 'NONE',  ( -0.000000000000000000, 1.000000000000000000, -0.000000000000000000 ) ) ;
#171722 = CARTESIAN_POINT ( 'NONE',  ( 4.346505277090593644, -1.939800950321630690, -0.2920161945778113055 ) ) ;
#171723 = CARTESIAN_POINT ( 'NONE',  ( 7.527801604085637699, 9.805521176231838609, 1.599625672291281386 ) ) ;
#171724 = CARTESIAN_POINT ( 'NONE',  ( 0.7037502660087076034, 1.864169469917423161, 0.7691187473759173443 ) ) ;
#171725 = ORIENTED_EDGE ( 'NONE', *, *, #114638, .T. ) ;
#171726 = CARTESIAN_POINT ( 'NONE',  ( 2.009133639091817525, 0.005444305534021975056, 2.117513411327852868 ) ) ;
#171727 = CARTESIAN_POINT ( 'NONE',  ( -1.201851678989727383E-14, 2.243750000682818158, 1.732050807568877637 ) ) ;
#171729 = CARTESIAN_POINT ( 'NONE',  ( -7.217017841176048165, 7.314275657660511243, 1.040834085586084257E-14 ) ) ;
#171728 = CARTESIAN_POINT ( 'NONE',  ( -3.755772246185468788, 4.340488027759846545, -1.199719254218452047 ) ) ;
#171730 = CARTESIAN_POINT ( 'NONE',  ( 3.081803158279991628, -1.813988701161291628, -0.3140598505507880556 ) ) ;
#171731 = ORIENTED_EDGE ( 'NONE', *, *, #19236, .F. ) ;
#171732 = CARTESIAN_POINT ( 'NONE',  ( -8.597841969360544567, 13.18256606422934674, 0.7998128361456341429 ) ) ;
#171733 = CARTESIAN_POINT ( 'NONE',  ( 3.667627899390076607, 3.521066046765033430, 2.447586748966623649 ) ) ;
#171734 = CARTESIAN_POINT ( 'NONE',  ( 3.656581996618038843, 2.110704406498860486, 0.2042969539849878724 ) ) ;
#171735 = CARTESIAN_POINT ( 'NONE',  ( 0.1285073612291263989, -1.684675954457705682, 0.7431698939026829542 ) ) ;
#171736 = CARTESIAN_POINT ( 'NONE',  ( -1.499999999999997780, 5.431250000682820378, 1.214306433183764966E-14 ) ) ;
#171737 = CARTESIAN_POINT ( 'NONE',  ( 8.125414133291656071, 8.374071331795406081, -0.7998128361456291469 ) ) ;
#171738 = CARTESIAN_POINT ( 'NONE',  ( 6.444921918449731280, 8.612437886315108315, 1.599625672291268286 ) ) ;
#171739 = CARTESIAN_POINT ( 'NONE',  ( 3.971991334398959239, 1.141669855754149365, 1.715422085859653833 ) ) ;
#171741 = CARTESIAN_POINT ( 'NONE',  ( 1.645803748337611783, 0.5784278848013635344, 1.748079663633335334 ) ) ;
#171740 = CARTESIAN_POINT ( 'NONE',  ( -7.121056995675673740, 9.330985799753529264, -1.599625672291263179 ) ) ;
#171742 = CARTESIAN_POINT ( 'NONE',  ( 0.6823417656249917140, 4.342708333674755394, 1.181850606188765695 ) ) ;
#171743 = FACE_BOUND ( 'NONE', #192737, .T. ) ;
#171744 = CARTESIAN_POINT ( 'NONE',  ( -9.499610831742323569, -9.904389604292740401, 0.08598863555141569859 ) ) ;
#171745 = DIRECTION ( 'NONE',  ( -8.638326563840809144E-31, -5.962633348652903386E-61, 1.000000000000000000 ) ) ;
#171746 = MECHANICAL_DESIGN_GEOMETRIC_PRESENTATION_REPRESENTATION (  '', ( #202798 ), #140563 ) ;
#171747 = CARTESIAN_POINT ( 'NONE',  ( 1.418904949497600487, 1.480075412272121582, -1.637148382315711359 ) ) ;
#171748 = CARTESIAN_POINT ( 'NONE',  ( 3.655803326253406649, 0.5538646471104657909, -2.193435612772106413 ) ) ;
#171749 = CARTESIAN_POINT ( 'NONE',  ( -7.524412065904404479, 11.72230514362308185, 0.000000000000000000 ) ) ;
#171750 = CARTESIAN_POINT ( 'NONE',  ( 3.410248120744460376, -1.809760825414870267, -0.08362741940017533182 ) ) ;
#171751 = B_SPLINE_CURVE_WITH_KNOTS ( 'NONE', 3,
 ( #106099, #101779, #172121, #205662, #23715, #155869, #167848, #19447 ),
 .UNSPECIFIED., .F., .F.,
 ( 4, 2, 2, 4 ),
 ( 6.505213034912872530E-19, 0.0002224730689913817223, 0.0004449461379827644204, 0.0008898922759655299251 ),
 .UNSPECIFIED. ) ;
#171752 = CARTESIAN_POINT ( 'NONE',  ( 4.417137112658839015, -1.749089155124187389, 0.7819188135024003339 ) ) ;
#171753 = CARTESIAN_POINT ( 'NONE',  ( 4.914543119725925280, 0.7892175071393169317, 1.914236960262293508 ) ) ;
#171754 = CARTESIAN_POINT ( 'NONE',  ( -0.6823417656250212460, 3.863541667008085767, 1.181850606188767472 ) ) ;
#171755 = AXIS2_PLACEMENT_3D ( 'NONE', #49694, #181810, #148277 ) ;
#171756 = CARTESIAN_POINT ( 'NONE',  ( 3.239098446765543482, -1.739280071990648935, 0.9281937050133574063 ) ) ;
#171757 = CARTESIAN_POINT ( 'NONE',  ( 1.606340841434449329, -0.6908775452558654218, -1.798418176235560662 ) ) ;
#171758 = CARTESIAN_POINT ( 'NONE',  ( 4.346470048663173102, 0.4987854378066917116, 1.802870001028591407 ) ) ;
#171759 = CARTESIAN_POINT ( 'NONE',  ( 2.965757426574578304, 0.3381026970978153745, -2.282680038778000853 ) ) ;
#171760 = CARTESIAN_POINT ( 'NONE',  ( 3.191705266286504639, -1.248028223939607884, -1.380750640708436006 ) ) ;
#171761 = CARTESIAN_POINT ( 'NONE',  ( -1.364683531250010295, 4.030208333674751842, 0.7879004041258379498 ) ) ;
#171762 = CARTESIAN_POINT ( 'NONE',  ( 5.318541398310776103, 9.426991741329731056, -0.7998128361456481317 ) ) ;
#171763 = CARTESIAN_POINT ( 'NONE',  ( 6.531277313481192337, 8.642909503859968368, 1.599625672291281386 ) ) ;
#171764 = CYLINDRICAL_SURFACE ( 'NONE', #193393, 1.500000000000000222 ) ;
#171765 = CARTESIAN_POINT ( 'NONE',  ( 0.5574226275508349371, -1.780365264567655759, -1.124781644112993417 ) ) ;
#171766 = CARTESIAN_POINT ( 'NONE',  ( 2.860407222358956503, 6.280966159486672140, 0.7216878364870338292 ) ) ;
#171768 = CARTESIAN_POINT ( 'NONE',  ( 0.000000000000000000, -6.893137084989842123, 0.000000000000000000 ) ) ;
#171767 = CARTESIAN_POINT ( 'NONE',  ( 1.364683531249990311, 5.176041667008085767, 0.7879004041258500513 ) ) ;
#171769 = CARTESIAN_POINT ( 'NONE',  ( 1.881254504445781794, -1.940830296247602949, -0.8548571619346673200 ) ) ;
#171770 = CARTESIAN_POINT ( 'NONE',  ( -1.284279953904128524, 10.64264068711930733, -0.7749999999999892530 ) ) ;
#171771 = CARTESIAN_POINT ( 'NONE',  ( 0.6858141477139628739, 1.945346236745447488, -0.5429362378739016615 ) ) ;
#171772 = CARTESIAN_POINT ( 'NONE',  ( 1.364683531249986537, 0.6552083336747522857, -0.7879004041258239610 ) ) ;
#171773 = PRESENTATION_LAYER_ASSIGNMENT (  '', '', ( #175337 ) ) ;
#171774 = CARTESIAN_POINT ( 'NONE',  ( -2.968872451712654126, 6.407508927065978632, 1.040834085586084257E-14 ) ) ;
#171775 = CARTESIAN_POINT ( 'NONE',  ( 3.662674053986138656, 7.424870162959149589, 0.7998128361456321445 ) ) ;
#171776 = EDGE_LOOP ( 'NONE', ( #174668, #17800, #202134, #187152, #148926 ) ) ;
#171777 = CARTESIAN_POINT ( 'NONE',  ( 1.247603677004164746, -1.703183937513498281, -1.330886036463780009 ) ) ;
#171778 = DIRECTION ( 'NONE',  ( 0.000000000000000000, -1.000000000000000000, 0.000000000000000000 ) ) ;
#171781 = CARTESIAN_POINT ( 'NONE',  ( 4.256897045010922476, 5.029096643009940415, -1.082531754730548412 ) ) ;
#171780 = CARTESIAN_POINT ( 'NONE',  ( 6.925078400183553917, 6.038071034253152725, 2.450556290382682523 ) ) ;
#171779 = CARTESIAN_POINT ( 'NONE',  ( 5.037736595929563244, 8.035053907629919223, -1.199719254218452047 ) ) ;
#171782 = LINE ( 'NONE', #104663, #89467 ) ;
#171783 = CARTESIAN_POINT ( 'NONE',  ( 5.911342272548038679, -1.897112096406332382, 0.6839327336411115121 ) ) ;
#171784 = CARTESIAN_POINT ( 'NONE',  ( -8.676855123066022912, 10.18571440074093282, -1.082531754730543971 ) ) ;
#171785 = CARTESIAN_POINT ( 'NONE',  ( 0.09952931447375359952, -0.5783855404800625211, 2.113812074898171023 ) ) ;
#171786 = CARTESIAN_POINT ( 'NONE',  ( -5.273758566035884776, 5.255065869904374409, 0.000000000000000000 ) ) ;
#171788 = CARTESIAN_POINT ( 'NONE',  ( -1.402160292154681736E-14, 10.42187500034139624, 1.575800808251682339 ) ) ;
#171787 = CARTESIAN_POINT ( 'NONE',  ( 6.789893189004300389, -0.9291300992274166282, 1.949920244826188309 ) ) ;
#171789 = CARTESIAN_POINT ( 'NONE',  ( -8.513630394377489807, 12.01998699582738972, -1.199719254218446718 ) ) ;
#171791 = CARTESIAN_POINT ( 'NONE',  ( 1.106889576528688801, -0.04550283046177550778, 1.915226712711289636 ) ) ;
#171790 = CARTESIAN_POINT ( 'NONE',  ( -4.704316113817535339, 8.432193199521691440, 0.7216878364870458196 ) ) ;
#171792 = CARTESIAN_POINT ( 'NONE',  ( 1.364683531249986537, 0.1760416670080860446, 0.7879004041258500513 ) ) ;
#171793 = CARTESIAN_POINT ( 'NONE',  ( 6.966220764712121927, 6.002124920821316323, 2.500000000000000444 ) ) ;
#171794 = EDGE_CURVE ( 'NONE', #202127, #213959, #414, .T. ) ;
#171795 = CARTESIAN_POINT ( 'NONE',  ( 1.500000000000001332, 9.375000000000001776, 0.000000000000000000 ) ) ;
#171796 = CARTESIAN_POINT ( 'NONE',  ( 3.193694537771115449, -0.6981934656059236577, 1.577442374586303320 ) ) ;
#171797 = CARTESIAN_POINT ( 'NONE',  ( 4.529305835417093640, 7.441884687032027657, -1.199719254218450271 ) ) ;
#171798 = CARTESIAN_POINT ( 'NONE',  ( 2.547821756505376012, 1.769265940657601011, 0.04812675368598590825 ) ) ;
#171799 = FILL_AREA_STYLE_COLOUR ( '', #36692 ) ;
#171800 = CARTESIAN_POINT ( 'NONE',  ( 8.374132434735052755, 12.92157160716627295, -0.7998128361456352531 ) ) ;
#171801 = CARTESIAN_POINT ( 'NONE',  ( 5.192482782645277517, -2.189556457885518892, -0.2746672974567528347 ) ) ;
#171802 = ORIENTED_EDGE ( 'NONE', *, *, #101474, .F. ) ;
#171803 = CARTESIAN_POINT ( 'NONE',  ( 4.394789018838915595, -1.960137222954833502, -0.4867870608649630393 ) ) ;
#171804 = CARTESIAN_POINT ( 'NONE',  ( -7.208094944320834863, 8.438474185576302133, -1.199719254218452047 ) ) ;
#171806 = CARTESIAN_POINT ( 'NONE',  ( 3.884388800492278193, -0.6352171928143932611, -1.913798906059568594 ) ) ;
#171805 = CARTESIAN_POINT ( 'NONE',  ( 4.125719030757846184, -0.3612518283466863434, 2.089324717668067599 ) ) ;
#171808 = ORIENTED_EDGE ( 'NONE', *, *, #109767, .T. ) ;
#171807 = CARTESIAN_POINT ( 'NONE',  ( 4.166123871162411341, 1.811061351045451850, -0.05074819156030555695 ) ) ;
#171809 = CARTESIAN_POINT ( 'NONE',  ( 5.845500506147374153, 6.848780674373954547, 1.199719254218453823 ) ) ;
#171810 = EDGE_CURVE ( 'NONE', #30835, #163314, #121607, .T. ) ;
#171811 = ORIENTED_EDGE ( 'NONE', *, *, #78415, .T. ) ;
#171812 = CARTESIAN_POINT ( 'NONE',  ( 1.164687902950040321, -1.689591380799923215, -0.8031939614948148121 ) ) ;
#171813 = EDGE_CURVE ( 'NONE', #11835, #61877, #114117, .T. ) ;
#171814 = CARTESIAN_POINT ( 'NONE',  ( 6.164714480961021259, 0.5753438643430182076, 1.717747506070513852 ) ) ;
#171815 = CARTESIAN_POINT ( 'NONE',  ( -3.765413976293358278, 5.416068943807445635, 1.599625672291267398 ) ) ;
#171816 = CARTESIAN_POINT ( 'NONE',  ( 0.000000000000000000, 7.500000000000000000, -1.500000000000000222 ) ) ;
#171817 = CARTESIAN_POINT ( 'NONE',  ( -0.4019237886466933696, 8.582585450998170273, 1.500000000000005995 ) ) ;
#171818 = CARTESIAN_POINT ( 'NONE',  ( 0.6823417656249899377, 2.405208333674753618, 1.181850606188767472 ) ) ;
#171819 = SURFACE_STYLE_FILL_AREA ( #122091 ) ;
#171820 = CARTESIAN_POINT ( 'NONE',  ( 7.675324359112103423, 8.127168971818530707, 0.7216878364870267237 ) ) ;
#171821 = CARTESIAN_POINT ( 'NONE',  ( -3.933273961740340496, 5.682181936820735579, 1.443375672974065660 ) ) ;
#171822 = CARTESIAN_POINT ( 'NONE',  ( -5.529746549527323474, 7.544733289238903851, -1.599625672291271394 ) ) ;
#171823 = CARTESIAN_POINT ( 'NONE',  ( 4.377262645480927361, -1.895543854172193399, -0.9507902649282941043 ) ) ;
#171825 = CARTESIAN_POINT ( 'NONE',  ( -10.07159190936562432, 5.946254181132138328, -5.792974557957699666 ) ) ;
#171824 = CARTESIAN_POINT ( 'NONE',  ( -0.1296875068448125057, 2.889142263448498227, -2.315371602238533555 ) ) ;
#171826 = CARTESIAN_POINT ( 'NONE',  ( 5.378184286887115029, -1.097432272127541131, 1.637457850930480241 ) ) ;
#171827 = CARTESIAN_POINT ( 'NONE',  ( -1.364683531250012516, 0.5302083336747518416, 0.7879004041258379498 ) ) ;
#171828 = CARTESIAN_POINT ( 'NONE',  ( 1.054940647564650336, 0.3968280277809080880, 1.973547778087578308 ) ) ;
#171829 = VERTEX_POINT ( 'NONE', #56745 ) ;
#171830 = VECTOR ( 'NONE', #28496, 1000.000000000000000 ) ;
#171831 = CARTESIAN_POINT ( 'NONE',  ( 6.438674896094000566, -1.635394517905249145, 1.344423162301669361 ) ) ;
#171832 = CARTESIAN_POINT ( 'NONE',  ( 8.433927911510377129, 13.95651121305023601, 8.536819633252605399 ) ) ;
#171833 = CARTESIAN_POINT ( 'NONE',  ( 1.803268859043684058, -1.750145871244257467, 1.105767233283899920 ) ) ;
#171834 = ORIENTED_EDGE ( 'NONE', *, *, #110968, .F. ) ;
#171835 = CARTESIAN_POINT ( 'NONE',  ( 5.554000203453580475, 6.508696987897830688, -1.199719254218452047 ) ) ;
#171836 = CARTESIAN_POINT ( 'NONE',  ( 5.224688093219824303, 7.188831756880171397, -1.599625672291283607 ) ) ;
#171838 = CARTESIAN_POINT ( 'NONE',  ( 5.331380718671758778, 7.243030143248949670, -1.599625672291256295 ) ) ;
#171837 = CARTESIAN_POINT ( 'NONE',  ( 4.207035958355084482, -0.3574298538902004885, 2.059684413417623094 ) ) ;
#171839 = CARTESIAN_POINT ( 'NONE',  ( 6.658989722967328717, 7.797851427330578566, 1.199719254218452935 ) ) ;
#171842 = ORIENTED_EDGE ( 'NONE', *, *, #145707, .F. ) ;
#171841 = CARTESIAN_POINT ( 'NONE',  ( 2.103910407274149907, -0.7736040573625382333, 1.638098421638082947 ) ) ;
#171840 = CARTESIAN_POINT ( 'NONE',  ( 2.766400663125650361, -1.260407102598060103, 1.320874842943790872 ) ) ;
#171843 = CARTESIAN_POINT ( 'NONE',  ( 6.721333373144884327, -0.1645177889858795151, 2.170883633896856679 ) ) ;
#171844 = FACE_OUTER_BOUND ( 'NONE', #111930, .T. ) ;
#171845 = CARTESIAN_POINT ( 'NONE',  ( 4.313639225654395837, -0.3805011380913872476, 2.173570407251995018 ) ) ;
#171846 = CARTESIAN_POINT ( 'NONE',  ( 5.933664784275179294, 10.07435934829639912, -0.7998128361456291469 ) ) ;
#171847 = CARTESIAN_POINT ( 'NONE',  ( -1.402160292154681736E-14, 8.484375000341403350, 1.575800808251682339 ) ) ;
#171848 = CARTESIAN_POINT ( 'NONE',  ( 2.525908831824146716, -1.891188341833284881, 0.2824699455093656053 ) ) ;
#171849 = CARTESIAN_POINT ( 'NONE',  ( 8.392660782059197189, 9.750191319612612872, 1.199719254218462483 ) ) ;
#171850 = CARTESIAN_POINT ( 'NONE',  ( 6.654741963219191980, -0.5482099483974657295, -1.996413779700876079 ) ) ;
#171851 = DIRECTION ( 'NONE',  ( 0.000000000000000000, 1.000000000000000000, 0.000000000000000000 ) ) ;
#171852 = CARTESIAN_POINT ( 'NONE',  ( 6.163654587501778970, 1.125051486859941718, 1.880622087419632882 ) ) ;
#171853 = CARTESIAN_POINT ( 'NONE',  ( 4.913571454530422322, 8.125067815752732514, -1.031885869761673069 ) ) ;
#171854 = ORIENTED_EDGE ( 'NONE', *, *, #191572, .T. ) ;
#171855 = CARTESIAN_POINT ( 'NONE',  ( 0.3999999999999834799, 2.982849289862649744, 2.023857702508388812 ) ) ;
#171856 = CARTESIAN_POINT ( 'NONE',  ( 3.549202351727371862, 7.362762853649070571, -0.7998128361456362523 ) ) ;
#171857 = CARTESIAN_POINT ( 'NONE',  ( -0.02319159430947368566, 6.948789054712430691, -2.406029888528108618 ) ) ;
#171858 = CIRCLE ( 'NONE', #5770, 0.08000000000000041800 ) ;
#171859 = CARTESIAN_POINT ( 'NONE',  ( -0.4019237886466871523, 12.47991455036742892, -1.499999999999998668 ) ) ;
#171860 = CARTESIAN_POINT ( 'NONE',  ( -8.866669273657352690, 9.446795028796142191, 0.7216878364870438212 ) ) ;
#171862 = CARTESIAN_POINT ( 'NONE',  ( 3.790386463472274148, 6.579812086429759788, 1.199719254218452047 ) ) ;
#171861 = PRESENTATION_LAYER_ASSIGNMENT (  '', '', ( #74926 ) ) ;
#171863 = CARTESIAN_POINT ( 'NONE',  ( 5.928598010555855780, -1.317819122799672504, 1.596621505246295314 ) ) ;
#171864 = CARTESIAN_POINT ( 'NONE',  ( 4.529859951405730278, -1.186268397688082343, -1.517871513682719886 ) ) ;
#171865 = CARTESIAN_POINT ( 'NONE',  ( 1.177361486786612899, 1.528755565978222819, 1.314981834344926437 ) ) ;
#171866 = CARTESIAN_POINT ( 'NONE',  ( -10.45741655484220267, 11.09474082360439873, -0.7998128361456221525 ) ) ;
#171867 = CARTESIAN_POINT ( 'NONE',  ( 5.657495238652423097, 9.822437888394988548, 0.000000000000000000 ) ) ;
#171868 = LINE ( 'NONE', #41896, #980 ) ;
#171869 = CARTESIAN_POINT ( 'NONE',  ( 1.447511513890851864, 0.6336015447323711802, -2.097855558553712196 ) ) ;
#171870 = CARTESIAN_POINT ( 'NONE',  ( 5.197797600609998625, -0.6536857159176562293, 1.704833070275885598 ) ) ;
#171871 = CARTESIAN_POINT ( 'NONE',  ( -5.382750679825375251, 6.238629533673094585, -1.199719254218446718 ) ) ;
#171872 = CARTESIAN_POINT ( 'NONE',  ( 7.051649292883499953, 7.399548061218447437, -0.7216878364870317197 ) ) ;
#171874 = ADVANCED_FACE ( 'NONE', ( #155314 ), #131610, .T. ) ;
#171873 = CARTESIAN_POINT ( 'NONE',  ( 8.778014389843965759, 12.32843499053828928, 1.199719254218450271 ) ) ;
#171875 = CARTESIAN_POINT ( 'NONE',  ( -4.606738333593328072, 8.596554832492683929, 0.7998128361456281477 ) ) ;
#171876 = CARTESIAN_POINT ( 'NONE',  ( 5.867981556616276073, 5.740399992340775803, -0.7998128361456281477 ) ) ;
#171877 = CARTESIAN_POINT ( 'NONE',  ( 4.848976215542928792, 5.686169002002086970, 1.199719254218452047 ) ) ;
#171878 = ORIENTED_EDGE ( 'NONE', *, *, #132056, .T. ) ;
#171880 = CARTESIAN_POINT ( 'NONE',  ( 5.765890645310551399, 0.5801508929094216782, -1.927831218222434195 ) ) ;
#171879 = CARTESIAN_POINT ( 'NONE',  ( 2.630204301513817455, 0.2276190002089127917, 1.827071974840013269 ) ) ;
#171881 = CARTESIAN_POINT ( 'NONE',  ( 2.425563141628499064, 0.9819131520533967983, 2.078181775667542475 ) ) ;
#171882 = CARTESIAN_POINT ( 'NONE',  ( 0.3208626164478335374, -1.658663274457260473, -0.8439677346868018626 ) ) ;
#171883 = CARTESIAN_POINT ( 'NONE',  ( -6.175902666224832416, 7.163973517805802160, -1.199719254218446718 ) ) ;
#171884 = CARTESIAN_POINT ( 'NONE',  ( -4.326776511726841967, 7.444344370598463989, -0.9316558831735276547 ) ) ;
#171885 = CARTESIAN_POINT ( 'NONE',  ( 3.902528505893249733, -1.892296425594198750, -0.2755589300712790735 ) ) ;
#171886 = CARTESIAN_POINT ( 'NONE',  ( -9.917953063596627317, 11.52969898140628047, -1.199719254218441611 ) ) ;
#171887 = CARTESIAN_POINT ( 'NONE',  ( 0.6958625912084138720, -1.462932864358768459, -1.465259690088885014 ) ) ;
#171888 = CARTESIAN_POINT ( 'NONE',  ( -6.455090533882193782, 9.584670485287619002, -1.082531754730549967 ) ) ;
#171890 = CARTESIAN_POINT ( 'NONE',  ( 1.322894217037654085, -0.04941562205608432401, 1.870173573632450958 ) ) ;
#171889 = CARTESIAN_POINT ( 'NONE',  ( 3.087527064991796077, -0.8449906179068911172, 1.912563079267016297 ) ) ;
#171891 = CARTESIAN_POINT ( 'NONE',  ( 2.495470048217228065, 1.954872899240958972, 0.4925676099705801891 ) ) ;
#171892 = CARTESIAN_POINT ( 'NONE',  ( 9.273413882067330860, 9.921330405274451536, -0.7216878364870257245 ) ) ;
#171893 = VERTEX_POINT ( 'NONE', #187164 ) ;
#171894 = CARTESIAN_POINT ( 'NONE',  ( 0.6823417656249899377, 4.738541667008086655, -1.181850606188754593 ) ) ;
#171895 = CARTESIAN_POINT ( 'NONE',  ( 3.016877700344788416, -1.676514204431644783, 0.4670218299706177523 ) ) ;
#171896 = CARTESIAN_POINT ( 'NONE',  ( 3.985207087413062066, 6.736826471035503694, -1.199719254218452047 ) ) ;
#171897 = CARTESIAN_POINT ( 'NONE',  ( 0.000000000000000000, 3.300000000000025135, 1.561251128379126385E-14 ) ) ;
#171898 = CARTESIAN_POINT ( 'NONE',  ( 2.508071618744921238, -0.6595455166902574051, -1.594007932167235131 ) ) ;
#171899 = CARTESIAN_POINT ( 'NONE',  ( 2.648187065138879692, 0.7411268365287645432, 2.062558662443473523 ) ) ;
#171900 = CARTESIAN_POINT ( 'NONE',  ( 4.934293700819583073, 1.136511309699510308, -1.891595316245115788 ) ) ;
#171901 = CARTESIAN_POINT ( 'NONE',  ( -9.707245187965476418, 5.109025436760802563, -6.475459982491707400 ) ) ;
#171902 = SURFACE_SIDE_STYLE ('',( #105878 ) ) ;
#171903 = AXIS2_PLACEMENT_3D ( 'NONE', #114877, #100692, #148396 ) ;
#171904 = CARTESIAN_POINT ( 'NONE',  ( 4.047858276791187038, 1.568658707867241819, 1.501164901757213288 ) ) ;
#171905 = CARTESIAN_POINT ( 'NONE',  ( 2.226930044512597906, -0.0006860120723567450030, 1.825872481329051222 ) ) ;
#171906 = CARTESIAN_POINT ( 'NONE',  ( 1.506201402929115973, 8.679372656207114289, -2.542017642366260155 ) ) ;
#171907 = CARTESIAN_POINT ( 'NONE',  ( 4.874263506423556436, -2.101702868649154343, -0.2561063476108938475 ) ) ;
#171908 = CARTESIAN_POINT ( 'NONE',  ( 6.639320575229239019, 3.696696400505532942, 2.511109302898812956 ) ) ;
#171909 = ORIENTED_EDGE ( 'NONE', *, *, #33178, .F. ) ;
#171911 = CARTESIAN_POINT ( 'NONE',  ( 0.6823417656249882723, 1.738541667008083991, -1.181850606188749264 ) ) ;
#171910 = CARTESIAN_POINT ( 'NONE',  ( 4.933284685991359275, -1.619851263076008019, -1.622297632854825755 ) ) ;
#171912 = CARTESIAN_POINT ( 'NONE',  ( 0.000000000000000000, 0.4999999999999998890, 0.000000000000000000 ) ) ;
#171913 = CARTESIAN_POINT ( 'NONE',  ( 9.999301985278609806, 11.62460605670194447, 1.199719254218452047 ) ) ;
#171914 = AXIS2_PLACEMENT_3D ( 'NONE', #199971, #51619, #68893 ) ;
#171915 = CARTESIAN_POINT ( 'NONE',  ( -0.02259406399240069044, -1.896172633340575064, -0.9493637518730788649 ) ) ;
#171916 = CARTESIAN_POINT ( 'NONE',  ( -4.609409038966229666, 8.321468278861834378, -0.7216878364870267237 ) ) ;
#171917 = CARTESIAN_POINT ( 'NONE',  ( 5.205967797967541166, 5.175976640491323444, -0.7216878364870197293 ) ) ;
#171918 = CARTESIAN_POINT ( 'NONE',  ( -6.738039155867462604, 7.923762439009225389, 1.082531754730549967 ) ) ;
#171919 = CARTESIAN_POINT ( 'NONE',  ( 6.825078400183553384, 0.5907600490881077526, 1.908621492364571903 ) ) ;
#171920 = ORIENTED_EDGE ( 'NONE', *, *, #10408, .T. ) ;
#171921 = CARTESIAN_POINT ( 'NONE',  ( 5.625625018759272677, 0.3960990390993284205, 1.976956468877195894 ) ) ;
#171923 = CARTESIAN_POINT ( 'NONE',  ( 3.204023084367659813, 0.7466497159868844546, -1.922840047214324333 ) ) ;
#171922 = CARTESIAN_POINT ( 'NONE',  ( 5.015626762051672571, 7.938982758113895422, 1.199719254218462483 ) ) ;
#171925 = CARTESIAN_POINT ( 'NONE',  ( -0.1409997244345879974, 2.021982482314553131, -2.415666835770650778 ) ) ;
#171924 = LINE ( 'NONE', #92831, #29852 ) ;
#171926 = CARTESIAN_POINT ( 'NONE',  ( 5.370438244344566847, 5.438135171256338829, 0.000000000000000000 ) ) ;
#171928 = ADVANCED_FACE ( 'NONE', ( #38793 ), #171999, .T. ) ;
#171927 = CARTESIAN_POINT ( 'NONE',  ( 0.000000000000000000, -0.8968749995220406390, -3.793834371823813001 ) ) ;
#171929 = FACE_OUTER_BOUND ( 'NONE', #106901, .T. ) ;
#171930 = CARTESIAN_POINT ( 'NONE',  ( 5.824229312739954700, 2.111140916326431416, 0.5876101183235474812 ) ) ;
#171931 = CARTESIAN_POINT ( 'NONE',  ( 3.147111449167848019, 0.9091449406319618287, 1.799922684605055556 ) ) ;
#171932 = CARTESIAN_POINT ( 'NONE',  ( 3.227900028218867234, 1.797025815167479390, 0.4004103908350764573 ) ) ;
#171933 = COLOUR_RGB ( '', 0.72549020, 0.75294118, 0.79215686) ;
#171934 = ADVANCED_FACE ( 'NONE', ( #204459 ), #122270, .F. ) ;
#171935 = CARTESIAN_POINT ( 'NONE',  ( 5.982172092127724383, 8.002286745614243912, -1.599625672291262513 ) ) ;
#171936 =( LENGTH_UNIT ( ) NAMED_UNIT ( * ) SI_UNIT ( .MILLI., .METRE. ) );
#171937 = CARTESIAN_POINT ( 'NONE',  ( 6.563509198815889789, 0.3086105522638156184, -1.799150958419073909 ) ) ;
#171938 = CARTESIAN_POINT ( 'NONE',  ( -5.876569516519495551, 8.943415971659659292, 1.199719254218452047 ) ) ;
#171939 = CARTESIAN_POINT ( 'NONE',  ( 6.561402770032070286, 0.3947617697056918784, -2.227681008968500631 ) ) ;
#171940 = CARTESIAN_POINT ( 'NONE',  ( 1.664816323125760889, -1.488367931135538891, 1.490329786196037398 ) ) ;
#171941 = CARTESIAN_POINT ( 'NONE',  ( -6.069210040772897052, 7.109775131437022999, -1.199719254218453823 ) ) ;
#171942 = CARTESIAN_POINT ( 'NONE',  ( 8.423693512792301163, 8.722063941212843119, 0.7998128361456481317 ) ) ;
#171943 = CARTESIAN_POINT ( 'NONE',  ( 6.509323147892504657, 6.766834225395614411, 0.000000000000000000 ) ) ;
#171944 = B_SPLINE_CURVE_WITH_KNOTS ( 'NONE', 3,
 ( #136589, #143821, #177348, #91853, #92916, #61453, #86756, #59320, #125477, #54263, #109218, #120399, #186374, #104083, #21715, #163234 ),
 .UNSPECIFIED., .F., .F.,
 ( 4, 2, 2, 2, 2, 2, 2, 4 ),
 ( 0.000000000000000000, 0.001339152797105230700, 0.002678305594210461400, 0.004017458391315694051, 0.005356611188420927136, 0.006695763985526160221, 0.008034916782631393306, 0.01071322237684185948 ),
 .UNSPECIFIED. ) ;
#171945 = CARTESIAN_POINT ( 'NONE',  ( 8.378074386687003994, 15.00815134976859078, 15.76159487570644124 ) ) ;
#171946 = CARTESIAN_POINT ( 'NONE',  ( -5.713871673155502151, 8.753601821068331290, 1.199719254218452047 ) ) ;
#171947 = CARTESIAN_POINT ( 'NONE',  ( 5.124618875841165710, 8.922546421882614709, 1.040834085586084257E-14 ) ) ;
#171948 = CARTESIAN_POINT ( 'NONE',  ( 5.447554933476544292, 6.459834866240243834, 1.284201090641323040 ) ) ;
#171949 = CARTESIAN_POINT ( 'NONE',  ( -5.922214171070950606, 5.803671375871217286, -0.7998128361456291469 ) ) ;
#171950 = CARTESIAN_POINT ( 'NONE',  ( 4.359788498249434596, -1.718402401499378840, -1.407797849641032828 ) ) ;
#171951 = CARTESIAN_POINT ( 'NONE',  ( 2.589988673929614738, -2.185656584452956075, -0.1600571409424780822 ) ) ;
#171952 = CARTESIAN_POINT ( 'NONE',  ( -7.061099074618889304, 7.132370430010492868, -0.7998128361456291469 ) ) ;
#171953 = CARTESIAN_POINT ( 'NONE',  ( 6.883263157960373135, 2.058310207169287143, 2.252834201749584153 ) ) ;
#171954 = CARTESIAN_POINT ( 'NONE',  ( -6.283277845290492714, 6.295188672452495915, -0.7998128361456362523 ) ) ;
#171955 = CARTESIAN_POINT ( 'NONE',  ( 5.898874287966751950, 0.3812104124719677412, 1.924297140916144233 ) ) ;
#171956 =( BOUNDED_CURVE ( )  B_SPLINE_CURVE ( 2, ( #13506, #76375, #161916, #128427, #95860, #111082, #142482, #78508, #159764 ),
 .UNSPECIFIED., .F., .T. ) 
 B_SPLINE_CURVE_WITH_KNOTS ( ( 3, 2, 2, 2, 3 ),
 ( 0.6458333333333333703, 0.6527777777777777901, 0.6666666666666666297, 0.6805555555555555802, 0.6875000000000000000 ),
 .UNSPECIFIED. ) 
 CURVE ( )  GEOMETRIC_REPRESENTATION_ITEM ( )  RATIONAL_B_SPLINE_CURVE ( ( 0.9330127018922192983, 0.9330127018922198534, 1.000000000000000000, 0.8660254037844387076, 1.000000000000000000, 0.8660254037844387076, 1.000000000000000000, 0.9330127018922194093, 0.9330127018922194093 ) ) 
 REPRESENTATION_ITEM ( '' )  );
#171957 = CARTESIAN_POINT ( 'NONE',  ( -3.922244425448907279, 2.804391244181470011, -0.7749999999999944711 ) ) ;
#171958 = CARTESIAN_POINT ( 'NONE',  ( 1.364683531249988535, 1.863541667008086211, 0.7879004041258500513 ) ) ;
#171959 = CARTESIAN_POINT ( 'NONE',  ( -4.665414256878304577, 5.575976400180357118, -1.082531754730549967 ) ) ;
#171960 = CARTESIAN_POINT ( 'NONE',  ( -4.744990575102892905, 8.479646737687938085, 0.7216878364870458196 ) ) ;
#171961 = CARTESIAN_POINT ( 'NONE',  ( 4.517907016363444939, -0.5628432189327194912, 2.044499502628312371 ) ) ;
#171962 = CARTESIAN_POINT ( 'NONE',  ( -4.442231607132987925, 5.211633625523774960, -1.199719254218453823 ) ) ;
#171963 = ORIENTED_EDGE ( 'NONE', *, *, #103930, .T. ) ;
#171964 = CARTESIAN_POINT ( 'NONE',  ( 5.735289742212391850, -1.956171686333206816, 0.9202595734885756773 ) ) ;
#171965 = CARTESIAN_POINT ( 'NONE',  ( 6.277588818327314080, 7.282607361925381717, 1.199719254218462483 ) ) ;
#171966 = CARTESIAN_POINT ( 'NONE',  ( 4.563899478665734755, -1.199029595066217313, 1.397436126395680267 ) ) ;
#171967 = DIRECTION ( 'NONE',  ( 0.6250000000000057732, 7.952367169259533937E-16, 0.7806247497997951257 ) ) ;
#171968 = CARTESIAN_POINT ( 'NONE',  ( 1.364683531249986537, 1.717708333674749399, -0.7879004041258239610 ) ) ;
#171969 = CARTESIAN_POINT ( 'NONE',  ( 0.3623613221122607420, 0.1732436440316066917, -1.731762550003753898 ) ) ;
#171970 = CARTESIAN_POINT ( 'NONE',  ( 6.727182134110207379, 6.038252846411742425, 2.505853901327475874 ) ) ;
#171971 = CARTESIAN_POINT ( 'NONE',  ( 3.551873057100287223, 5.166937871415542283, 1.443375672974062551 ) ) ;
#171972 = CARTESIAN_POINT ( 'NONE',  ( 3.231779075379113131, 6.036511184309971689, 2.420000000000000373 ) ) ;
#171973 = CARTESIAN_POINT ( 'NONE',  ( 4.434552454296070145, 2.119417814153037316, 0.4246342833542292028 ) ) ;
#171974 = CARTESIAN_POINT ( 'NONE',  ( -5.220052836461385404, 6.048815383081766583, -1.199719254218446718 ) ) ;
#171975 = EDGE_CURVE ( 'NONE', #186977, #182051, #148729, .T. ) ;
#171976 = CARTESIAN_POINT ( 'NONE',  ( 6.309922681198771421, -1.704675833164914778, 1.076154833852351000 ) ) ;
#171977 = CARTESIAN_POINT ( 'NONE',  ( -6.670248387799091461, 10.72578085250020585, 0.000000000000000000 ) ) ;
#171978 = CARTESIAN_POINT ( 'NONE',  ( 2.958072429731006370, 2.151414462573512765, -0.2105227563667099733 ) ) ;
#171979 = CARTESIAN_POINT ( 'NONE',  ( 4.358636338273668365, -1.462950666040288006, 1.321578431016472654 ) ) ;
#171980 = CARTESIAN_POINT ( 'NONE',  ( 3.725721709451996322, -1.528540617003815383, -0.8183948105100163906 ) ) ;
#171981 = CARTESIAN_POINT ( 'NONE',  ( 0.7674258922165803076, 2.110627382301712540, -0.5898035449652739848 ) ) ;
#171982 = CARTESIAN_POINT ( 'NONE',  ( 0.9566253870459644482, 2.304745586553739400, -0.1165920040033379956 ) ) ;
#171983 = CARTESIAN_POINT ( 'NONE',  ( 3.831368270176987334, -1.905513148489059283, 0.7852520889023787420 ) ) ;
#171984 = CARTESIAN_POINT ( 'NONE',  ( 6.058146487192490603, -1.370253782545840293, 1.376481248621561182 ) ) ;
#171986 = ORIENTED_EDGE ( 'NONE', *, *, #137088, .T. ) ;
#171985 = CARTESIAN_POINT ( 'NONE',  ( -7.334597914868735025, 9.580116872145431728, -1.443375672974058777 ) ) ;
#171987 = CARTESIAN_POINT ( 'NONE',  ( -5.468734858265826837, 7.473552982767158070, 1.599625672291263179 ) ) ;
#171988 = CARTESIAN_POINT ( 'NONE',  ( -15.75000000000000000, 13.40000000000000036, -1.400000000000001910 ) ) ;
#171990 = VERTEX_POINT ( 'NONE', #74498 ) ;
#171989 = CARTESIAN_POINT ( 'NONE',  ( -4.625266680917477835, 5.425174544939014964, -1.199719254218453823 ) ) ;
#171991 = CARTESIAN_POINT ( 'NONE',  ( -8.337901282280023807, 8.829899038855916871, 0.7216878364870438212 ) ) ;
#171992 = CARTESIAN_POINT ( 'NONE',  ( 3.452368941479638131, 2.206952907609287973, 0.002057427529567057434 ) ) ;
#171993 = CARTESIAN_POINT ( 'NONE',  ( -1.642778471874998480, -3.638541666188710444, 2.845375778867863303 ) ) ;
#171994 = ORIENTED_EDGE ( 'NONE', *, *, #183399, .T. ) ;
#171995 = CARTESIAN_POINT ( 'NONE',  ( 1.023987020198445341, 0.9106972337104453086, 1.622782493823480943 ) ) ;
#171996 = CARTESIAN_POINT ( 'NONE',  ( -0.02919842301641033255, 0.7163969788333038879, -2.157531187298274311 ) ) ;
#171997 =( NAMED_UNIT ( * ) SI_UNIT ( $, .STERADIAN. ) SOLID_ANGLE_UNIT ( ) );
#171998 = CARTESIAN_POINT ( 'NONE',  ( -9.492545994383801755, -8.199730735665985648, 0.3846410972798168237 ) ) ;
#172001 = VECTOR ( 'NONE', #205709, 1000.000000000000000 ) ;
#172000 = CARTESIAN_POINT ( 'NONE',  ( -0.4330588727801884530, -9.006862915010128035, 9.570206894979145673 ) ) ;
#171999 = SPHERICAL_SURFACE ( 'NONE', #156173, 0.08000000000000000167 ) ;
#172002 = CARTESIAN_POINT ( 'NONE',  ( 6.122987604524110949, -1.732013368603693593, 0.6248225064409973495 ) ) ;
#172003 = VERTEX_POINT ( 'NONE', #123340 ) ;
#172004 = CARTESIAN_POINT ( 'NONE',  ( 2.465760480296646850, 2.021364445465044124, -0.4007626210408669620 ) ) ;
#172005 = CARTESIAN_POINT ( 'NONE',  ( 5.007715329123863766E-16, 0.8281250003414059035, -1.570758158831786266 ) ) ;
#172006 = CARTESIAN_POINT ( 'NONE',  ( -5.357443255694392725, 9.402100898285455699, 0.000000000000000000 ) ) ;
#172007 = CARTESIAN_POINT ( 'NONE',  ( 11.94980361058169116, 10.89999999999999858, 1.099999999999994982 ) ) ;
#172008 = CARTESIAN_POINT ( 'NONE',  ( 4.304877467538922531, 4.981110786005563007, 1.199719254218464037 ) ) ;
#172009 = CARTESIAN_POINT ( 'NONE',  ( 1.182575006203628210, -2.010449142642761089, -0.4523898644508434486 ) ) ;
#172011 = CARTESIAN_POINT ( 'NONE',  ( 5.179192671508887180, 1.240781939916297372, 1.360553736468192554 ) ) ;
#172010 = CARTESIAN_POINT ( 'NONE',  ( 1.333477130265051214, 8.249568609204947833, 9.911050286642563378 ) ) ;
#172012 = CARTESIAN_POINT ( 'NONE',  ( 6.714312387265682247, 8.856450423275211037, 1.599625672291281386 ) ) ;
#172013 = CARTESIAN_POINT ( 'NONE',  ( -4.457598643843001973, 8.422558527783969851, 0.000000000000000000 ) ) ;
#172014 = B_SPLINE_CURVE_WITH_KNOTS ( 'NONE', 3,
 ( #128769, #213113, #179578, #97274, #208848, #210980 ),
 .UNSPECIFIED., .F., .F.,
 ( 4, 2, 4 ),
 ( 0.001251957608719239234, 0.001565178843344208022, 0.001878400077969176376 ),
 .UNSPECIFIED. ) ;
#172015 = FACE_OUTER_BOUND ( 'NONE', #40243, .T. ) ;
#172016 = CARTESIAN_POINT ( 'NONE',  ( 4.002700589841681200, -0.6913439845411989415, -2.095861086919461602 ) ) ;
#172017 = CARTESIAN_POINT ( 'NONE',  ( 6.714178486276241919, -1.057601618853749148, -1.999996817866441123 ) ) ;
#172018 = CARTESIAN_POINT ( 'NONE',  ( -6.399085315970151733, 7.528316292462387871, -1.082531754730544860 ) ) ;
#172019 = CARTESIAN_POINT ( 'NONE',  ( 0.3340484552533556362, -1.024938778295768849, -1.614363347046356756 ) ) ;
#172020 = CARTESIAN_POINT ( 'NONE',  ( 0.8840003597419334724, -2.016708404047353742, 0.004841148455551891328 ) ) ;
#172021 = CARTESIAN_POINT ( 'NONE',  ( 7.634649897826745857, 8.079715433652276957, 0.7216878364870267237 ) ) ;
#172022 = DIRECTION ( 'NONE',  ( -0.000000000000000000, -1.000000000000000000, -0.000000000000000000 ) ) ;
#172023 = CARTESIAN_POINT ( 'NONE',  ( -0.08000000000000714873, -5.907420853759270507, 10.99970695577494872 ) ) ;
#172024 = CARTESIAN_POINT ( 'NONE',  ( 1.813763795902409548, 4.000000000000003553, -0.4500000000000250466 ) ) ;
#172025 = CARTESIAN_POINT ( 'NONE',  ( 2.131529507118444133, -1.219933349377068099, -1.418231869465089057 ) ) ;
#172026 = AXIS2_PLACEMENT_3D ( 'NONE', #168611, #3949, #99360 ) ;
#172027 = CARTESIAN_POINT ( 'NONE',  ( 2.430875351317234756, -1.673853735218135741, 1.124246214196801485 ) ) ;
#172029 = CARTESIAN_POINT ( 'NONE',  ( 6.639320575229257670, 3.688898292602959650, 2.617366112374151399 ) ) ;
#172028 = CARTESIAN_POINT ( 'NONE',  ( 1.364683531249988757, 1.134375000341421247, 0.000000000000000000 ) ) ;
#172030 = B_SPLINE_CURVE_WITH_KNOTS ( 'NONE', 3,
 ( #50104, #53297, #186488, #116224, #182216, #17567 ),
 .UNSPECIFIED., .F., .F.,
 ( 4, 2, 4 ),
 ( 0.000000000000000000, 0.0003239988925529258120, 0.0006479977851058516241 ),
 .UNSPECIFIED. ) ;
#172032 = CARTESIAN_POINT ( 'NONE',  ( 4.740906146847382985, 0.3592350385927112200, 2.075039481041524247 ) ) ;
#172031 = CARTESIAN_POINT ( 'NONE',  ( -7.934546212495630968, 10.28005655271014795, -1.599625672291263179 ) ) ;
#172033 = CARTESIAN_POINT ( 'NONE',  ( 8.284195553149872993, 9.623648552551724578, -1.199719254218445830 ) ) ;
#172035 = CARTESIAN_POINT ( 'NONE',  ( -9.027031348600448979, 9.425958082989001952, 1.040834085586084257E-14 ) ) ;
#172034 = CARTESIAN_POINT ( 'NONE',  ( 5.422335090822693715, 5.290755458906732933, 0.000000000000000000 ) ) ;
#172036 = CARTESIAN_POINT ( 'NONE',  ( -0.2834499523633308704, -6.554910290221268809, -9.477100695693451371 ) ) ;
#172037 = CARTESIAN_POINT ( 'NONE',  ( 4.482678814652188315, -1.316266026504675057, 1.532109124154117596 ) ) ;
#172038 = CARTESIAN_POINT ( 'NONE',  ( -1.201851678989727383E-14, 4.446875000341417916, -1.575800808251660134 ) ) ;
#172039 = CARTESIAN_POINT ( 'NONE',  ( 6.584441931359013900, 1.190761153509769521, -1.684076666428784064 ) ) ;
#172040 = CARTESIAN_POINT ( 'NONE',  ( 8.270110514656021650, 11.63191745286530576, 1.082531754730557072 ) ) ;
#172041 = CARTESIAN_POINT ( 'NONE',  ( 4.622454487542248636, 1.333869025858843704, -1.700861402727947391 ) ) ;
#172042 = CARTESIAN_POINT ( 'NONE',  ( 6.821687566331318564, 7.987665577921906568, 1.199719254218452935 ) ) ;
#172043 = CARTESIAN_POINT ( 'NONE',  ( 1.364683531249988757, -0.5531249996585801965, 0.000000000000000000 ) ) ;
#172045 = FILL_AREA_STYLE ('',( #22562 ) ) ;
#172044 = CARTESIAN_POINT ( 'NONE',  ( 6.099189001301251523, 8.209082816308541197, 1.599625672291268286 ) ) ;
#172046 = CARTESIAN_POINT ( 'NONE',  ( 7.334597914868727919, 9.580116872145431728, -1.443375672974058777 ) ) ;
#172048 = CARTESIAN_POINT ( 'NONE',  ( -0.4382560683119281486, -7.700000000000008171, 10.99126615174920474 ) ) ;
#172047 = CARTESIAN_POINT ( 'NONE',  ( 2.401036581340802556, 0.4739146800750834165, 2.118683212603386767 ) ) ;
#172050 = CARTESIAN_POINT ( 'NONE',  ( 1.329379181053941483, 0.9071106928158387817, -1.602193565413398968 ) ) ;
#172049 = CARTESIAN_POINT ( 'NONE',  ( -4.772106882330223954, 8.511282429453158827, -0.7216878364870267237 ) ) ;
#172051 = CARTESIAN_POINT ( 'NONE',  ( -1.364683531250012516, 2.280208333674751842, 0.7879004041258379498 ) ) ;
#172052 = CARTESIAN_POINT ( 'NONE',  ( 2.700927432832851860, 1.852951201923001223, 1.169960570980829839 ) ) ;
#172053 = DIRECTION ( 'NONE',  ( 1.000000000000000000, -0.000000000000000000, -0.000000000000000000 ) ) ;
#172054 = CARTESIAN_POINT ( 'NONE',  ( 3.626065245518626412, -1.345661663401491293, -1.818709669598504997 ) ) ;
#172055 = CARTESIAN_POINT ( 'NONE',  ( -5.259673527097670664, 8.223703984000886535, -1.199719254218446718 ) ) ;
#172056 = DIRECTION ( 'NONE',  ( -3.330669073875725015E-16, 0.000000000000000000, 1.000000000000000000 ) ) ;
#172057 = CARTESIAN_POINT ( 'NONE',  ( 6.357275476766607980, 6.835366726881293431, -0.6123070361637416026 ) ) ;
#172058 = CARTESIAN_POINT ( 'NONE',  ( -0.7500000000000006661, 13.70833333333333570, -1.299038105676657340 ) ) ;
#172059 = CARTESIAN_POINT ( 'NONE',  ( 5.153507786970260796, 7.105788066255672497, -1.443375672974078761 ) ) ;
#172060 = CARTESIAN_POINT ( 'NONE',  ( 5.132005351226563761, 0.9095619001311354701, -1.517971549226182715 ) ) ;
#172061 = CIRCLE ( 'NONE', #185789, 0.07999999999999948819 ) ;
#172062 = CARTESIAN_POINT ( 'NONE',  ( 6.936968151686458306, 11.24487994360957188, 0.7998128361456462443 ) ) ;
#172063 = CARTESIAN_POINT ( 'NONE',  ( 1.905437291041052195, 1.750494195096408800, 1.170504954829422850 ) ) ;
#172065 = CARTESIAN_POINT ( 'NONE',  ( -1.402160292154681736E-14, 1.337500000000025446, -1.732050807568863648 ) ) ;
#172064 = CARTESIAN_POINT ( 'NONE',  ( -8.012344526598182026E-15, 10.79687500034139624, -1.575800808251669460 ) ) ;
#172066 = CARTESIAN_POINT ( 'NONE',  ( 0.8011416495431540330, -1.691081937322042483, 1.009368880822520298 ) ) ;
#172067 = CARTESIAN_POINT ( 'NONE',  ( -3.526002468005825286, 6.271364091718859335, -1.199719254218450271 ) ) ;
#172068 = CARTESIAN_POINT ( 'NONE',  ( 0.1390251588108057101, -0.1389306544097475005, -1.930426113910483688 ) ) ;
#172070 = ORIENTED_EDGE ( 'NONE', *, *, #122310, .F. ) ;
#172069 = CARTESIAN_POINT ( 'NONE',  ( 5.361500737056818622, -1.433101695931580100, -1.108104203189824277 ) ) ;
#172071 = CARTESIAN_POINT ( 'NONE',  ( 7.971831135155394321, 8.402817200543854170, -0.7216878364870267237 ) ) ;
#172073 = EDGE_CURVE ( 'NONE', #199311, #210868, #59363, .T. ) ;
#172072 = CIRCLE ( 'NONE', #96020, 3.150000000000000799 ) ;
#172074 = CARTESIAN_POINT ( 'NONE',  ( 4.750782166719051069, -1.502237938222051650, 1.114538048626475986 ) ) ;
#172075 = ORIENTED_EDGE ( 'NONE', *, *, #33910, .T. ) ;
#172076 = CARTESIAN_POINT ( 'NONE',  ( 4.364170320198999420, -2.065056620294950740, 0.1471644388686063065 ) ) ;
#172077 = CARTESIAN_POINT ( 'NONE',  ( -1.225000000000014078, 1.479166666666654972, -0.7072540797573018123 ) ) ;
#172078 = CARTESIAN_POINT ( 'NONE',  ( -5.112833325684916552, 7.058334528089422300, -1.443375672974066548 ) ) ;
#172079 = CARTESIAN_POINT ( 'NONE',  ( 8.263858322729371153, 9.599921783727809910, -1.199719254218446718 ) ) ;
#172080 = CARTESIAN_POINT ( 'NONE',  ( -7.316596452869116973, 11.68777962832266049, 0.7998128361456481317 ) ) ;
#172081 = CARTESIAN_POINT ( 'NONE',  ( 8.005163354226054295, 8.304055099544019214, 0.000000000000000000 ) ) ;
#172082 = CARTESIAN_POINT ( 'NONE',  ( -4.334696837225959776, 7.118203947705221246, -1.092094898011612747 ) ) ;
#172083 = CARTESIAN_POINT ( 'NONE',  ( -0.6823417656250246877, -0.4489583329919111243, 1.181850606188755259 ) ) ;
#172084 = COLOUR_RGB ( '', 0.66274510, 0.83137255, 0.94901961) ;
#172085 = CARTESIAN_POINT ( 'NONE',  ( 1.499999999999987121, 1.045833333333352266, -0.8660254037844253849 ) ) ;
#172087 = CARTESIAN_POINT ( 'NONE',  ( 4.852928918687680948, 7.749168607522574526, 1.199719254218462483 ) ) ;
#172086 = CARTESIAN_POINT ( 'NONE',  ( 5.248475795274027078, -1.946838731704622072, -0.2419367024937419397 ) ) ;
#172088 = CARTESIAN_POINT ( 'NONE',  ( 1.792342068719571468, -1.899328565777322231, 0.6766080823841430503 ) ) ;
#172089 = ADVANCED_FACE ( 'NONE', ( #190357 ), #108128, .T. ) ;
#172090 = CARTESIAN_POINT ( 'NONE',  ( -0.1108833634136767443, 0.0002062650063822807356, -1.896853557917008271 ) ) ;
#172091 = CARTESIAN_POINT ( 'NONE',  ( 6.639320575229276322, 3.701785489019034259, 2.411212692025939131 ) ) ;
#172092 = CARTESIAN_POINT ( 'NONE',  ( 6.539320575229249144, 0.007148032025052972194, 1.896977914940492393 ) ) ;
#172093 = CARTESIAN_POINT ( 'NONE',  ( 2.055717040066493695, 1.865871300129381183, -0.1328275987748789300 ) ) ;
#172094 = CARTESIAN_POINT ( 'NONE',  ( 0.6823417656249899377, 5.676041667008087543, -1.181850606188754593 ) ) ;
#172095 = CARTESIAN_POINT ( 'NONE',  ( -7.309817376062285099, 11.67987070538135264, 0.000000000000000000 ) ) ;
#172097 = CARTESIAN_POINT ( 'NONE',  ( 2.900141384978659698, -1.046112932010187624, -1.840686247649555796 ) ) ;
#172096 = CARTESIAN_POINT ( 'NONE',  ( -4.690757960648240577, 6.495636925554817864, 1.443375672974064550 ) ) ;
#172098 = CARTESIAN_POINT ( 'NONE',  ( 3.615147460157889903, 7.348606074266929689, 0.4009180521483968196 ) ) ;
#172099 = CARTESIAN_POINT ( 'NONE',  ( 4.791501694037465953, -1.894250426384593844, 0.8359921707915063394 ) ) ;
#172100 = CARTESIAN_POINT ( 'NONE',  ( 5.668190738965027897, 8.770583741171307679, -1.199719254218452047 ) ) ;
#172102 = CARTESIAN_POINT ( 'NONE',  ( 6.620655732516668834, 6.034240673559561507, 2.768629221164942145 ) ) ;
#172101 = CARTESIAN_POINT ( 'NONE',  ( 1.593426000515285157, -0.7013512306414200204, 1.969750900790192549 ) ) ;
#172104 = ORIENTED_EDGE ( 'NONE', *, *, #63903, .F. ) ;
#172103 = CARTESIAN_POINT ( 'NONE',  ( 6.352569596097208837, 0.5757234290239590102, 1.732508359437078482 ) ) ;
#172105 = CARTESIAN_POINT ( 'NONE',  ( 7.721532178182734185, 8.967207948423393304, 1.199719254218462483 ) ) ;
#172106 = CARTESIAN_POINT ( 'NONE',  ( 0.006200025029510404170, 14.55606717504231362, 11.95073768095064004 ) ) ;
#172107 = DIRECTION ( 'NONE',  ( 0.000000000000000000, 0.000000000000000000, 1.000000000000000000 ) ) ;
#172108 = CARTESIAN_POINT ( 'NONE',  ( -9.915825940873133959, 4.173851563286998356, 6.175246223022227809 ) ) ;
#172109 = CARTESIAN_POINT ( 'NONE',  ( 8.256552360598020002, 8.734991963560254646, -0.7216878364870267237 ) ) ;
#172110 = CARTESIAN_POINT ( 'NONE',  ( -1.284279953904125193, 10.64264068711930733, 0.7750000000000117906 ) ) ;
#172111 = CARTESIAN_POINT ( 'NONE',  ( 6.006500814222540008, -1.903516144586704151, -0.1827706444143817055 ) ) ;
#172112 = CARTESIAN_POINT ( 'NONE',  ( -9.332089804907933939, 9.781859615347734405, 1.040834085586084257E-14 ) ) ;
#172113 = CARTESIAN_POINT ( 'NONE',  ( 5.843727902690005749, 6.776436293681846301, -1.199719254218445830 ) ) ;
#172114 = CARTESIAN_POINT ( 'NONE',  ( -7.346809171966454777, -6.836568542494980250, -8.002408263930250953 ) ) ;
#172115 = CARTESIAN_POINT ( 'NONE',  ( 10.73535870392234237, 11.41900666419791399, 0.000000000000000000 ) ) ;
#172116 = CARTESIAN_POINT ( 'NONE',  ( -1.000000000000014433, 6.468705557303653819, 4.925226524755080604 ) ) ;
#172117 = CARTESIAN_POINT ( 'NONE',  ( 4.546061579283848353, 4.198160018786257552, -0.7998128361456211532 ) ) ;
#172118 = EDGE_LOOP ( 'NONE', ( #181888, #24648, #211679, #189821, #99122, #83662, #50773, #60501 ) ) ;
#172119 = CARTESIAN_POINT ( 'NONE',  ( 5.747672784407955149, 1.986098415631059932, -0.3474865836668520336 ) ) ;
#172120 = CARTESIAN_POINT ( 'NONE',  ( -4.048498009130195641, 7.637439037563395594, 0.4772038154421194278 ) ) ;
#172121 = CARTESIAN_POINT ( 'NONE',  ( 10.96384327792182134, -7.754568858751050620, -0.4817895937885937618 ) ) ;
#172122 = CARTESIAN_POINT ( 'NONE',  ( 0.1399997263885795484, 5.723012109828673921, -2.593777676649943409 ) ) ;
#172123 = CARTESIAN_POINT ( 'NONE',  ( -4.121315508874262790, 6.791656612786516334, -1.082531754730549967 ) ) ;
#172124 = CARTESIAN_POINT ( 'NONE',  ( 2.361091307074211887, 5.906356958228550447, 0.7998128361456462443 ) ) ;
#172125 = CARTESIAN_POINT ( 'NONE',  ( 3.590635625024854338, 1.920399590389043620, 0.4359694148904534328 ) ) ;
#172126 = CARTESIAN_POINT ( 'NONE',  ( 4.939077454563308933, -1.704950310733845065, -1.076300583479961048 ) ) ;
#172127 = CARTESIAN_POINT ( 'NONE',  ( -7.718669524881690336, 7.899535955317097624, 0.7998128361456462443 ) ) ;
#172128 = FACE_OUTER_BOUND ( 'NONE', #32655, .T. ) ;
#172129 = CARTESIAN_POINT ( 'NONE',  ( 5.085950966588184130, -2.174626929279792176, -0.2704268894557353975 ) ) ;
#172130 = CARTESIAN_POINT ( 'NONE',  ( 0.000000000000000000, -6.836568542494925182, 0.000000000000000000 ) ) ;
#172131 = CARTESIAN_POINT ( 'NONE',  ( 2.907156789938716290, 1.626457378340099069, 1.032021673995666911 ) ) ;
#172132 = CARTESIAN_POINT ( 'NONE',  ( -7.648771216403934758, 12.07531685244661723, -0.7998128361456291469 ) ) ;
#172133 = CARTESIAN_POINT ( 'NONE',  ( -0.02948999725182511675, 6.948707995275583471, -2.521364601437687369 ) ) ;
#172134 = CARTESIAN_POINT ( 'NONE',  ( 0.1357705729100426029, -2.015811560716780360, 0.8986578214904349382 ) ) ;
#172135 = CARTESIAN_POINT ( 'NONE',  ( -5.600682673023330338, 15.51843887165996705, -10.62222671273976538 ) ) ;
#172137 = ADVANCED_FACE ( 'NONE', ( #192489 ), #160010, .F. ) ;
#172136 = CARTESIAN_POINT ( 'NONE',  ( -8.012344526598182026E-15, 13.04687500034139980, -1.575800808251669460 ) ) ;
#172138 = CARTESIAN_POINT ( 'NONE',  ( 5.820528018968444961, 5.685037531751635953, 0.7998128361456341429 ) ) ;
#172139 =( BOUNDED_CURVE ( )  B_SPLINE_CURVE ( 2, ( #103933, #85531, #41884, #8279, #74363, #107995, #25591, #80763, #61308 ),
 .UNSPECIFIED., .F., .T. ) 
 B_SPLINE_CURVE_WITH_KNOTS ( ( 3, 2, 2, 2, 3 ),
 ( 0.4375000000000000000, 0.4444444444444444198, 0.4583333333333333148, 0.4722222222222222099, 0.4791666666666666852 ),
 .UNSPECIFIED. ) 
 CURVE ( )  GEOMETRIC_REPRESENTATION_ITEM ( )  RATIONAL_B_SPLINE_CURVE ( ( 0.9330127018922194093, 0.9330127018922194093, 1.000000000000000000, 0.8660254037844387076, 1.000000000000000000, 0.8660254037844387076, 1.000000000000000000, 0.9330127018922190762, 0.9330127018922194093 ) ) 
 REPRESENTATION_ITEM ( '' )  );
#172140 = CARTESIAN_POINT ( 'NONE',  ( -6.511106444359256784, 5.279176164187211917, -2.499999999999995115 ) ) ;
#172141 = CARTESIAN_POINT ( 'NONE',  ( 4.421367491832268293, 7.211993602896056288, 1.082531754730549078 ) ) ;
#172142 = ORIENTED_EDGE ( 'NONE', *, *, #15512, .T. ) ;
#172144 = CARTESIAN_POINT ( 'NONE',  ( 2.490887342608373078, -1.927107516443892221, -0.5821121120333644372 ) ) ;
#172143 = CARTESIAN_POINT ( 'NONE',  ( 6.444863656277017405, -1.483217659742748218, -1.090817886357238198 ) ) ;
#172145 = CARTESIAN_POINT ( 'NONE',  ( 4.903846967696810388, 0.3865712588492843937, 2.265520236764162920 ) ) ;
#172147 = CARTESIAN_POINT ( 'NONE',  ( 2.975287861635074194, -0.1872683251897942214, 1.851525965346143554 ) ) ;
#172146 = CARTESIAN_POINT ( 'NONE',  ( -7.445362632559989535, 8.715286488521982733, 1.199719254218452047 ) ) ;
#172148 = CARTESIAN_POINT ( 'NONE',  ( -1.642778471875000035, -0.5177083328553738761, -2.845375778867859751 ) ) ;
#172149 = CARTESIAN_POINT ( 'NONE',  ( 0.000000000000000000, -2.000000000000001776, 0.000000000000000000 ) ) ;
#172150 = CARTESIAN_POINT ( 'NONE',  ( 6.187759705938407073, 1.828009178079874841, -0.5617473972939349691 ) ) ;
#172151 = CARTESIAN_POINT ( 'NONE',  ( -5.747767057189642870, 8.793146435774861658, -1.199719254218440723 ) ) ;
#172152 = CARTESIAN_POINT ( 'NONE',  ( -5.316205630334276400, 5.374863788244313767, -0.7216878364870338292 ) ) ;
#172153 = CARTESIAN_POINT ( 'NONE',  ( 6.462449937854951365, -1.911777437574797345, -0.8467615847161328313 ) ) ;
#172154 = CARTESIAN_POINT ( 'NONE',  ( 5.097502569058200983, 6.970172302033127210, -1.443375672974051449 ) ) ;
#172155 = EDGE_LOOP ( 'NONE', ( #49006, #42294, #209640, #186358 ) ) ;
#172156 = DIRECTION ( 'NONE',  ( -0.000000000000000000, -1.000000000000000000, -0.000000000000000000 ) ) ;
#172157 = CARTESIAN_POINT ( 'NONE',  ( 0.4626273691814121181, 3.108307088186288869, -0.4053073865230417128 ) ) ;
#172158 = CARTESIAN_POINT ( 'NONE',  ( 6.674431755534494748, -1.054235620458108702, 1.365612558063566073 ) ) ;
#172159 = CARTESIAN_POINT ( 'NONE',  ( -6.274726165026268454, 6.214935368819085149, 0.7998128361456341429 ) ) ;
#172160 = CARTESIAN_POINT ( 'NONE',  ( 2.092031233620697872, -0.3790036544207425195, 1.692025817237676311 ) ) ;
#172161 = CARTESIAN_POINT ( 'NONE',  ( -6.730388996436583504, 14.55213502910268453, 9.891260588912654583 ) ) ;
#172162 = CARTESIAN_POINT ( 'NONE',  ( 0.4917504562595223505, 10.46609003534429405, -2.420000000000000373 ) ) ;
#172163 = CARTESIAN_POINT ( 'NONE',  ( -5.747767057189642870, 8.793146435774861658, -1.199719254218440723 ) ) ;
#172164 = AXIS2_PLACEMENT_3D ( 'NONE', #90400, #27518, #108842 ) ;
#172165 = DIRECTION ( 'NONE',  ( 1.000000000000000000, 0.000000000000000000, 0.000000000000000000 ) ) ;
#172166 = CARTESIAN_POINT ( 'NONE',  ( 0.3036855567021545244, -1.598042064648269811, -1.315789336611736138 ) ) ;
#172167 = CARTESIAN_POINT ( 'NONE',  ( 5.795480788678070816, 1.385457615097264394, 1.189071861804301466 ) ) ;
#172168 = CARTESIAN_POINT ( 'NONE',  ( 2.940231979924610606, -1.012623612260230566, 1.680088604585870060 ) ) ;
#172169 = CARTESIAN_POINT ( 'NONE',  ( -3.837393226078555042, 7.491049807724315279, 0.05206913311947320572 ) ) ;
#172170 = CARTESIAN_POINT ( 'NONE',  ( -10.49131193887636826, 11.13428543831092909, 1.040834085586084257E-14 ) ) ;
#172171 = CARTESIAN_POINT ( 'NONE',  ( 5.587931867126699537, 9.671004278289832001, -0.7998128361456291469 ) ) ;
#172172 = CARTESIAN_POINT ( 'NONE',  ( 3.580828998445852562, -1.422877522674294681, 1.572404880189558485 ) ) ;
#172173 = CARTESIAN_POINT ( 'NONE',  ( -4.460269349215930212, 4.305995116947750390, 1.214306433183764966E-14 ) ) ;
#172174 = SURFACE_STYLE_USAGE ( .BOTH. , #106150 ) ;
#172176 = AXIS2_PLACEMENT_3D ( 'NONE', #61349, #45123, #111233 ) ;
#172175 = AXIS2_PLACEMENT_3D ( 'NONE', #117801, #70016, #2881 ) ;
#172177 = CARTESIAN_POINT ( 'NONE',  ( 1.727480438796034745, 0.1563249218069600044, -2.064440809470533544 ) ) ;
#172179 = CARTESIAN_POINT ( 'NONE',  ( -6.009258394948636914E-15, 14.96875000068279427, -1.732050807568875195 ) ) ;
#172178 = CARTESIAN_POINT ( 'NONE',  ( -11.94105721237523277, 10.90000000000000036, 1.187919463087245386 ) ) ;
#172181 = VERTEX_POINT ( 'NONE', #211939 ) ;
#172180 = CARTESIAN_POINT ( 'NONE',  ( 4.055513949679364849, -1.932427950605047018, 1.095304516859375799 ) ) ;
#172182 = CARTESIAN_POINT ( 'NONE',  ( 1.706133075696044221, 2.146806223983906747, 0.8221538945956968769 ) ) ;
#172184 = CARTESIAN_POINT ( 'NONE',  ( 6.737180511075488987, -0.09540316190201691970, -2.060463472160603882 ) ) ;
#172183 = CARTESIAN_POINT ( 'NONE',  ( 7.768458830950378591, 12.00702636951006497, 1.040834085586084257E-14 ) ) ;
#172186 = CARTESIAN_POINT ( 'NONE',  ( 1.737499999999999378, -0.8166666666666668739, -3.009438278150925683 ) ) ;
#172185 = CARTESIAN_POINT ( 'NONE',  ( 5.252858170651868441, 5.093032385374103299, -0.7998128361456481317 ) ) ;
#172187 = EDGE_CURVE ( 'NONE', #78339, #206450, #83466, .T. ) ;
#172188 = FACE_OUTER_BOUND ( 'NONE', #197559, .T. ) ;
#172189 = CARTESIAN_POINT ( 'NONE',  ( -10.96499746917716500, -5.350147675656139690, 0.1749484593404612431 ) ) ;
#172190 = CARTESIAN_POINT ( 'NONE',  ( -1.850000000000000089, 2.265195232789710231E-16, 0.5999999999999969802 ) ) ;
#172191 = CARTESIAN_POINT ( 'NONE',  ( 3.006014587165442453, -0.7710369221427433306, 1.750240277048662030 ) ) ;
#172192 = CARTESIAN_POINT ( 'NONE',  ( -0.2104748580754183529, 0.2283854016844401591, -2.137091067173245929 ) ) ;
#172193 = CARTESIAN_POINT ( 'NONE',  ( 4.647282941162062642, -1.334376716645750971, -1.092789356466111972 ) ) ;
#172194 = CARTESIAN_POINT ( 'NONE',  ( 2.518767860054324625, 0.2516336668320385828, 2.000731427934741902 ) ) ;
#172195 = CARTESIAN_POINT ( 'NONE',  ( 4.342621253679892490, 0.5038326875656545800, -2.242679570940506739 ) ) ;
#172196 = CARTESIAN_POINT ( 'NONE',  ( 3.690934243623856581, -0.4369955660583099699, -2.219648300357620396 ) ) ;
#172197 = CARTESIAN_POINT ( 'NONE',  ( 5.901026713257129686, 1.722607154707327615, -1.211383145191318400 ) ) ;
#172198 = CARTESIAN_POINT ( 'NONE',  ( -6.292392690518209264, 8.434487120394948079, -1.443375672974066548 ) ) ;
#172199 = CARTESIAN_POINT ( 'NONE',  ( 4.956192180792302615, 0.6771475221719803761, 1.635265836519818716 ) ) ;
#172200 = EDGE_CURVE ( 'NONE', #201551, #49868, #152739, .T. ) ;
#172202 = CARTESIAN_POINT ( 'NONE',  ( 0.4984804791418595560, -0.7777643670432095035, -2.156416217022334436 ) ) ;
#172201 = CARTESIAN_POINT ( 'NONE',  ( 7.225569521440261767, 7.394528961293920233, -0.7998128361456341429 ) ) ;
#172203 = CARTESIAN_POINT ( 'NONE',  ( 5.964778383650899407, 0.1308802983275309528, -1.836551591404868233 ) ) ;
#172204 = CARTESIAN_POINT ( 'NONE',  ( -4.959585264500673496, 4.680604318205876524, 1.214306433183764966E-14 ) ) ;
#172205 = CARTESIAN_POINT ( 'NONE',  ( 6.193348084369689310, -0.7418380161853587174, 2.062208804312585020 ) ) ;
#172206 = CARTESIAN_POINT ( 'NONE',  ( -4.298098390732130625, 4.973201863064262263, 1.199719254218462483 ) ) ;
#172207 = CARTESIAN_POINT ( 'NONE',  ( -11.33772463945037146, 10.19999999999998153, 3.599999999999999201 ) ) ;
#172208 = CARTESIAN_POINT ( 'NONE',  ( 5.723117673755029777, -1.870111591731966616, -0.8886290660751752224 ) ) ;
#172209 = CARTESIAN_POINT ( 'NONE',  ( 0.5500180045474002410, 0.9981291480291035745, 1.752136972055001518 ) ) ;
#172210 = CIRCLE ( 'NONE', #78803, 0.04999999999999991257 ) ;
#172211 = CARTESIAN_POINT ( 'NONE',  ( 0.7499999999999867883, -0.9020833326505162120, -1.299038105676652011 ) ) ;
#172212 = CARTESIAN_POINT ( 'NONE',  ( 4.846275584324886587, 1.921458954407113451, 0.1401587531122197583 ) ) ;
#172213 = CARTESIAN_POINT ( 'NONE',  ( 0.6823417656249934904, 9.942708333674735499, 1.181850606188764807 ) ) ;
#172214 = CARTESIAN_POINT ( 'NONE',  ( -2.657034918598338180, 6.043698471765932112, -0.7216878364870267237 ) ) ;
#172215 = CARTESIAN_POINT ( 'NONE',  ( 1.582608957317205522, 1.147345939325004283, 1.902073548153013327 ) ) ;
#172216 = VERTEX_POINT ( 'NONE', #178404 ) ;
#172218 = CARTESIAN_POINT ( 'NONE',  ( 4.963960565410041603, 8.060099936542098220, -1.154953748940761971 ) ) ;
#172217 = DIRECTION ( 'NONE',  ( 0.9446243521954068578, 0.000000000000000000, -0.3281536732072456997 ) ) ;
#172219 = CARTESIAN_POINT ( 'NONE',  ( 2.367870383881045981, 5.914265881169853856, 0.000000000000000000 ) ) ;
#172220 = CARTESIAN_POINT ( 'NONE',  ( -1.500000000000015099, 9.010416667349462116, -0.8660254037844309360 ) ) ;
#172221 = CARTESIAN_POINT ( 'NONE',  ( 0.000000000000000000, 6.999999999999999112, 0.000000000000000000 ) ) ;
#172222 = CARTESIAN_POINT ( 'NONE',  ( 3.904855289079228076, 2.800000000000017586, -0.7749999999999935829 ) ) ;
#172223 = CARTESIAN_POINT ( 'NONE',  ( 8.378575743120986630, 12.71882943370911789, 1.040834085586084257E-14 ) ) ;
#172225 = CARTESIAN_POINT ( 'NONE',  ( 1.469116868872882398, 1.728625619535430369, 0.9278086228877155950 ) ) ;
#172224 = AXIS2_PLACEMENT_3D ( 'NONE', #68172, #115945, #147336 ) ;
#172226 = CARTESIAN_POINT ( 'NONE',  ( 0.6823417656249882723, 2.738541667008084879, -1.181850606188749264 ) ) ;
#172227 = CARTESIAN_POINT ( 'NONE',  ( 0.4465194593917913846, 3.080450244942120719, -0.4155024747329958412 ) ) ;
#172228 = CARTESIAN_POINT ( 'NONE',  ( 6.830524215763060347, -1.208013408316032322, 1.546442907991877558 ) ) ;
#172229 = CARTESIAN_POINT ( 'NONE',  ( -8.188234707649510113, 11.64035869464474082, -1.199719254218446718 ) ) ;
#172230 = EDGE_CURVE ( 'NONE', #19248, #138713, #136092, .T. ) ;
#172231 = CARTESIAN_POINT ( 'NONE',  ( -4.229780737339226881, 7.878568593630327577, 1.040834085586084257E-14 ) ) ;
#172232 = CARTESIAN_POINT ( 'NONE',  ( 0.5150084580479041829, 1.557691122620246116, -1.641117935488043633 ) ) ;
#172234 = ORIENTED_EDGE ( 'NONE', *, *, #186461, .F. ) ;
#172233 = CARTESIAN_POINT ( 'NONE',  ( -5.368138756007025947, 8.350246751061767725, 1.199719254218452047 ) ) ;
#172235 = CARTESIAN_POINT ( 'NONE',  ( -1.602468905319636405E-14, -1.131249999317182064, -1.732050807568870754 ) ) ;
#172236 = CARTESIAN_POINT ( 'NONE',  ( 0.9658262494645246665, 0.9167188063998463754, 1.630421345857439475 ) ) ;
#172237 = CARTESIAN_POINT ( 'NONE',  ( 0.7208516900601771304, 1.708106959156988847, 0.2981761063507569198 ) ) ;
#172239 = CARTESIAN_POINT ( 'NONE',  ( 4.353197867323560288, 0.4795420089713005041, -2.138300074133951068 ) ) ;
#172238 = CARTESIAN_POINT ( 'NONE',  ( -0.6801582343750316451, 2.098958333674738608, -1.178068619123862515 ) ) ;
#172240 = CARTESIAN_POINT ( 'NONE',  ( 4.612551310933718618, -0.9822873175598394457, -2.088206479280288796 ) ) ;
#172241 = CARTESIAN_POINT ( 'NONE',  ( 0.09275324736048547181, -0.4491109574935348014, -2.018345435551980316 ) ) ;
#172242 = CARTESIAN_POINT ( 'NONE',  ( 2.501813746025891128, -0.7434988463325925556, -1.794173334931578712 ) ) ;
#172243 = CARTESIAN_POINT ( 'NONE',  ( -5.463572716182839351, 7.397254140345190798, 1.443375672974064550 ) ) ;
#172244 = CARTESIAN_POINT ( 'NONE',  ( -1.387358672527289727, 7.251968950354596544, -4.302625267139392307 ) ) ;
#172245 = CARTESIAN_POINT ( 'NONE',  ( 5.695592476053609410, 1.958610405324921588, -0.8133567297157192622 ) ) ;
#172246 = FILL_AREA_STYLE ('',( #8657 ) ) ;
#172247 = CARTESIAN_POINT ( 'NONE',  ( 3.235000160576475992, 2.016597019841442240, -0.002811030766311505089 ) ) ;
#172248 = CARTESIAN_POINT ( 'NONE',  ( -4.080641047588902559, 7.704572288921609058, -0.7216878364870257245 ) ) ;
#172249 = CARTESIAN_POINT ( 'NONE',  ( 4.326460416092276162, 7.101268681199365496, -1.082531754730548412 ) ) ;
#172250 = CARTESIAN_POINT ( 'NONE',  ( 8.452618703115982512, 11.94880668935564216, 1.199719254218450271 ) ) ;
#172251 = CARTESIAN_POINT ( 'NONE',  ( 0.5393321728033516615, -1.288848960320065462, -1.293324666950084190 ) ) ;
#172252 = CARTESIAN_POINT ( 'NONE',  ( -5.749539660647037032, 8.865490816466966351, 1.199719254218454489 ) ) ;
#172253 = CARTESIAN_POINT ( 'NONE',  ( -5.607095878192051686, 5.679663321520620478, 0.4065408311600144375 ) ) ;
#172254 = CARTESIAN_POINT ( 'NONE',  ( -9.420034542028389524, 2.999999999999999556, 6.906487091023606695 ) ) ;
#172255 = EDGE_LOOP ( 'NONE', ( #213905, #172893, #87881, #151078 ) ) ;
#172256 = CARTESIAN_POINT ( 'NONE',  ( 5.067286680778130936, 0.2040240636430467047, -2.050771057314598966 ) ) ;
#172257 = CARTESIAN_POINT ( 'NONE',  ( -7.227905289416814760, 7.605180057173966723, -0.7216878364870338292 ) ) ;
#172258 = CARTESIAN_POINT ( 'NONE',  ( -5.115504031057831469, 4.862509545855891346, 0.7998128361456341429 ) ) ;
#172259 = DIRECTION ( 'NONE',  ( 0.7366372490351829061, 1.218064704987765655E-12, -0.6762880771785629852 ) ) ;
#172260 = CARTESIAN_POINT ( 'NONE',  ( 6.024083573256426405, -2.004181050114914875, 0.2492093081243785258 ) ) ;
#172262 = EDGE_LOOP ( 'NONE', ( #65898, #26800, #132855, #208871 ) ) ;
#172261 = CARTESIAN_POINT ( 'NONE',  ( 5.901095752275416828, -0.3235219084677161128, -2.197517257070471075 ) ) ;
#172263 = AXIS2_PLACEMENT_3D ( 'NONE', #194924, #126818, #159225 ) ;
#172264 = CARTESIAN_POINT ( 'NONE',  ( -7.262327558775498737, 8.501745569106741840, 1.199719254218452047 ) ) ;
#172265 = CARTESIAN_POINT ( 'NONE',  ( 6.277588818327314080, 7.282607361925381717, 1.199719254218462483 ) ) ;
#172266 = CARTESIAN_POINT ( 'NONE',  ( 4.258703985924441326, -1.528322205979601334, 1.382770117495622397 ) ) ;
#172267 = CARTESIAN_POINT ( 'NONE',  ( 4.289685514112329123, 1.556909497225898109, -1.281360267751927129 ) ) ;
#172268 = EDGE_LOOP ( 'NONE', ( #68441, #8145, #42949, #99671 ) ) ;
#172269 = CARTESIAN_POINT ( 'NONE',  ( 1.907862554904935060, 3.236716050607304052, -0.4606469147255498608 ) ) ;
#172270 = CARTESIAN_POINT ( 'NONE',  ( 3.999819011231439347, 4.625209253646830554, 1.199719254218464037 ) ) ;
#172272 = EDGE_LOOP ( 'NONE', ( #126412, #185292, #124287, #111191 ) ) ;
#172271 = CARTESIAN_POINT ( 'NONE',  ( -7.605197822622922210, 7.837428646007010613, -0.7998128361456362523 ) ) ;
#172273 = CARTESIAN_POINT ( 'NONE',  ( 4.722521264130603136, 8.336029038342307018, -0.7037175076533495055 ) ) ;
#172274 = CARTESIAN_POINT ( 'NONE',  ( 3.761092154037175117, -2.013677596940225190, -0.1017350580494805479 ) ) ;
#172275 = CARTESIAN_POINT ( 'NONE',  ( 3.327899939431624876, 1.796474422365784029, 0.4023406486387756664 ) ) ;
#172276 = CARTESIAN_POINT ( 'NONE',  ( 4.415294977175556745, 5.022068982770194090, -0.9668805111738097979 ) ) ;
#172277 = CARTESIAN_POINT ( 'NONE',  ( 1.296046498377702472, 1.750325484892759409, 1.504033841696296836 ) ) ;
#172278 = CARTESIAN_POINT ( 'NONE',  ( 3.410758162289653672, 6.136912401716668519, -1.199719254218453823 ) ) ;
#172279 = CARTESIAN_POINT ( 'NONE',  ( 3.796290242343594468, -2.158924006851222988, -0.1102321833298808978 ) ) ;
#172280 = CARTESIAN_POINT ( 'NONE',  ( 7.151035956204054855, 10.43029348462504124, 1.199719254218460707 ) ) ;
#172281 = AXIS2_PLACEMENT_3D ( 'NONE', #166440, #199988, #144114 ) ;
#172282 = CARTESIAN_POINT ( 'NONE',  ( -4.415151579544611238, 8.302760609444034046, -0.7998128361456281477 ) ) ;
#172283 = CARTESIAN_POINT ( 'NONE',  ( 1.224999999999965006, 2.395833333333299286, -0.7072540797573078075 ) ) ;
#172284 = CARTESIAN_POINT ( 'NONE',  ( 1.955717210371358483, 1.865846021326333926, -0.1348392221205765851 ) ) ;
#172285 = CARTESIAN_POINT ( 'NONE',  ( 6.819227947992137828, -0.1355634432321853045, 1.940828160714276995 ) ) ;
#172287 = CARTESIAN_POINT ( 'NONE',  ( -6.129167961829681488, 9.308390501180058507, -1.199719254218452047 ) ) ;
#172286 = CARTESIAN_POINT ( 'NONE',  ( 1.364683531249988535, 4.155208333674753618, -0.7879004041258239610 ) ) ;
#172289 = CARTESIAN_POINT ( 'NONE',  ( 2.086817400036289794, -2.164668306305051804, -0.4287355390964405211 ) ) ;
#172288 = CARTESIAN_POINT ( 'NONE',  ( -5.117312914154178216, 8.057616602233474978, -1.199719254218452047 ) ) ;
#172290 = CARTESIAN_POINT ( 'NONE',  ( 6.589320575229280053, 7.629137130509070275, 2.496737603865983868 ) ) ;
#172291 = CARTESIAN_POINT ( 'NONE',  ( 4.143988507271280319, 7.986403691791820414, -0.7998128361456221525 ) ) ;
#172292 = CARTESIAN_POINT ( 'NONE',  ( -5.870844209917351009, 6.808071985447069707, -1.199719254218446718 ) ) ;
#172293 = CARTESIAN_POINT ( 'NONE',  ( 11.89942855770813956, 13.79999999999999893, 0.6999999999999992895 ) ) ;
#172294 = CARTESIAN_POINT ( 'NONE',  ( 6.209841870239331207, -1.956602576295646490, 0.2410399859902948028 ) ) ;
#172295 = CARTESIAN_POINT ( 'NONE',  ( 5.953837893508783452, 0.6757001976828447276, -2.206575258351393565 ) ) ;
#172296 = CARTESIAN_POINT ( 'NONE',  ( 6.707467475981614413, -1.495571456699902546, -1.107353707014941069 ) ) ;
#172297 = CARTESIAN_POINT ( 'NONE',  ( 3.028243468416950357, 1.099549687589720826, 1.744862417660711262 ) ) ;
#172298 = CARTESIAN_POINT ( 'NONE',  ( 6.480434237652124452, 8.583592582059388576, 1.443375672974076540 ) ) ;
#172299 = CARTESIAN_POINT ( 'NONE',  ( 7.614839552730775729, 8.913009562054615031, 1.199719254218452047 ) ) ;
#172300 = CARTESIAN_POINT ( 'NONE',  ( 6.087247782411444597, 10.04561347954795281, -0.7216878364870267237 ) ) ;
#172301 = CARTESIAN_POINT ( 'NONE',  ( 0.6823417656249899377, 3.155208333674754062, 1.181850606188765695 ) ) ;
#172302 = CARTESIAN_POINT ( 'NONE',  ( -8.762930527791271018, 14.55305236194923602, 8.184482591177637545 ) ) ;
#172303 = CARTESIAN_POINT ( 'NONE',  ( 3.809477975315569864, 7.388215371269402532, -0.7216878364870197293 ) ) ;
#172304 = CARTESIAN_POINT ( 'NONE',  ( 5.231008634329041840, -2.042658762482005841, -0.7362343983412369397 ) ) ;
#172306 = CARTESIAN_POINT ( 'NONE',  ( 4.915489835137424102, -0.9894786724786635013, -1.552603174752004600 ) ) ;
#172305 = CARTESIAN_POINT ( 'NONE',  ( -1.154700538379266339, -2.500000000000002220, 2.602085213965210642E-15 ) ) ;
#172307 = CARTESIAN_POINT ( 'NONE',  ( 11.87828357750012209, 12.29689747259587129, 1.708055325888913289 ) ) ;
#172308 = CARTESIAN_POINT ( 'NONE',  ( 0.3999999999999576672, 3.949999999999981526, 0.8338124244295311849 ) ) ;
#172309 = CARTESIAN_POINT ( 'NONE',  ( 0.1747926744264660381, 0.006858446013176254172, -1.855468577918440776 ) ) ;
#172310 = CARTESIAN_POINT ( 'NONE',  ( 0.5271418889439123401, 2.165442452462429834, 0.6551351998097357798 ) ) ;
#172311 = CARTESIAN_POINT ( 'NONE',  ( -5.443514322282436702, 6.457176790571845792, 1.314492736914568027 ) ) ;
#172312 = CARTESIAN_POINT ( 'NONE',  ( -4.101444922696786399, 3.685019076479660427, -2.420000000000000373 ) ) ;
#172313 = CARTESIAN_POINT ( 'NONE',  ( 6.590809034589254267, 6.776089313701147532, -0.2235409772415736240 ) ) ;
#172314 = CARTESIAN_POINT ( 'NONE',  ( -5.465345319640241506, 5.548860092434608760, 0.7216878364870257245 ) ) ;
#172315 = CARTESIAN_POINT ( 'NONE',  ( 0.1879522776407696050, 1.101030317643518330, 1.563299796079109072 ) ) ;
#172316 = CARTESIAN_POINT ( 'NONE',  ( 1.885279724593362793, 1.217781634009064806, 1.284517237999055039 ) ) ;
#172318 = CARTESIAN_POINT ( 'NONE',  ( 6.639320575229259447, 0.002292789353198348111, 1.996863816985874118 ) ) ;
#172317 = CIRCLE ( 'NONE', #78898, 0.7500000000000006661 ) ;
#172320 = CARTESIAN_POINT ( 'NONE',  ( 3.726117878570588626, 1.906711264527670258, 0.1841570787439601176 ) ) ;
#172319 = CARTESIAN_POINT ( 'NONE',  ( -7.980945979938748103, 12.46285407657057220, 0.000000000000000000 ) ) ;
#172321 = CARTESIAN_POINT ( 'NONE',  ( 4.383363735919856730, 4.008345868194933104, -0.7998128361456211532 ) ) ;
#172322 = CARTESIAN_POINT ( 'NONE',  ( 4.351979406267578732, -0.7558620137302939357, 1.818942442720396624 ) ) ;
#172323 = CARTESIAN_POINT ( 'NONE',  ( 6.469012451414649867, -1.558587985773008278, 1.284399031846704009 ) ) ;
#172324 = CARTESIAN_POINT ( 'NONE',  ( -2.839543107058306592, 5.400218493954923815, -1.199719254218446718 ) ) ;
#172325 = CARTESIAN_POINT ( 'NONE',  ( 3.010468980803046257, 1.356049738124785353, -1.288842618233053683 ) ) ;
#172327 = ORIENTED_EDGE ( 'NONE', *, *, #22937, .T. ) ;
#172326 = CARTESIAN_POINT ( 'NONE',  ( 6.006443931695136129, -0.6276177885309804916, -1.606848298988555301 ) ) ;
#172329 = CARTESIAN_POINT ( 'NONE',  ( 3.226477370372305753, 4.787309570232886280, 1.443375672974062551 ) ) ;
#172328 = CARTESIAN_POINT ( 'NONE',  ( 2.104404934925046877, -2.206339196854599116, 0.05594281105186085790 ) ) ;
#172330 = ADVANCED_FACE ( 'NONE', ( #47349 ), #180426, .T. ) ;
#172331 = CARTESIAN_POINT ( 'NONE',  ( -0.6823417656249969321, 3.280208333674754062, -1.181850606188749264 ) ) ;
#172332 = CARTESIAN_POINT ( 'NONE',  ( 6.180128940399614912, -1.088687182605744042, -1.631870318916525120 ) ) ;
#172333 = CARTESIAN_POINT ( 'NONE',  ( 8.076906825439115423, 10.44614393447756129, -1.599625672291262513 ) ) ;
#172334 = CARTESIAN_POINT ( 'NONE',  ( -7.362820735711497200, -5.796536394785085200, 7.362820735712229059 ) ) ;
#172335 = DIRECTION ( 'NONE',  ( 0.000000000000000000, 0.000000000000000000, 1.000000000000000000 ) ) ;
#172336 = CARTESIAN_POINT ( 'NONE',  ( -3.079673448598517549, 6.744702790006905424, 1.040834085586084257E-14 ) ) ;
#172337 = CARTESIAN_POINT ( 'NONE',  ( -1.499999999999960254, 7.564371094685077068, 10.87018506808107965 ) ) ;
#172339 = AXIS2_PLACEMENT_3D ( 'NONE', #71927, #105550, #23178 ) ;
#172338 = AXIS2_PLACEMENT_3D ( 'NONE', #136481, #56287, #202504 ) ;
#172340 = CARTESIAN_POINT ( 'NONE',  ( 1.697802635435996743, -1.498143435978617877, -1.429203828351800487 ) ) ;
#172341 = CARTESIAN_POINT ( 'NONE',  ( -1.201851678989727383E-14, 3.212500000000018119, 1.732050807568877637 ) ) ;
#172342 = CARTESIAN_POINT ( 'NONE',  ( 4.798696304233017074, 7.685897223992134819, -1.199719254218452047 ) ) ;
#172343 = CARTESIAN_POINT ( 'NONE',  ( 3.393283585170187688, 7.180857625999046867, 0.7998128361456271485 ) ) ;
#172344 = CARTESIAN_POINT ( 'NONE',  ( 0.3639331001695153001, 0.6315192924679478015, -1.918485960686921565 ) ) ;
#172345 = CARTESIAN_POINT ( 'NONE',  ( -0.6823417656249969321, 4.217708333674755394, -1.181850606188749264 ) ) ;
#172347 = CARTESIAN_POINT ( 'NONE',  ( 9.137832345930652522, 10.72352116074969075, -1.082531754730543083 ) ) ;
#172346 = CARTESIAN_POINT ( 'NONE',  ( 0.07479286986305369589, 0.2526433113205875935, -1.890777245541554574 ) ) ;
#172348 = CARTESIAN_POINT ( 'NONE',  ( 5.747422657745248742, -1.966344092054626680, -0.4444320411668146731 ) ) ;
#172349 = CARTESIAN_POINT ( 'NONE',  ( 5.612480213242726279, 1.848112342440700440, 0.5042863886801035589 ) ) ;
#172350 = CARTESIAN_POINT ( 'NONE',  ( 6.639320575229291421, 2.053731943030055795, 2.310327526069462234 ) ) ;
#172351 = CARTESIAN_POINT ( 'NONE',  ( 4.089532599075940134, -0.8378280566024614018, 2.025282237563410526 ) ) ;
#172352 = CARTESIAN_POINT ( 'NONE',  ( -1.201851678989727383E-14, 1.493750000682814383, 1.732050807568877637 ) ) ;
#172353 = CARTESIAN_POINT ( 'NONE',  ( 2.619282413590624525, 1.617716081779559278, 1.019604094833974628 ) ) ;
#172354 = CARTESIAN_POINT ( 'NONE',  ( -6.579784621333750749, 6.570836901177822931, 0.7998128361456341429 ) ) ;
#172356 = CARTESIAN_POINT ( 'NONE',  ( 3.836594282542902246, 7.419851063034623273, 0.7216878364870317197 ) ) ;
#172355 = B_SPLINE_CURVE_WITH_KNOTS ( 'NONE', 3,
 ( #176307, #78781, #156862, #143844, #28983, #95069 ),
 .UNSPECIFIED., .F., .F.,
 ( 4, 2, 4 ),
 ( 0.000000000000000000, 0.0003168911866439334617, 0.0006337823732878669234 ),
 .UNSPECIFIED. ) ;
#172358 = CARTESIAN_POINT ( 'NONE',  ( 0.3336115229473045618, 0.6298545048411038350, -1.915608025624820909 ) ) ;
#172357 = CARTESIAN_POINT ( 'NONE',  ( 6.925078400183548588, 0.0006614011395407459748, 1.855452278108092656 ) ) ;
#172359 = CARTESIAN_POINT ( 'NONE',  ( 1.364683531249997417, 11.29687500034139802, 2.602085213965210642E-15 ) ) ;
#172361 = CARTESIAN_POINT ( 'NONE',  ( -6.629010762438975135, 6.698543742459062145, -0.7998128361456362523 ) ) ;
#172360 = CARTESIAN_POINT ( 'NONE',  ( 5.671465802443460547, 1.304529079428708549, 1.760837017921567771 ) ) ;
#172363 = ORIENTED_EDGE ( 'NONE', *, *, #108076, .F. ) ;
#172362 = CARTESIAN_POINT ( 'NONE',  ( 3.065164753754692661, 0.2545988855646770244, -1.705743084088023664 ) ) ;
#172364 = DIRECTION ( 'NONE',  ( 0.000000000000000000, 0.000000000000000000, -1.000000000000000000 ) ) ;
#172365 = CARTESIAN_POINT ( 'NONE',  ( 6.500244582748090139, 9.671036882259738121, 1.199719254218460707 ) ) ;
#172366 = CARTESIAN_POINT ( 'NONE',  ( 4.497554271431305040, 6.270232621468402989, -1.599625672291256295 ) ) ;
#172367 = CARTESIAN_POINT ( 'NONE',  ( 2.482948226198858688, 5.072301959192136778, -2.499999999999995115 ) ) ;
#172368 = CARTESIAN_POINT ( 'NONE',  ( 0.2562055958934654210, -1.961350414083770977, -0.05204156388862594962 ) ) ;
#172369 = CARTESIAN_POINT ( 'NONE',  ( 11.43195036480942051, 9.944755037147421817, -3.649565797774410036 ) ) ;
#172370 = CARTESIAN_POINT ( 'NONE',  ( 6.277588818327314080, 7.282607361925381717, 1.199719254218462483 ) ) ;
#172371 = CARTESIAN_POINT ( 'NONE',  ( -1.500000000000015099, 10.72916666666666607, -0.8660254037844309360 ) ) ;
#172372 = ORIENTED_EDGE ( 'NONE', *, *, #69227, .F. ) ;
#172373 = AXIS2_PLACEMENT_3D ( 'NONE', #131920, #135105, #117833 ) ;
#172374 = DIRECTION ( 'NONE',  ( 0.000000000000000000, 0.000000000000000000, 1.000000000000000000 ) ) ;
#172375 = ORIENTED_EDGE ( 'NONE', *, *, #61547, .F. ) ;
#172376 = CARTESIAN_POINT ( 'NONE',  ( 3.123486050149349769, -0.3508677868355335461, 1.776971544703136452 ) ) ;
#172377 = VERTEX_POINT ( 'NONE', #76616 ) ;
#172378 = CARTESIAN_POINT ( 'NONE',  ( 9.083072846151447166, 12.68433652289702884, 1.199719254218450271 ) ) ;
#172379 = CARTESIAN_POINT ( 'NONE',  ( 3.576318658954677598, 7.394398545414291313, 0.7998128361456281477 ) ) ;
#172380 = CARTESIAN_POINT ( 'NONE',  ( 3.264119686811095988, 1.811656971725349896, -0.002766503545040265976 ) ) ;
#172381 = CARTESIAN_POINT ( 'NONE',  ( -1.499999999999997780, 6.280000000000042881, -2.579999999999995630 ) ) ;
#172382 = CARTESIAN_POINT ( 'NONE',  ( -2.788906526875773208E-15, 9.218750000682799595, -1.499999999999998446 ) ) ;
#172383 = CARTESIAN_POINT ( 'NONE',  ( 5.134314571617769829, 6.480444997182255307, 1.201143065674977528 ) ) ;
#172384 = COLOUR_RGB ( '', 0.66274510, 0.83137255, 0.94901961) ;
#172386 = CARTESIAN_POINT ( 'NONE',  ( -0.6823417656250003738, 14.65104166700806410, 1.181850606188754593 ) ) ;
#172385 = CARTESIAN_POINT ( 'NONE',  ( 4.967181581899757781, 1.619035083845013157, 0.9176225028624994673 ) ) ;
#172387 = CARTESIAN_POINT ( 'NONE',  ( 2.161615495643732565, 1.180369796089770995, 1.508615382416353290 ) ) ;
#172388 = CARTESIAN_POINT ( 'NONE',  ( 1.500715674837904468, 1.494693011815557471, -1.047886037138339166 ) ) ;
#172389 = CARTESIAN_POINT ( 'NONE',  ( 4.694814482132247946, 8.250513237351190909, 0.6064353157786159798 ) ) ;
#172390 = CARTESIAN_POINT ( 'NONE',  ( -11.69243366784185945, 8.407932920124673970, 1.097391832464843286 ) ) ;
#172391 = CARTESIAN_POINT ( 'NONE',  ( 5.701630405109389343, 7.302376724489803905, 1.216486997566777584 ) ) ;
#172392 = CARTESIAN_POINT ( 'NONE',  ( -11.44779963594988814, 10.19999999999998153, 3.600000000000001421 ) ) ;
#172393 = DIRECTION ( 'NONE',  ( 0.000000000000000000, 1.000000000000000000, 0.000000000000000000 ) ) ;
#172394 = DIRECTION ( 'NONE',  ( 0.000000000000000000, 0.000000000000000000, 1.000000000000000000 ) ) ;
#172395 = CARTESIAN_POINT ( 'NONE',  ( 6.724481002698112775, 8.868313807946373473, -1.443375672974057666 ) ) ;
#172396 = CARTESIAN_POINT ( 'NONE',  ( -5.264643720808155791, 5.036505850564608089, 0.000000000000000000 ) ) ;
#172397 = FACE_OUTER_BOUND ( 'NONE', #66269, .T. ) ;
#172398 = CARTESIAN_POINT ( 'NONE',  ( 0.9551577523512165824, 0.4061005957273036704, -2.050632492140195939 ) ) ;
#172399 = CARTESIAN_POINT ( 'NONE',  ( 6.299827777084090918, -0.6482784301091691903, 1.814149458844191320 ) ) ;
#172400 = CARTESIAN_POINT ( 'NONE',  ( -5.585069213825653023, 8.603332285183535433, -1.199719254218440723 ) ) ;
#172401 = CARTESIAN_POINT ( 'NONE',  ( 1.905030480050071251, 1.515927946353814892, 1.016894063925778635 ) ) ;
#172402 = CARTESIAN_POINT ( 'NONE',  ( 3.317197348578094562, 1.995112415077514356, 0.9436014139095407760 ) ) ;
#172403 = CARTESIAN_POINT ( 'NONE',  ( 0.5098338327763075606, -0.6861045072398126443, 1.785269576063217567 ) ) ;
#172404 = CARTESIAN_POINT ( 'NONE',  ( 1.961320326556061922, 1.635743983707088622, 1.096704005335534138 ) ) ;
#172405 = CARTESIAN_POINT ( 'NONE',  ( 3.438947998021203656, -1.472602994093423545, -1.266235326041851961 ) ) ;
#172406 = VERTEX_POINT ( 'NONE', #113463 ) ;
#172407 = CARTESIAN_POINT ( 'NONE',  ( 1.469576158976824144E-15, 4.518459255872630642, 12.00000000000000178 ) ) ;
#172409 = CARTESIAN_POINT ( 'NONE',  ( 6.754761327113334879, -0.4959639348531270642, -1.793591138363290316 ) ) ;
#172408 = CARTESIAN_POINT ( 'NONE',  ( -4.573896719763875574, 6.429575154514868274, -1.599625672291271394 ) ) ;
#172410 = CARTESIAN_POINT ( 'NONE',  ( 6.086684617892325733, 6.065829907154645539, -0.7998128361456481317 ) ) ;
#172411 = CARTESIAN_POINT ( 'NONE',  ( 0.007565906569757733027, -9.598697202504085979, -9.591786056756832934 ) ) ;
#172412 = DIRECTION ( 'NONE',  ( 0.000000000000000000, 0.000000000000000000, -1.000000000000000000 ) ) ;
#172413 = CARTESIAN_POINT ( 'NONE',  ( -7.286581212701773502, 7.465709267765667789, 0.7998128361456341429 ) ) ;
#172414 = CARTESIAN_POINT ( 'NONE',  ( 2.402122600552298870, -0.8417629408748151798, -2.023652355447076001 ) ) ;
#172415 = EDGE_LOOP ( 'NONE', ( #154933, #118875, #75218, #83523 ) ) ;
#172416 = MECHANICAL_DESIGN_GEOMETRIC_PRESENTATION_REPRESENTATION (  '', ( #168987 ), #127506 ) ;
#172417 = CARTESIAN_POINT ( 'NONE',  ( 6.496291879603339758, 7.608037276739255006, 1.199719254218452935 ) ) ;
#172418 = CARTESIAN_POINT ( 'NONE',  ( -15.75000000000000000, 13.79999999999999893, -1.800000000000001155 ) ) ;
#172419 = CARTESIAN_POINT ( 'NONE',  ( 3.387140609607977026, 1.650079954178599539, -0.7815607168924765258 ) ) ;
#172420 = CARTESIAN_POINT ( 'NONE',  ( 1.419999999999820739, 7.388542872122566330, -4.154462424328212222 ) ) ;
#172421 = CARTESIAN_POINT ( 'NONE',  ( -3.789667630219657912, 4.380032642466370696, 1.199719254218462483 ) ) ;
#172422 = CARTESIAN_POINT ( 'NONE',  ( -4.648357846327917819, 8.420182996469929293, -0.5132882116619559287 ) ) ;
#172423 = CARTESIAN_POINT ( 'NONE',  ( -1.734723475976807094E-15, 2.999999999999988898, -6.938893903907228378E-15 ) ) ;
#172424 = CARTESIAN_POINT ( 'NONE',  ( 4.012460596634464416, 1.323225596166040186, -1.322536486416127977 ) ) ;
#172425 = CARTESIAN_POINT ( 'NONE',  ( 6.889514614038635187, 11.18951748302043114, -0.7998128361456291469 ) ) ;
#172426 = CARTESIAN_POINT ( 'NONE',  ( 2.385270436692279006, 1.761333987333755013, -0.7808530812865380755 ) ) ;
#172427 = CARTESIAN_POINT ( 'NONE',  ( -4.638229190868998764, 5.411267389347211854, -2.420000000000000373 ) ) ;
#172428 = COLOUR_RGB ( '', 0.72549020, 0.75294118, 0.79215686) ;
#172429 = CARTESIAN_POINT ( 'NONE',  ( -1.500000000000015099, 14.47916666666666785, -0.8660254037844309360 ) ) ;
#172430 = CARTESIAN_POINT ( 'NONE',  ( -6.684333426737305572, 7.757142738403693727, -1.199719254218446718 ) ) ;
#172431 = CARTESIAN_POINT ( 'NONE',  ( 5.172599298813543633, 5.993452922492633839, -1.199719254218452047 ) ) ;
#172432 = CARTESIAN_POINT ( 'NONE',  ( -5.600926855776894975, 6.667407765562058053, -1.082531754730549967 ) ) ;
#172433 = CARTESIAN_POINT ( 'NONE',  ( 6.456269881894531437, -1.301449686459619226, 1.670992065744638433 ) ) ;
#172434 = CARTESIAN_POINT ( 'NONE',  ( 10.24048609702354717, 10.84165528948263457, -0.7998128361456281477 ) ) ;
#172435 = CARTESIAN_POINT ( 'NONE',  ( -1.408744241983817425, 4.236591513440624013, -0.5205678189275618761 ) ) ;
#172437 = ADVANCED_FACE ( 'NONE', ( #11611 ), #170863, .F. ) ;
#172436 = CARTESIAN_POINT ( 'NONE',  ( 5.348515126027270306, -2.053966340784090239, -0.2589089449258550890 ) ) ;
#172439 = CARTESIAN_POINT ( 'NONE',  ( -0.6823417656250212460, 3.113541667008084879, 1.181850606188767472 ) ) ;
#172438 = CARTESIAN_POINT ( 'NONE',  ( 0.5558949066124979632, -1.334021266253348381, 1.269314063962425854 ) ) ;
#172440 = CARTESIAN_POINT ( 'NONE',  ( 4.746898448635796797, 2.273877242543398403, -0.3363112362181965853 ) ) ;
#172441 = CARTESIAN_POINT ( 'NONE',  ( 7.185458225562760148, 8.445751353653788485, -1.082531754730543083 ) ) ;
#172443 = CARTESIAN_POINT ( 'NONE',  ( 0.7499999999999902300, 4.597916667349482012, -1.299038105676658228 ) ) ;
#172442 = CARTESIAN_POINT ( 'NONE',  ( 5.736508392357904107, 5.865217010605237924, 0.000000000000000000 ) ) ;
#172444 = CARTESIAN_POINT ( 'NONE',  ( 0.5160991691709617690, -1.231265438625952724, -1.933346247471772861 ) ) ;
#172445 = CARTESIAN_POINT ( 'NONE',  ( 7.004500933659043582, -6.920331743269733771, -7.004500933659070228 ) ) ;
#172446 = CARTESIAN_POINT ( 'NONE',  ( -6.831329296439251131, 9.063246493969506545, -1.599625672291271394 ) ) ;
#172447 = CARTESIAN_POINT ( 'NONE',  ( 5.068278781427039803, -1.829183178514147690, -0.6524800764661740082 ) ) ;
#172448 = VERTEX_POINT ( 'NONE', #114526 ) ;
#172449 = CARTESIAN_POINT ( 'NONE',  ( 8.717529583462646059, 11.19353715217169309, 1.443375672974076540 ) ) ;
#172450 = ORIENTED_EDGE ( 'NONE', *, *, #147441, .F. ) ;
#172451 = CARTESIAN_POINT ( 'NONE',  ( 6.310809538426106258, -0.5167911955388967415, -1.841158844219364044 ) ) ;
#172452 = CARTESIAN_POINT ( 'NONE',  ( 0.5567383370381777663, -1.454440682700371079, -0.9269339563611042054 ) ) ;
#172453 = CARTESIAN_POINT ( 'NONE',  ( 5.805875103277515770, -1.124240986939632592, -1.673857227857282082 ) ) ;
#172454 = CARTESIAN_POINT ( 'NONE',  ( -7.831806290188425557, 12.28885777186185990, -0.7998128361456281477 ) ) ;
#172455 = CARTESIAN_POINT ( 'NONE',  ( -3.285556943750000070, -1.946874999522042682, 0.000000000000000000 ) ) ;
#172457 = CARTESIAN_POINT ( 'NONE',  ( 0.7425837709835466649, -1.521049679623546425, 0.9045992453171716186 ) ) ;
#172456 = CARTESIAN_POINT ( 'NONE',  ( 2.572312895708084302, -2.000810251872984225, -0.6062274732134291799 ) ) ;
#172458 = CARTESIAN_POINT ( 'NONE',  ( 11.44789321844504215, 9.799999999999982947, 3.303298730975393838 ) ) ;
#172459 = EDGE_CURVE ( 'NONE', #18401, #179696, #192994, .T. ) ;
#172461 = CARTESIAN_POINT ( 'NONE',  ( 4.435649837374885607, 0.9824219174630977047, -2.071190651000577976 ) ) ;
#172460 = CARTESIAN_POINT ( 'NONE',  ( 3.573456005653643519, 6.326726552307992080, -1.199719254218453823 ) ) ;
#172462 = CARTESIAN_POINT ( 'NONE',  ( 2.202700171921621042, -0.3823900931277899318, 1.697618373880743325 ) ) ;
#172463 = CARTESIAN_POINT ( 'NONE',  ( 5.217190183160311356, 4.981143389975473568, -0.7998128361456211532 ) ) ;
#172464 = CARTESIAN_POINT ( 'NONE',  ( 2.795306286867365486, -0.1602278063087131110, -2.114629986603839829 ) ) ;
#172465 = CARTESIAN_POINT ( 'NONE',  ( 4.376249722160992839, 8.327651452488305850, 0.000000000000000000 ) ) ;
#172466 = CARTESIAN_POINT ( 'NONE',  ( 2.512703819571511232, 1.733401479428131609, 0.04661458952265155886 ) ) ;
#172467 = CARTESIAN_POINT ( 'NONE',  ( -0.6801582343750403048, 2.463541667008038782, 1.178068619123829430 ) ) ;
#172468 = CARTESIAN_POINT ( 'NONE',  ( 1.222862307070234911, -1.680409034227359211, -0.8001750615637763797 ) ) ;
#172469 = CARTESIAN_POINT ( 'NONE',  ( 1.908858375081338377, 0.6798548000985217277, 2.062075944584631504 ) ) ;
#172470 = CARTESIAN_POINT ( 'NONE',  ( 6.484877546038077867, 6.460111979999551224, 1.040834085586084257E-14 ) ) ;
#172471 = CARTESIAN_POINT ( 'NONE',  ( 3.538296236868877731, 0.7303062672313584969, 1.879804216660937666 ) ) ;
#172472 = CARTESIAN_POINT ( 'NONE',  ( 2.906250000000002220, 1.895863743164021509, -0.7852924748301391977 ) ) ;
#172473 = AXIS2_PLACEMENT_3D ( 'NONE', #86630, #71420, #100743 ) ;
#172474 = CARTESIAN_POINT ( 'NONE',  ( -1.500000000000013101, 2.452083334016154748, 0.8660254037844403729 ) ) ;
#172475 = CARTESIAN_POINT ( 'NONE',  ( 0.4461525089796612997, 1.920980128883168714, 0.1452595308072956448 ) ) ;
#172476 = CARTESIAN_POINT ( 'NONE',  ( -8.012344526598182026E-15, 13.79687500034139624, -1.575800808251669460 ) ) ;
#172477 = CARTESIAN_POINT ( 'NONE',  ( 4.377308812845062569, -1.984989629755340435, -0.9973083610524589027 ) ) ;
#172478 = ORIENTED_EDGE ( 'NONE', *, *, #44939, .F. ) ;
#172479 = LINE ( 'NONE', #209206, #74016 ) ;
#172480 = CARTESIAN_POINT ( 'NONE',  ( -0.7500000000000215383, 0.1916666666666871910, 1.299038105676659116 ) ) ;
#172481 = CARTESIAN_POINT ( 'NONE',  ( 5.926885707468349196, 10.06645042535509660, 1.040834085586084257E-14 ) ) ;
#172482 = CARTESIAN_POINT ( 'NONE',  ( -0.6823417656250003738, -0.03229166632524871350, -1.181850606188749264 ) ) ;
#172483 = CARTESIAN_POINT ( 'NONE',  ( 6.345936316318473658, -1.449877878406122145, -1.683046035897132420 ) ) ;
#172484 = CARTESIAN_POINT ( 'NONE',  ( 5.230891786122516152, -1.846674803186045821, -0.6626716404555529349 ) ) ;
#172485 = CARTESIAN_POINT ( 'NONE',  ( 8.080296364064698977, 12.37083682481011060, -0.7216878364870328300 ) ) ;
#172486 =( NAMED_UNIT ( * ) PLANE_ANGLE_UNIT ( ) SI_UNIT ( $, .RADIAN. ) );
#172487 = CARTESIAN_POINT ( 'NONE',  ( 5.325545376182048152, -2.150690057981026193, 0.7024452394915041697 ) ) ;
#172488 = AXIS2_PLACEMENT_3D ( 'NONE', #20204, #119928, #151302 ) ;
#172489 = CARTESIAN_POINT ( 'NONE',  ( -5.966997003790232235, 7.094489604910957148, -1.082531754730549967 ) ) ;
#172490 = CARTESIAN_POINT ( 'NONE',  ( 3.139185485588998237, -0.1492200975972737820, -2.057319831125117737 ) ) ;
#172491 = CARTESIAN_POINT ( 'NONE',  ( -5.799137018343247796, 7.788745826199009237, -1.599625672291256295 ) ) ;
#172492 = ADVANCED_FACE ( 'NONE', ( #51596 ), #96645, .T. ) ;
#172493 = CARTESIAN_POINT ( 'NONE',  ( 0.7499999999999885647, 2.847916667349487341, -1.299038105676658228 ) ) ;
#172494 = CARTESIAN_POINT ( 'NONE',  ( 1.364683531249992088, 5.446875000341417916, 1.214306433183764966E-14 ) ) ;
#172495 = CARTESIAN_POINT ( 'NONE',  ( 4.903500725120335524, -0.5004011548357701900, 1.802273645872286334 ) ) ;
#172496 = CARTESIAN_POINT ( 'NONE',  ( 3.779676010894826188, 1.462474260537292681, -0.9315460551484288088 ) ) ;
#172497 = CARTESIAN_POINT ( 'NONE',  ( 2.893823712666950598, -0.5078125688623453815, -1.664683006417116751 ) ) ;
#172498 = CARTESIAN_POINT ( 'NONE',  ( 0.9257723888009254942, -1.459437212925698502, -1.767766894381626486 ) ) ;
#172499 = CARTESIAN_POINT ( 'NONE',  ( 1.554063478550568256, 0.6399170599369340406, -2.111937735441645980 ) ) ;
#172500 = CARTESIAN_POINT ( 'NONE',  ( 5.091392180243133225, -0.7513228403347729234, 1.951278057808901512 ) ) ;
#172501 = CARTESIAN_POINT ( 'NONE',  ( 5.525317926099265087, -1.233401178653690033, -1.499961942869533438 ) ) ;
#172503 = ORIENTED_EDGE ( 'NONE', *, *, #76698, .F. ) ;
#172502 = CARTESIAN_POINT ( 'NONE',  ( 8.384960142880849787, 15.11786449873486582, 8.585919489561741003 ) ) ;
#172504 = SURFACE_STYLE_USAGE ( .BOTH. , #56612 ) ;
#172505 = CARTESIAN_POINT ( 'NONE',  ( 0.5279704824466545654, -1.728000714500482982, 1.038995864524896673 ) ) ;
#172506 = CARTESIAN_POINT ( 'NONE',  ( 0.8266187642571948269, -0.9586779626098644869, -1.891633453305548773 ) ) ;
#172507 = DIRECTION ( 'NONE',  ( 0.000000000000000000, -1.000000000000000000, -9.023263958591317418E-17 ) ) ;
#172508 = DIRECTION ( 'NONE',  ( 0.000000000000000000, 0.000000000000000000, -1.000000000000000000 ) ) ;
#172509 = CARTESIAN_POINT ( 'NONE',  ( -7.655550293210764856, 12.08322577538792331, 0.000000000000000000 ) ) ;
#172510 = CARTESIAN_POINT ( 'NONE',  ( 6.012151052656117933, 9.101594430485762999, 1.199719254218460707 ) ) ;
#172511 = CARTESIAN_POINT ( 'NONE',  ( 1.620863580070950549, -1.399999999999998579, -1.903365770102947163 ) ) ;
#172512 = CARTESIAN_POINT ( 'NONE',  ( 4.160648861918358143, -1.351394993475165673, 1.227733137840483879 ) ) ;
#172513 = ORIENTED_EDGE ( 'NONE', *, *, #195893, .F. ) ;
#172514 = CARTESIAN_POINT ( 'NONE',  ( -5.745623237141265882, 9.925253886631958622, 0.7998128361456291469 ) ) ;
#172515 = DIRECTION ( 'NONE',  ( -1.000000000000000000, 0.000000000000000000, 0.000000000000000000 ) ) ;
#172516 = CARTESIAN_POINT ( 'NONE',  ( 0.000000000000000000, -3.084374999522042859, -3.793834371823813001 ) ) ;
#172517 = CARTESIAN_POINT ( 'NONE',  ( -5.506582945444718824, 9.576097202994168001, 0.7998128361456481317 ) ) ;
#172518 = CARTESIAN_POINT ( 'NONE',  ( 1.740496097130298958, 1.159487406938706888, -1.653631796535762755 ) ) ;
#172519 = CARTESIAN_POINT ( 'NONE',  ( 5.473716482686670659, 2.128106746890707335, -0.5837492795209007213 ) ) ;
#172520 = CARTESIAN_POINT ( 'NONE',  ( -3.298376509874564988, 7.070132704820777825, 0.000000000000000000 ) ) ;
#172521 = CARTESIAN_POINT ( 'NONE',  ( 2.570971337753673147, 1.659905555536644872, 0.8415416509589612737 ) ) ;
#172522 = CARTESIAN_POINT ( 'NONE',  ( 2.693266070609028784, 6.293894182352508970, 0.000000000000000000 ) ) ;
#172523 = CIRCLE ( 'NONE', #193376, 11.09999999999999964 ) ;
#172524 = CARTESIAN_POINT ( 'NONE',  ( 6.373741612200174878, 6.608655767087928012, 0.7216878364870328300 ) ) ;
#172525 = ORIENTED_EDGE ( 'NONE', *, *, #42099, .F. ) ;
#172526 = CARTESIAN_POINT ( 'NONE',  ( -4.229253852459088137, 7.021547696922494808, 1.199719254218464037 ) ) ;
#172527 = CARTESIAN_POINT ( 'NONE',  ( -8.296699936558862731, 11.76690146170562201, 1.199719254218453823 ) ) ;
#172528 = CARTESIAN_POINT ( 'NONE',  ( 5.320859459983126705, 1.688362619374352613, 0.6951667914897319278 ) ) ;
#172530 = CARTESIAN_POINT ( 'NONE',  ( -3.980123661693549142, 7.843117270353603843, 0.1539385989055529202 ) ) ;
#172529 = CARTESIAN_POINT ( 'NONE',  ( -5.340986169140711226, 5.195848383611072485, 0.000000000000000000 ) ) ;
#172531 = CARTESIAN_POINT ( 'NONE',  ( 5.713240515264599750, 7.403118591225121392, -1.316831503761767719 ) ) ;
#172532 = CARTESIAN_POINT ( 'NONE',  ( 0.1394461523056798324, 0.009327122704651937685, -1.719853553173174232 ) ) ;
#172533 = CARTESIAN_POINT ( 'NONE',  ( -0.02988540731103071432, 0.005807295984020746475, -1.726291166677936362 ) ) ;
#172534 = CARTESIAN_POINT ( 'NONE',  ( 5.795647523915807398, 1.743732541305573758, 1.511695197786174782 ) ) ;
#172535 = CARTESIAN_POINT ( 'NONE',  ( 6.215487077222150880, 6.216099443039444949, 0.000000000000000000 ) ) ;
#172536 = CARTESIAN_POINT ( 'NONE',  ( 0.5443023342626990280, 2.055102546481206272, 0.1540600304409632249 ) ) ;
#172537 = CARTESIAN_POINT ( 'NONE',  ( 6.667912619822566000, 6.673652899414787676, 1.040834085586084257E-14 ) ) ;
#172538 = CARTESIAN_POINT ( 'NONE',  ( 6.116662973727256869, 0.6756443950356945116, -2.196842021360578823 ) ) ;
#172539 = CARTESIAN_POINT ( 'NONE',  ( 6.518203450479836292, 5.167241622962440495, 2.437504649502901799 ) ) ;
#172540 = CARTESIAN_POINT ( 'NONE',  ( -5.586841817283045408, 8.675676665875643678, 1.199719254218454489 ) ) ;
#172541 = CARTESIAN_POINT ( 'NONE',  ( 5.436355746168001879, 1.843147576875401983, 0.3187000444574567548 ) ) ;
#172543 = CARTESIAN_POINT ( 'NONE',  ( -5.659602779061863487, 5.567567761852417085, 0.7998128361456281477 ) ) ;
#172542 = CARTESIAN_POINT ( 'NONE',  ( 3.076317393561965208, 0.8638369986560844316, 1.706277067364105893 ) ) ;
#172544 = CARTESIAN_POINT ( 'NONE',  ( 4.951907052881864502, 0.6945806438464275923, -2.094803410698709900 ) ) ;
#172545 = CARTESIAN_POINT ( 'NONE',  ( 4.399685268140280492, -2.075804279169701339, 0.4165508703993703876 ) ) ;
#172546 = CARTESIAN_POINT ( 'NONE',  ( -0.6125000000000314637, 0.8541666673494846540, 1.060881119635901593 ) ) ;
#172547 = CARTESIAN_POINT ( 'NONE',  ( 6.983263157960371004, 2.969675876345272858, 2.399270433241917466 ) ) ;
#172548 = CARTESIAN_POINT ( 'NONE',  ( 5.438229012412886476, 7.437962829272074750, -1.443375672974078761 ) ) ;
#172549 = CARTESIAN_POINT ( 'NONE',  ( -6.102578539482539810, 6.292298848917299736, 0.000000000000000000 ) ) ;
#172550 = CARTESIAN_POINT ( 'NONE',  ( 5.760427271636393343, 2.118038551301495875, 0.1041057254967461404 ) ) ;
#172551 = CARTESIAN_POINT ( 'NONE',  ( 2.608792587697115639, -0.8827421749361822334, -2.132256252471361524 ) ) ;
#172552 = CARTESIAN_POINT ( 'NONE',  ( 4.000408739481801312, 1.952204270133122810, 0.1946113827649766925 ) ) ;
#172553 = CARTESIAN_POINT ( 'NONE',  ( -6.134138155540168391, 6.121192367743780949, 0.000000000000000000 ) ) ;
#172554 = CARTESIAN_POINT ( 'NONE',  ( 6.561391914609854936, 1.711577788671992062, 1.150682440272139617 ) ) ;
#172555 = CARTESIAN_POINT ( 'NONE',  ( 3.199361063144961825, 6.676412307070352270, -0.7216878364870267237 ) ) ;
#172556 = CARTESIAN_POINT ( 'NONE',  ( 4.740510986633625024, 5.559626234941203116, -1.199719254218450271 ) ) ;
#172557 = EDGE_LOOP ( 'NONE', ( #61880, #82011, #74869, #12262 ) ) ;
#172558 = CARTESIAN_POINT ( 'NONE',  ( 5.419157771004846857, -1.820987890746316173, 0.8666037247077316152 ) ) ;
#172559 = CARTESIAN_POINT ( 'NONE',  ( -9.657485491635913633, 10.16148791653038330, 1.040834085586084257E-14 ) ) ;
#172560 =( BOUNDED_SURFACE ( )  B_SPLINE_SURFACE ( 3, 3, ( 
 ( #180696, #102659, #16040, #167652, #131996, #19253, #33377, #118968, #85333, #2990 ),
 ( #115756, #198005, #99458, #86406, #39794, #202257, #61100, #189238, #38726, #90695 ),
 ( #173007, #143458, #22442, #87479, #88553, #72262, #193230, #155679, #105901, #187092 ),
 ( #136234, #23521, #209456, #176988, #171925, #156757, #106982, #44877, #123276, #24588 ),
 ( #5114, #40877, #110982, #11268, #77346, #120043, #204387, #127259, #71191, #154614 ),
 ( #28606, #121128, #4053, #94695, #6193, #70123, #104807, #153545, #89627, #170852 ),
 ( #7261, #53908, #186017, #73337, #57107, #188161, #138370, #137308, #56043, #103731 ) ),
 .UNSPECIFIED., .T., .F., .F. ) 
 B_SPLINE_SURFACE_WITH_KNOTS ( ( 4, 3, 4 ),
 ( 4, 1, 1, 1, 1, 1, 1, 4 ),
 ( 0.000000000000000000, 0.5000000000000000000, 1.000000000000000000 ),
 ( 0.000000000000000000, 0.09489293188423997272, 0.1878783894049059211, 0.2584743716234961797, 0.3617987437640678983, 0.5212292184658617877, 0.7337638816394396191, 1.000000000000000000 ),
 .UNSPECIFIED. ) 
 GEOMETRIC_REPRESENTATION_ITEM ( )  RATIONAL_B_SPLINE_SURFACE ( (
 ( 1.000000000000000222, 1.000000000000000222, 1.000000000000000000, 1.000000000000000000, 1.000000000000000000, 1.000000000000000000, 1.000000000000000000, 0.9999999999999997780, 1.000000000000000000, 1.000000000000000000),
 ( 0.3333333333333334259, 0.3333333333333333703, 0.3333333333333334259, 0.3333333333333334259, 0.3333333333333333703, 0.3333333333333333703, 0.3333333333333333703, 0.3333333333333332038, 0.3333333333333333703, 0.3333333333333333703),
 ( 0.3333333333333334259, 0.3333333333333333703, 0.3333333333333334259, 0.3333333333333334259, 0.3333333333333333703, 0.3333333333333333703, 0.3333333333333333703, 0.3333333333333332038, 0.3333333333333333703, 0.3333333333333333703),
 ( 1.000000000000000222, 1.000000000000000222, 1.000000000000000000, 1.000000000000000000, 1.000000000000000000, 1.000000000000000000, 1.000000000000000000, 0.9999999999999997780, 1.000000000000000000, 1.000000000000000000),
 ( 0.3333333333333334259, 0.3333333333333333703, 0.3333333333333334259, 0.3333333333333334259, 0.3333333333333333703, 0.3333333333333333703, 0.3333333333333333703, 0.3333333333333332038, 0.3333333333333333703, 0.3333333333333333703),
 ( 0.3333333333333334259, 0.3333333333333333703, 0.3333333333333334259, 0.3333333333333334259, 0.3333333333333333703, 0.3333333333333333703, 0.3333333333333333703, 0.3333333333333332038, 0.3333333333333333703, 0.3333333333333333703),
 ( 1.000000000000000222, 1.000000000000000222, 1.000000000000000000, 1.000000000000000000, 1.000000000000000000, 1.000000000000000000, 1.000000000000000000, 0.9999999999999997780, 1.000000000000000000, 1.000000000000000000) ) ) 
 REPRESENTATION_ITEM ( '' )  SURFACE ( )  );
#172561 = DIRECTION ( 'NONE',  ( 0.000000000000000000, 1.000000000000000000, 0.000000000000000000 ) ) ;
#172562 = CARTESIAN_POINT ( 'NONE',  ( 2.571331741745811250, 1.937545498039330960, 0.9797267027546376905 ) ) ;
#172563 = CARTESIAN_POINT ( 'NONE',  ( 6.539320575229290000, 0.004092658091040673150, 2.003502637948690879 ) ) ;
#172564 = CARTESIAN_POINT ( 'NONE',  ( 0.7499999999999885647, 2.097916667349486453, -1.299038105676652899 ) ) ;
#172565 = CARTESIAN_POINT ( 'NONE',  ( -5.601522606845680485, 14.48156018084685925, -10.62176276536360398 ) ) ;
#172566 = DIRECTION ( 'NONE',  ( 0.000000000000000000, 0.000000000000000000, -1.000000000000000000 ) ) ;
#172567 = CARTESIAN_POINT ( 'NONE',  ( 4.783863686166085039, 8.265937597628173705, 0.8363946479656783062 ) ) ;
#172568 = VECTOR ( 'NONE', #17969, 1000.000000000000000 ) ;
#172569 = CARTESIAN_POINT ( 'NONE',  ( 1.317730169365991522, -2.011166735366700209, 0.4487503453191737934 ) ) ;
#172571 = CARTESIAN_POINT ( 'NONE',  ( 6.727182134110205602, 7.053355583909074689, 2.409100679957976165 ) ) ;
#172570 = CARTESIAN_POINT ( 'NONE',  ( -9.317477881089553549, 11.89347683273641820, 1.599625672291281386 ) ) ;
#172572 = CARTESIAN_POINT ( 'NONE',  ( -0.6823417656250246877, 0.5510416670080897639, 1.181850606188755259 ) ) ;
#172573 = DIRECTION ( 'NONE',  ( 0.000000000000000000, -1.000000000000000000, -1.496258514059622730E-16 ) ) ;
#172574 =( BOUNDED_SURFACE ( )  B_SPLINE_SURFACE ( 1, 2, ( 
 ( #88799, #56288, #21608, #139695, #205717, #154858, #72518, #40044, #155926, #190534, #173256, #123516, #106153, #9657, #103979, #172179, #73593, #189480, #41123, #87716, #170022, #157002, #74670, #54155, #140773, #42190, #174325, #120294, #92011, #158069, #153788, #5358, #71440, #55221, #121367, #94143, #159115, #160182, #143980, #47521, #12840, #76785, #29117, #95203, #141846, #26967, #179639, #142907, #78914, #127782, #110436, #125634, #161253, #178574, #191595, #208907, #46442, #44314, #113634, #207851, #126699, #61612, #212103, #60540, #11783, #63740, #75733, #211039, #31259, #146092, #77856, #30181, #192660, #145036, #62665, #128824, #194806, #112561, #96272, #43256, #162322, #13906, #176438, #195883, #79988, #129898, #28050, #59477, #109375, #97333, #163391, #175382, #93073, #45383, #209971, #193737, #10716, #111499, #177505, #1913, #99451, #34435, #2984, #135171, #98382, #134116, #133045, #101577, #64802, #49624, #114695, #166583, #83178, #199046, #100508, #214211, #130948, #65840, #167645, #164445, #201186, #181739, #149261, #180689, #18172, #84259, #33370, #165508, #17100, #116817, #85326, #51778, #150344, #50693, #102653, #196939, #839, #182819, #115749, #66905, #32314, #48579, #67972, #131989, #14965, #197998, #200125, #117895, #213173, #69051, #183888, #52825, #35500, #19245, #151409, #118962, #184940, #16032, #36567, #81062, #147147, #82116, #148209, #125117, #191075, #20314, #120037, #61097, #21365, #174873, #9142, #206265, #4047, #42742, #60027, #70117, #169776, #142384, #140244, #143455, #86400, #8064, #157546, #93622, #90405, #41671, #159664, #168710, #92562, #127256, #27523, #173807, #126178, #74150, #108847, #26453, #158602, #10201, #76276, #208393, #136228, #192142, #43806, #156475, #77343, #109919, #57890, #53901, #44874, #193227, #37647, #202250, #175930, #11265, #152467, #209453, #186011, #75216, #124053, #103725, #190019, #107782, #25386, #91485, #141327, #207340, #58962, #115245, #110979, #29675, #98939, #79478, #81608, #94692, #31810, #114189, #180188, #62171, #161812, #194293, #210537, #176985, #144528, #211592, #181235, #14456, #196434, #130446, #113118, #212659, #147692, #95759, #179124, #198536, #28603, #213710, #160733, #65333, #145596, #13402, #78407, #129391, #96827, #30746, #164993, #148750, #16584, #80547, #48078, #63228, #97886, #128330, #12327, #162876, #195370, #112057, #64301, #146644, #163947, #47002, #131480, #45938, #15522, #197484, #49127, #32863, #82666, #320, #66390, #132538, #178057, #34976, #166061, #67455, #83732, #102126, #101047, #4588, #85877, #54450, #53373, #133601, #202801, #199606, #120593, #1394, #118442, #99995, #117374, #37119, #154085, #70662, #153012, #151954, #88014, #103198, #200663, #3524, #136772, #69598, #38198, #68532, #168195, #119508, #186570, #134660, #19794, #185494, #135706, #201732, #169260, #149824, #33920, #51249, #104271, #116303, #170316 ),
 ( #183371, #20846, #86945, #52312, #167137, #21904, #182293, #5653, #71733, #137847, #84806, #50182, #184429, #17648, #18722, #150895, #2456, #36046, #6737, #22983, #41423, #188710, #158360, #25134, #208146, #207083, #72816, #142132, #138918, #59776, #155156, #57652, #39261, #56588, #190829, #93373, #9953, #92319, #91236, #27266, #42488, #139995, #157296, #76029, #8886, #191892, #7809, #107531, #58714, #125934, #73902, #173562, #124863, #74965, #141075, #108597, #89102, #187634, #204937, #43554, #55512, #109675, #122748, #174625, #40346, #175677, #159409, #121667, #26201, #11009, #77086, #106452, #203868, #105355, #171392, #172476, #24063, #90166, #156232, #206016, #123811, #189772, #61917, #131240, #111800, #113935, #127005, #64044, #146388, #212402, #94440, #194033, #12086, #28345, #209203, #176731, #29422, #147436, #46751, #14197, #162621, #145343, #30490, #179931, #128077, #211344, #16326, #60843, #31555, #192963, #97630, #177806, #45684, #110731, #161561, #129138, #62969, #197227, #180983, #48867, #112863, #80290, #95513, #130189, #160479, #143213, #195114, #13149, #144284, #96574, #178878, #196182, #79226, #163687, #44616, #47824, #15269, #81356, #213460, #65084, #114983, #32604, #98679, #164735, #78153, #210277, #99735, #116044, #134406, #67202, #36852, #118183, #86681, #85612, #165807, #20595, #17391, #152748, #33661, #150636, #132274, #149555, #69336, #186301, #102936, #185229, #184171, #120325, #135447, #18468, #35791, #168996, #101867, #70399, #100792, #200410, #151700, #4330, #166877, #52056, #3269, #167935, #19535, #201469, #182032, #66130, #83474, #136517, #148498, #202536, #1140, #53112, #133339, #54185, #37937, #66, #119245, #104011, #170056, #199343, #82409, #198282, #49923, #50990, #117111, #183113, #34721, #84546, #2197, #68274, #154894, #9691, #204672, #206819, #5395, #157034, #24868, #90972, #187375, #72552, #105090, #121403, #87748, #55256, #122481, #25937, #139729, #107266, #41157, #23802, #123547, #58453, #6475, #89907, #109411, #153824, #124608, #71474, #190566, #56321, #138650, #203603, #40076, #7545, #155959, #75768, #59508, #141876, #205752, #173286, #188442, #88836, #106188, #158102, #21641, #8621, #125665, #92045, #73630, #42222, #172213, #74703, #140807, #108339, #174359, #189512, #207885, #137586, #191627, #43290, #57383, #39006, #171128, #22722, #60575, #48612, #64836, #44348, #208940, #146125, #13939, #61649, #175416, #93106, #128860, #31292, #163425, #142940, #145073, #144014, #45417, #47558, #80022, #196973, #162360, #111533, #194842, #15002, #81093, #110470, #212138, #78951, #113668, #10749, #210007, #126734, #112598, #29151, #211076, #46475, #160216, #76820, #11817, #179672, #176471, #147181, #127816, #95240, #192694, #178610, #30220, #193771, #177540, #161289, #62699, #97367, #63774, #96304, #129932, #27000, #28081, #12875, #195921, #213207, #130982, #94177, #77893 ) ),
 .UNSPECIFIED., .F., .F., .F. ) 
 B_SPLINE_SURFACE_WITH_KNOTS ( ( 2, 2 ),
 ( 3, 2, 2, 2, 2, 2, 2, 2, 2, 2, 2, 2, 2, 2, 2, 2, 2, 2, 2, 2, 2, 2, 2, 2, 2, 2, 2, 2, 2, 2, 2, 2, 2, 2, 2, 2, 2, 2, 2, 2, 2, 2, 2, 2, 2, 2, 2, 2, 2, 2, 2, 2, 2, 2, 2, 2, 2, 2, 2, 2, 2, 2, 2, 2, 2, 2, 2, 2, 2, 2, 2, 2, 2, 2, 2, 2, 2, 2, 2, 2, 2, 2, 2, 2, 2, 2, 2, 2, 2, 2, 2, 2, 2, 2, 2, 2, 2, 2, 2, 2, 2, 2, 2, 2, 2, 2, 2, 2, 2, 2, 2, 2, 2, 2, 2, 2, 2, 2, 2, 2, 2, 2, 2, 2, 2, 2, 2, 2, 2, 2, 2, 2, 2, 2, 2, 2, 2, 2, 2, 2, 2, 2, 2, 2, 2, 2, 2, 2, 2, 2, 2, 2, 2, 2, 2, 2, 2, 2, 2, 2, 2, 2, 2, 2, 2, 2, 2, 2, 3 ),
 ( 0.000000000000000000, 1.000000000000000000 ),
 ( 0.000000000000000000, 0.005952380952380952051, 0.01190476190476190410, 0.01785714285714285615, 0.02380952380952380820, 0.02976190476190476025, 0.03571428571428571230, 0.04166666666666666435, 0.04761904761904761640, 0.05357142857142856845, 0.05952380952380952051, 0.06547619047619047949, 0.07142857142857142461, 0.07738095238095238360, 0.08333333333333332871, 0.08928571428571428770, 0.09523809523809523281, 0.1011904761904761918, 0.1071428571428571369, 0.1130952380952380959, 0.1190476190476190410, 0.1250000000000000000, 0.1309523809523809590, 0.1369047619047619180, 0.1428571428571428492, 0.1488095238095238082, 0.1547619047619047672, 0.1607142857142857262, 0.1666666666666666574, 0.1726190476190476164, 0.1785714285714285754, 0.1845238095238095344, 0.1904761904761904656, 0.1964285714285714246, 0.2023809523809523836, 0.2083333333333333426, 0.2142857142857142738, 0.2202380952380952328, 0.2261904761904761918, 0.2321428571428571508, 0.2380952380952380820, 0.2440476190476190410, 0.2500000000000000000, 0.2559523809523809312, 0.2619047619047619180, 0.2678571428571428492, 0.2738095238095238360, 0.2797619047619047672, 0.2857142857142856984, 0.2916666666666666852, 0.2976190476190476164, 0.3035714285714285476, 0.3095238095238095344, 0.3154761904761904656, 0.3214285714285714524, 0.3273809523809523836, 0.3333333333333333148, 0.3392857142857143016, 0.3452380952380952328, 0.3511904761904761640, 0.3571428571428571508, 0.3630952380952380820, 0.3690476190476190688, 0.3750000000000000000, 0.3809523809523809312, 0.3869047619047619180, 0.3928571428571428492, 0.3988095238095238360, 0.4047619047619047672, 0.4107142857142856984, 0.4166666666666666852, 0.4226190476190476164, 0.4285714285714285476, 0.4345238095238095344, 0.4404761904761904656, 0.4464285714285714524, 0.4523809523809523836, 0.4583333333333333148, 0.4642857142857143016, 0.4702380952380952328, 0.4761904761904761640, 0.4821428571428571508, 0.4880952380952380820, 0.4940476190476190688, 0.5000000000000000000, 0.5059523809523809312, 0.5119047619047618625, 0.5178571428571429047, 0.5238095238095238360, 0.5297619047619047672, 0.5357142857142856984, 0.5416666666666666297, 0.5476190476190476719, 0.5535714285714286031, 0.5595238095238095344, 0.5654761904761904656, 0.5714285714285713969, 0.5773809523809523281, 0.5833333333333333703, 0.5892857142857143016, 0.5952380952380952328, 0.6011904761904761640, 0.6071428571428570953, 0.6130952380952381375, 0.6190476190476190688, 0.6250000000000000000, 0.6309523809523809312, 0.6369047619047618625, 0.6428571428571429047, 0.6488095238095238360, 0.6547619047619047672, 0.6607142857142856984, 0.6666666666666666297, 0.6726190476190476719, 0.6785714285714286031, 0.6845238095238095344, 0.6904761904761904656, 0.6964285714285713969, 0.7023809523809523281, 0.7083333333333333703, 0.7142857142857143016, 0.7202380952380952328, 0.7261904761904761640, 0.7321428571428570953, 0.7380952380952381375, 0.7440476190476190688, 0.7500000000000000000, 0.7559523809523809312, 0.7619047619047618625, 0.7678571428571429047, 0.7738095238095238360, 0.7797619047619047672, 0.7857142857142856984, 0.7916666666666666297, 0.7976190476190476719, 0.8035714285714286031, 0.8095238095238095344, 0.8154761904761904656, 0.8214285714285713969, 0.8273809523809523281, 0.8333333333333333703, 0.8392857142857143016, 0.8452380952380952328, 0.8511904761904761640, 0.8571428571428570953, 0.8630952380952381375, 0.8690476190476190688, 0.8750000000000000000, 0.8809523809523809312, 0.8869047619047618625, 0.8928571428571429047, 0.8988095238095238360, 0.9047619047619047672, 0.9107142857142856984, 0.9166666666666666297, 0.9226190476190476719, 0.9285714285714286031, 0.9345238095238095344, 0.9404761904761904656, 0.9464285714285713969, 0.9523809523809523281, 0.9583333333333333703, 0.9642857142857143016, 0.9702380952380952328, 0.9761904761904761640, 0.9821428571428570953, 0.9880952380952381375, 0.9940476190476190688, 1.000000000000000000 ),
 .UNSPECIFIED. ) 
 GEOMETRIC_REPRESENTATION_ITEM ( )  RATIONAL_B_SPLINE_SURFACE ( (
 ( 1.000000000000000000, 0.8660254037844387076, 1.000000000000000000, 0.8660254037844387076, 1.000000000000000000, 0.8660254037844387076, 1.000000000000000000, 0.8660254037844387076, 1.000000000000000000, 0.8660254037844387076, 1.000000000000000000, 0.8660254037844387076, 1.000000000000000000, 0.8660254037844387076, 1.000000000000000000, 0.8660254037844387076, 1.000000000000000000, 0.8660254037844387076, 1.000000000000000000, 0.8660254037844387076, 1.000000000000000000, 0.8660254037844387076, 1.000000000000000000, 0.8660254037844387076, 1.000000000000000000, 0.8660254037844387076, 1.000000000000000000, 0.8660254037844387076, 1.000000000000000000, 0.8660254037844387076, 1.000000000000000000, 0.8660254037844387076, 1.000000000000000000, 0.8660254037844387076, 1.000000000000000000, 0.8660254037844387076, 1.000000000000000000, 0.8660254037844387076, 1.000000000000000000, 0.8660254037844387076, 1.000000000000000000, 0.8660254037844387076, 1.000000000000000000, 0.8660254037844387076, 1.000000000000000000, 0.8660254037844387076, 1.000000000000000000, 0.8660254037844387076, 1.000000000000000000, 0.8660254037844387076, 1.000000000000000000, 0.8660254037844387076, 1.000000000000000000, 0.8660254037844387076, 1.000000000000000000, 0.8660254037844387076, 1.000000000000000000, 0.8660254037844387076, 1.000000000000000000, 0.8660254037844387076, 1.000000000000000000, 0.8660254037844387076, 1.000000000000000000, 0.8660254037844387076, 1.000000000000000000, 0.8660254037844387076, 1.000000000000000000, 0.8660254037844387076, 1.000000000000000000, 0.8660254037844387076, 1.000000000000000000, 0.8660254037844387076, 1.000000000000000000, 0.8660254037844387076, 1.000000000000000000, 0.8660254037844387076, 1.000000000000000000, 0.8660254037844387076, 1.000000000000000000, 0.8660254037844387076, 1.000000000000000000, 0.8660254037844387076, 1.000000000000000000, 0.8660254037844387076, 1.000000000000000000, 0.8660254037844387076, 1.000000000000000000, 0.8660254037844387076, 1.000000000000000000, 0.8660254037844387076, 1.000000000000000000, 0.8660254037844387076, 1.000000000000000000, 0.8660254037844387076, 1.000000000000000000, 0.8660254037844387076, 1.000000000000000000, 0.8660254037844387076, 1.000000000000000000, 0.8660254037844387076, 1.000000000000000000, 0.8660254037844387076, 1.000000000000000000, 0.8660254037844387076, 1.000000000000000000, 0.8660254037844387076, 1.000000000000000000, 0.8660254037844387076, 1.000000000000000000, 0.8660254037844387076, 1.000000000000000000, 0.8660254037844387076, 1.000000000000000000, 0.8660254037844387076, 1.000000000000000000, 0.8660254037844387076, 1.000000000000000000, 0.8660254037844387076, 1.000000000000000000, 0.8660254037844387076, 1.000000000000000000, 0.8660254037844387076, 1.000000000000000000, 0.8660254037844387076, 1.000000000000000000, 0.8660254037844387076, 1.000000000000000000, 0.8660254037844387076, 1.000000000000000000, 0.8660254037844387076, 1.000000000000000000, 0.8660254037844387076, 1.000000000000000000, 0.8660254037844387076, 1.000000000000000000, 0.8660254037844387076, 1.000000000000000000, 0.8660254037844387076, 1.000000000000000000, 0.8660254037844387076, 1.000000000000000000, 0.8660254037844387076, 1.000000000000000000, 0.8660254037844387076, 1.000000000000000000, 0.8660254037844387076, 1.000000000000000000, 0.8660254037844387076, 1.000000000000000000, 0.8660254037844387076, 1.000000000000000000, 0.8660254037844387076, 1.000000000000000000, 0.8660254037844387076, 1.000000000000000000, 0.8660254037844387076, 1.000000000000000000, 0.8660254037844387076, 1.000000000000000000, 0.8660254037844387076, 1.000000000000000000, 0.8660254037844387076, 1.000000000000000000, 0.8660254037844387076, 1.000000000000000000, 0.8660254037844387076, 1.000000000000000000, 0.8660254037844387076, 1.000000000000000000, 0.8660254037844387076, 1.000000000000000000, 0.8660254037844387076, 1.000000000000000000, 0.8660254037844387076, 1.000000000000000000, 0.8660254037844387076, 1.000000000000000000, 0.8660254037844387076, 1.000000000000000000, 0.8660254037844387076, 1.000000000000000000, 0.8660254037844387076, 1.000000000000000000, 0.8660254037844387076, 1.000000000000000000, 0.8660254037844387076, 1.000000000000000000, 0.8660254037844387076, 1.000000000000000000, 0.8660254037844387076, 1.000000000000000000, 0.8660254037844387076, 1.000000000000000000, 0.8660254037844387076, 1.000000000000000000, 0.8660254037844387076, 1.000000000000000000, 0.8660254037844387076, 1.000000000000000000, 0.8660254037844387076, 1.000000000000000000, 0.8660254037844387076, 1.000000000000000000, 0.8660254037844387076, 1.000000000000000000, 0.8660254037844387076, 1.000000000000000000, 0.8660254037844387076, 1.000000000000000000, 0.8660254037844387076, 1.000000000000000000, 0.8660254037844387076, 1.000000000000000000, 0.8660254037844387076, 1.000000000000000000, 0.8660254037844387076, 1.000000000000000000, 0.8660254037844387076, 1.000000000000000000, 0.8660254037844387076, 1.000000000000000000, 0.8660254037844387076, 1.000000000000000000, 0.8660254037844387076, 1.000000000000000000, 0.8660254037844387076, 1.000000000000000000, 0.8660254037844387076, 1.000000000000000000, 0.8660254037844387076, 1.000000000000000000, 0.8660254037844387076, 1.000000000000000000, 0.8660254037844387076, 1.000000000000000000, 0.8660254037844387076, 1.000000000000000000, 0.8660254037844387076, 1.000000000000000000, 0.8660254037844387076, 1.000000000000000000, 0.8660254037844387076, 1.000000000000000000, 0.8660254037844387076, 1.000000000000000000, 0.8660254037844387076, 1.000000000000000000, 0.8660254037844387076, 1.000000000000000000, 0.8660254037844387076, 1.000000000000000000, 0.8660254037844387076, 1.000000000000000000, 0.8660254037844387076, 1.000000000000000000, 0.8660254037844387076, 1.000000000000000000, 0.8660254037844387076, 1.000000000000000000, 0.8660254037844387076, 1.000000000000000000, 0.8660254037844387076, 1.000000000000000000, 0.8660254037844387076, 1.000000000000000000, 0.8660254037844387076, 1.000000000000000000, 0.8660254037844387076, 1.000000000000000000, 0.8660254037844387076, 1.000000000000000000, 0.8660254037844387076, 1.000000000000000000, 0.8660254037844387076, 1.000000000000000000, 0.8660254037844387076, 1.000000000000000000, 0.8660254037844387076, 1.000000000000000000, 0.8660254037844387076, 1.000000000000000000, 0.8660254037844387076, 1.000000000000000000, 0.8660254037844387076, 1.000000000000000000, 0.8660254037844387076, 1.000000000000000000, 0.8660254037844387076, 1.000000000000000000, 0.8660254037844387076, 1.000000000000000000, 0.8660254037844387076, 1.000000000000000000, 0.8660254037844387076, 1.000000000000000000, 0.8660254037844387076, 1.000000000000000000, 0.8660254037844387076, 1.000000000000000000, 0.8660254037844387076, 1.000000000000000000, 0.8660254037844387076, 1.000000000000000000, 0.8660254037844387076, 1.000000000000000000, 0.8660254037844387076, 1.000000000000000000, 0.8660254037844387076, 1.000000000000000000, 0.8660254037844387076, 1.000000000000000000, 0.8660254037844387076, 1.000000000000000000, 0.8660254037844387076, 1.000000000000000000, 0.8660254037844387076, 1.000000000000000000, 0.8660254037844387076, 1.000000000000000000, 0.8660254037844387076, 1.000000000000000000, 0.8660254037844387076, 1.000000000000000000, 0.8660254037844387076, 1.000000000000000000, 0.8660254037844387076, 1.000000000000000000, 0.8660254037844387076, 1.000000000000000000, 0.8660254037844387076, 1.000000000000000000, 0.8660254037844387076, 1.000000000000000000, 0.8660254037844387076, 1.000000000000000000, 0.8660254037844387076, 1.000000000000000000),
 ( 1.000000000000000000, 0.8660254037844387076, 1.000000000000000000, 0.8660254037844387076, 1.000000000000000000, 0.8660254037844387076, 1.000000000000000000, 0.8660254037844387076, 1.000000000000000000, 0.8660254037844387076, 1.000000000000000000, 0.8660254037844387076, 1.000000000000000000, 0.8660254037844387076, 1.000000000000000000, 0.8660254037844387076, 1.000000000000000000, 0.8660254037844387076, 1.000000000000000000, 0.8660254037844387076, 1.000000000000000000, 0.8660254037844387076, 1.000000000000000000, 0.8660254037844387076, 1.000000000000000000, 0.8660254037844387076, 1.000000000000000000, 0.8660254037844387076, 1.000000000000000000, 0.8660254037844387076, 1.000000000000000000, 0.8660254037844387076, 1.000000000000000000, 0.8660254037844387076, 1.000000000000000000, 0.8660254037844387076, 1.000000000000000000, 0.8660254037844387076, 1.000000000000000000, 0.8660254037844387076, 1.000000000000000000, 0.8660254037844387076, 1.000000000000000000, 0.8660254037844387076, 1.000000000000000000, 0.8660254037844387076, 1.000000000000000000, 0.8660254037844387076, 1.000000000000000000, 0.8660254037844387076, 1.000000000000000000, 0.8660254037844387076, 1.000000000000000000, 0.8660254037844387076, 1.000000000000000000, 0.8660254037844387076, 1.000000000000000000, 0.8660254037844387076, 1.000000000000000000, 0.8660254037844387076, 1.000000000000000000, 0.8660254037844387076, 1.000000000000000000, 0.8660254037844387076, 1.000000000000000000, 0.8660254037844387076, 1.000000000000000000, 0.8660254037844387076, 1.000000000000000000, 0.8660254037844387076, 1.000000000000000000, 0.8660254037844387076, 1.000000000000000000, 0.8660254037844387076, 1.000000000000000000, 0.8660254037844387076, 1.000000000000000000, 0.8660254037844387076, 1.000000000000000000, 0.8660254037844387076, 1.000000000000000000, 0.8660254037844387076, 1.000000000000000000, 0.8660254037844387076, 1.000000000000000000, 0.8660254037844387076, 1.000000000000000000, 0.8660254037844387076, 1.000000000000000000, 0.8660254037844387076, 1.000000000000000000, 0.8660254037844387076, 1.000000000000000000, 0.8660254037844387076, 1.000000000000000000, 0.8660254037844387076, 1.000000000000000000, 0.8660254037844387076, 1.000000000000000000, 0.8660254037844387076, 1.000000000000000000, 0.8660254037844387076, 1.000000000000000000, 0.8660254037844387076, 1.000000000000000000, 0.8660254037844387076, 1.000000000000000000, 0.8660254037844387076, 1.000000000000000000, 0.8660254037844387076, 1.000000000000000000, 0.8660254037844387076, 1.000000000000000000, 0.8660254037844387076, 1.000000000000000000, 0.8660254037844387076, 1.000000000000000000, 0.8660254037844387076, 1.000000000000000000, 0.8660254037844387076, 1.000000000000000000, 0.8660254037844387076, 1.000000000000000000, 0.8660254037844387076, 1.000000000000000000, 0.8660254037844387076, 1.000000000000000000, 0.8660254037844387076, 1.000000000000000000, 0.8660254037844387076, 1.000000000000000000, 0.8660254037844387076, 1.000000000000000000, 0.8660254037844387076, 1.000000000000000000, 0.8660254037844387076, 1.000000000000000000, 0.8660254037844387076, 1.000000000000000000, 0.8660254037844387076, 1.000000000000000000, 0.8660254037844387076, 1.000000000000000000, 0.8660254037844387076, 1.000000000000000000, 0.8660254037844387076, 1.000000000000000000, 0.8660254037844387076, 1.000000000000000000, 0.8660254037844387076, 1.000000000000000000, 0.8660254037844387076, 1.000000000000000000, 0.8660254037844387076, 1.000000000000000000, 0.8660254037844387076, 1.000000000000000000, 0.8660254037844387076, 1.000000000000000000, 0.8660254037844387076, 1.000000000000000000, 0.8660254037844387076, 1.000000000000000000, 0.8660254037844387076, 1.000000000000000000, 0.8660254037844387076, 1.000000000000000000, 0.8660254037844387076, 1.000000000000000000, 0.8660254037844387076, 1.000000000000000000, 0.8660254037844387076, 1.000000000000000000, 0.8660254037844387076, 1.000000000000000000, 0.8660254037844387076, 1.000000000000000000, 0.8660254037844387076, 1.000000000000000000, 0.8660254037844387076, 1.000000000000000000, 0.8660254037844387076, 1.000000000000000000, 0.8660254037844387076, 1.000000000000000000, 0.8660254037844387076, 1.000000000000000000, 0.8660254037844387076, 1.000000000000000000, 0.8660254037844387076, 1.000000000000000000, 0.8660254037844387076, 1.000000000000000000, 0.8660254037844387076, 1.000000000000000000, 0.8660254037844387076, 1.000000000000000000, 0.8660254037844387076, 1.000000000000000000, 0.8660254037844387076, 1.000000000000000000, 0.8660254037844387076, 1.000000000000000000, 0.8660254037844387076, 1.000000000000000000, 0.8660254037844387076, 1.000000000000000000, 0.8660254037844387076, 1.000000000000000000, 0.8660254037844387076, 1.000000000000000000, 0.8660254037844387076, 1.000000000000000000, 0.8660254037844387076, 1.000000000000000000, 0.8660254037844387076, 1.000000000000000000, 0.8660254037844387076, 1.000000000000000000, 0.8660254037844387076, 1.000000000000000000, 0.8660254037844387076, 1.000000000000000000, 0.8660254037844387076, 1.000000000000000000, 0.8660254037844387076, 1.000000000000000000, 0.8660254037844387076, 1.000000000000000000, 0.8660254037844387076, 1.000000000000000000, 0.8660254037844387076, 1.000000000000000000, 0.8660254037844387076, 1.000000000000000000, 0.8660254037844387076, 1.000000000000000000, 0.8660254037844387076, 1.000000000000000000, 0.8660254037844387076, 1.000000000000000000, 0.8660254037844387076, 1.000000000000000000, 0.8660254037844387076, 1.000000000000000000, 0.8660254037844387076, 1.000000000000000000, 0.8660254037844387076, 1.000000000000000000, 0.8660254037844387076, 1.000000000000000000, 0.8660254037844387076, 1.000000000000000000, 0.8660254037844387076, 1.000000000000000000, 0.8660254037844387076, 1.000000000000000000, 0.8660254037844387076, 1.000000000000000000, 0.8660254037844387076, 1.000000000000000000, 0.8660254037844387076, 1.000000000000000000, 0.8660254037844387076, 1.000000000000000000, 0.8660254037844387076, 1.000000000000000000, 0.8660254037844387076, 1.000000000000000000, 0.8660254037844387076, 1.000000000000000000, 0.8660254037844387076, 1.000000000000000000, 0.8660254037844387076, 1.000000000000000000, 0.8660254037844387076, 1.000000000000000000, 0.8660254037844387076, 1.000000000000000000, 0.8660254037844387076, 1.000000000000000000, 0.8660254037844387076, 1.000000000000000000, 0.8660254037844387076, 1.000000000000000000, 0.8660254037844387076, 1.000000000000000000, 0.8660254037844387076, 1.000000000000000000, 0.8660254037844387076, 1.000000000000000000, 0.8660254037844387076, 1.000000000000000000, 0.8660254037844387076, 1.000000000000000000, 0.8660254037844387076, 1.000000000000000000, 0.8660254037844387076, 1.000000000000000000, 0.8660254037844387076, 1.000000000000000000, 0.8660254037844387076, 1.000000000000000000, 0.8660254037844387076, 1.000000000000000000, 0.8660254037844387076, 1.000000000000000000, 0.8660254037844387076, 1.000000000000000000, 0.8660254037844387076, 1.000000000000000000, 0.8660254037844387076, 1.000000000000000000, 0.8660254037844387076, 1.000000000000000000, 0.8660254037844387076, 1.000000000000000000, 0.8660254037844387076, 1.000000000000000000, 0.8660254037844387076, 1.000000000000000000, 0.8660254037844387076, 1.000000000000000000, 0.8660254037844387076, 1.000000000000000000, 0.8660254037844387076, 1.000000000000000000, 0.8660254037844387076, 1.000000000000000000, 0.8660254037844387076, 1.000000000000000000, 0.8660254037844387076, 1.000000000000000000, 0.8660254037844387076, 1.000000000000000000, 0.8660254037844387076, 1.000000000000000000) ) ) 
 REPRESENTATION_ITEM ( '' )  SURFACE ( )  );
#172575 = ORIENTED_EDGE ( 'NONE', *, *, #25641, .T. ) ;
#172576 = CARTESIAN_POINT ( 'NONE',  ( 3.580628178849315280, -1.282259035790348722, 1.418852674340838060 ) ) ;
#172577 = CARTESIAN_POINT ( 'NONE',  ( 4.944116541256327935, 1.765280609655010879, 0.1280878748119110566 ) ) ;
#172578 = CARTESIAN_POINT ( 'NONE',  ( 4.688087255275310561, 8.691461907788344377, -0.7998128361456381397 ) ) ;
#172579 = CARTESIAN_POINT ( 'NONE',  ( -5.413783410558481002, 5.210502155273325720, -0.7998128361456221525 ) ) ;
#172580 = CARTESIAN_POINT ( 'NONE',  ( 0.2459857770662046417, 0.9310377468562742731, -1.553837941864342875 ) ) ;
#172582 = CARTESIAN_POINT ( 'NONE',  ( 0.2510146965912671835, 0.1847738873272772309, -1.906744464555621521 ) ) ;
#172581 = CARTESIAN_POINT ( 'NONE',  ( 1.438721403194443083, 7.870009100115442635, -3.684356824108416362 ) ) ;
#172583 = CIRCLE ( 'NONE', #10058, 0.04999999999999991257 ) ;
#172584 = B_SPLINE_CURVE_WITH_KNOTS ( 'NONE', 3,
 ( #63711, #162290, #195852, #31226, #148177, #115718, #97300, #17070, #127750, #193707, #166548, #202216, #52791, #118930, #36534, #102621 ),
 .UNSPECIFIED., .F., .F.,
 ( 4, 2, 2, 2, 2, 2, 2, 4 ),
 ( 0.000000000000000000, 8.859500144023226638E-05, 0.0001771900028804645328, 0.0003543800057609234819, 0.0007087600115218431690, 0.001063140017282762856, 0.001240330020163218959, 0.001417520023043675279 ),
 .UNSPECIFIED. ) ;
#172585 = CARTESIAN_POINT ( 'NONE',  ( 0.5200892513525963157, 2.048054262204841880, -0.3022008342252607838 ) ) ;
#172586 = CARTESIAN_POINT ( 'NONE',  ( 0.6823417656249864960, -0.5114583329919111243, -1.181850606188749264 ) ) ;
#172587 = CARTESIAN_POINT ( 'NONE',  ( 6.368025811218641863, 0.9635043244729593059, 1.603280169136585220 ) ) ;
#172588 = CARTESIAN_POINT ( 'NONE',  ( 3.000428103051573814, -0.5303778429210231904, -1.746945217264872507 ) ) ;
#172590 = CARTESIAN_POINT ( 'NONE',  ( 6.361499291607088935, 6.832587723092125032, 0.6030276918116053153 ) ) ;
#172589 = CARTESIAN_POINT ( 'NONE',  ( 6.252570086353132162, 0.6882034672392455255, 2.096894461246688213 ) ) ;
#172591 = EDGE_CURVE ( 'NONE', #213109, #167380, #138858, .T. ) ;
#172592 = CARTESIAN_POINT ( 'NONE',  ( 1.364683531249986537, 0.1135416670080857532, 0.7879004041258500513 ) ) ;
#172593 = CARTESIAN_POINT ( 'NONE',  ( 3.156738326643961923, -0.5960753502360670586, -1.974691822637637761 ) ) ;
#172594 = CARTESIAN_POINT ( 'NONE',  ( -8.552495972122143186, 8.872333477097637200, 0.7998128361456462443 ) ) ;
#172595 = CARTESIAN_POINT ( 'NONE',  ( 9.752392566931574081, 10.27221283770866300, -0.7998128361456281477 ) ) ;
#172596 = CARTESIAN_POINT ( 'NONE',  ( 4.517891501851804215, 6.293959390292322986, -1.599625672291255185 ) ) ;
#172597 = CARTESIAN_POINT ( 'NONE',  ( 0.9312127099814873077, 0.1580370610147242560, 2.155845405312675211 ) ) ;
#172598 = CARTESIAN_POINT ( 'NONE',  ( 0.2038950025188591975, -1.678810847859620869, -1.376375048264495859 ) ) ;
#172599 = CARTESIAN_POINT ( 'NONE',  ( -1.402160292154681736E-14, 0.3843750003414230232, 1.575800808251672791 ) ) ;
#172600 = CARTESIAN_POINT ( 'NONE',  ( 4.235729478701364847, -1.487246874726022350, -1.568870776130903089 ) ) ;
#172602 = CARTESIAN_POINT ( 'NONE',  ( 2.629291921057617554, 0.09916324773191761976, -1.959495597191794225 ) ) ;
#172601 = CARTESIAN_POINT ( 'NONE',  ( 4.705726078268232193, 1.497967940706146805, 1.354894159888963001 ) ) ;
#172603 = CARTESIAN_POINT ( 'NONE',  ( 6.720655732516649827, 2.940181725866806151, 2.725612257524675730 ) ) ;
#172604 = ADVANCED_FACE ( 'NONE', ( #133942 ), #183499, .F. ) ;
#172605 = ORIENTED_EDGE ( 'NONE', *, *, #212483, .T. ) ;
#172608 = CARTESIAN_POINT ( 'NONE',  ( 5.639828713604826405, 9.523624565940227882, -0.7216878364870267237 ) ) ;
#172607 = CARTESIAN_POINT ( 'NONE',  ( 2.520459450608881991, -4.091624429771669291, -2.338646429533238535 ) ) ;
#172606 = DIRECTION ( 'NONE',  ( 0.6249999999996046496, -1.550603090070706853E-14, -0.7806247498001163132 ) ) ;
#172609 = CARTESIAN_POINT ( 'NONE',  ( -5.596483547390937119, 9.751257581923240991, 0.000000000000000000 ) ) ;
#172610 = CARTESIAN_POINT ( 'NONE',  ( 3.028530041973789722, 0.4946322284519070189, 1.954779462066410733 ) ) ;
#172612 = FILL_AREA_STYLE ('',( #135840 ) ) ;
#172611 = CARTESIAN_POINT ( 'NONE',  ( -2.767835915484202047, 6.380892334706859792, -0.7998128361456281477 ) ) ;
#172613 = CARTESIAN_POINT ( 'NONE',  ( -0.7499999999999972244, 5.639583334016151639, -1.299038105676652899 ) ) ;
#172614 = CARTESIAN_POINT ( 'NONE',  ( 5.502191098127390489, -0.8541586074963626318, 1.711093258865265421 ) ) ;
#172615 = CARTESIAN_POINT ( 'NONE',  ( -11.86145017354119879, 12.59514365543876124, 1.099999999999996980 ) ) ;
#172616 = CARTESIAN_POINT ( 'NONE',  ( 6.466876083594112146, 6.647036307055676829, -0.7216878364870257245 ) ) ;
#172618 = CARTESIAN_POINT ( 'NONE',  ( 3.761342352588430860, 1.897692735847063661, -0.6820134568972098243 ) ) ;
#172617 = CARTESIAN_POINT ( 'NONE',  ( -7.659993601596713830, 9.959745173328078849, -1.443375672974058777 ) ) ;
#172619 = CARTESIAN_POINT ( 'NONE',  ( 0.7499999999999902300, 3.733333333333352488, 1.299038105676669330 ) ) ;
#172620 = CARTESIAN_POINT ( 'NONE',  ( -0.6823417656250039265, 15.13020833367473372, -1.181850606188755259 ) ) ;
#172621 = CARTESIAN_POINT ( 'NONE',  ( 5.983370841356476788, 1.591773204597257463, -0.6646525218769030463 ) ) ;
#172622 = CARTESIAN_POINT ( 'NONE',  ( 5.338878628731272613, 9.450718510153643948, -0.7998128361456481317 ) ) ;
#172623 = CARTESIAN_POINT ( 'NONE',  ( 9.436111725431318931, 10.11114455586577776, -0.7216878364870257245 ) ) ;
#172624 = DIRECTION ( 'NONE',  ( 0.000000000000000000, 1.000000000000000000, 0.000000000000000000 ) ) ;
#172625 = CARTESIAN_POINT ( 'NONE',  ( 4.130043426961079511, 1.002751595458702738, -1.578879078160302818 ) ) ;
#172626 = DIRECTION ( 'NONE',  ( 0.000000000000000000, 1.000000000000000000, 0.000000000000000000 ) ) ;
#172628 =( BOUNDED_CURVE ( )  B_SPLINE_CURVE ( 2, ( #39166, #22882, #88998, #204831, #120493, #172371, #56483, #23961, #20751 ),
 .UNSPECIFIED., .F., .T. ) 
 B_SPLINE_CURVE_WITH_KNOTS ( ( 3, 2, 2, 2, 3 ),
 ( 0.6696428571428570953, 0.6726190476190476719, 0.6785714285714286031, 0.6845238095238095344, 0.6875000000000000000 ),
 .UNSPECIFIED. ) 
 CURVE ( )  GEOMETRIC_REPRESENTATION_ITEM ( )  RATIONAL_B_SPLINE_CURVE ( ( 0.9330127018922194093, 0.9330127018922180770, 1.000000000000000000, 0.8660254037844387076, 1.000000000000000000, 0.8660254037844387076, 1.000000000000000000, 0.9330127018922194093, 0.9330127018922194093 ) ) 
 REPRESENTATION_ITEM ( '' )  );
#172627 = CARTESIAN_POINT ( 'NONE',  ( 2.676698048161993082, 1.355622082481915847, -1.564734663558226879 ) ) ;
#172629 = CARTESIAN_POINT ( 'NONE',  ( -1.435115314735500691, 7.268684689231141860, -4.324912918974784581 ) ) ;
#172630 = ORIENTED_EDGE ( 'NONE', *, *, #121643, .F. ) ;
#172631 = CARTESIAN_POINT ( 'NONE',  ( 5.388439706788500594, 5.251210844200210559, 0.7998128361456352531 ) ) ;
#172633 = EDGE_CURVE ( 'NONE', #159273, #121309, #123090, .T. ) ;
#172632 = CARTESIAN_POINT ( 'NONE',  ( -3.946537740501743219, 2.817530495241825417, -0.7749999999999944711 ) ) ;
#172634 = CARTESIAN_POINT ( 'NONE',  ( 0.08776524826303951088, 1.042983370315919478, 1.480986741271082430 ) ) ;
#172635 = CARTESIAN_POINT ( 'NONE',  ( 4.543390873910913896, 5.433615786718446472, 1.082531754730549078 ) ) ;
#172636 = CARTESIAN_POINT ( 'NONE',  ( 5.608194732729899101, 5.660561533053829031, 0.1769238548265182898 ) ) ;
#172637 = CARTESIAN_POINT ( 'NONE',  ( 7.958272981097359811, 9.347368568444167636, -1.082531754730537976 ) ) ;
#172638 = CARTESIAN_POINT ( 'NONE',  ( 8.599949509769960088, 8.927695937686774386, 1.040834085586084257E-14 ) ) ;
#172640 = CARTESIAN_POINT ( 'NONE',  ( 5.642171489992906075, 0.7808347329528000369, 1.749441798972359408 ) ) ;
#172639 = CARTESIAN_POINT ( 'NONE',  ( -6.742482464697739708, 6.760651051769146491, 0.7998128361456341429 ) ) ;
#172641 = AXIS2_PLACEMENT_3D ( 'NONE', #73001, #188897, #158547 ) ;
#172642 =( LENGTH_UNIT ( ) NAMED_UNIT ( * ) SI_UNIT ( .MILLI., .METRE. ) );
#172643 = DIRECTION ( 'NONE',  ( -0.000000000000000000, -1.000000000000000000, -0.000000000000000000 ) ) ;
#172644 = EDGE_CURVE ( 'NONE', #124391, #94456, #20130, .T. ) ;
#172646 = ORIENTED_EDGE ( 'NONE', *, *, #118767, .T. ) ;
#172645 = CARTESIAN_POINT ( 'NONE',  ( 4.880572111239557920, 4.796348339308675435, -0.7216878364870197293 ) ) ;
#172647 = CARTESIAN_POINT ( 'NONE',  ( -9.002250809794013264, 9.604973487622245898, -0.7216878364870267237 ) ) ;
#172648 = CARTESIAN_POINT ( 'NONE',  ( 2.817419395390472037, -0.2130390993498078311, 2.151187356804876050 ) ) ;
#172649 = ADVANCED_FACE ( 'NONE', ( #74242, #189047 ), #4923, .T. ) ;
#172650 = CARTESIAN_POINT ( 'NONE',  ( -5.628043163448566588, 9.580151100749725757, 0.000000000000000000 ) ) ;
#172651 = CARTESIAN_POINT ( 'NONE',  ( 2.905190055078214595, 6.611415174225076186, 0.7998128361456271485 ) ) ;
#172652 = CARTESIAN_POINT ( 'NONE',  ( 0.4574861729177078229, -1.815669959853306370, 1.095388807130371900 ) ) ;
#172653 = CARTESIAN_POINT ( 'NONE',  ( 5.473610661177239933, 1.758888005172161373, -0.4887267171112125164 ) ) ;
#172654 = CARTESIAN_POINT ( 'NONE',  ( 11.69539920569646618, 6.979297235929839083, 4.155077259296042769 ) ) ;
#172655 = CARTESIAN_POINT ( 'NONE',  ( 1.053909416342192484, 1.969286043147522980, -0.09259992539933233069 ) ) ;
#172656 = CARTESIAN_POINT ( 'NONE',  ( 3.006014587165442453, -0.7710369221427433306, 1.750240277048662030 ) ) ;
#172657 = ORIENTED_EDGE ( 'NONE', *, *, #117363, .T. ) ;
#172658 = CARTESIAN_POINT ( 'NONE',  ( -11.35569630219380777, 9.987315607086337366, -3.554478010595065296 ) ) ;
#172659 = CARTESIAN_POINT ( 'NONE',  ( 5.160591359625510854, -0.6618325696593707619, -1.855173450206740071 ) ) ;
#172660 = CARTESIAN_POINT ( 'NONE',  ( 0.4451279286748652808, 0.6098585162058448583, -1.843775557458992687 ) ) ;
#172661 = ORIENTED_EDGE ( 'NONE', *, *, #87337, .F. ) ;
#172662 = CARTESIAN_POINT ( 'NONE',  ( -4.827585214917754719, 7.789877296449459365, -1.199719254218453823 ) ) ;
#172663 = CARTESIAN_POINT ( 'NONE',  ( -5.808742468812186033, 5.741564066561132940, 0.000000000000000000 ) ) ;
#172664 = CARTESIAN_POINT ( 'NONE',  ( 5.844973620822830895, 8.872867420051733234, 1.082531754730549967 ) ) ;
#172666 = ORIENTED_EDGE ( 'NONE', *, *, #96386, .T. ) ;
#172665 = CARTESIAN_POINT ( 'NONE',  ( 3.756429630051653312, 1.903336793139896788, 0.1845653119916731144 ) ) ;
#172667 = CARTESIAN_POINT ( 'NONE',  ( 1.132168909276673796, -1.401036632855560349, -1.704990472574128502 ) ) ;
#172668 = CARTESIAN_POINT ( 'NONE',  ( 9.367496997597635655, 4.469082183885419113, -7.499999999999953815 ) ) ;
#172669 = CARTESIAN_POINT ( 'NONE',  ( 6.428391161641624940, -0.9511404050406097044, -1.774240594045069841 ) ) ;
#172670 = CARTESIAN_POINT ( 'NONE',  ( 0.5654481856764899117, 7.808910395760752188, 1.918425245283303715 ) ) ;
#172672 = CARTESIAN_POINT ( 'NONE',  ( 5.823453932400854960, -1.463924103857511039, -1.387103351090559711 ) ) ;
#172671 = LINE ( 'NONE', #154281, #121664 ) ;
#172673 = CARTESIAN_POINT ( 'NONE',  ( 2.383334800519558705, -0.002349189141126820958, 2.070544812199434315 ) ) ;
#172674 = CARTESIAN_POINT ( 'NONE',  ( -6.847031270101295419, 7.946956888995021728, -1.199719254218446718 ) ) ;
#172675 = CARTESIAN_POINT ( 'NONE',  ( -4.879429750001362365, 8.060225557361109239, -0.9362273787268098335 ) ) ;
#172676 = CARTESIAN_POINT ( 'NONE',  ( 0.1105426557568081891, -0.9253945370547181914, -1.951590883024490353 ) ) ;
#172677 = CARTESIAN_POINT ( 'NONE',  ( 4.961394147597008697, 7.875711374583454827, -1.199719254218452047 ) ) ;
#172678 = SURFACE_STYLE_USAGE ( .BOTH. , #105556 ) ;
#172679 = CARTESIAN_POINT ( 'NONE',  ( 4.041739190649647817, 6.769093918182960579, -1.082531754730548412 ) ) ;
#172680 = CARTESIAN_POINT ( 'NONE',  ( 1.889151116980546385, 3.755413325229098653, -0.4000000000000479283 ) ) ;
#172681 = CARTESIAN_POINT ( 'NONE',  ( 2.354312230267378236, 5.898448035287240820, -0.7998128361456281477 ) ) ;
#172682 = CARTESIAN_POINT ( 'NONE',  ( 1.364683531250000303, 12.56770833367473372, -0.7879004041258355073 ) ) ;
#172684 = CARTESIAN_POINT ( 'NONE',  ( -5.271087860662956537, 9.371629280740593870, 0.000000000000000000 ) ) ;
#172683 = CARTESIAN_POINT ( 'NONE',  ( 6.825078400183513416, 0.6012913621265563169, 1.809472532188656890 ) ) ;
#172685 = CARTESIAN_POINT ( 'NONE',  ( 5.168516884834092551, 1.170641038942145995, 1.279587065987584982 ) ) ;
#172686 = CARTESIAN_POINT ( 'NONE',  ( -4.627410500965859264, 4.293067094081919777, 0.7998128361456341429 ) ) ;
#172687 = CARTESIAN_POINT ( 'NONE',  ( 2.026315959858393967, 1.060668813445601044, 1.777738962378045295 ) ) ;
#172688 = CARTESIAN_POINT ( 'NONE',  ( 3.849298028564145380, 0.2572143275579537591, -2.101468238826177615 ) ) ;
#172689 = CARTESIAN_POINT ( 'NONE',  ( 6.076025397218672630, 10.24044673006381245, -0.7998128361456291469 ) ) ;
#172690 = CARTESIAN_POINT ( 'NONE',  ( 0.6823417656249917140, 3.842708333674754506, 1.181850606188765695 ) ) ;
#172691 = CARTESIAN_POINT ( 'NONE',  ( 1.428490153906246007, -1.253617920133040853, 1.518890472526812419 ) ) ;
#172692 = CARTESIAN_POINT ( 'NONE',  ( 6.025359521845701671, 6.071890788804434891, 0.5399204162177869692 ) ) ;
#172693 = CARTESIAN_POINT ( 'NONE',  ( 0.01762790050853849447, -0.5081247445114078776, 1.843608005305336528 ) ) ;
#172694 = CARTESIAN_POINT ( 'NONE',  ( 3.802894434091105946, 1.965436290923015639, 1.179407150283459105 ) ) ;
#172695 = CARTESIAN_POINT ( 'NONE',  ( 1.594096589105632011, -1.816728215151931058, -0.1805768397986490248 ) ) ;
#172696 = CARTESIAN_POINT ( 'NONE',  ( 5.391302360089590628, 6.318882837306503575, -1.199719254218452047 ) ) ;
#172697 = CARTESIAN_POINT ( 'NONE',  ( 6.927853306458749749, 8.145212281365775908, 1.082531754730558626 ) ) ;
#172698 = CARTESIAN_POINT ( 'NONE',  ( -7.100719765255177229, 9.307259030929609267, -1.599625672291263179 ) ) ;
#172699 = CARTESIAN_POINT ( 'NONE',  ( 2.496342308839387680, -1.031403195114518390, 1.728778584395810114 ) ) ;
#172700 = CARTESIAN_POINT ( 'NONE',  ( 3.485159065011545376, 0.04355839926390054490, 1.961427607708134957 ) ) ;
#172701 = CARTESIAN_POINT ( 'NONE',  ( -8.995998617867369873, 10.45408546138876993, 1.199719254218462483 ) ) ;
#172702 = CARTESIAN_POINT ( 'NONE',  ( -7.088215381846223906, 7.164006121775713609, 0.7998128361456341429 ) ) ;
#172703 = CARTESIAN_POINT ( 'NONE',  ( 0.07516593201273635838, 7.629137130509072939, -2.644199648255764590 ) ) ;
#172705 = CARTESIAN_POINT ( 'NONE',  ( 4.065142161210800076, 0.2162087174472343276, -1.756520380257739822 ) ) ;
#172704 = CARTESIAN_POINT ( 'NONE',  ( 5.806606243248950250, 1.843357943042901459, 0.9862787698241348711 ) ) ;
#172706 = FACE_OUTER_BOUND ( 'NONE', #194846, .T. ) ;
#172707 = ADVANCED_FACE ( 'NONE', ( #6001 ), #6357, .T. ) ;
#172708 = CARTESIAN_POINT ( 'NONE',  ( 0.5861907285475282947, -2.175377356269320828, -0.2643977408666315365 ) ) ;
#172709 = CARTESIAN_POINT ( 'NONE',  ( 5.736210779895188239, 0.3457693788900301768, 1.705448404129115580 ) ) ;
#172710 = AXIS2_PLACEMENT_3D ( 'NONE', #146998, #98234, #15877 ) ;
#172711 = CARTESIAN_POINT ( 'NONE',  ( 6.753933077901968396, 11.03133902419432566, 0.7998128361456462443 ) ) ;
#172712 = CARTESIAN_POINT ( 'NONE',  ( 1.286813488861806354, 4.047007041464545374, -0.4595522011843541366 ) ) ;
#172713 = CARTESIAN_POINT ( 'NONE',  ( 5.818996626390088522, 1.136386364665368687, -1.998068361519554248 ) ) ;
#172714 = DIRECTION ( 'NONE',  ( 0.000000000000000000, 0.000000000000000000, 1.000000000000000000 ) ) ;
#172715 = CARTESIAN_POINT ( 'NONE',  ( 5.167242596723413683, -0.5858957144197572964, -1.632003580468445847 ) ) ;
#172716 = CARTESIAN_POINT ( 'NONE',  ( 1.752831059180045115, 0.6944836804415283060, 2.094827981560241970 ) ) ;
#172717 = CARTESIAN_POINT ( 'NONE',  ( 5.934065736658769019, 1.288437188380668452, 1.747434731901863936 ) ) ;
#172718 = CARTESIAN_POINT ( 'NONE',  ( 0.000000000000000000, 6.999999999999999112, 0.000000000000000000 ) ) ;
#172719 = CARTESIAN_POINT ( 'NONE',  ( 0.3744018202470792978, -2.102136181054746089, -0.2526282858289953248 ) ) ;
#172720 = CARTESIAN_POINT ( 'NONE',  ( 2.687500000000001332, -1.451031289061010421, 1.451031289061227136 ) ) ;
#172721 = CARTESIAN_POINT ( 'NONE',  ( 6.727182134110199385, 1.257034414284210921, 2.204727292504021108 ) ) ;
#172722 = CARTESIAN_POINT ( 'NONE',  ( 4.471652382922743030, 1.868735325311605688, -0.4673391499005700722 ) ) ;
#172723 = CARTESIAN_POINT ( 'NONE',  ( 1.418920233055203761, -0.8037200727962053870, -2.070967414838392084 ) ) ;
#172724 = EDGE_LOOP ( 'NONE', ( #146478, #209139 ) ) ;
#172725 = CARTESIAN_POINT ( 'NONE',  ( -1.499999999999997780, 4.150000000000021672, 1.214306433183764966E-14 ) ) ;
#172726 = CARTESIAN_POINT ( 'NONE',  ( 3.499976210622149253, 7.235056012367825140, 0.7998128361456321445 ) ) ;
#172727 = CARTESIAN_POINT ( 'NONE',  ( 5.472687561410540802, 9.536552588287639409, 0.7998128361456462443 ) ) ;
#172728 = CARTESIAN_POINT ( 'NONE',  ( 3.686370400671713732, 1.234840205895268328, 1.846255301073204791 ) ) ;
#172729 = CARTESIAN_POINT ( 'NONE',  ( -8.432808358020034589, 10.86136238915529084, 1.443375672974064550 ) ) ;
#172731 = SURFACE_STYLE_FILL_AREA ( #86132 ) ;
#172730 = MECHANICAL_DESIGN_GEOMETRIC_PRESENTATION_REPRESENTATION (  '', ( #186480 ), #200371 ) ;
#172732 = CARTESIAN_POINT ( 'NONE',  ( 5.151735183512854199, 8.954182114166247430, -0.7216878364870257245 ) ) ;
#172733 = EDGE_CURVE ( 'NONE', #188147, #151327, #94971, .T. ) ;
#172734 = CARTESIAN_POINT ( 'NONE',  ( -8.961576348508652146, 10.51788916375733685, -1.082531754730543083 ) ) ;
#172735 = CARTESIAN_POINT ( 'NONE',  ( 7.214347136247488912, 7.589362211809770997, -0.7216878364870317197 ) ) ;
#172736 = CARTESIAN_POINT ( 'NONE',  ( 2.039685609654022347, -1.556907966322677472, 1.281362143053674130 ) ) ;
#172738 = CARTESIAN_POINT ( 'NONE',  ( 0.2860855845884663351, -1.266418373674676134, -1.628825195542679793 ) ) ;
#172737 = CARTESIAN_POINT ( 'NONE',  ( 7.344766530301147789, 9.591980256816594164, 1.599625672291281386 ) ) ;
#172739 = CARTESIAN_POINT ( 'NONE',  ( -0.07933194154489606187, -9.900000000000005684, -9.499668754385620417 ) ) ;
#172740 = CARTESIAN_POINT ( 'NONE',  ( 6.156811153937166381, 10.19704708965311468, 0.000000000000000000 ) ) ;
#172741 = CARTESIAN_POINT ( 'NONE',  ( 0.2570343420702363435, 1.821350608449383124, -0.2692129421619017804 ) ) ;
#172742 = SURFACE_SIDE_STYLE ('',( #175946 ) ) ;
#172743 = CARTESIAN_POINT ( 'NONE',  ( -1.364683531250012516, 1.780208333674757615, 0.7879004041258379498 ) ) ;
#172745 = CARTESIAN_POINT ( 'NONE',  ( 1.387592303909779279, -0.8018289002829273038, 1.577768680615166952 ) ) ;
#172744 = B_SPLINE_CURVE_WITH_KNOTS ( 'NONE', 3,
 ( #152951, #68475, #120529, #104211, #21843, #87951 ),
 .UNSPECIFIED., .F., .F.,
 ( 4, 2, 4 ),
 ( 0.001279092382393100377, 0.001599469101539997178, 0.001919845820686893979 ),
 .UNSPECIFIED. ) ;
#172746 = CARTESIAN_POINT ( 'NONE',  ( -0.03452862918938356951, -1.956592590566148093, -0.4871966601913205186 ) ) ;
#172747 = CARTESIAN_POINT ( 'NONE',  ( 0.3976880421775743635, -0.6195963491163231085, -1.733980255833282191 ) ) ;
#172748 = CARTESIAN_POINT ( 'NONE',  ( 3.948992478018618080, -1.906111675684089901, -1.273188117731700597 ) ) ;
#172749 = CARTESIAN_POINT ( 'NONE',  ( 2.009460956091331685, -0.8672641894471898594, -1.624084198382821587 ) ) ;
#172750 = CARTESIAN_POINT ( 'NONE',  ( 8.374132434735052755, 12.92157160716627295, -0.7998128361456352531 ) ) ;
#172751 = CARTESIAN_POINT ( 'NONE',  ( 0.000000000000000000, 3.999999999999996447, 0.000000000000000000 ) ) ;
#172752 = CARTESIAN_POINT ( 'NONE',  ( 3.451995160207482538, 1.825762228170943136, 0.001041782061617091849 ) ) ;
#172753 = CARTESIAN_POINT ( 'NONE',  ( 3.586564705785996843, -0.5826563296015655480, 1.930417576838711957 ) ) ;
#172754 = CARTESIAN_POINT ( 'NONE',  ( -9.480175724453545172, 12.08329098332774265, 1.599625672291281386 ) ) ;
#172756 = CARTESIAN_POINT ( 'NONE',  ( -1.115562610750309283E-14, 11.09375000068279427, 1.500000000000001554 ) ) ;
#172755 = CARTESIAN_POINT ( 'NONE',  ( 3.309705378935084763, -0.4432241279512488807, 2.218521802316391511 ) ) ;
#172757 = CARTESIAN_POINT ( 'NONE',  ( 5.667048493276758414, -1.902512422570214357, -0.9033719842039839021 ) ) ;
#172758 = CARTESIAN_POINT ( 'NONE',  ( 7.449721630645223414, 15.00158243878686726, 10.26201403118819044 ) ) ;
#172759 = CARTESIAN_POINT ( 'NONE',  ( 1.979048004138800998, 1.930994533390210544, 0.7472069620131777112 ) ) ;
#172760 = CARTESIAN_POINT ( 'NONE',  ( 3.948449050077836642, 5.629609863222681199, 1.599625672291267398 ) ) ;
#172761 = CARTESIAN_POINT ( 'NONE',  ( 0.6801582343749917881, 1.005208333674747934, 1.178068619123807004 ) ) ;
#172762 = CARTESIAN_POINT ( 'NONE',  ( 5.778019675193696969, 2.089136139637823852, -0.3624112956793351659 ) ) ;
#172763 = ITEM_DEFINED_TRANSFORMATION ( 'NONE', 'NONE', #103962,  #200407 ) ;
#172765 = CARTESIAN_POINT ( 'NONE',  ( 0.8207749864527034145, 1.779613767027238502, 0.7382806748287008558 ) ) ;
#172764 = CARTESIAN_POINT ( 'NONE',  ( -8.666686507633592385, 11.13422023037111330, 1.599625672291269396 ) ) ;
#172766 = B_SPLINE_CURVE_WITH_KNOTS ( 'NONE', 3,
 ( #148777, #208174, #89130, #5685, #121698, #137878, #156260 ),
 .UNSPECIFIED., .F., .F.,
 ( 4, 3, 4 ),
 ( 0.0001135037246156244756, 0.0006171834326598004457, 0.002007692286214975488 ),
 .UNSPECIFIED. ) ;
#172767 = CARTESIAN_POINT ( 'NONE',  ( -3.654804927335652209, 6.421633627603656080, 1.199719254218452935 ) ) ;
#172768 = CARTESIAN_POINT ( 'NONE',  ( 7.397945374551106568, 11.78268670361832093, -0.7998128361456291469 ) ) ;
#172769 = CARTESIAN_POINT ( 'NONE',  ( 5.102592784488711786, 6.504070869828495027, 1.211835919174956366 ) ) ;
#172770 = CARTESIAN_POINT ( 'NONE',  ( 1.217526595471194906, 2.800000000000017586, -0.8761443883974120439 ) ) ;
#172771 = CARTESIAN_POINT ( 'NONE',  ( -3.093231602212184850, 6.760520635889515795, -0.7998128361456281477 ) ) ;
#172772 = CARTESIAN_POINT ( 'NONE',  ( 0.8268048150999330881, -1.005496690709275720, -1.980927387359689318 ) ) ;
#172773 = CARTESIAN_POINT ( 'NONE',  ( 2.116374960856721277, -0.9918371849380368532, -1.857756019195427877 ) ) ;
#172774 = CARTESIAN_POINT ( 'NONE',  ( -3.481411583659053566, 7.283673624236017830, 0.000000000000000000 ) ) ;
#172775 = CARTESIAN_POINT ( 'NONE',  ( 8.535021395002688749, 9.916278701380017324, 1.199719254218462483 ) ) ;
#172776 = CARTESIAN_POINT ( 'NONE',  ( 6.860206125033806224, -1.860540838789390694, 0.04523802485481390190 ) ) ;
#172777 = CARTESIAN_POINT ( 'NONE',  ( 6.414979237560321401, 10.63589287712906462, 1.040834085586084257E-14 ) ) ;
#172778 = SURFACE_STYLE_FILL_AREA ( #108902 ) ;
#172779 = CARTESIAN_POINT ( 'NONE',  ( -6.129694847154211423, 9.205042184104968328, -1.082531754730549967 ) ) ;
#172780 = CARTESIAN_POINT ( 'NONE',  ( -9.192064960385334160, 9.826423329978791088, 0.7216878364870438212 ) ) ;
#172782 = CARTESIAN_POINT ( 'NONE',  ( 0.07077104593807002908, 0.8175350930016941353, 1.956879683024402183 ) ) ;
#172781 = TOROIDAL_SURFACE ( 'NONE', #117479, -0.1799999999926198968, 0.5000000000000013323 ) ;
#172783 = CARTESIAN_POINT ( 'NONE',  ( -7.075376061485238566, 9.347967719856493218, 1.599625672291269396 ) ) ;
#172785 = CARTESIAN_POINT ( 'NONE',  ( 3.209375601822930690, -1.602329130913646926, -1.131729396966949963 ) ) ;
#172784 = CARTESIAN_POINT ( 'NONE',  ( -1.225000000000022293, -0.5208333333333224902, -0.7072540797573136917 ) ) ;
#172786 = CARTESIAN_POINT ( 'NONE',  ( 2.184651956524386041, -2.119909832212972578, -0.4221607449544013679 ) ) ;
#172787 = CARTESIAN_POINT ( 'NONE',  ( 3.309780021317248355, -1.205041885261768808, -1.616693488061982098 ) ) ;
#172789 = CARTESIAN_POINT ( 'NONE',  ( -4.837732268475038566, 6.745175811576873848, -1.249133900884531467 ) ) ;
#172788 = CARTESIAN_POINT ( 'NONE',  ( -3.447516199624892419, 7.244129009529488350, 0.7998128361456352531 ) ) ;
#172790 = CARTESIAN_POINT ( 'NONE',  ( -1.201851678989727383E-14, 1.321875000341419248, 1.575800808251672791 ) ) ;
#172791 = CARTESIAN_POINT ( 'NONE',  ( 3.732115773437282513, 0.2573812008909857618, 1.721053547986243215 ) ) ;
#172792 = CARTESIAN_POINT ( 'NONE',  ( 5.504247177468168495, 9.365446107114122398, 0.7216878364870438212 ) ) ;
#172793 = CARTESIAN_POINT ( 'NONE',  ( -10.87631885467295945, 5.775928357311673089, -6.414435785039473537 ) ) ;
#172794 = CARTESIAN_POINT ( 'NONE',  ( 1.006953172832128152, 1.636353683469338183, -1.412668763314451903 ) ) ;
#172795 = EDGE_CURVE ( 'NONE', #156928, #60352, #15533, .T. ) ;
#172796 = CARTESIAN_POINT ( 'NONE',  ( 2.565779641467882399, 1.620934753846922982, -1.198676126143098486 ) ) ;
#172797 = CARTESIAN_POINT ( 'NONE',  ( -11.01135777277262129, 12.69999999999999929, -1.400000000000001910 ) ) ;
#172798 = CARTESIAN_POINT ( 'NONE',  ( 0.5148121308554790554, 1.489681748880047563, -1.566682057046255849 ) ) ;
#172799 = CARTESIAN_POINT ( 'NONE',  ( 2.149238863156129220, -1.582378584423797419, -1.175707468242733977 ) ) ;
#172802 = ORIENTED_EDGE ( 'NONE', *, *, #95954, .T. ) ;
#172801 = CARTESIAN_POINT ( 'NONE',  ( -6.129694847154231852, 6.323934541200937787, -0.7216878364870338292 ) ) ;
#172800 = CARTESIAN_POINT ( 'NONE',  ( 11.00592705432737972, 11.11019307346892759, 1.444010445236424856 ) ) ;
#172803 = CARTESIAN_POINT ( 'NONE',  ( -5.112833325684908559, 8.018703742390766109, -1.082531754730549967 ) ) ;
#172804 = CARTESIAN_POINT ( 'NONE',  ( 6.875920180786008196, 8.050936961452347163, -1.199719254218452047 ) ) ;
#172805 = CARTESIAN_POINT ( 'NONE',  ( -5.981082042284069367, 7.006959133200059142, 1.199719254218452935 ) ) ;
#172806 = CARTESIAN_POINT ( 'NONE',  ( 2.156904581142269350, 0.4447176379400120672, 1.969927323211942083 ) ) ;
#172807 = LINE ( 'NONE', #191156, #48996 ) ;
#172808 = CARTESIAN_POINT ( 'NONE',  ( 5.860475213782774695, 0.9281710514958280145, 2.112872520220021144 ) ) ;
#172809 = CARTESIAN_POINT ( 'NONE',  ( -15.75000000000000000, 9.799999999999998934, -1.800000000000001155 ) ) ;
#172810 = CARTESIAN_POINT ( 'NONE',  ( 2.623818369222921554, 1.924856029493416276, -0.3778354045670463401 ) ) ;
#172811 = CARTESIAN_POINT ( 'NONE',  ( 9.368847842243145152, 10.88907622316056312, 1.199719254218453823 ) ) ;
#172812 = CARTESIAN_POINT ( 'NONE',  ( 0.3521856818783953846, 0.1948384997633167970, -2.006960225185448810 ) ) ;
#172813 = ORIENTED_EDGE ( 'NONE', *, *, #51382, .T. ) ;
#172814 = CARTESIAN_POINT ( 'NONE',  ( 2.747379667311528273, 0.3059357446031922834, -2.094990568135519649 ) ) ;
#172816 = CARTESIAN_POINT ( 'NONE',  ( -6.449928391799210736, 8.548002428564306143, -1.599625672291263179 ) ) ;
#172815 = CARTESIAN_POINT ( 'NONE',  ( -2.839543107058306592, 5.400218493954923815, -1.199719254218446718 ) ) ;
#172817 = CARTESIAN_POINT ( 'NONE',  ( 2.202840038917678545, -0.4038221959529255112, 1.796142596185656526 ) ) ;
#172818 = ORIENTED_EDGE ( 'NONE', *, *, #87041, .T. ) ;
#172819 = CARTESIAN_POINT ( 'NONE',  ( -8.123306592882240551, 12.62894145833798376, 0.000000000000000000 ) ) ;
#172820 = CARTESIAN_POINT ( 'NONE',  ( 2.795860172527830922, 2.967839529530313936, 2.452799336324935631 ) ) ;
#172821 = CARTESIAN_POINT ( 'NONE',  ( 4.359710196644346780, -1.641147893522959089, -1.343014508298406628 ) ) ;
#172822 = CARTESIAN_POINT ( 'NONE',  ( 0.1461044202776436429, -1.480667811789614596, 1.094048858351577724 ) ) ;
#172823 = CARTESIAN_POINT ( 'NONE',  ( 0.7499999999999902300, 5.097916667349482012, -1.299038105676658228 ) ) ;
#172824 = CARTESIAN_POINT ( 'NONE',  ( 7.130698725783555680, 10.40656671580112658, 1.199719254218460707 ) ) ;
#172825 = CARTESIAN_POINT ( 'NONE',  ( -0.6125000000000262457, 2.604166667349451458, 1.060881119635917136 ) ) ;
#172826 = CARTESIAN_POINT ( 'NONE',  ( 4.587218493272061437, 1.842632243969796413, -0.9228815313185294578 ) ) ;
#172827 =( GEOMETRIC_REPRESENTATION_CONTEXT ( 3 ) GLOBAL_UNCERTAINTY_ASSIGNED_CONTEXT ( ( #133888 ) ) GLOBAL_UNIT_ASSIGNED_CONTEXT ( ( #81990, #128706, #31134 ) ) REPRESENTATION_CONTEXT ( 'NONE', 'WORKASPACE' ) );
#172829 = CARTESIAN_POINT ( 'NONE',  ( 1.856743374925871715, 0.3135980649527739250, -1.814175028193690808 ) ) ;
#172828 = CARTESIAN_POINT ( 'NONE',  ( -6.364663046611467756, 9.512858423433634414, 1.199719254218452047 ) ) ;
#172830 = CARTESIAN_POINT ( 'NONE',  ( 0.6823417656249917140, 5.342708333674749177, 1.181850606188765695 ) ) ;
#172831 = CARTESIAN_POINT ( 'NONE',  ( -1.608462485350631077, 8.735270501766754236, 2.463594439587651230 ) ) ;
#172832 = CARTESIAN_POINT ( 'NONE',  ( 2.877399083922144385, 6.438195321532787396, -0.3536239397737388490 ) ) ;
#172833 = B_SPLINE_CURVE_WITH_KNOTS ( 'NONE', 3,
 ( #150777, #54331, #35930, #199484, #51130, #117252 ),
 .UNSPECIFIED., .F., .F.,
 ( 4, 2, 4 ),
 ( 0.001490700410107413275, 0.002078801942328931812, 0.002666903474550450567 ),
 .UNSPECIFIED. ) ;
#172834 = CARTESIAN_POINT ( 'NONE',  ( 1.454063653991678473, 0.6380318336138122159, -2.112638918738508398 ) ) ;
#172835 = CARTESIAN_POINT ( 'NONE',  ( 3.374574379025939486, -1.350666858538966064, 1.814832908163630742 ) ) ;
#172836 = CARTESIAN_POINT ( 'NONE',  ( -6.887178846062105286, 10.97886638714038554, -0.7216878364870267237 ) ) ;
#172837 = CARTESIAN_POINT ( 'NONE',  ( 3.427799431637909233, -1.783865866189004556, 0.3147462633073249139 ) ) ;
#172838 = ADVANCED_FACE ( 'NONE', ( #81617 ), #113127, .F. ) ;
#172839 = CARTESIAN_POINT ( 'NONE',  ( 3.485460621946351534, -0.5511008185722067187, 1.834767741543178676 ) ) ;
#172840 = CARTESIAN_POINT ( 'NONE',  ( 3.895033709675084221, 0.3008086390649654662, 2.048262060622765279 ) ) ;
#172841 = CARTESIAN_POINT ( 'NONE',  ( -1.364683531250012516, 3.592708333674750509, 0.7879004041258379498 ) ) ;
#172842 = CARTESIAN_POINT ( 'NONE',  ( 3.116049734078304212, -0.9705229388551097625, -1.715950581178276479 ) ) ;
#172843 = CARTESIAN_POINT ( 'NONE',  ( 1.412975430660408538, 1.697568229685364249, 0.9106500277177332903 ) ) ;
#172844 = CARTESIAN_POINT ( 'NONE',  ( 3.959713429720784106, 1.856571849420919795, -0.2284545790810637578 ) ) ;
#172845 = VECTOR ( 'NONE', #13021, 1000.000000000000227 ) ;
#172846 = CARTESIAN_POINT ( 'NONE',  ( 2.579137097422959712, -2.208767019342866345, -0.6684429575241066512 ) ) ;
#172847 = CARTESIAN_POINT ( 'NONE',  ( 3.314761293198214887, -1.410806105172614178, 1.213857476866337937 ) ) ;
#172848 = CARTESIAN_POINT ( 'NONE',  ( -1.364683531250012516, 3.988541667008088876, -0.7879004041258300672 ) ) ;
#172849 = CARTESIAN_POINT ( 'NONE',  ( -5.922214171070950606, 5.803671375871217286, -0.7998128361456291469 ) ) ;
#172850 = CARTESIAN_POINT ( 'NONE',  ( 6.972971076130050072, 7.029554431773520129, 1.040834085586084257E-14 ) ) ;
#172851 = CARTESIAN_POINT ( 'NONE',  ( 4.000000000000012434, 0.000000000000000000, 0.7500000000000006661 ) ) ;
#172852 = CARTESIAN_POINT ( 'NONE',  ( 0.4519647057620000408, 0.6586765168765180700, -2.000488393216502292 ) ) ;
#172853 = B_SPLINE_CURVE_WITH_KNOTS ( 'NONE', 3,
 ( #132064, #84333, #164522, #198075 ),
 .UNSPECIFIED., .F., .F.,
 ( 4, 4 ),
 ( 3.900039219166819614E-15, 0.0006467211803968906259 ),
 .UNSPECIFIED. ) ;
#172854 = CARTESIAN_POINT ( 'NONE',  ( 3.511198595814926993, 6.079853547550633230, 1.082531754730558626 ) ) ;
#172856 = DIRECTION ( 'NONE',  ( -0.9998476951563912696, -0.000000000000000000, 0.01745240643728004568 ) ) ;
#172855 = CARTESIAN_POINT ( 'NONE',  ( 1.364683531249992088, 5.696875000341418804, 1.214306433183764966E-14 ) ) ;
#172857 = CARTESIAN_POINT ( 'NONE',  ( 6.819591527820957566, -2.098570527662356522, 0.5178885164088961046 ) ) ;
#172858 = CARTESIAN_POINT ( 'NONE',  ( 2.391022662813433453, -2.030629854096975606, -0.6112283555373964061 ) ) ;
#172859 = CARTESIAN_POINT ( 'NONE',  ( 5.558836782162523527, 7.518240855878357110, -1.384758111419038817 ) ) ;
#172860 = CARTESIAN_POINT ( 'NONE',  ( 1.142838682686732277, 1.947676595115959586, 0.5347052314127549444 ) ) ;
#172861 = CARTESIAN_POINT ( 'NONE',  ( -0.6823417656250003738, 0.7177083336747519526, -1.181850606188749264 ) ) ;
#172862 = CARTESIAN_POINT ( 'NONE',  ( -3.958617665510279160, 5.641473247893851628, -1.443375672974053447 ) ) ;
#172863 = CARTESIAN_POINT ( 'NONE',  ( 4.798696304233017074, 7.685897223992134819, -1.199719254218452047 ) ) ;
#172864 = EDGE_CURVE ( 'NONE', #148633, #190246, #26172, .T. ) ;
#172865 = CARTESIAN_POINT ( 'NONE',  ( 1.282749207608822495, -2.108609127331688260, -0.4749100009155197699 ) ) ;
#172868 = CARTESIAN_POINT ( 'NONE',  ( 3.633221978782282147, 5.261844946711204507, -1.443375672974057666 ) ) ;
#172867 = CARTESIAN_POINT ( 'NONE',  ( 6.825078400183573812, 7.629137130509070275, 2.455651831298297338 ) ) ;
#172866 = CARTESIAN_POINT ( 'NONE',  ( 4.389807875774629942, 8.343469298370917997, 0.7998128361456271485 ) ) ;
#172869 = DIRECTION ( 'NONE',  ( 1.000000000000000000, 0.000000000000000000, 0.000000000000000000 ) ) ;
#172870 = CARTESIAN_POINT ( 'NONE',  ( 5.700407750362016301, 1.350738941191354625, -1.497498989668680114 ) ) ;
#172871 = CARTESIAN_POINT ( 'NONE',  ( -7.863365906246054138, 11.15738207638699464, -1.082531754730543971 ) ) ;
#172872 = CARTESIAN_POINT ( 'NONE',  ( -0.1114211809780316365, -0.4883405756051837354, -2.144353428667714390 ) ) ;
#172873 = CARTESIAN_POINT ( 'NONE',  ( -9.333041836230696831, 14.55305236563169302, -7.472413793098840351 ) ) ;
#172875 = CARTESIAN_POINT ( 'NONE',  ( -1.402160292154681736E-14, 10.67187500034139624, 1.575800808251682339 ) ) ;
#172874 = CARTESIAN_POINT ( 'NONE',  ( 6.614160618316515361, -1.014195557614630205, -1.909021090911746654 ) ) ;
#172876 = CARTESIAN_POINT ( 'NONE',  ( -9.134442807305063639, 11.67993591332117376, 1.599625672291281386 ) ) ;
#172878 = CARTESIAN_POINT ( 'NONE',  ( 0.6146668332816725977, 0.1418531279011990553, 1.910429497406636479 ) ) ;
#172877 = CARTESIAN_POINT ( 'NONE',  ( -6.249945625775490399, 7.354319987235250267, 1.082531754730549967 ) ) ;
#172879 = CARTESIAN_POINT ( 'NONE',  ( -1.364683531250014514, 1.051041667008090208, -0.7879004041258289570 ) ) ;
#172880 = CARTESIAN_POINT ( 'NONE',  ( 1.224999999999974332, 2.687500000682768508, -4.163336342344337027E-14 ) ) ;
#172881 = CARTESIAN_POINT ( 'NONE',  ( 2.490480453433571384, -0.2941264275767330183, -1.699438164531028583 ) ) ;
#172882 = CARTESIAN_POINT ( 'NONE',  ( 3.867818961648523235, 7.734482231890414283, 1.040834085586084257E-14 ) ) ;
#172883 = CARTESIAN_POINT ( 'NONE',  ( 0.4207181242068900873, -0.09552205520973154618, 1.767312625620009126 ) ) ;
#172884 = CARTESIAN_POINT ( 'NONE',  ( 1.524088986950965730, -1.997618534301074833, 0.2487294023021668354 ) ) ;
#172885 = CARTESIAN_POINT ( 'NONE',  ( 9.096228393767193054, 0.9691415390508323346, 7.669416753559205269 ) ) ;
#172886 = CARTESIAN_POINT ( 'NONE',  ( 4.296070028909639404, -0.8476096858263427736, 2.037697185916572007 ) ) ;
#172887 = EDGE_LOOP ( 'NONE', ( #54485, #212918, #37094, #122784 ) ) ;
#172888 = CARTESIAN_POINT ( 'NONE',  ( 8.907343734053986495, 9.494248565925552441, -0.7216878364870197293 ) ) ;
#172889 = CARTESIAN_POINT ( 'NONE',  ( -6.454563648557663846, 9.688018802362710957, -1.199719254218452047 ) ) ;
#172891 = CARTESIAN_POINT ( 'NONE',  ( 4.517203946846011675, -1.842441744247227842, 0.8197884948388590720 ) ) ;
#172890 = CARTESIAN_POINT ( 'NONE',  ( 3.879626234357834047, 0.2581020070546445888, -2.104639248629774251 ) ) ;
#172893 = ORIENTED_EDGE ( 'NONE', *, *, #200959, .T. ) ;
#172892 = CARTESIAN_POINT ( 'NONE',  ( 2.935611553675514518, -1.744650271585326484, 0.4875094811955403284 ) ) ;
#172894 = CARTESIAN_POINT ( 'NONE',  ( 4.389807875774629942, 8.343469298370917997, 0.7998128361456271485 ) ) ;
#172895 = VERTEX_POINT ( 'NONE', #2467 ) ;
#172896 = AXIS2_PLACEMENT_3D ( 'NONE', #18896, #51429, #197660 ) ;
#172897 = CARTESIAN_POINT ( 'NONE',  ( 1.217418975555501826, -1.825842229346545498, 0.4062821374252246764 ) ) ;
#172898 = CARTESIAN_POINT ( 'NONE',  ( 6.410779360540267646, 1.349177972556347971, -1.230185023894624141 ) ) ;
#172899 = CARTESIAN_POINT ( 'NONE',  ( -4.464712657601869417, 4.103252943490596216, 0.7998128361456341429 ) ) ;
#172900 = DIRECTION ( 'NONE',  ( 1.000000000000000000, 0.000000000000000000, 0.000000000000000000 ) ) ;
#172901 = CARTESIAN_POINT ( 'NONE',  ( -1.500000000000015099, 8.510416667349460340, -0.8660254037844309360 ) ) ;
#172902 = ADVANCED_FACE ( 'NONE', ( #1405 ), #17660, .F. ) ;
#172903 = CARTESIAN_POINT ( 'NONE',  ( -1.201851678989727383E-14, 2.134375000341423689, 1.575800808251672791 ) ) ;
#172904 = DIRECTION ( 'NONE',  ( 0.000000000000000000, 0.000000000000000000, 1.000000000000000000 ) ) ;
#172905 = CARTESIAN_POINT ( 'NONE',  ( 5.397554552016204710, 9.311247720745345902, 0.7216878364870317197 ) ) ;
#172906 = EDGE_CURVE ( 'NONE', #206352, #40383, #20857, .T. ) ;
#172907 = CARTESIAN_POINT ( 'NONE',  ( -3.350273356352693188, 6.922752992471175482, 0.000000000000000000 ) ) ;
#172908 = CARTESIAN_POINT ( 'NONE',  ( -6.123442655227560927, 7.173046514967467147, 1.199719254218452047 ) ) ;
#172909 = CARTESIAN_POINT ( 'NONE',  ( 4.289387122732970958, -0.003046686910593982868, -2.120778211268215419 ) ) ;
#172911 = CARTESIAN_POINT ( 'NONE',  ( -10.87631885467295945, 5.775928357311673089, -6.414435785039473537 ) ) ;
#172910 = CARTESIAN_POINT ( 'NONE',  ( -0.02948999725178609935, 2.037268340021273882, -2.343334633859140315 ) ) ;
#172912 = CARTESIAN_POINT ( 'NONE',  ( 6.081318999601531772, 1.822420489394786625, -0.7521447986948930353 ) ) ;
#172913 = CARTESIAN_POINT ( 'NONE',  ( -0.6823417656250003738, 0.9677083336747521747, -1.181850606188749264 ) ) ;
#172914 = CARTESIAN_POINT ( 'NONE',  ( 6.539320575229249144, 0.007148032025052972194, 1.896977914940492393 ) ) ;
#172915 = ORIENTED_EDGE ( 'NONE', *, *, #136835, .T. ) ;
#172916 = CARTESIAN_POINT ( 'NONE',  ( 0.2810647479330531939, 1.757583132164267647, -1.180221762011339326 ) ) ;
#172917 = CARTESIAN_POINT ( 'NONE',  ( 8.730775170176714894, 13.51259826081505899, 8.232739887797778877 ) ) ;
#172918 = CARTESIAN_POINT ( 'NONE',  ( 1.926316106172959230, 1.062450747350886848, 1.776810178100460824 ) ) ;
#172919 = CARTESIAN_POINT ( 'NONE',  ( 7.205232291019763480, 7.370802192470005565, -0.7998128361456341429 ) ) ;
#172920 = CARTESIAN_POINT ( 'NONE',  ( 4.746236293235721604, 7.694970221153795364, 1.199719254218451159 ) ) ;
#172921 = CARTESIAN_POINT ( 'NONE',  ( 4.929271367020211514, 7.908511140569038922, 1.199719254218452047 ) ) ;
#172923 = CARTESIAN_POINT ( 'NONE',  ( 6.491656622844908853, 6.468020902940851968, 0.7998128361456341429 ) ) ;
#172922 = CARTESIAN_POINT ( 'NONE',  ( 3.890639641997388765, 1.766133395052928101, -1.118410975085604608 ) ) ;
#172924 = CARTESIAN_POINT ( 'NONE',  ( 7.876360894896227371, 8.153785563659219804, -0.7998128361456341429 ) ) ;
#172927 = ORIENTED_EDGE ( 'NONE', *, *, #46133, .T. ) ;
#172926 = CARTESIAN_POINT ( 'NONE',  ( 1.787489318380721448, 1.733277665728020001, -0.5263807565755849183 ) ) ;
#172925 = CARTESIAN_POINT ( 'NONE',  ( 2.256629077056008015, -1.412982602626071671, 1.155960151518524937 ) ) ;
#172928 = CARTESIAN_POINT ( 'NONE',  ( 5.461621781982892720, 0.4335984126433762853, -2.163701019753036192 ) ) ;
#172929 =( NAMED_UNIT ( * ) SI_UNIT ( $, .STERADIAN. ) SOLID_ANGLE_UNIT ( ) );
#172930 = CARTESIAN_POINT ( 'NONE',  ( 4.665167916288286420, -1.969490514480085164, -0.9956290437203789701 ) ) ;
#172931 = CARTESIAN_POINT ( 'NONE',  ( 8.281332899848809603, 8.555976559445431562, 0.7998128361456481317 ) ) ;
#172932 = CARTESIAN_POINT ( 'NONE',  ( -11.86239285000045918, 12.29999999999997939, 1.812080536912751283 ) ) ;
#172933 = ADVANCED_FACE ( 'NONE', ( #132547 ), #30178, .T. ) ;
#172934 = CARTESIAN_POINT ( 'NONE',  ( 3.264218543254516103, 1.912461472423478970, -0.002497826895729581952 ) ) ;
#172935 = CARTESIAN_POINT ( 'NONE',  ( 8.289920859751990889, 11.75899253876431416, 1.199719254218450271 ) ) ;
#172936 = CARTESIAN_POINT ( 'NONE',  ( 4.914543119725925280, 0.7892175071393169317, 1.914236960262293508 ) ) ;
#172938 = CARTESIAN_POINT ( 'NONE',  ( -1.545144449789736862, 8.695096949162934408, -2.507961912884401734 ) ) ;
#172937 = CARTESIAN_POINT ( 'NONE',  ( -3.035736007439495232, 6.452393136558649545, 0.6403810252995913999 ) ) ;
#172939 = CARTESIAN_POINT ( 'NONE',  ( 5.618738332679400038, -0.05485954975367920983, 2.191026952110195491 ) ) ;
#172940 = ORIENTED_EDGE ( 'NONE', *, *, #148514, .T. ) ;
#172941 = ORIENTED_EDGE ( 'NONE', *, *, #185371, .F. ) ;
#172942 = CARTESIAN_POINT ( 'NONE',  ( -0.3175553531547188890, 3.956598013261175772, 11.53924059509144051 ) ) ;
#172943 = CARTESIAN_POINT ( 'NONE',  ( 4.573896719763862251, 6.429575154514868274, -1.599625672291273171 ) ) ;
#172944 = CARTESIAN_POINT ( 'NONE',  ( -1.642778471874998480, -1.538541666188709245, 2.845375778867863303 ) ) ;
#172945 =( NAMED_UNIT ( * ) SI_UNIT ( $, .STERADIAN. ) SOLID_ANGLE_UNIT ( ) );
#172946 = CARTESIAN_POINT ( 'NONE',  ( -7.022760382198764084, 11.13704484596649635, 0.7216878364870458196 ) ) ;
#172947 = CARTESIAN_POINT ( 'NONE',  ( 5.246079093845007257, 5.085123462432798114, 0.7998128361456352531 ) ) ;
#172948 = CARTESIAN_POINT ( 'NONE',  ( 5.313363446356571984, -1.745981802610725442, -1.112170280247841703 ) ) ;
#172949 = CARTESIAN_POINT ( 'NONE',  ( 4.354074215503287881, 1.926045596674738514, -0.04874250487575670227 ) ) ;
#172950 = CARTESIAN_POINT ( 'NONE',  ( 6.603150282362637569, -0.1459358296138096867, 2.084196934165093662 ) ) ;
#172951 =( BOUNDED_CURVE ( )  B_SPLINE_CURVE ( 2, ( #25053, #59688, #42409, #125851, #72735 ),
 .UNSPECIFIED., .F., .T. ) 
 B_SPLINE_CURVE_WITH_KNOTS ( ( 3, 2, 3 ),
 ( 0.9910714285714286031, 0.9940476190476190688, 1.000000000000000000 ),
 .UNSPECIFIED. ) 
 CURVE ( )  GEOMETRIC_REPRESENTATION_ITEM ( )  RATIONAL_B_SPLINE_CURVE ( ( 0.9330127018922194093, 0.9330127018922194093, 1.000000000000000000, 0.8660254037844387076, 1.000000000000000000 ) ) 
 REPRESENTATION_ITEM ( '' )  );
#172952 = CARTESIAN_POINT ( 'NONE',  ( 0.000000000000000000, 0.000000000000000000, 0.000000000000000000 ) ) ;
#172953 = CARTESIAN_POINT ( 'NONE',  ( 5.833751235630055376, 10.02806988486892514, 0.7998128361456331437 ) ) ;
#172954 = CARTESIAN_POINT ( 'NONE',  ( 0.7500000000000006661, 13.08333333333333570, 1.299038105676657340 ) ) ;
#172955 = CARTESIAN_POINT ( 'NONE',  ( 0.7795418844130063141, 1.474435645617519164, 1.621430000501473900 ) ) ;
#172956 = CARTESIAN_POINT ( 'NONE',  ( 5.320859459983126705, 1.688362619374352613, 0.6951667914897319278 ) ) ;
#172957 = CARTESIAN_POINT ( 'NONE',  ( 5.560252395380206991, 7.580323442733986283, 1.443375672974065660 ) ) ;
#172958 = CARTESIAN_POINT ( 'NONE',  ( 2.860407222358963608, 5.320596945185329218, 1.082531754730548412 ) ) ;
#172959 = CARTESIAN_POINT ( 'NONE',  ( -6.140917232347002042, 6.129101290685087911, -0.7998128361456362523 ) ) ;
#172960 = CARTESIAN_POINT ( 'NONE',  ( 4.843287188579786573, 6.673587691474970107, -1.599625672291256295 ) ) ;
#172961 = CARTESIAN_POINT ( 'NONE',  ( 3.854260808034858155, 7.718664386007802136, -0.7998128361456362523 ) ) ;
#172962 = ORIENTED_EDGE ( 'NONE', *, *, #11637, .T. ) ;
#172964 = CARTESIAN_POINT ( 'NONE',  ( -0.005209864377695229073, -1.953240142932886725, -0.4869125064202137199 ) ) ;
#172963 = CARTESIAN_POINT ( 'NONE',  ( 2.964219115174483665, -1.702287218311925310, -0.7022057971969236645 ) ) ;
#172965 = CARTESIAN_POINT ( 'NONE',  ( 1.950936211155746447, 1.584691988697755960, 1.664941613344946836 ) ) ;
#172966 = CARTESIAN_POINT ( 'NONE',  ( 6.614115624646348834, 1.956711779489667125, -0.1410536379464824575 ) ) ;
#172967 = CARTESIAN_POINT ( 'NONE',  ( -5.229694566569281555, 7.124396299129368337, 1.599625672291267398 ) ) ;
#172968 = CARTESIAN_POINT ( 'NONE',  ( -4.647415939163805909, 7.189517123537264354, -1.183184842545903948 ) ) ;
#172969 = CARTESIAN_POINT ( 'NONE',  ( -3.810004860640155311, 4.403759411290286252, 1.199719254218462483 ) ) ;
#172970 = FACE_OUTER_BOUND ( 'NONE', #25993, .T. ) ;
#172971 = CARTESIAN_POINT ( 'NONE',  ( -3.984117037569407938, 5.741498858621315371, 1.599625672291270506 ) ) ;
#172973 = CARTESIAN_POINT ( 'NONE',  ( 0.6197280442463182215, -0.9970892369244135356, -1.582582228963416160 ) ) ;
#172972 = CARTESIAN_POINT ( 'NONE',  ( 2.542619699696859303, -1.736688010486141520, 1.163783427146478200 ) ) ;
#172974 = CARTESIAN_POINT ( 'NONE',  ( 2.513045873335068237, 2.015604327017831654, 0.05229110803010171560 ) ) ;
#172975 = CARTESIAN_POINT ( 'NONE',  ( 7.782016984564049444, 11.06247500109133064, 1.082531754730557072 ) ) ;
#172976 = VERTEX_POINT ( 'NONE', #85889 ) ;
#172977 = CARTESIAN_POINT ( 'NONE',  ( -1.364683531249997417, 4.071875000341417028, 1.214306433183764966E-14 ) ) ;
#172978 = CARTESIAN_POINT ( 'NONE',  ( 1.856607919947508956, 0.2971036446917668106, -1.714703581143263156 ) ) ;
#172979 = AXIS2_PLACEMENT_3D ( 'NONE', #151274, #1784, #136091 ) ;
#172980 = CARTESIAN_POINT ( 'NONE',  ( 4.286349120214771879, 8.152491073559232859, -0.7998128361456221525 ) ) ;
#172982 = CARTESIAN_POINT ( 'NONE',  ( -0.1216878429548682999, 3.463015919485879834, -1.996294584693599994 ) ) ;
#172981 = CARTESIAN_POINT ( 'NONE',  ( -7.034482758620708154, 5.227586206896615018, 1.300454001123785972E-14 ) ) ;
#172983 = CARTESIAN_POINT ( 'NONE',  ( 2.402614999361089243, 1.385809671090399986, -1.026769200382530167 ) ) ;
#172984 = CARTESIAN_POINT ( 'NONE',  ( 2.823975127348025804, 1.215230906543849354, -1.823574674616668556 ) ) ;
#172985 = CARTESIAN_POINT ( 'NONE',  ( 4.899154391205060577, 1.836108854712194649, -1.224054507610386366 ) ) ;
#172986 = CARTESIAN_POINT ( 'NONE',  ( -11.23979429089589033, 4.930458577253933328, -5.866063493660276684 ) ) ;
#172987 = CARTESIAN_POINT ( 'NONE',  ( 2.817415258179640336, -1.886890863808653007, -1.073800027038468219 ) ) ;
#172988 = CARTESIAN_POINT ( 'NONE',  ( 0.5393321728033516615, -1.288848960320065462, -1.293324666950084190 ) ) ;
#172989 = CARTESIAN_POINT ( 'NONE',  ( 4.276635374070654194, -0.4674139498860945263, -2.064944810692950217 ) ) ;
#172990 = DIRECTION ( 'NONE',  ( 0.000000000000000000, 0.000000000000000000, 1.000000000000000000 ) ) ;
#172991 = VERTEX_POINT ( 'NONE', #169271 ) ;
#172993 = CARTESIAN_POINT ( 'NONE',  ( -1.364683531250000748, 0.8218750003414210248, 0.000000000000000000 ) ) ;
#172992 = CARTESIAN_POINT ( 'NONE',  ( 4.265347265089792117, 2.223640956194427254, -0.5566138344911036873 ) ) ;
#172994 = CARTESIAN_POINT ( 'NONE',  ( 1.224999999999979217, 2.604166666666692720, 0.7072540797572558491 ) ) ;
#172995 = CARTESIAN_POINT ( 'NONE',  ( 4.813308228051395687, 5.574280006603454574, 1.199719254218462483 ) ) ;
#172996 = CARTESIAN_POINT ( 'NONE',  ( 0.6102159345307588412, -0.7594153588383574238, 1.980023364433493693 ) ) ;
#172997 = CARTESIAN_POINT ( 'NONE',  ( -6.751597309925468693, 6.979211071108916364, 0.7216878364870317197 ) ) ;
#172998 = VECTOR ( 'NONE', #112895, 1000.000000000000000 ) ;
#172999 = CARTESIAN_POINT ( 'NONE',  ( 3.226477370372302644, 5.747678784534228313, 1.082531754730546636 ) ) ;
#173000 = CARTESIAN_POINT ( 'NONE',  ( -6.358410854684789726, 8.441231968597481483, -1.443375672974058777 ) ) ;
#173001 = CARTESIAN_POINT ( 'NONE',  ( 4.475600106286968582, 5.354526557823810151, -1.082531754730548412 ) ) ;
#173002 = ORIENTED_EDGE ( 'NONE', *, *, #65071, .T. ) ;
#173003 = CARTESIAN_POINT ( 'NONE',  ( 5.045546153961558922, -1.458558117013383892, 1.392544180963309230 ) ) ;
#173005 = CARTESIAN_POINT ( 'NONE',  ( 2.957939313049274599, -0.6512127342562739063, 1.957104789517728483 ) ) ;
#173004 = CARTESIAN_POINT ( 'NONE',  ( 5.847644326195776010, 5.716673223516856694, -0.7998128361456281477 ) ) ;
#173007 = CARTESIAN_POINT ( 'NONE',  ( -0.1408020194049781904, -0.005144001661201018025, -2.100147592658160089 ) ) ;
#173006 = CARTESIAN_POINT ( 'NONE',  ( 6.373214726875630731, 9.593111727067046957, 1.199719254218452047 ) ) ;
#173008 = CARTESIAN_POINT ( 'NONE',  ( 4.882344714252594642, 4.868692719482363707, 0.000000000000000000 ) ) ;
#173009 = CARTESIAN_POINT ( 'NONE',  ( 3.285556943750000070, -3.784374999522041705, 0.000000000000000000 ) ) ;
#173010 = DIRECTION ( 'NONE',  ( 0.000000000000000000, 0.000000000000000000, -1.000000000000000000 ) ) ;
#173011 = CARTESIAN_POINT ( 'NONE',  ( 6.421842908546859796, 1.265077015623069512, -1.789241164368003290 ) ) ;
#173012 = CARTESIAN_POINT ( 'NONE',  ( 3.410779880581996437, -1.203353552534730309, -1.617818353255597863 ) ) ;
#173013 = CARTESIAN_POINT ( 'NONE',  ( 3.368544699895597461, 0.04196216268675251326, -1.840931771443871101 ) ) ;
#173014 = CARTESIAN_POINT ( 'NONE',  ( 7.955937213120826357, 8.176348258262782664, 0.7998128361456481317 ) ) ;
#173015 = CARTESIAN_POINT ( 'NONE',  ( 6.598675984083053336, -0.4903212918116289787, -1.758449130657411263 ) ) ;
#173016 = CARTESIAN_POINT ( 'NONE',  ( 0.1593517250534680629, 1.330572521919655360, 1.874314102060254505 ) ) ;
#173017 = CARTESIAN_POINT ( 'NONE',  ( -5.768104287610143821, 8.816873204598778102, -1.199719254218440723 ) ) ;
#173018 = CARTESIAN_POINT ( 'NONE',  ( 6.772354121900423962, -1.399018086243536407, 1.779017302379340748 ) ) ;
#173019 = CARTESIAN_POINT ( 'NONE',  ( 1.717544045074904213, -0.2563126921724939167, 2.090340884163774948 ) ) ;
#173020 = CARTESIAN_POINT ( 'NONE',  ( -4.437261413422502798, 8.398831758960053406, 0.000000000000000000 ) ) ;
#173021 = CARTESIAN_POINT ( 'NONE',  ( 7.995557903757111617, 10.35123685918189729, 1.599625672291281386 ) ) ;
#173022 = CARTESIAN_POINT ( 'NONE',  ( 7.661766205054107992, 8.111351125417501251, -0.7216878364870317197 ) ) ;
#173023 = CARTESIAN_POINT ( 'NONE',  ( 8.378074386687000441, 7.008151349768591665, 15.76159487570644124 ) ) ;
#173024 = CARTESIAN_POINT ( 'NONE',  ( -7.009729113465285266, 8.136771039586342624, -1.199719254218446718 ) ) ;
#173025 = CARTESIAN_POINT ( 'NONE',  ( 5.938108092661121162, 9.871617174839238729, 1.040834085586084257E-14 ) ) ;
#173026 = CARTESIAN_POINT ( 'NONE',  ( 4.012431654125413694, 7.810675627703163038, 0.2615036927465386740 ) ) ;
#173027 = CARTESIAN_POINT ( 'NONE',  ( -5.250031796989778066, 7.148123067953287446, 1.599625672291267398 ) ) ;
#173028 = CARTESIAN_POINT ( 'NONE',  ( 4.096076364168971473, 1.452574950358286765, 1.680725415074139306 ) ) ;
#173029 = CARTESIAN_POINT ( 'NONE',  ( 2.554835828347111093, -1.907293181126702653, -1.079063956894068976 ) ) ;
#173030 = CARTESIAN_POINT ( 'NONE',  ( 0.6103625832605160673, -2.195865045534075133, 0.2202409711149767024 ) ) ;
#173031 = CARTESIAN_POINT ( 'NONE',  ( -4.553559489343377287, 6.405848385690952718, -1.599625672291271394 ) ) ;
#173032 = CARTESIAN_POINT ( 'NONE',  ( 4.176187491914356897, -1.006606191838583131, -1.683785057063936552 ) ) ;
#173033 = CARTESIAN_POINT ( 'NONE',  ( 8.565000355531088516, 11.01558638625153286, -1.599625672291257406 ) ) ;
#173034 = CARTESIAN_POINT ( 'NONE',  ( -3.895595285070177383, 2.800000000000024691, -0.7749999999999944711 ) ) ;
#173035 = CARTESIAN_POINT ( 'NONE',  ( -0.6823417656250003738, 0.9677083336747521747, -1.181850606188749264 ) ) ;
#173036 = CARTESIAN_POINT ( 'NONE',  ( -4.855228407469635243, 4.837057028235559386, 0.7216878364870257245 ) ) ;
#173038 = ORIENTED_EDGE ( 'NONE', *, *, #29437, .F. ) ;
#173037 = CARTESIAN_POINT ( 'NONE',  ( -6.290620087060847965, 7.401773525401500464, 1.082531754730549967 ) ) ;
#173039 = CARTESIAN_POINT ( 'NONE',  ( 3.164422831683691761, 2.120778211551369807, -0.003951117757632071313 ) ) ;
#173040 = CARTESIAN_POINT ( 'NONE',  ( -4.604929450496978660, 5.401447776115099408, -1.199719254218453823 ) ) ;
#173041 = CARTESIAN_POINT ( 'NONE',  ( 5.401312781148373432, 1.764888628567516049, 1.247983453017486699 ) ) ;
#173042 = CARTESIAN_POINT ( 'NONE',  ( 3.421284184235491743, -1.099380227797893905, -1.476844927387373163 ) ) ;
#173043 = CARTESIAN_POINT ( 'NONE',  ( -5.703936002245207249, 6.126809468943200443, 0.7377312291968595170 ) ) ;
#173044 = CARTESIAN_POINT ( 'NONE',  ( 1.364683531249988757, 1.196875000341421469, 0.000000000000000000 ) ) ;
#173045 = CARTESIAN_POINT ( 'NONE',  ( 0.5381063436600447281, -1.494009556959356999, 0.8925505203737462701 ) ) ;
#173047 = EDGE_CURVE ( 'NONE', #168888, #71781, #134549, .T. ) ;
#173046 = CARTESIAN_POINT ( 'NONE',  ( 6.827182134110233669, 2.103728865748891508, 2.021873693915546610 ) ) ;
#173048 = CARTESIAN_POINT ( 'NONE',  ( 2.548569689688999329, 5.917155704705049146, -0.7216878364870267237 ) ) ;
#173049 = CARTESIAN_POINT ( 'NONE',  ( 10.37944572521833742, 9.120024990325399372, 6.075587282785552823 ) ) ;
#173050 = VECTOR ( 'NONE', #164147, 1000.000000000000000 ) ;
#173051 = CARTESIAN_POINT ( 'NONE',  ( 4.680646922328831394, -2.095996545452833981, -0.5284188670612932626 ) ) ;
#173052 = EDGE_CURVE ( 'NONE', #35502, #210699, #54461, .T. ) ;
#173053 = CARTESIAN_POINT ( 'NONE',  ( -4.141125853970233806, 6.918731698685530063, -1.199719254218452047 ) ) ;
#173054 = CARTESIAN_POINT ( 'NONE',  ( 5.149767453795408123, -0.2439937967673235231, -2.001204641050558397 ) ) ;
#173055 = CARTESIAN_POINT ( 'NONE',  ( -8.649738815394339753, 9.193709494155953621, 1.040834085586084257E-14 ) ) ;
#173056 = CARTESIAN_POINT ( 'NONE',  ( 3.239309987758617115, -1.907233169736745060, 1.017530501952010447 ) ) ;
#173057 = CARTESIAN_POINT ( 'NONE',  ( 4.094965523422711584, 1.667053662060855812, -1.051937181705852931 ) ) ;
#173058 = DIRECTION ( 'NONE',  ( -0.000000000000000000, 0.000000000000000000, -1.000000000000000000 ) ) ;
#173059 = CARTESIAN_POINT ( 'NONE',  ( 1.325685429717119446, -0.05423940138811130657, 2.307114084963398870 ) ) ;
#173060 = CARTESIAN_POINT ( 'NONE',  ( 3.128252755821586906, 1.147704512706015922, -1.711389856620056493 ) ) ;
#173061 = CARTESIAN_POINT ( 'NONE',  ( 5.355005569747676830, 0.3749256243090701712, -1.905367961469102811 ) ) ;
#173063 = EDGE_LOOP ( 'NONE', ( #64630, #27020, #23134, #141943 ) ) ;
#173062 = CARTESIAN_POINT ( 'NONE',  ( -6.995644074527074707, 11.10540915368285475, 0.000000000000000000 ) ) ;
#173064 = CARTESIAN_POINT ( 'NONE',  ( -6.607619761813764647, 8.802252036906432764, 1.599625672291269396 ) ) ;
#173065 = CARTESIAN_POINT ( 'NONE',  ( -4.318600669050631780, 4.999583595936801572, -2.420000000000000373 ) ) ;
#173067 = ORIENTED_EDGE ( 'NONE', *, *, #110609, .T. ) ;
#173066 = CARTESIAN_POINT ( 'NONE',  ( -1.668847547942637130E-13, 1.972237431424126441, -11.78526707783712624 ) ) ;
#173068 = CARTESIAN_POINT ( 'NONE',  ( -7.280365300414089802, 10.47721470291632784, 1.082531754730549967 ) ) ;
#173069 = CARTESIAN_POINT ( 'NONE',  ( 2.257103711190447282, -1.706036888594957723, 1.399758388914617013 ) ) ;
#173070 = CARTESIAN_POINT ( 'NONE',  ( -3.285556943750000070, -0.1093749995220438809, 0.000000000000000000 ) ) ;
#173071 = ORIENTED_EDGE ( 'NONE', *, *, #137433, .F. ) ;
#173072 = CARTESIAN_POINT ( 'NONE',  ( 6.965691013979927959, -0.4331334938386353084, 1.920344510276907890 ) ) ;
#173073 = CARTESIAN_POINT ( 'NONE',  ( 6.539320575229256249, 7.052319431262985105, 2.701414634427783845 ) ) ;
#173074 = CARTESIAN_POINT ( 'NONE',  ( -1.500000000000011324, 4.952083334016150751, 0.8660254037844403729 ) ) ;
#173075 = SURFACE_STYLE_FILL_AREA ( #154678 ) ;
#173077 = CARTESIAN_POINT ( 'NONE',  ( -10.99526901688165381, -7.794005300192725194, 0.3296348669024621314 ) ) ;
#173076 = CARTESIAN_POINT ( 'NONE',  ( -6.218052724642120666, 7.025831364812846758, -1.032658732443512584 ) ) ;
#173078 = CARTESIAN_POINT ( 'NONE',  ( 5.736236344406846932, 0.3633543575551900773, 1.804753862313414281 ) ) ;
#173079 = EDGE_LOOP ( 'NONE', ( #167316, #136607, #195077, #67292, #51118, #34299, #118153 ) ) ;
#173080 = CARTESIAN_POINT ( 'NONE',  ( 2.606383665309390363, -0.7875068868475536554, -1.904698518741376079 ) ) ;
#173081 = CARTESIAN_POINT ( 'NONE',  ( 1.360316468749949825, 0.2447916670081152490, 0.7853790794158741484 ) ) ;
#173082 = CARTESIAN_POINT ( 'NONE',  ( -7.366157530926372488, 7.488271962369228874, -0.7998128361456291469 ) ) ;
#173083 = CARTESIAN_POINT ( 'NONE',  ( 10.91819195543074450, -9.943514287384804362, -0.1813054759508098968 ) ) ;
#173084 = CARTESIAN_POINT ( 'NONE',  ( -15.75000000000000000, 13.40000000000000036, -0.7000000000000009548 ) ) ;
#173085 = B_SPLINE_CURVE_WITH_KNOTS ( 'NONE', 3,
 ( #141652, #175196, #156808, #8395, #190340, #25711 ),
 .UNSPECIFIED., .F., .F.,
 ( 4, 2, 4 ),
 ( 0.000000000000000000, 0.0002955107118804045814, 0.0005910214237608091628 ),
 .UNSPECIFIED. ) ;
#173086 = CARTESIAN_POINT ( 'NONE',  ( 3.635557746758808495, 7.393234471193928847, -0.7998128361456291469 ) ) ;
#173087 = CARTESIAN_POINT ( 'NONE',  ( 0.6728171419645075924, -1.940266777691628919, -0.6950667680841491336 ) ) ;
#173089 = CARTESIAN_POINT ( 'NONE',  ( 5.020983453748395497, -1.746657797055195305, 0.5827527221545365510 ) ) ;
#173088 = CARTESIAN_POINT ( 'NONE',  ( 4.871399016515830738, 4.969688109501518625, 0.6151586745235249065 ) ) ;
#173090 = CARTESIAN_POINT ( 'NONE',  ( 6.446011968293428041, 9.607765498729298415, -1.199719254218440723 ) ) ;
#173091 = CARTESIAN_POINT ( 'NONE',  ( -6.954406449166956605, 7.078172043641714595, -0.7998128361456362523 ) ) ;
#173093 = VERTEX_POINT ( 'NONE', #108608 ) ;
#173092 = CARTESIAN_POINT ( 'NONE',  ( 2.728371075039198512, 2.952267909019295367, 2.500000000000000000 ) ) ;
#173094 = CARTESIAN_POINT ( 'NONE',  ( 3.950008152305323428, 0.7444041667201054535, -2.077678867657362538 ) ) ;
#173095 = CARTESIAN_POINT ( 'NONE',  ( 0.8257154465432202661, -2.052837714267462754, 0.6772920067378007669 ) ) ;
#173096 = CARTESIAN_POINT ( 'NONE',  ( -5.097502569058215194, 6.970172302033127210, -1.443375672974053447 ) ) ;
#173097 = CARTESIAN_POINT ( 'NONE',  ( -0.1581436608063293003, -1.178060542814472367, -1.506996232563104776 ) ) ;
#173098 = CARTESIAN_POINT ( 'NONE',  ( 0.7961116948485976730, -0.9110139862544311962, -1.799120828532501326 ) ) ;
#173099 = CARTESIAN_POINT ( 'NONE',  ( 7.526184668917440312, 8.913541880892736913, -1.082531754730548412 ) ) ;
#173100 = CARTESIAN_POINT ( 'NONE',  ( 1.722429217803717938, -1.971362081364759655, -1.181495133065799230 ) ) ;
#173101 = DIRECTION ( 'NONE',  ( 0.000000000000000000, -1.000000000000000000, 0.000000000000000000 ) ) ;
#173102 = CARTESIAN_POINT ( 'NONE',  ( 6.498695769366850783, -1.876353784076413067, -0.3680397143606057853 ) ) ;
#173103 = B_SPLINE_CURVE_WITH_KNOTS ( 'NONE', 3,
 ( #44093, #124349, #159960, #93920 ),
 .UNSPECIFIED., .F., .F.,
 ( 4, 4 ),
 ( 8.674676106452419934E-19, 9.170750103568725835E-05 ),
 .UNSPECIFIED. ) ;
#173104 = CARTESIAN_POINT ( 'NONE',  ( 11.33772463945036790, 12.69999999999999929, -3.600000000000000977 ) ) ;
#173105 = CARTESIAN_POINT ( 'NONE',  ( 0.2681426532152464959, -1.225442487749365483, 1.413462724991432218 ) ) ;
#173106 = CARTESIAN_POINT ( 'NONE',  ( 2.870327622459168726, -1.987497926849005836, -0.3399570244180456502 ) ) ;
#173108 = CARTESIAN_POINT ( 'NONE',  ( -4.515041659042474897, 7.522260248201400934, 0.9990323037335177014 ) ) ;
#173107 = CARTESIAN_POINT ( 'NONE',  ( 0.6823417656249882723, 1.176041667008083325, -1.181850606188749264 ) ) ;
#173110 = CARTESIAN_POINT ( 'NONE',  ( 4.055375990838584244, -1.750834834141304697, -1.170193647660602965 ) ) ;
#173109 = CARTESIAN_POINT ( 'NONE',  ( -8.799405390469187793, 10.22472669609091689, -1.199719254218446718 ) ) ;
#173111 = CARTESIAN_POINT ( 'NONE',  ( 8.121497709785879593, 9.433834401960398353, -1.199719254218445830 ) ) ;
#173113 = CARTESIAN_POINT ( 'NONE',  ( -6.842061076390810292, 11.13415502243129218, 0.000000000000000000 ) ) ;
#173112 = CARTESIAN_POINT ( 'NONE',  ( 4.411198876399872404, 6.239761003923544713, -1.599625672291273171 ) ) ;
#173114 = CARTESIAN_POINT ( 'NONE',  ( 11.48784849554594345, 9.769504728180750774, 3.469614872287801521 ) ) ;
#173115 = CARTESIAN_POINT ( 'NONE',  ( 4.535418805095452477, -0.09482428102505417733, 2.017666594091566346 ) ) ;
#173116 = CARTESIAN_POINT ( 'NONE',  ( -1.364683531250010295, 4.530208333674754506, 0.7879004041258379498 ) ) ;
#173117 = CARTESIAN_POINT ( 'NONE',  ( 8.053180056837369705, 11.37883191874353805, -1.082531754730543083 ) ) ;
#173118 = ADVANCED_FACE ( 'NONE', ( #171403 ), #141086, .F. ) ;
#173119 = CARTESIAN_POINT ( 'NONE',  ( 4.657600047955182454, 0.4785990281669267876, -2.107782517917502929 ) ) ;
#173120 = CARTESIAN_POINT ( 'NONE',  ( 7.537407054554579489, 7.758339416593960536, 0.000000000000000000 ) ) ;
#173121 = CARTESIAN_POINT ( 'NONE',  ( -1.364683531250014514, -0.1572916663252435232, 0.7879004041258379498 ) ) ;
#173123 = SURFACE_STYLE_USAGE ( .BOTH. , #40989 ) ;
#173122 = CARTESIAN_POINT ( 'NONE',  ( 5.692444392891300886, 7.734547439830227411, -1.599625672291281386 ) ) ;
#173124 = CARTESIAN_POINT ( 'NONE',  ( 8.473482818416664841, 10.90881592628469932, -1.443375672974063439 ) ) ;
#173126 = CARTESIAN_POINT ( 'NONE',  ( -2.296876792725286887, 2.697690400687393630, -2.500000000000000000 ) ) ;
#173125 = CARTESIAN_POINT ( 'NONE',  ( 1.574930973106080545, 1.458645925580204006, -1.608354241196547685 ) ) ;
#173128 = CARTESIAN_POINT ( 'NONE',  ( 0.3273695209934923689, 0.9472894719858866441, -1.578709817245539604 ) ) ;
#173127 = CARTESIAN_POINT ( 'NONE',  ( -6.588899466561478846, 6.789396920517583922, 0.7216878364870317197 ) ) ;
#173129 = CARTESIAN_POINT ( 'NONE',  ( 1.364683531249988535, 1.613541667008084879, 0.7879004041258500513 ) ) ;
#173130 = CARTESIAN_POINT ( 'NONE',  ( 3.333693798916517625, 0.9835563995168915552, -1.958507884819527867 ) ) ;
#173131 = CARTESIAN_POINT ( 'NONE',  ( -0.4373225248172924462, -7.723431457505077979, 10.96785329849814161 ) ) ;
#173132 = CARTESIAN_POINT ( 'NONE',  ( 3.467884472470097457, 2.207893551020873257, -0.4935151710872084929 ) ) ;
#173133 = CARTESIAN_POINT ( 'NONE',  ( -6.157374318900681764, 10.33535380535947290, 0.7998128361456481317 ) ) ;
#173134 = CARTESIAN_POINT ( 'NONE',  ( -1.001543065824772872E-14, 5.384375000341415252, 1.575800808251672791 ) ) ;
#173135 = CARTESIAN_POINT ( 'NONE',  ( 6.080034374691865473, 7.023743017405461586, -0.9950221519831742301 ) ) ;
#173136 = CARTESIAN_POINT ( 'NONE',  ( 1.499999999999993117, 12.60416666666666785, 0.8660254037844409281 ) ) ;
#173137 = CARTESIAN_POINT ( 'NONE',  ( 5.316205630334249754, 7.295602216847000498, -1.443375672974078761 ) ) ;
#173138 = EDGE_CURVE ( 'NONE', #188369, #210693, #83632, .T. ) ;
#173139 = CARTESIAN_POINT ( 'NONE',  ( 3.778344457583324711, -1.704853921413415296, -0.4744283172272641957 ) ) ;
#173140 = CARTESIAN_POINT ( 'NONE',  ( 8.769426429940780920, 9.125419011219408461, 0.7998128361456462443 ) ) ;
#173141 = CARTESIAN_POINT ( 'NONE',  ( 0.9210891864466156376, 1.945811402625597486, 0.8060233215861163369 ) ) ;
#173143 = CARTESIAN_POINT ( 'NONE',  ( 0.7499999999999902300, 1.483333333333357373, 1.299038105676657340 ) ) ;
#173142 = CARTESIAN_POINT ( 'NONE',  ( -1.364683531250014514, 10.08854166700806410, -0.7879004041258335089 ) ) ;
#173144 = CARTESIAN_POINT ( 'NONE',  ( 0.6253724811571198527, 0.1964764651697422093, -1.959740272926189464 ) ) ;
#173145 = CARTESIAN_POINT ( 'NONE',  ( -3.284818356260900796, 7.054314858938165678, 0.7998128361456352531 ) ) ;
#173146 = CARTESIAN_POINT ( 'NONE',  ( 8.917737905728806425, 3.447199233515649386, 8.029567276306217138 ) ) ;
#173148 = VERTEX_POINT ( 'NONE', #121679 ) ;
#173147 = CARTESIAN_POINT ( 'NONE',  ( 5.291193953664572902, -0.05252268709225348109, -1.811016617013387009 ) ) ;
#173149 = CARTESIAN_POINT ( 'NONE',  ( 5.978782553946477840, 9.919070713005490703, 1.040834085586084257E-14 ) ) ;
#173150 = CARTESIAN_POINT ( 'NONE',  ( 9.694243528971124846, 11.26870452434320491, 1.199719254218450271 ) ) ;
#173151 = CARTESIAN_POINT ( 'NONE',  ( 4.539837415608827698, 0.7997722286730184482, -1.691214532891088362 ) ) ;
#173152 = CARTESIAN_POINT ( 'NONE',  ( 3.623053363349855172, 5.249981562040033189, 1.599625672291267398 ) ) ;
#173153 = EDGE_LOOP ( 'NONE', ( #165697, #78498 ) ) ;
#173154 = CARTESIAN_POINT ( 'NONE',  ( 4.100488025649267954, 2.059819936833905185, 0.2079151390043249559 ) ) ;
#173155 = CARTESIAN_POINT ( 'NONE',  ( -1.225000000000044276, 1.770833333333392545, 0.7072540797572737237 ) ) ;
#173156 =( BOUNDED_SURFACE ( )  B_SPLINE_SURFACE ( 3, 3, ( 
 ( #142918, #172192, #23781, #109388, #207863, #206798, #76797, #125644, #58431, #89887 ),
 ( #189492, #108316, #155938, #208918, #158081, #59487, #57365, #191606, #10727, #122462 ),
 ( #43268, #60552, #157015, #72530, #175393, #141856, #41136, #173267, #7524, #26979 ),
 ( #110448, #73607, #93084, #159126, #90948, #74683, #139706, #8599, #140784, #188420 ),
 ( #205729, #192672, #126712, #40056, #138627, #174337, #44326, #124584, #22700, #88812 ),
 ( #107246, #154870, #123527, #6453, #25915, #190544, #204651, #42201, #92023, #9668 ),
 ( #56300, #75744, #196953, #147161, #180704, #162336, #211052, #177516, #29129, #32327 ) ),
 .UNSPECIFIED., .T., .F., .T. ) 
 B_SPLINE_SURFACE_WITH_KNOTS ( ( 4, 3, 4 ),
 ( 4, 1, 1, 1, 1, 1, 1, 4 ),
 ( 0.000000000000000000, 0.5000000000000000000, 1.000000000000000000 ),
 ( 0.000000000000000000, 0.09272347919791326665, 0.1850049962306132278, 0.2567072177207115891, 0.3610482009861257779, 0.5209239196176974618, 0.7336689415868371533, 1.000000000000000000 ),
 .UNSPECIFIED. ) 
 GEOMETRIC_REPRESENTATION_ITEM ( )  RATIONAL_B_SPLINE_SURFACE ( (
 ( 1.000000000000000444, 1.000000000000000444, 1.000000000000000222, 1.000000000000000444, 1.000000000000000222, 1.000000000000000444, 1.000000000000000222, 1.000000000000000222, 1.000000000000000222, 1.000000000000000222),
 ( 0.3333333333333334814, 0.3333333333333335369, 0.3333333333333334814, 0.3333333333333334259, 0.3333333333333334259, 0.3333333333333334259, 0.3333333333333334259, 0.3333333333333334259, 0.3333333333333334259, 0.3333333333333334259),
 ( 0.3333333333333334814, 0.3333333333333335369, 0.3333333333333334814, 0.3333333333333334259, 0.3333333333333334259, 0.3333333333333334259, 0.3333333333333334259, 0.3333333333333334259, 0.3333333333333334259, 0.3333333333333334259),
 ( 1.000000000000000444, 1.000000000000000444, 1.000000000000000222, 1.000000000000000444, 1.000000000000000222, 1.000000000000000444, 1.000000000000000222, 1.000000000000000222, 1.000000000000000222, 1.000000000000000222),
 ( 0.3333333333333334814, 0.3333333333333335369, 0.3333333333333334814, 0.3333333333333334259, 0.3333333333333334259, 0.3333333333333334259, 0.3333333333333334259, 0.3333333333333334259, 0.3333333333333334259, 0.3333333333333334259),
 ( 0.3333333333333334814, 0.3333333333333335369, 0.3333333333333334814, 0.3333333333333334259, 0.3333333333333334259, 0.3333333333333334259, 0.3333333333333334259, 0.3333333333333334259, 0.3333333333333334259, 0.3333333333333334259),
 ( 1.000000000000000444, 1.000000000000000444, 1.000000000000000222, 1.000000000000000444, 1.000000000000000222, 1.000000000000000444, 1.000000000000000222, 1.000000000000000222, 1.000000000000000222, 1.000000000000000222) ) ) 
 REPRESENTATION_ITEM ( '' )  SURFACE ( )  );
#173157 = CARTESIAN_POINT ( 'NONE',  ( -4.570507181138272479, 7.385989907086349504, 1.082531754730549967 ) ) ;
#173158 = CARTESIAN_POINT ( 'NONE',  ( 2.228883261964242912, -0.9158852807988100420, -2.473645833743700173 ) ) ;
#173159 = CARTESIAN_POINT ( 'NONE',  ( 9.185812768458653466, 10.67553530374532045, 1.199719254218453823 ) ) ;
#173160 = CARTESIAN_POINT ( 'NONE',  ( -1.503277409322750779, 8.660639097433820766, 2.556074651073470427 ) ) ;
#173161 = CARTESIAN_POINT ( 'NONE',  ( 6.668631453075247073, 8.873432343378178544, -1.599625672291281386 ) ) ;
#173162 = CARTESIAN_POINT ( 'NONE',  ( 4.879147978569815969, 4.879180288469956217, -0.1512534140984626019 ) ) ;
#173163 = EDGE_CURVE ( 'NONE', #165149, #149524, #132076, .T. ) ;
#173164 = B_SPLINE_CURVE_WITH_KNOTS ( 'NONE', 1,
 ( #114133, #115184 ),
 .UNSPECIFIED., .F., .F.,
 ( 2, 2 ),
 ( 0.07258517961950859687, 1.000000000000000000 ),
 .UNSPECIFIED. ) ;
#173165 = CARTESIAN_POINT ( 'NONE',  ( -1.364683531250000748, -0.2406249996585799189, 0.000000000000000000 ) ) ;
#173166 = CARTESIAN_POINT ( 'NONE',  ( -1.402160292154681736E-14, 0.3375000000000208389, -1.732050807568870754 ) ) ;
#173167 = CARTESIAN_POINT ( 'NONE',  ( 4.017981030900905637, 1.947309607215493621, -0.2378496960543720617 ) ) ;
#173168 = EDGE_CURVE ( 'NONE', #207594, #149695, #208158, .T. ) ;
#173169 = CARTESIAN_POINT ( 'NONE',  ( 2.091172504846372959, 1.163092143266548639, -1.646586049616038494 ) ) ;
#173170 = CARTESIAN_POINT ( 'NONE',  ( 9.491012693391987787E-16, 7.250000000000006217, -7.750000000000000888 ) ) ;
#173171 = CARTESIAN_POINT ( 'NONE',  ( -0.1290005225502675879, -0.006633637972621592160, -2.173875058097324064 ) ) ;
#173172 = CARTESIAN_POINT ( 'NONE',  ( 2.002991962376502233, 1.552455721610061179, 1.043161660468715279 ) ) ;
#173173 = CARTESIAN_POINT ( 'NONE',  ( -0.6823417656250212460, 4.801041667008086655, 1.181850606188767472 ) ) ;
#173175 = CARTESIAN_POINT ( 'NONE',  ( 2.812237032231167611, 1.173781612916646289, -1.761886306039317285 ) ) ;
#173174 = CARTESIAN_POINT ( 'NONE',  ( -5.694061328059534688, 8.626526735169329996, 1.082531754730548412 ) ) ;
#173176 = DIRECTION ( 'NONE',  ( 5.551115123125764829E-17, 0.000000000000000000, -1.000000000000000000 ) ) ;
#173177 = CARTESIAN_POINT ( 'NONE',  ( 5.125469573878929097, 0.2063957376101481500, -2.060066405364005426 ) ) ;
#173178 = CARTESIAN_POINT ( 'NONE',  ( 5.332099551924443404, 9.442809587212341427, 0.000000000000000000 ) ) ;
#173180 = CARTESIAN_POINT ( 'NONE',  ( 6.620655732516649294, 2.950034989283246478, 2.626075342966327497 ) ) ;
#173179 = CARTESIAN_POINT ( 'NONE',  ( 0.3102505407175432661, 1.438864707272140775, -1.517118456267575022 ) ) ;
#173182 = VERTEX_POINT ( 'NONE', #59788 ) ;
#173181 = CARTESIAN_POINT ( 'NONE',  ( 5.368107995252269227, 0.9013511576922846880, 1.587453057759043551 ) ) ;
#173183 = CARTESIAN_POINT ( 'NONE',  ( 9.738834413317897898, 10.25639499182604730, 0.000000000000000000 ) ) ;
#173184 = CARTESIAN_POINT ( 'NONE',  ( -4.446711195602252253, 6.210915699667824974, -1.443375672974053892 ) ) ;
#173185 = FILL_AREA_STYLE ('',( #88731 ) ) ;
#173186 = CARTESIAN_POINT ( 'NONE',  ( -11.30310531956832598, 5.150576456239967627, 5.742040133384030298 ) ) ;
#173187 = CARTESIAN_POINT ( 'NONE',  ( 6.277061933002769045, 10.26706332190449622, 0.7216878364870438212 ) ) ;
#173188 = CARTESIAN_POINT ( 'NONE',  ( -1.364683531250010740, 12.44270833367473195, 0.7879004041258445001 ) ) ;
#173189 = CARTESIAN_POINT ( 'NONE',  ( 5.795548653916324788, 1.765151677092157811, -0.7360495477024899813 ) ) ;
#173190 = CARTESIAN_POINT ( 'NONE',  ( -8.809047120577080392, 11.30030761213851953, 1.599625672291269396 ) ) ;
#173191 = CARTESIAN_POINT ( 'NONE',  ( 4.547870462380197765, 7.393267075163835855, 1.199719254218462483 ) ) ;
#173192 = CARTESIAN_POINT ( 'NONE',  ( 0.6801582343750022241, 2.838541667008094738, -1.178068619123834759 ) ) ;
#173193 = CARTESIAN_POINT ( 'NONE',  ( 0.9999999999999833467, 5.868705557303652398, 4.125226524755083446 ) ) ;
#173194 = CARTESIAN_POINT ( 'NONE',  ( 4.684505768721569652, 5.424010470718658716, -1.199719254218452047 ) ) ;
#173195 = EDGE_LOOP ( 'NONE', ( #210939, #144432, #194008, #165434 ) ) ;
#173196 = EDGE_CURVE ( 'NONE', #155317, #171094, #6749, .T. ) ;
#173197 = AXIS2_PLACEMENT_3D ( 'NONE', #30733, #95747, #181223 ) ;
#173198 = CARTESIAN_POINT ( 'NONE',  ( -7.286581212701773502, 7.465709267765667789, 0.7998128361456341429 ) ) ;
#173199 = CARTESIAN_POINT ( 'NONE',  ( 5.290638740200859225, 1.525033539048275877, -1.319242139327673424 ) ) ;
#173200 = CARTESIAN_POINT ( 'NONE',  ( 0.01315889736931378021, -9.583523248314012477, -9.500441148488286913 ) ) ;
#173201 = CYLINDRICAL_SURFACE ( 'NONE', #126558, 1.500000000000000222 ) ;
#173202 = CARTESIAN_POINT ( 'NONE',  ( -6.497544600628390121, 6.760421010857692536, 0.1165534177344582784 ) ) ;
#173203 = CARTESIAN_POINT ( 'NONE',  ( -5.585596099150199834, 5.618876325204420930, -0.7216878364870207285 ) ) ;
#173204 = CARTESIAN_POINT ( 'NONE',  ( 3.195971524519376494, 4.751719416737803847, -1.599625672291262513 ) ) ;
#173205 = CARTESIAN_POINT ( 'NONE',  ( 2.272252165359678333, -0.9238012212633615050, -1.739302338446031548 ) ) ;
#173206 = CARTESIAN_POINT ( 'NONE',  ( 5.009388752257521560, -1.913799287717246500, 0.6352160319311253023 ) ) ;
#173207 = CARTESIAN_POINT ( 'NONE',  ( -5.032047568966410367, 9.022472597102808578, 1.214306433183764966E-14 ) ) ;
#173208 = CARTESIAN_POINT ( 'NONE',  ( 6.827182134110238110, 0.5514785450725538940, 2.340047124761033714 ) ) ;
#173209 = CARTESIAN_POINT ( 'NONE',  ( 5.068408068084750973, -2.062719301109996461, -0.7404068969242217912 ) ) ;
#173210 = SURFACE_SIDE_STYLE ('',( #44269 ) ) ;
#173211 = CARTESIAN_POINT ( 'NONE',  ( 2.942313797947668785, 1.911627860423757097, 0.2376154225440275658 ) ) ;
#173212 = CARTESIAN_POINT ( 'NONE',  ( -8.320953590485107298, 10.73086516036454618, 1.599625672291269396 ) ) ;
#173213 = PRESENTATION_STYLE_ASSIGNMENT (( #57311 ) ) ;
#173214 = DIRECTION ( 'NONE',  ( 0.000000000000000000, 7.228014483236694583E-17, -1.000000000000000000 ) ) ;
#173215 = LINE ( 'NONE', #107190, #47814 ) ;
#173216 = CARTESIAN_POINT ( 'NONE',  ( 0.6823417656249934904, 12.94270833367473017, 1.181850606188764807 ) ) ;
#173217 = CARTESIAN_POINT ( 'NONE',  ( 4.137209430464448445, 7.978494768850520558, 1.040834085586084257E-14 ) ) ;
#173218 = CARTESIAN_POINT ( 'NONE',  ( 1.071256458935646111E-16, 3.500000000000000888, 1.600000000000005196 ) ) ;
#173219 = CARTESIAN_POINT ( 'NONE',  ( 6.549997609177859559, 6.814287763561861944, 0.000000000000000000 ) ) ;
#173220 = ORIENTED_EDGE ( 'NONE', *, *, #136253, .T. ) ;
#173222 = CARTESIAN_POINT ( 'NONE',  ( 2.420566579892877268, -0.7724838186086988578, -1.859170112617714699 ) ) ;
#173221 = CARTESIAN_POINT ( 'NONE',  ( 5.899929530298204661, -0.6689130865737795695, -1.715630562827724637 ) ) ;
#173223 = CARTESIAN_POINT ( 'NONE',  ( 5.765083458594993715, -2.298542321979883507, -0.008455817729055568541 ) ) ;
#173224 = CARTESIAN_POINT ( 'NONE',  ( 2.834617457269935414, -1.779228943046967437, -0.5452927797432933765 ) ) ;
#173225 = CARTESIAN_POINT ( 'NONE',  ( -3.285556943749998737, -0.4302083328553760744, 1.896917185911908499 ) ) ;
#173226 = CARTESIAN_POINT ( 'NONE',  ( -0.1290005225502433017, 0.6921039065478848951, -2.255494067288220439 ) ) ;
#173227 = CARTESIAN_POINT ( 'NONE',  ( 6.533470333208203584, -0.1312131129157616261, 1.882018712217728318 ) ) ;
#173228 = CARTESIAN_POINT ( 'NONE',  ( -6.333630315878337136, 10.54098580183340772, 0.000000000000000000 ) ) ;
#173229 = CARTESIAN_POINT ( 'NONE',  ( -5.478903473698268023, 5.564677938835638216, -0.7216878364870338292 ) ) ;
#173230 = CARTESIAN_POINT ( 'NONE',  ( 6.198786912940476235, 1.738631647849303130, 1.160874564816395615 ) ) ;
#173231 = CARTESIAN_POINT ( 'NONE',  ( 5.341549334104184865, 8.215262742221458581, 1.082531754730558626 ) ) ;
#173232 = ORIENTED_EDGE ( 'NONE', *, *, #46509, .F. ) ;
#173233 = FACE_OUTER_BOUND ( 'NONE', #187321, .T. ) ;
#173235 = CARTESIAN_POINT ( 'NONE',  ( 4.650610384687404952, 5.384465856012134566, 1.199719254218462483 ) ) ;
#173234 = PLANE ( 'NONE',  #127571 ) ;
#173236 = CARTESIAN_POINT ( 'NONE',  ( 6.568995754424670430, -1.580519633186812767, -0.6912669513192554183 ) ) ;
#173237 = CARTESIAN_POINT ( 'NONE',  ( -4.737684612971557740, 7.614716917520386374, 1.199719254218464037 ) ) ;
#173238 =( BOUNDED_CURVE ( )  B_SPLINE_CURVE ( 2, ( #10056, #126031, #77191 ),
 .UNSPECIFIED., .F., .T. ) 
 B_SPLINE_CURVE_WITH_KNOTS ( ( 3, 3 ),
 ( 0.000000000000000000, 0.004781798612014134114 ),
 .UNSPECIFIED. ) 
 CURVE ( )  GEOMETRIC_REPRESENTATION_ITEM ( )  RATIONAL_B_SPLINE_CURVE ( ( 1.000000000000000000, 0.9231232554125530232, 0.9344726973605665954 ) ) 
 REPRESENTATION_ITEM ( '' )  );
#173239 = AXIS2_PLACEMENT_3D ( 'NONE', #113413, #144819, #12621 ) ;
#173240 = CARTESIAN_POINT ( 'NONE',  ( 0.9494047574800461575, -1.567277312892487284, -0.7424874142042283687 ) ) ;
#173241 = FACE_OUTER_BOUND ( 'NONE', #57806, .T. ) ;
#173242 = ADVANCED_FACE ( 'NONE', ( #24074 ), #133970, .T. ) ;
#173243 = CARTESIAN_POINT ( 'NONE',  ( 0.000000000000000000, 7.980384757729337863, 0.000000000000000000 ) ) ;
#173244 = CARTESIAN_POINT ( 'NONE',  ( 5.383699271828307431, -2.063871618437407740, 0.6740922461795120224 ) ) ;
#173245 = CARTESIAN_POINT ( 'NONE',  ( 4.705575438601840688, -0.4840451379145363497, 1.760283039881085809 ) ) ;
#173246 = CARTESIAN_POINT ( 'NONE',  ( 2.166782468979636000, 1.457124453068344039, -1.313723524322525815 ) ) ;
#173247 = TOROIDAL_SURFACE ( 'NONE', #79837, 2.649999999999999911, 0.1000000000000000056 ) ;
#173248 =( LENGTH_UNIT ( ) NAMED_UNIT ( * ) SI_UNIT ( .MILLI., .METRE. ) );
#173249 = CARTESIAN_POINT ( 'NONE',  ( 7.182068686937156166, 9.402166106225269715, 1.599625672291281386 ) ) ;
#173250 = CARTESIAN_POINT ( 'NONE',  ( 3.352298257493666167, 0.9517314053594098100, -1.894962337767625904 ) ) ;
#173251 = CARTESIAN_POINT ( 'NONE',  ( -0.3275200278799458298, 3.116672424413460263, 0.4674645318177237940 ) ) ;
#173252 = PLANE ( 'NONE',  #187949 ) ;
#173253 = CARTESIAN_POINT ( 'NONE',  ( -4.744851797206062649, 6.824086272657805985, -1.238183395270262999 ) ) ;
#173254 = CARTESIAN_POINT ( 'NONE',  ( 2.043885321627556095, 1.424625833772466210, 1.502381739045772546 ) ) ;
#173256 = CARTESIAN_POINT ( 'NONE',  ( -0.7500000000000179856, 15.07291666734946567, 1.299038105676658228 ) ) ;
#173255 = CARTESIAN_POINT ( 'NONE',  ( -10.18412789821966413, 3.641746037092307819, 6.362472743772858763 ) ) ;
#173258 = VERTEX_POINT ( 'NONE', #195126 ) ;
#173257 = CARTESIAN_POINT ( 'NONE',  ( 3.387547421374631273, 0.05309406834838430178, -2.220816570709438498 ) ) ;
#173259 = CARTESIAN_POINT ( 'NONE',  ( 2.250986472945924355, 2.253575863342609065, -0.4525425749238082829 ) ) ;
#173261 = CARTESIAN_POINT ( 'NONE',  ( 6.948098685450462497, -0.8862217868219750549, 1.860397500250488001 ) ) ;
#173260 = CARTESIAN_POINT ( 'NONE',  ( 8.676855123066012254, 11.14608361504227574, -1.443375672974052559 ) ) ;
#173263 = CARTESIAN_POINT ( 'NONE',  ( -3.475000000000000533, -0.6999999999999992895, 0.000000000000000000 ) ) ;
#173262 = CARTESIAN_POINT ( 'NONE',  ( 4.258142763143749399, 7.125527769379820242, 1.199719254218451159 ) ) ;
#173264 = CYLINDRICAL_SURFACE ( 'NONE', #92484, 1.500000000000000222 ) ;
#173265 = CARTESIAN_POINT ( 'NONE',  ( -11.04985331135689108, 11.10920893529997855, 1.056514597312212755 ) ) ;
#173266 = CARTESIAN_POINT ( 'NONE',  ( -5.796211742350026341, 6.069872996917573538, -0.5622600474562855499 ) ) ;
#173267 = CARTESIAN_POINT ( 'NONE',  ( -0.1102773484823963285, 5.719690680991945442, -2.797532285072940272 ) ) ;
#173268 = CARTESIAN_POINT ( 'NONE',  ( 2.959633327367673150, 1.716642837065301519, -0.1670560860976433859 ) ) ;
#173269 = CARTESIAN_POINT ( 'NONE',  ( 2.255092540634635156, 0.09411513195021346811, -2.014433103604281960 ) ) ;
#173270 = CARTESIAN_POINT ( 'NONE',  ( 2.989241104188970155, -2.295904969233518500, 0.1156830036863568528 ) ) ;
#173271 = CARTESIAN_POINT ( 'NONE',  ( 3.813984095001612395, -2.229740912845196377, 0.3821933647679372492 ) ) ;
#173272 = CARTESIAN_POINT ( 'NONE',  ( 5.637368906844186789, -1.904612104999114708, 0.8991850809280316215 ) ) ;
#173273 = CARTESIAN_POINT ( 'NONE',  ( -7.105881907338169157, 8.423188659050232729, -1.082531754730549967 ) ) ;
#173274 = CARTESIAN_POINT ( 'NONE',  ( 3.268565602506213974, -1.633896335792903054, -0.6804537918285047393 ) ) ;
#173276 = CARTESIAN_POINT ( 'NONE',  ( 6.497627784488766878, -2.291974509058695375, 0.05125074467529803363 ) ) ;
#173275 = CARTESIAN_POINT ( 'NONE',  ( 8.174640274396848483, 8.501778173076651512, 0.7998128361456291469 ) ) ;
#173277 = CARTESIAN_POINT ( 'NONE',  ( 5.279192629422701621, 1.239228542960477242, 1.361826556748657602 ) ) ;
#173278 = CARTESIAN_POINT ( 'NONE',  ( -4.810445574750349174, 4.506608013497163334, 0.7998128361456341429 ) ) ;
#173279 = CARTESIAN_POINT ( 'NONE',  ( 5.490230790444213582, -0.5297859672059505032, -2.126319610106224278 ) ) ;
#173280 = CARTESIAN_POINT ( 'NONE',  ( -2.788173145904702555, 6.404619103530779789, -0.7998128361456281477 ) ) ;
#173281 = DIRECTION ( 'NONE',  ( 0.000000000000000000, 0.000000000000000000, -1.000000000000000000 ) ) ;
#173282 = CARTESIAN_POINT ( 'NONE',  ( 5.582505937350194181, 1.236201877336528643, -1.660625051266072960 ) ) ;
#173283 = CARTESIAN_POINT ( 'NONE',  ( -0.2234322562767385167, -0.4468160588090731022, -1.973564571300358228 ) ) ;
#173284 = CARTESIAN_POINT ( 'NONE',  ( -0.7500000000000249800, -1.027083332650516212, 1.299038105676659116 ) ) ;
#173285 = CARTESIAN_POINT ( 'NONE',  ( 3.861874329138580197, 1.911805356762337205, -0.2370204922254297297 ) ) ;
#173286 = CARTESIAN_POINT ( 'NONE',  ( -1.402160292154681736E-14, 10.17187500034139447, 1.575800808251682339 ) ) ;
#173287 = DIRECTION ( 'NONE',  ( 0.000000000000000000, -1.000000000000000000, 0.000000000000000000 ) ) ;
#173288 = CARTESIAN_POINT ( 'NONE',  ( -0.06965283525045895541, -2.176852707449424607, 0.4419662969857121038 ) ) ;
#173290 = EDGE_LOOP ( 'NONE', ( #202238, #92434, #8233, #5039, #206880, #132932, #131426, #117286 ) ) ;
#173289 = CARTESIAN_POINT ( 'NONE',  ( 5.090160327287878594, 4.903218234782778850, -0.7998128361456481317 ) ) ;
#173291 = CARTESIAN_POINT ( 'NONE',  ( -5.329763783947941036, 5.390681634126922361, 0.000000000000000000 ) ) ;
#173292 = CARTESIAN_POINT ( 'NONE',  ( 3.460355519985863548, 5.060167411448709629, 1.599625672291267398 ) ) ;
#173293 = CARTESIAN_POINT ( 'NONE',  ( 6.170369307550812366, 6.371388078330368465, 0.7216878364870467077 ) ) ;
#173294 = DIRECTION ( 'NONE',  ( 5.551115123125764829E-17, 0.000000000000000000, -1.000000000000000000 ) ) ;
#173295 = DIRECTION ( 'NONE',  ( 7.387867266669436732E-31, -1.000000000000000000, -8.546850786086424434E-32 ) ) ;
#173296 = CARTESIAN_POINT ( 'NONE',  ( 9.531018800282598846, 12.14260790512831889, 1.443375672974076540 ) ) ;
#173298 = EDGE_CURVE ( 'NONE', #52465, #164408, #130200, .T. ) ;
#173297 = CARTESIAN_POINT ( 'NONE',  ( 0.9241798626423224361, 0.9638202082158978667, 1.708698881219716137 ) ) ;
#173299 = CARTESIAN_POINT ( 'NONE',  ( 0.6823417656249899377, 0.9052083336747520637, 1.181850606188755259 ) ) ;
#173300 = CARTESIAN_POINT ( 'NONE',  ( -0.4170821662629279336, 3.033599471985628959, -0.4170821662629279336 ) ) ;
#173301 = EDGE_CURVE ( 'NONE', #193391, #77381, #156322, .T. ) ;
#173302 = CARTESIAN_POINT ( 'NONE',  ( 5.564887814092526419, 1.486691789297951871, -1.280227714881218892 ) ) ;
#173303 = CARTESIAN_POINT ( 'NONE',  ( -9.104463846776669200, 10.58062822844965645, -1.199719254218441611 ) ) ;
#173304 = AXIS2_PLACEMENT_3D ( 'NONE', #90156, #21896, #202792 ) ;
#173305 = CARTESIAN_POINT ( 'NONE',  ( -5.056828107772860292, 6.922718763866881453, -1.443375672974051449 ) ) ;
#173306 = CARTESIAN_POINT ( 'NONE',  ( 0.2513181340676704512, -1.814898432050582766, 1.350810986113021750 ) ) ;
#173308 = VERTEX_POINT ( 'NONE', #43565 ) ;
#173307 = CARTESIAN_POINT ( 'NONE',  ( -5.032047568966410367, 9.022472597102808578, 1.214306433183764966E-14 ) ) ;
#173309 = CARTESIAN_POINT ( 'NONE',  ( -1.001543065824772872E-14, 5.321875000341422357, 1.575800808251672791 ) ) ;
#173310 = CARTESIAN_POINT ( 'NONE',  ( 1.967826412060974084, 0.9573937279930484490, 1.606809688844474726 ) ) ;
#173311 = CARTESIAN_POINT ( 'NONE',  ( 0.5099215751255279372, -1.647279052675547861, 0.5420907402255652485 ) ) ;
#173313 = CARTESIAN_POINT ( 'NONE',  ( 4.054362073078698891, -1.623213109359676443, 1.472610181411204922 ) ) ;
#173312 = CARTESIAN_POINT ( 'NONE',  ( 1.360316468749994012, 2.265625000341386919, -1.387778780781445676E-14 ) ) ;
#173314 = CARTESIAN_POINT ( 'NONE',  ( 3.962222562901392742, 2.290579029535879219, -0.2790985642298955405 ) ) ;
#173315 = CARTESIAN_POINT ( 'NONE',  ( 6.919229409281150822, -0.1609914934341447335, 2.026046322553672674 ) ) ;
#173316 = CARTESIAN_POINT ( 'NONE',  ( 2.308448745193259821, 1.734665721750632938, 0.8731161087585439518 ) ) ;
#173317 = CARTESIAN_POINT ( 'NONE',  ( -4.216222583725562245, 7.862750747747711877, 0.7216878364870317197 ) ) ;
#173318 = PRODUCT_DEFINITION_SHAPE ( 'NONE', 'NONE',  #214416 ) ;
#173319 = FACE_OUTER_BOUND ( 'NONE', #30910, .T. ) ;
#173321 = EDGE_CURVE ( 'NONE', #26714, #198442, #28528, .T. ) ;
#173320 = CARTESIAN_POINT ( 'NONE',  ( 5.537388447972660721, -0.05000006065614125139, 2.120159173171487055 ) ) ;
#173322 = CARTESIAN_POINT ( 'NONE',  ( -1.360316468750046859, 0.3697916670080757529, -0.7853790794159101196 ) ) ;
#173323 = CARTESIAN_POINT ( 'NONE',  ( 3.621720349255663773, 0.2986264320336135536, 1.994071497604548382 ) ) ;
#173324 = CARTESIAN_POINT ( 'NONE',  ( -4.080641047588907888, 6.744203074620265248, -1.082531754730548412 ) ) ;
#173325 = CARTESIAN_POINT ( 'NONE',  ( -7.957709816578236506, 8.248692638954882028, 0.7998128361456341429 ) ) ;
#173326 = CARTESIAN_POINT ( 'NONE',  ( 7.886038904643079661, 12.35212915539230139, -0.7998128361456352531 ) ) ;
#173327 = CARTESIAN_POINT ( 'NONE',  ( 1.400715809426569702, 1.493624456287694358, -1.049586478250638999 ) ) ;
#173328 = CARTESIAN_POINT ( 'NONE',  ( -4.911796789900812144, 8.952456364851418158, 0.7998128361456291469 ) ) ;
#173329 = CARTESIAN_POINT ( 'NONE',  ( -5.306037014901836990, 7.283738832175834510, 1.599625672291263401 ) ) ;
#173330 = CARTESIAN_POINT ( 'NONE',  ( -10.57368757801325820, 3.061359382655743033, 7.009609602318408683 ) ) ;
#173331 = EDGE_LOOP ( 'NONE', ( #102369, #59673, #212378 ) ) ;
#173332 = CARTESIAN_POINT ( 'NONE',  ( 5.348532861604016198, 0.5962098156395375659, 1.972770010162463228 ) ) ;
#173333 = CARTESIAN_POINT ( 'NONE',  ( -6.197485614778184271, 9.284131412999601096, 1.082531754730549967 ) ) ;
#173334 = CARTESIAN_POINT ( 'NONE',  ( 3.212919216758630014, 6.692230152952963529, 0.000000000000000000 ) ) ;
#173335 = CARTESIAN_POINT ( 'NONE',  ( -4.765854690403601879, 5.518917546014321829, 1.199719254218462483 ) ) ;
#173336 = CARTESIAN_POINT ( 'NONE',  ( -3.318713740295064163, 7.093859473644694269, 0.000000000000000000 ) ) ;
#173337 = CARTESIAN_POINT ( 'NONE',  ( 4.108072977939541737, -0.7709450260172491243, 1.866947522544240901 ) ) ;
#173338 = CARTESIAN_POINT ( 'NONE',  ( 6.252596820807392319, 2.196675488376065744, 0.3289990992049235397 ) ) ;
#173340 = CARTESIAN_POINT ( 'NONE',  ( 7.700668062882064291, 10.00719871149432549, -1.443375672974057666 ) ) ;
#173339 = CARTESIAN_POINT ( 'NONE',  ( -4.462568837553487100, 5.235360394347691404, -1.199719254218453823 ) ) ;
#173341 = CARTESIAN_POINT ( 'NONE',  ( 7.156006149914539982, 7.243095351188763686, 1.040834085586084257E-14 ) ) ;
#173342 = CARTESIAN_POINT ( 'NONE',  ( 4.012614562483146408, 1.458688259485216854, -1.456115939812257620 ) ) ;
#173343 = CARTESIAN_POINT ( 'NONE',  ( 4.500625067706437221, -1.976956227568788638, 0.3961002554062897918 ) ) ;
#173344 = ORIENTED_EDGE ( 'NONE', *, *, #157926, .F. ) ;
#173345 = CARTESIAN_POINT ( 'NONE',  ( 1.908029163539552098, 3.237038651130924372, -0.4603255239806359200 ) ) ;
#173346 = CARTESIAN_POINT ( 'NONE',  ( 3.655894977179307226, 7.416961240017848844, -0.7998128361456291469 ) ) ;
#173348 = ORIENTED_EDGE ( 'NONE', *, *, #35731, .F. ) ;
#173347 = CARTESIAN_POINT ( 'NONE',  ( -6.420668264523499147, 9.648474187656182366, 1.199719254218452935 ) ) ;
#173349 = CARTESIAN_POINT ( 'NONE',  ( 5.551963943121584144, 7.421064284658021037, -1.246246109899084020 ) ) ;
#173350 = B_SPLINE_CURVE_WITH_KNOTS ( 'NONE', 3,
 ( #133694, #103290, #201821, #136866, #104364, #154179 ),
 .UNSPECIFIED., .F., .F.,
 ( 4, 2, 4 ),
 ( 0.001369432773569654585, 0.001631688116371318026, 0.001893943459172981250 ),
 .UNSPECIFIED. ) ;
#173351 = CARTESIAN_POINT ( 'NONE',  ( 3.725935337077026510, -1.776739457207517248, -0.9528653653038119398 ) ) ;
#173352 = CARTESIAN_POINT ( 'NONE',  ( 2.273173984786102775, 1.132353773513800510, 1.451651336590239927 ) ) ;
#173353 = CARTESIAN_POINT ( 'NONE',  ( 1.348709242277994269, 2.305235852375675076, 0.1091458774659745806 ) ) ;
#173354 = CARTESIAN_POINT ( 'NONE',  ( 7.614839552730775729, 8.913009562054615031, 1.199719254218452047 ) ) ;
#173355 = CARTESIAN_POINT ( 'NONE',  ( 3.497504216883956296, 1.701635573755799324, 1.332874705691905248 ) ) ;
#173356 = CARTESIAN_POINT ( 'NONE',  ( 8.585337585951586803, 11.03931315507545108, -1.599625672291255185 ) ) ;
#173357 = CARTESIAN_POINT ( 'NONE',  ( -5.982172092127739482, 8.002286745614243912, -1.599625672291263179 ) ) ;
#173358 = AXIS2_PLACEMENT_3D ( 'NONE', #40503, #107691, #88172 ) ;
#173359 = CARTESIAN_POINT ( 'NONE',  ( -9.030096778091493803, 1.000000000000000888, -7.742171412064445590 ) ) ;
#173360 = CARTESIAN_POINT ( 'NONE',  ( 2.149089010626914931, -1.500894351328721621, -1.116326037436713881 ) ) ;
#173361 = CARTESIAN_POINT ( 'NONE',  ( 5.313337694394675736, -0.2901137614541632881, 1.949896409304814116 ) ) ;
#173363 = CARTESIAN_POINT ( 'NONE',  ( 7.687109908824030668, 10.95175007939464606, -1.082531754730543083 ) ) ;
#173362 = CARTESIAN_POINT ( 'NONE',  ( -1.201851678989727383E-14, 4.071875000341425022, 1.575800808251672791 ) ) ;
#173365 = CARTESIAN_POINT ( 'NONE',  ( 0.2236267563471248943, -0.1037379595543522215, 2.204571545119632603 ) ) ;
#173364 = CARTESIAN_POINT ( 'NONE',  ( -4.564291269294938225, 8.476756914152748124, 1.040834085586084257E-14 ) ) ;
#173366 = LINE ( 'NONE', #5477, #185310 ) ;
#173367 = CARTESIAN_POINT ( 'NONE',  ( 3.655894977179307226, 7.416961240017848844, -0.7998128361456291469 ) ) ;
#173368 = CARTESIAN_POINT ( 'NONE',  ( -6.261168011412601153, 6.199117522936475666, 1.040834085586084257E-14 ) ) ;
#173369 = CARTESIAN_POINT ( 'NONE',  ( 3.001021497710600006, 6.452383585894986062, 0.2530183522923339923 ) ) ;
#173370 = CARTESIAN_POINT ( 'NONE',  ( 6.192255011402767018, -1.961924197356275323, -0.1938383548326528261 ) ) ;
#173371 = CARTESIAN_POINT ( 'NONE',  ( 5.672612835131308984, -1.468196381517340665, 1.780430754307258390 ) ) ;
#173372 = CARTESIAN_POINT ( 'NONE',  ( 6.812964112091245639, -1.437450002374938585, 1.181853997439401116 ) ) ;
#173373 = CARTESIAN_POINT ( 'NONE',  ( 3.116140835343351956, 2.053043485406472080, -0.1977005638095686579 ) ) ;
#173374 = CARTESIAN_POINT ( 'NONE',  ( 6.100805936469477331, 9.101062111647635788, -1.082531754730537088 ) ) ;
#173375 = EDGE_CURVE ( 'NONE', #90486, #157709, #55963, .T. ) ;
#173376 = CARTESIAN_POINT ( 'NONE',  ( 2.898410978271408922, 6.603506251283770112, -0.7998128361456362523 ) ) ;
#173377 = CARTESIAN_POINT ( 'NONE',  ( 5.924549939047454750, 9.855799328956630134, -0.7216878364870267237 ) ) ;
#173378 = CARTESIAN_POINT ( 'NONE',  ( -0.6823417656250212460, 3.863541667008085767, 1.181850606188767472 ) ) ;
#173379 = CARTESIAN_POINT ( 'NONE',  ( -6.689742616953707532, 14.55216527438033225, 9.919101817088241901 ) ) ;
#173380 = CARTESIAN_POINT ( 'NONE',  ( 5.477130869796502211, 5.492333557625114437, 1.040834085586084257E-14 ) ) ;
#173382 = CARTESIAN_POINT ( 'NONE',  ( 3.028530041973789722, 0.4946322284519070189, 1.954779462066410733 ) ) ;
#173381 = CARTESIAN_POINT ( 'NONE',  ( 5.529782829607038153, 2.093976201882574273, -0.5736635526294631138 ) ) ;
#173384 = CARTESIAN_POINT ( 'NONE',  ( 5.390138975101268493, -0.4531076923771395482, -1.784498753146485539 ) ) ;
#173383 = CARTESIAN_POINT ( 'NONE',  ( 9.305047017613608418, 3.481540744127370690, -7.450000000000005507 ) ) ;
#173386 = CARTESIAN_POINT ( 'NONE',  ( 6.720655732516684466, 7.052972427687314472, 2.524416814197846914 ) ) ;
#173385 = CARTESIAN_POINT ( 'NONE',  ( -1.201851678989727383E-14, 5.446875000341422357, -1.575800808251660134 ) ) ;
#173387 = CARTESIAN_POINT ( 'NONE',  ( 6.444889499930222421, -1.758869480593090673, -1.307235502039267860 ) ) ;
#173388 = CARTESIAN_POINT ( 'NONE',  ( -11.92045683181315674, 9.947240721205131919, 1.382340670101856350 ) ) ;
#173389 = CARTESIAN_POINT ( 'NONE',  ( 6.789870067575622947, -0.9739125386618008307, 2.039881742057749303 ) ) ;
#173390 = CARTESIAN_POINT ( 'NONE',  ( -4.597746731904842399, 7.146551969360384504, -1.363588915232381904 ) ) ;
#173391 = CARTESIAN_POINT ( 'NONE',  ( 3.023105066167310895, 5.702484939155337607, 2.420000000000000373 ) ) ;
#173392 = CARTESIAN_POINT ( 'NONE',  ( 6.606300428615679898, 6.765996464729716386, -0.04887194053871009303 ) ) ;
#173393 = CARTESIAN_POINT ( 'NONE',  ( -4.950135482320929370, 5.908151163196758482, -1.082531754730549967 ) ) ;
#173394 = CARTESIAN_POINT ( 'NONE',  ( 0.3637282827039616251, 0.5997036651611362679, -1.815894722023647656 ) ) ;
#173395 = PRODUCT_DEFINITION_FORMATION_WITH_SPECIFIED_SOURCE ( 'ANY', '', #199001, .NOT_KNOWN. ) ;
#173396 = CARTESIAN_POINT ( 'NONE',  ( 1.938023551401172773, 1.750023271871611996, 0.2632672158595899536 ) ) ;
#173397 = AXIS2_PLACEMENT_3D ( 'NONE', #72611, #189569, #5453 ) ;
#173398 = CARTESIAN_POINT ( 'NONE',  ( 5.953776513178359764, -1.459723235216038750, -1.386512712134661207 ) ) ;
#173399 = CARTESIAN_POINT ( 'NONE',  ( 5.579168075997259280, -0.04836659121091852614, -2.105573489274599197 ) ) ;
#173401 = CARTESIAN_POINT ( 'NONE',  ( 3.356958492073054412, 0.04375785802200299335, -1.915270648069177462 ) ) ;
#173400 = CARTESIAN_POINT ( 'NONE',  ( -4.406036734316906234, 4.242723732898890709, -0.7216878364870207285 ) ) ;
#173402 = VECTOR ( 'NONE', #87104, 1000.000000000000000 ) ;
#173403 = DIRECTION ( 'NONE',  ( 0.000000000000000000, 1.000000000000000000, 0.000000000000000000 ) ) ;
#173404 = CARTESIAN_POINT ( 'NONE',  ( 3.824621415324851892, -1.324631885467566716, 1.457714561274085163 ) ) ;
#173405 = CARTESIAN_POINT ( 'NONE',  ( 0.08834397731360790762, 1.226219587655341448, 1.729930300845914815 ) ) ;
#173406 = CARTESIAN_POINT ( 'NONE',  ( -4.322352044658376968, 3.937165561723182883, 0.7998128361456341429 ) ) ;
#173407 = CARTESIAN_POINT ( 'NONE',  ( 2.395189659270926086, 1.444574673180216706, 1.188490415850687265 ) ) ;
#173409 = ORIENTED_EDGE ( 'NONE', *, *, #3142, .F. ) ;
#173408 = CARTESIAN_POINT ( 'NONE',  ( 5.338411986983877533, 1.700291985010034201, 0.2892061366746317419 ) ) ;
#173411 = CARTESIAN_POINT ( 'NONE',  ( 5.178851490740205676, 6.104710163027444736, 1.082531754730558626 ) ) ;
#173410 = CARTESIAN_POINT ( 'NONE',  ( 2.174722684859807575, -1.356406721008751814, 1.740749382485320407 ) ) ;
#173412 = CARTESIAN_POINT ( 'NONE',  ( -0.6823417656250212460, 2.863541667008084879, 1.181850606188767472 ) ) ;
#173413 = CARTESIAN_POINT ( 'NONE',  ( 6.584431417889404337, 1.130572321132311098, -1.603143135845342515 ) ) ;
#173414 = CARTESIAN_POINT ( 'NONE',  ( 6.751070424600909448, 9.963667031088037973, -1.199719254218441611 ) ) ;
#173415 = FACE_OUTER_BOUND ( 'NONE', #126622, .T. ) ;
#173416 = CARTESIAN_POINT ( 'NONE',  ( 1.458833446111210685, 8.740432391875497586, 2.548463833528534561 ) ) ;
#173417 = CARTESIAN_POINT ( 'NONE',  ( -4.334856428067329404, 6.080418470877079429, -1.599625672291256517 ) ) ;
#173418 = CARTESIAN_POINT ( 'NONE',  ( 3.023105066167310895, 5.702484939155337607, 2.420000000000000373 ) ) ;
#173419 = ORIENTED_EDGE ( 'NONE', *, *, #181736, .F. ) ;
#173420 = CARTESIAN_POINT ( 'NONE',  ( 1.504437137538238600, 2.067909592606699487, 0.1035681241481553605 ) ) ;
#173421 = CARTESIAN_POINT ( 'NONE',  ( -0.7500000000000215383, 2.941666666666689522, 1.299038105676671107 ) ) ;
#173422 = CARTESIAN_POINT ( 'NONE',  ( 6.484877546038077867, 6.460111979999551224, 1.040834085586084257E-14 ) ) ;
#173423 = CARTESIAN_POINT ( 'NONE',  ( 4.309512724297349884, 6.121127159803966933, 1.599625672291261402 ) ) ;
#173424 = CARTESIAN_POINT ( 'NONE',  ( 0.1178396879437521028, -0.5365784638422869124, 1.947031292057841645 ) ) ;
#173425 = DIRECTION ( 'NONE',  ( -0.9989735196462991018, -4.834648123959315881E-16, 0.04529798058948755063 ) ) ;
#173426 = EDGE_CURVE ( 'NONE', #38781, #96770, #11106, .T. ) ;
#173427 = CARTESIAN_POINT ( 'NONE',  ( -1.364683531250012516, 4.238541667008090208, -0.7879004041258300672 ) ) ;
#173428 = EDGE_LOOP ( 'NONE', ( #72326, #129167 ) ) ;
#173430 = CARTESIAN_POINT ( 'NONE',  ( 8.378575743565351175, 11.75846021992619406, -1.082531754730543083 ) ) ;
#173429 = DIRECTION ( 'NONE',  ( -0.000000000000000000, 1.000000000000000000, -0.000000000000000000 ) ) ;
#173431 = CARTESIAN_POINT ( 'NONE',  ( 5.870470189955956819, -0.4925641237488035395, 1.954873771647095415 ) ) ;
#173432 = CARTESIAN_POINT ( 'NONE',  ( 4.364398177449787752, -1.859642558872817375, -0.4596742015197906595 ) ) ;
#173433 = CARTESIAN_POINT ( 'NONE',  ( 9.499606442108964544, -9.746166700193986898, -0.08647222121513538362 ) ) ;
#173434 = CARTESIAN_POINT ( 'NONE',  ( 2.665787806004876970, 1.174844384069907655, 1.849873475113596566 ) ) ;
#173435 =( BOUNDED_SURFACE ( )  B_SPLINE_SURFACE ( 3, 2, ( 
 ( #210738, #46136, #202994 ),
 ( #201914, #1586, #104465 ),
 ( #53567, #37313, #186759 ),
 ( #2652, #120781, #103388 ),
 ( #118633, #167327, #185684 ),
 ( #68726, #135896, #84997 ) ),
 .UNSPECIFIED., .F., .F., .T. ) 
 B_SPLINE_SURFACE_WITH_KNOTS ( ( 4, 2, 4 ),
 ( 3, 3 ),
 ( 8.104322365865941288E-05, 0.0002156911409636899451, 0.0003503390582687204908 ),
 ( 0.000000000000000000, 1.000000000000000000 ),
 .UNSPECIFIED. ) 
 GEOMETRIC_REPRESENTATION_ITEM ( )  RATIONAL_B_SPLINE_SURFACE ( (
 ( 1.000000000000000000, 0.8104931255418998948, 1.000000000000000000),
 ( 1.000000000000000000, 0.8505897838741076633, 1.000000000000000000),
 ( 1.000000000000000000, 0.8859283899323100453, 1.000000000000000000),
 ( 1.000000000000000000, 0.9158911669205149764, 1.000000000000000000),
 ( 1.000000000000000000, 0.9074584363678738219, 1.000000000000000000),
 ( 1.000000000000000000, 0.8789000212895043962, 1.000000000000000000) ) ) 
 REPRESENTATION_ITEM ( '' )  SURFACE ( )  );
#173436 = CARTESIAN_POINT ( 'NONE',  ( 0.7499999999999885647, 2.097916667349486453, -1.299038105676652899 ) ) ;
#173437 = CARTESIAN_POINT ( 'NONE',  ( 2.689602200614676697, 1.814610489020528350, -0.6038049036062518304 ) ) ;
#173438 = CARTESIAN_POINT ( 'NONE',  ( -4.557512192488103686, 8.468847991211438497, -0.7998128361456281477 ) ) ;
#173439 = EDGE_CURVE ( 'NONE', #75117, #211313, #11021, .T. ) ;
#173441 = CARTESIAN_POINT ( 'NONE',  ( 6.362923164919582319, -0.1041218986313949546, -2.114803170081226646 ) ) ;
#173440 = CARTESIAN_POINT ( 'NONE',  ( 0.07999999999999327094, -9.900000000000005684, 9.579665964948873125 ) ) ;
#173442 = CARTESIAN_POINT ( 'NONE',  ( -1.402160292154681736E-14, 9.984375000341401574, 1.575800808251682339 ) ) ;
#173444 = CARTESIAN_POINT ( 'NONE',  ( -7.130662446144611977, 7.283804040115648526, 0.000000000000000000 ) ) ;
#173443 = CARTESIAN_POINT ( 'NONE',  ( 5.601184584505256581, -0.5335315006234629953, 2.125516261704554211 ) ) ;
#173446 = ORIENTED_EDGE ( 'NONE', *, *, #166273, .T. ) ;
#173445 = CARTESIAN_POINT ( 'NONE',  ( 2.713528120726243831, -1.706327644498882634, 0.2505720552260106149 ) ) ;
#173447 = CARTESIAN_POINT ( 'NONE',  ( -1.403658749385957139, -1.209764585679680593, 1.481909061747194167 ) ) ;
#173448 = CARTESIAN_POINT ( 'NONE',  ( 4.416205349749311004, 6.175325546172740765, 1.599625672291267398 ) ) ;
#173449 = DIRECTION ( 'NONE',  ( -0.9999980456341538426, 0.000000000000000000, -0.001977050295958626691 ) ) ;
#173450 = PLANE ( 'NONE',  #86125 ) ;
#173451 = CARTESIAN_POINT ( 'NONE',  ( 0.000000000000000000, 3.553060279300227275, 0.000000000000000000 ) ) ;
#173452 = CARTESIAN_POINT ( 'NONE',  ( 4.157546660884947620, 8.002221537674429896, 1.040834085586084257E-14 ) ) ;
#173453 = CARTESIAN_POINT ( 'NONE',  ( 4.000000000000012434, 0.000000000000000000, 0.7500000000000006661 ) ) ;
#173454 = VERTEX_POINT ( 'NONE', #27278 ) ;
#173455 = DIRECTION ( 'NONE',  ( 0.000000000000000000, 0.000000000000000000, 1.000000000000000000 ) ) ;
#173456 = VERTEX_POINT ( 'NONE', #14208 ) ;
#173457 = CARTESIAN_POINT ( 'NONE',  ( 3.228980503213836339, 1.638859372766150679, 0.7719998214037685491 ) ) ;
#173458 = ORIENTED_EDGE ( 'NONE', *, *, #201653, .F. ) ;
#173459 = CARTESIAN_POINT ( 'NONE',  ( 8.540746701604824409, 12.05162268759261224, -1.199719254218446718 ) ) ;
#173460 = CARTESIAN_POINT ( 'NONE',  ( 5.435893244436359240, 5.306573304789342416, -0.7998128361456481317 ) ) ;
#173461 = CARTESIAN_POINT ( 'NONE',  ( 4.143061475816012695, 0.09292765117045087564, 1.809223169447377710 ) ) ;
#173462 = CARTESIAN_POINT ( 'NONE',  ( 0.4841688312534724870, 3.595529751363280457, -0.4351271339793956749 ) ) ;
#173463 = CARTESIAN_POINT ( 'NONE',  ( -10.99861980075107759, -8.407420853759271395, 0.1919816227428516597 ) ) ;
#173464 = CARTESIAN_POINT ( 'NONE',  ( 5.869075745953527878, 5.991122463535357490, 0.2593076673842714119 ) ) ;
#173465 = VERTEX_POINT ( 'NONE', #143223 ) ;
#173466 = EDGE_CURVE ( 'NONE', #1301, #107467, #204663, .T. ) ;
#173468 = CARTESIAN_POINT ( 'NONE',  ( 0.6823417656249969321, 14.27604166700806232, -1.181850606188757036 ) ) ;
#173467 = CARTESIAN_POINT ( 'NONE',  ( 4.685918305224146430, -1.144368955370359098, -1.467557204495354872 ) ) ;
#173469 = CARTESIAN_POINT ( 'NONE',  ( 1.476048981871850518, -1.906537803873010084, -0.1858940877890648546 ) ) ;
#173470 = CARTESIAN_POINT ( 'NONE',  ( 1.219449367515994309, -1.782015241123528826, 0.3957228718986585680 ) ) ;
#173471 = CARTESIAN_POINT ( 'NONE',  ( -6.486624235763164492, 6.835203243035253173, 0.7121179707554707861 ) ) ;
#173472 = CARTESIAN_POINT ( 'NONE',  ( -10.57232049882948388, 5.599334429189661400, -4.968988939937085014 ) ) ;
#173474 = ADVANCED_FACE ( 'NONE', ( #85627 ), #170217, .T. ) ;
#173473 = AXIS2_PLACEMENT_3D ( 'NONE', #136903, #172606, #152081 ) ;
#173475 = CARTESIAN_POINT ( 'NONE',  ( 5.779562687394081522, 7.242644825714458001, 1.188994900607452054 ) ) ;
#173476 = CARTESIAN_POINT ( 'NONE',  ( 5.375100870188143531, 7.683496445330359137, 1.324677879948222392 ) ) ;
#173477 = CARTESIAN_POINT ( 'NONE',  ( -8.917737905728749581, 4.000000000000003553, -8.029567276306266876 ) ) ;
#173478 = CARTESIAN_POINT ( 'NONE',  ( -4.200340102501783690, 3.977070660044089934, 0.5078479924994099282 ) ) ;
#173479 = CARTESIAN_POINT ( 'NONE',  ( 8.134528978519385944, 8.592631351135175066, -0.7216878364870267237 ) ) ;
#173480 = CARTESIAN_POINT ( 'NONE',  ( 5.559413648769178096, 1.607788300429791262, 1.137107417019854072 ) ) ;
#173481 = CARTESIAN_POINT ( 'NONE',  ( -3.928111819657352566, 5.605883094398769195, 1.599625672291267398 ) ) ;
#173482 = DIRECTION ( 'NONE',  ( 0.000000000000000000, 1.000000000000000000, 0.000000000000000000 ) ) ;
#173483 = CARTESIAN_POINT ( 'NONE',  ( 0.9375778709549039691, 0.8456052968917522339, -1.912177616049218098 ) ) ;
#173484 = CARTESIAN_POINT ( 'NONE',  ( 0.2526013166088726392, -1.469656019175567208, 1.082793315970068004 ) ) ;
#173485 = CARTESIAN_POINT ( 'NONE',  ( -6.501298352952815662, 7.543601818988450169, -1.199719254218446718 ) ) ;
#173486 = CARTESIAN_POINT ( 'NONE',  ( 1.553431815599433108, 0.5335803070953272220, -1.745854899344486233 ) ) ;
#173487 = CARTESIAN_POINT ( 'NONE',  ( 2.877765823869771644, 2.095344539500657799, -0.6929138170133213315 ) ) ;
#173488 = CARTESIAN_POINT ( 'NONE',  ( 6.938893903907228378E-15, 10.64264068711930733, 1.214306433183764966E-14 ) ) ;
#173489 = CARTESIAN_POINT ( 'NONE',  ( 1.336036003918249948, -1.064896177285217016, -1.588262137521757822 ) ) ;
#173490 = ORIENTED_EDGE ( 'NONE', *, *, #48405, .T. ) ;
#173491 = CARTESIAN_POINT ( 'NONE',  ( 1.469134468336911192, 1.735519167469494084, 0.9312130504785380847 ) ) ;
#173492 = CARTESIAN_POINT ( 'NONE',  ( 2.560020840168964806, -1.337455066581024976, 1.408356088163305042 ) ) ;
#173493 = ORIENTED_EDGE ( 'NONE', *, *, #125681, .T. ) ;
#173494 = CARTESIAN_POINT ( 'NONE',  ( -10.62873463776380056, 13.79999999999999893, -3.200000000000001510 ) ) ;
#173496 = CARTESIAN_POINT ( 'NONE',  ( 6.227394082031683986, 0.1379007965640146050, -1.855924616290964169 ) ) ;
#173495 = CARTESIAN_POINT ( 'NONE',  ( -4.522526758610270647, 7.433975764090723359, -1.199719254218453823 ) ) ;
#173497 = CARTESIAN_POINT ( 'NONE',  ( 3.386504508363381571, 7.172948703057747011, -0.7998128361456362523 ) ) ;
#173498 = CARTESIAN_POINT ( 'NONE',  ( -11.41381678389388377, 13.52879418241074561, -3.704697885617973530 ) ) ;
#173499 = CARTESIAN_POINT ( 'NONE',  ( -7.828177403543865154, -5.742104877864245616, -7.727873494160012235 ) ) ;
#173500 = CARTESIAN_POINT ( 'NONE',  ( -5.906512197408906317, 6.919960980845699439, -1.199719254218453823 ) ) ;
#173501 = CARTESIAN_POINT ( 'NONE',  ( 2.648187065138879692, 0.7411268365287645432, 2.062558662443473523 ) ) ;
#173502 = CARTESIAN_POINT ( 'NONE',  ( 3.768803514918948938, 4.459654191235965293, -1.082531754730543083 ) ) ;
#173503 = CIRCLE ( 'NONE', #204518, 0.8300000000000008482 ) ;
#173504 = CARTESIAN_POINT ( 'NONE',  ( 5.363132282657546490, 8.414682208812571673, -1.199719254218452047 ) ) ;
#173506 = CARTESIAN_POINT ( 'NONE',  ( 5.876185452347599814, -2.007255679753978228, -0.1928398672442974138 ) ) ;
#173505 = CARTESIAN_POINT ( 'NONE',  ( 3.000428103051573814, -0.5303778429210231904, -1.746945217264872507 ) ) ;
#173507 = DIRECTION ( 'NONE',  ( 0.000000000000000000, 0.000000000000000000, -1.000000000000000000 ) ) ;
#173508 = CARTESIAN_POINT ( 'NONE',  ( -9.490344339885973923, 12.09515436799890331, -1.443375672974059665 ) ) ;
#173509 = CARTESIAN_POINT ( 'NONE',  ( -5.281148723220589147, 7.765029056575591504, -1.308346332658766986 ) ) ;
#173510 = LINE ( 'NONE', #25083, #212530 ) ;
#173511 = CARTESIAN_POINT ( 'NONE',  ( 7.404724451357931336, 11.79059562655963056, 0.7998128361456462443 ) ) ;
#173512 = CARTESIAN_POINT ( 'NONE',  ( 1.963383859451812041, 0.3296633872902128282, -1.897934821152784446 ) ) ;
#173513 = CARTESIAN_POINT ( 'NONE',  ( 5.700043108275813175, 0.7984002208856562088, -1.792138013221859394 ) ) ;
#173514 = CIRCLE ( 'NONE', #14370, 2.000000000000000000 ) ;
#173515 = CARTESIAN_POINT ( 'NONE',  ( 1.499999999999997113, 14.89583333333333570, -0.8660254037844378194 ) ) ;
#173516 = CARTESIAN_POINT ( 'NONE',  ( -6.958359152311683893, 9.141171649162195934, -1.599625672291263179 ) ) ;
#173517 = CARTESIAN_POINT ( 'NONE',  ( 5.196852952739813070, 4.957416621151553571, -0.7998128361456221525 ) ) ;
#173518 = CARTESIAN_POINT ( 'NONE',  ( -4.136646265500964148, 6.879818838842817641, -1.082531754730551743 ) ) ;
#173519 = B_SPLINE_CURVE_WITH_KNOTS ( 'NONE', 3,
 ( #87829, #71550, #4402, #197560, #185306, #153899, #203678 ),
 .UNSPECIFIED., .F., .F.,
 ( 4, 3, 4 ),
 ( 0.000000000000000000, 7.109170824590711302E-05, 0.0001421874139631278545 ),
 .UNSPECIFIED. ) ;
#173520 = CARTESIAN_POINT ( 'NONE',  ( 10.16199982864259788, 11.81442020729326536, 1.199719254218452047 ) ) ;
#173521 = CARTESIAN_POINT ( 'NONE',  ( 2.969872605471105764, 6.605953636083951253, 0.1972538285620730192 ) ) ;
#173522 = CARTESIAN_POINT ( 'NONE',  ( 5.717656431054087385, 0.4094431674900833595, -2.029196096928844284 ) ) ;
#173524 = CARTESIAN_POINT ( 'NONE',  ( 1.364683531249988535, 2.926041667008082658, 0.7879004041258500513 ) ) ;
#173523 = DIRECTION ( 'NONE',  ( 0.000000000000000000, -1.000000000000000000, -0.000000000000000000 ) ) ;
#173525 = ORIENTED_EDGE ( 'NONE', *, *, #82593, .F. ) ;
#173526 = CARTESIAN_POINT ( 'NONE',  ( 4.992985585870878928, -2.287786813913486039, 0.2239274308311194894 ) ) ;
#173527 = CARTESIAN_POINT ( 'NONE',  ( 6.561783159334121152, 8.678499657355050800, -1.443375672974057666 ) ) ;
#173529 = CARTESIAN_POINT ( 'NONE',  ( -11.04536101718726293, 0.000000000000000000, 1.099999999999996758 ) ) ;
#173528 = CARTESIAN_POINT ( 'NONE',  ( 5.560252395380215873, 6.619954228432645138, 1.082531754730549078 ) ) ;
#173530 = CARTESIAN_POINT ( 'NONE',  ( 6.515150198369638268, -2.224820657066893137, 0.5519656782505685255 ) ) ;
#173531 = CARTESIAN_POINT ( 'NONE',  ( 5.045036709957831711, 4.903268083610561767, 0.3063280728123271568 ) ) ;
#173532 = CARTESIAN_POINT ( 'NONE',  ( -7.435720902452096936, 7.639705572474380091, 0.000000000000000000 ) ) ;
#173533 = CARTESIAN_POINT ( 'NONE',  ( 5.455005553751488989, 0.3768678912985870544, -1.904869181234331910 ) ) ;
#173534 = ORIENTED_EDGE ( 'NONE', *, *, #120795, .F. ) ;
#173535 = CARTESIAN_POINT ( 'NONE',  ( 8.880227426826634129, 11.38335130276301754, 1.443375672974076540 ) ) ;
#173536 = EDGE_LOOP ( 'NONE', ( #178853, #135172, #205470, #39310 ) ) ;
#173537 = CARTESIAN_POINT ( 'NONE',  ( 6.029550621839829816, -0.2273517531893587407, 1.898748578088353733 ) ) ;
#173538 = CARTESIAN_POINT ( 'NONE',  ( 6.176716277887216222, -1.639393978788429740, -0.5360894954027517478 ) ) ;
#173539 = CARTESIAN_POINT ( 'NONE',  ( 5.876185452347599814, -2.007255679753978228, -0.1928398672442974138 ) ) ;
#173541 = CARTESIAN_POINT ( 'NONE',  ( 3.449892483197225523, 6.324475487839650967, -1.000715626366242450 ) ) ;
#173540 = CARTESIAN_POINT ( 'NONE',  ( -8.748035429315585532, 11.22912730566677553, -1.599625672291263179 ) ) ;
#173542 = CARTESIAN_POINT ( 'NONE',  ( 3.285556943749998737, -2.092708332855377051, -1.896917185911906500 ) ) ;
#173544 = CARTESIAN_POINT ( 'NONE',  ( 0.09216213259799833912, -0.3764253007602496592, -1.735191564994809976 ) ) ;
#173543 = CARTESIAN_POINT ( 'NONE',  ( 1.728581982081365265, 0.2060769881795926906, 2.080452860985905428 ) ) ;
#173545 = DIRECTION ( 'NONE',  ( -0.000000000000000000, 1.000000000000000000, -0.000000000000000000 ) ) ;
#173547 = CARTESIAN_POINT ( 'NONE',  ( 3.820531118927258607, 2.176299813863972865, 0.7200661129266039406 ) ) ;
#173546 = CARTESIAN_POINT ( 'NONE',  ( 3.074666975249065626, 6.809138247757705820, 0.000000000000000000 ) ) ;
#173548 = CARTESIAN_POINT ( 'NONE',  ( 2.097218849865792212, -1.740012409040556429, 0.04131442251954255129 ) ) ;
#173549 = CARTESIAN_POINT ( 'NONE',  ( 2.900754761704402274, -2.089926006748676457, -0.3584049868644647585 ) ) ;
#173550 = CARTESIAN_POINT ( 'NONE',  ( 1.743066579297358008E-15, 0.7500000006828128063, -1.225000000000021849 ) ) ;
#173551 = CARTESIAN_POINT ( 'NONE',  ( 2.301686711942134256, -1.551025276819127496, 0.7750448480700108389 ) ) ;
#173552 = CARTESIAN_POINT ( 'NONE',  ( 0.6801582343749900117, 2.005208333674748822, 1.178068619123818994 ) ) ;
#173553 = CARTESIAN_POINT ( 'NONE',  ( 6.333220217719927270, -1.622483202430196725, -1.197309987464048486 ) ) ;
#173554 = CARTESIAN_POINT ( 'NONE',  ( 1.978732740145513480, 1.735006779315110492, 0.6737207639663128633 ) ) ;
#173555 = CARTESIAN_POINT ( 'NONE',  ( 2.682273331476907607, -1.248350377418592672, -1.776241996044833238 ) ) ;
#173556 = CARTESIAN_POINT ( 'NONE',  ( 6.796715079152391148, 6.823922435299587974, 0.7998128361456341429 ) ) ;
#173557 = CARTESIAN_POINT ( 'NONE',  ( 3.731657894805060938, 0.6748485617756972976, -1.900415309456899182 ) ) ;
#173558 = CARTESIAN_POINT ( 'NONE',  ( 3.312500000000002220, 1.451031289061251339, 1.451031289060983998 ) ) ;
#173559 = VECTOR ( 'NONE', #86472, 1000.000000000000000 ) ;
#173560 = CARTESIAN_POINT ( 'NONE',  ( -1.201851678989727383E-14, 3.243750000682814161, 1.732050807568877637 ) ) ;
#173561 = CARTESIAN_POINT ( 'NONE',  ( 0.9031967280443575774, 1.573137106080691572, 1.111599351221918663 ) ) ;
#173562 = CARTESIAN_POINT ( 'NONE',  ( -8.012344526598182026E-15, 14.29687500034139802, -1.575800808251669460 ) ) ;
#173563 = CARTESIAN_POINT ( 'NONE',  ( 4.324628213192062809, -0.9515899357304625772, -2.007430035002121471 ) ) ;
#173564 = ORIENTED_EDGE ( 'NONE', *, *, #128408, .F. ) ;
#173566 = AXIS2_PLACEMENT_3D ( 'NONE', #142081, #208096, #204879 ) ;
#173565 = FACE_OUTER_BOUND ( 'NONE', #185391, .T. ) ;
#173567 = CARTESIAN_POINT ( 'NONE',  ( 1.499999999999989120, 0.7750000000000187850, 0.000000000000000000 ) ) ;
#173568 = CARTESIAN_POINT ( 'NONE',  ( 5.940443861082012944, 10.08226827123770697, 0.7998128361456462443 ) ) ;
#173569 = CARTESIAN_POINT ( 'NONE',  ( 0.6823417656249882723, -0.6572916663252492686, 1.181850606188755259 ) ) ;
#173570 = CARTESIAN_POINT ( 'NONE',  ( 5.783471039277606529, 0.1639875503032099946, -2.215378355603670357 ) ) ;
#173572 = ADVANCED_FACE ( 'NONE', ( #166891 ), #98707, .T. ) ;
#173571 = CARTESIAN_POINT ( 'NONE',  ( 5.072687121480487171, 1.354251660176824856, -1.419695456575476689 ) ) ;
#173573 = PRODUCT_DEFINITION ( 'UNKNOWN', '', #107729, #130654 ) ;
#173575 = CARTESIAN_POINT ( 'NONE',  ( -5.070386261830872598, 8.859275038870594088, 0.7216878364870458196 ) ) ;
#173574 = CARTESIAN_POINT ( 'NONE',  ( 9.300530189294644146, 10.91333531134101165, -1.082531754730543083 ) ) ;
#173576 = CARTESIAN_POINT ( 'NONE',  ( -1.286813488861816790, 3.652992958535466794, -0.4595522011843584109 ) ) ;
#173577 = CARTESIAN_POINT ( 'NONE',  ( 5.870491743106223126, -1.441790217864300283, 1.743476569090945061 ) ) ;
#173578 = CARTESIAN_POINT ( 'NONE',  ( -5.316205630334255972, 8.255971431148344308, -1.082531754730549967 ) ) ;
#173579 = CARTESIAN_POINT ( 'NONE',  ( 3.227062719040986405, -1.904794013395166186, -0.7919108894221676964 ) ) ;
#173580 = CARTESIAN_POINT ( 'NONE',  ( -4.706651882238427120, 8.642844295920152575, 1.040834085586084257E-14 ) ) ;
#173581 = ORIENTED_EDGE ( 'NONE', *, *, #61620, .F. ) ;
#173582 = CARTESIAN_POINT ( 'NONE',  ( -0.7500000000000006661, 2.889583334016148974, -1.299038105676652011 ) ) ;
#173583 = CARTESIAN_POINT ( 'NONE',  ( 1.364683531249990311, 4.446875000341417028, 1.214306433183764966E-14 ) ) ;
#173584 = CARTESIAN_POINT ( 'NONE',  ( 4.938664768831325880, 0.3182328507864223277, 1.843102042236575588 ) ) ;
#173585 = CARTESIAN_POINT ( 'NONE',  ( 3.164447786964882603, 1.103041557463914524, 1.338080049202054145 ) ) ;
#173586 = CARTESIAN_POINT ( 'NONE',  ( 1.979654113181174901, -1.706931329119738772, -0.3388794841660112689 ) ) ;
#173587 = CARTESIAN_POINT ( 'NONE',  ( 0.7852321044731135347, 2.018311417075705272, -1.086964541883679303 ) ) ;
#173588 = CARTESIAN_POINT ( 'NONE',  ( 1.395868886378356821, 1.671639904693554168, 1.440724375100350008 ) ) ;
#173589 = CARTESIAN_POINT ( 'NONE',  ( 4.159774813393120496, 0.9870934738810345221, 1.843074783240926884 ) ) ;
#173590 = CARTESIAN_POINT ( 'NONE',  ( 6.105412738798914773, -1.926975682693391700, 0.2402159021005992046 ) ) ;
#173592 = ORIENTED_EDGE ( 'NONE', *, *, #41976, .T. ) ;
#173591 = DIRECTION ( 'NONE',  ( -1.000000000000000000, -3.451266460341926211E-31, -8.638326563840810896E-31 ) ) ;
#173593 = FILL_AREA_STYLE ('',( #104298 ) ) ;
#173594 = CARTESIAN_POINT ( 'NONE',  ( 0.08851783505585240908, -0.5350849913869708541, 1.944072358963434555 ) ) ;
#173595 = DIRECTION ( 'NONE',  ( 0.000000000000000000, 1.000000000000000000, 0.000000000000000000 ) ) ;
#173596 = SURFACE_STYLE_USAGE ( .BOTH. , #190860 ) ;
#173597 = CARTESIAN_POINT ( 'NONE',  ( -8.829384350997580455, 11.32403438096243775, 1.599625672291269396 ) ) ;
#173598 = CARTESIAN_POINT ( 'NONE',  ( 6.174848896020108668, 9.291408581077091000, 1.199719254218460707 ) ) ;
#173599 = CARTESIAN_POINT ( 'NONE',  ( -10.95855051086948606, -7.723431457505092190, 0.6286713519884027379 ) ) ;
#173600 = CARTESIAN_POINT ( 'NONE',  ( 4.283705427790140519, 1.194290084605063251, 1.380960126487425166 ) ) ;
#173601 = CARTESIAN_POINT ( 'NONE',  ( 1.747397587315655088, -1.864034986486883039, 1.180896971623420999 ) ) ;
#173602 = ORIENTED_EDGE ( 'NONE', *, *, #100462, .T. ) ;
#173603 = CARTESIAN_POINT ( 'NONE',  ( -7.944151662964566540, 8.232874793072271657, 0.000000000000000000 ) ) ;
#173604 = CARTESIAN_POINT ( 'NONE',  ( 0.07933191752141914577, -7.643695121331862019, -9.499668754586256370 ) ) ;
#173605 = CARTESIAN_POINT ( 'NONE',  ( -3.285556943750000070, -2.296874999522042327, 0.000000000000000000 ) ) ;
#173606 = CARTESIAN_POINT ( 'NONE',  ( -6.021792782764022078, 10.17717534653336209, -0.7998128361456291469 ) ) ;
#173607 = CARTESIAN_POINT ( 'NONE',  ( 1.248313549685893475, 0.9916667988653109500, -1.759473928524292630 ) ) ;
#173608 = CARTESIAN_POINT ( 'NONE',  ( -1.878313713275499675, 13.99999999999846167, -12.68000002627077905 ) ) ;
#173609 = CARTESIAN_POINT ( 'NONE',  ( -4.390861645979385663, 6.216034235099629157, -1.599625672291271394 ) ) ;
#173610 = CARTESIAN_POINT ( 'NONE',  ( 2.676407432925419272, 1.219717815897247259, -1.405545362062944559 ) ) ;
#173611 = CARTESIAN_POINT ( 'NONE',  ( 3.460355519985863548, 5.060167411448709629, 1.599625672291267398 ) ) ;
#173612 = CARTESIAN_POINT ( 'NONE',  ( -1.499999999999997780, 5.431250000682820378, 1.214306433183764966E-14 ) ) ;
#173613 = ORIENTED_EDGE ( 'NONE', *, *, #115527, .F. ) ;
#173614 = CARTESIAN_POINT ( 'NONE',  ( -4.928552533767591726, 5.708731696605642725, 1.199719254218462483 ) ) ;
#173615 = CARTESIAN_POINT ( 'NONE',  ( -9.429859533504656000, 10.96025652963230534, -1.199719254218441611 ) ) ;
#173616 = CARTESIAN_POINT ( 'NONE',  ( 4.318856058802469811, 1.670182456744148336, 0.7377305746401884301 ) ) ;
#173618 = CARTESIAN_POINT ( 'NONE',  ( -3.999074104275988972, 7.816954204906529924, 0.3413819327131896175 ) ) ;
#173617 = CARTESIAN_POINT ( 'NONE',  ( -6.912678218121246942, 9.158153569265168770, 1.599625672291269396 ) ) ;
#173619 = CARTESIAN_POINT ( 'NONE',  ( 5.911136963822321455, 7.250628055112136039, -1.245581879728396846 ) ) ;
#173620 = CARTESIAN_POINT ( 'NONE',  ( 1.053531109644106678, 1.532759392139435128, -0.8104334526845609066 ) ) ;
#173621 = CARTESIAN_POINT ( 'NONE',  ( 5.788959344212086577, 1.397023377451442228, 1.199316859253784839 ) ) ;
#173622 = CARTESIAN_POINT ( 'NONE',  ( 4.828937647557053126, 2.207305988086407655, 0.6732806465959675357 ) ) ;
#173623 = CARTESIAN_POINT ( 'NONE',  ( 4.041212305325117882, 6.872442235258051646, -1.199719254218448494 ) ) ;
#173624 = CARTESIAN_POINT ( 'NONE',  ( 6.819591527820957566, -2.098570527662356522, 0.5178885164088961046 ) ) ;
#173625 = CARTESIAN_POINT ( 'NONE',  ( 7.318703993278529829, 7.432909501780090800, 1.040834085586084257E-14 ) ) ;
#173626 = CARTESIAN_POINT ( 'NONE',  ( 5.571695488097110349, 1.745893177897942738, -1.494929824115182937 ) ) ;
#173627 = CARTESIAN_POINT ( 'NONE',  ( 1.123270288254022198, 3.158552654332631882, -0.7749999999939810591 ) ) ;
#173628 = CARTESIAN_POINT ( 'NONE',  ( -5.589704470584107909, 9.743348658981940247, -0.7998128361456362523 ) ) ;
#173629 = CARTESIAN_POINT ( 'NONE',  ( 6.227412191919261986, -1.760757567598171480, 0.6321290105378990498 ) ) ;
#173630 = VERTEX_POINT ( 'NONE', #180822 ) ;
#173632 = CARTESIAN_POINT ( 'NONE',  ( -2.986538976760251263, 6.706322249520737522, -0.7998128361456481317 ) ) ;
#173631 = CARTESIAN_POINT ( 'NONE',  ( 2.091926199050548441, 1.179367891222588005, 1.505316542580182659 ) ) ;
#173633 = CARTESIAN_POINT ( 'NONE',  ( 4.336686996305870068, 2.164023489887345164, 0.4319772483800735086 ) ) ;
#173634 = CARTESIAN_POINT ( 'NONE',  ( 4.645784029343587918, 2.093824292288968270, -0.3141051717527267861 ) ) ;
#173635 = CARTESIAN_POINT ( 'NONE',  ( 0.6124999999999862776, 0.3958333340161462877, 1.060881119635934455 ) ) ;
#173636 = CARTESIAN_POINT ( 'NONE',  ( 6.883263157960391787, -0.001104538646235289417, 1.946037152736757925 ) ) ;
#173637 = CARTESIAN_POINT ( 'NONE',  ( 6.333067150914820864, 6.561202228921677815, 0.7216878364870328300 ) ) ;
#173638 = CARTESIAN_POINT ( 'NONE',  ( -4.462041952228942954, 8.219816354326809460, -0.7216878364870338292 ) ) ;
#173639 = CARTESIAN_POINT ( 'NONE',  ( 2.643975807074511408, -1.709602402607094396, -1.550068159870971574 ) ) ;
#173640 = CARTESIAN_POINT ( 'NONE',  ( 4.017981030900905637, 1.947309607215493621, -0.2378496960543720617 ) ) ;
#173641 = CARTESIAN_POINT ( 'NONE',  ( -4.610654757099099221, 7.536791762327691657, 1.199719254218452935 ) ) ;
#173642 = CARTESIAN_POINT ( 'NONE',  ( 6.121949867982135807, 2.033011618171334245, -0.3470327977990442792 ) ) ;
#173643 = CARTESIAN_POINT ( 'NONE',  ( 4.717874267875568961, 4.606534188717351874, -0.7216878364870188411 ) ) ;
#173644 = CARTESIAN_POINT ( 'NONE',  ( 3.715816618597135523, 6.492813934075403637, -1.199719254218453823 ) ) ;
#173645 = ORIENTED_EDGE ( 'NONE', *, *, #129564, .F. ) ;
#173646 = CARTESIAN_POINT ( 'NONE',  ( 6.192592252150040721, 1.490973663936447258, -1.357864438797616868 ) ) ;
#173647 = CARTESIAN_POINT ( 'NONE',  ( -10.30827686509187835, 10.92074451889568643, 1.040834085586084257E-14 ) ) ;
#173648 = CARTESIAN_POINT ( 'NONE',  ( -1.001543065824772872E-14, 4.212500000000023448, 1.732050807568877637 ) ) ;
#173649 = CARTESIAN_POINT ( 'NONE',  ( -10.78237064342727791, 6.270194388237658956, -4.501389708959286473 ) ) ;
#173650 = CARTESIAN_POINT ( 'NONE',  ( 8.934986926605834157, 10.38290515491702770, -1.199719254218446718 ) ) ;
#173651 = CARTESIAN_POINT ( 'NONE',  ( 1.885821443427546207, -2.045346407173433967, 0.7285060392495151804 ) ) ;
#173652 = CARTESIAN_POINT ( 'NONE',  ( 0.000000000000000000, 15.51845925587262798, 0.000000000000000000 ) ) ;
#173653 = CARTESIAN_POINT ( 'NONE',  ( -4.779943825041865324, 14.55303459918272679, -10.96777621109715462 ) ) ;
#173654 = CARTESIAN_POINT ( 'NONE',  ( -11.89942855770814134, 9.799999999999998934, -0.7000000000000009548 ) ) ;
#173655 = CARTESIAN_POINT ( 'NONE',  ( 4.749341595749815070, 8.305088035112140332, 0.7662636247844747395 ) ) ;
#173656 = CARTESIAN_POINT ( 'NONE',  ( 1.388040899126226302, -0.9290452130323262336, 1.839580399304826752 ) ) ;
#173657 = VECTOR ( 'NONE', #107542, 1000.000000000000000 ) ;
#173659 = CARTESIAN_POINT ( 'NONE',  ( 6.727182134110164746, 4.698490487241143043, 2.473633340027088678 ) ) ;
#173658 = CARTESIAN_POINT ( 'NONE',  ( -11.48243876534946040, 13.79999999999999893, -3.200000000000001510 ) ) ;
#173660 = CARTESIAN_POINT ( 'NONE',  ( -1.364683531250000748, 1.009375000341421247, 0.000000000000000000 ) ) ;
#173661 = CARTESIAN_POINT ( 'NONE',  ( 0.000000000000000000, 4.000000000000003553, 0.000000000000000000 ) ) ;
#173662 = ORIENTED_EDGE ( 'NONE', *, *, #83952, .T. ) ;
#173663 = CARTESIAN_POINT ( 'NONE',  ( 3.440010667329951310, -1.141173813254949820, -1.534285795567114974 ) ) ;
#173664 = CARTESIAN_POINT ( 'NONE',  ( 4.908955397393719444, 1.540865433829426090, 0.8705488387463419242 ) ) ;
#173665 = CARTESIAN_POINT ( 'NONE',  ( 6.713222337422018349, 7.861122810861019161, -1.199719254218452047 ) ) ;
#173666 = CARTESIAN_POINT ( 'NONE',  ( -5.251085567194491155, 5.020688004682002159, -0.7998128361456221525 ) ) ;
#173668 = CARTESIAN_POINT ( 'NONE',  ( 6.222283718431360633, 1.895538691748376081, 0.2756032664797089526 ) ) ;
#173667 = LINE ( 'NONE', #46860, #69902 ) ;
#173669 = CARTESIAN_POINT ( 'NONE',  ( 0.7499999999999867883, 0.3166666666666873020, -1.299038105676652899 ) ) ;
#173670 = CARTESIAN_POINT ( 'NONE',  ( 1.012269475826784060, 2.068064858651061932, -0.09981174449213289779 ) ) ;
#173671 = CARTESIAN_POINT ( 'NONE',  ( 1.499999999999990896, 5.775000000000023448, 1.040834085586084257E-14 ) ) ;
#173672 = CARTESIAN_POINT ( 'NONE',  ( 6.737182200980119440, -1.669782060861616291, 0.8434366901180423426 ) ) ;
#173673 = CARTESIAN_POINT ( 'NONE',  ( 3.387140609607977026, 1.650079954178599539, -0.7815607168924765258 ) ) ;
#173675 = CARTESIAN_POINT ( 'NONE',  ( 4.651083699394226834, 8.303454393088664176, 0.4639335724816190942 ) ) ;
#173674 = CARTESIAN_POINT ( 'NONE',  ( 5.918643953348324160, 1.484978324971843566, -1.632713241052483832 ) ) ;
#173676 = CARTESIAN_POINT ( 'NONE',  ( -0.6823417656250246877, 0.3010416670080895418, 1.181850606188755259 ) ) ;
#173677 = CARTESIAN_POINT ( 'NONE',  ( 2.699736158553706300, -1.526808845971421968, -1.387057796406083732 ) ) ;
#173678 = CARTESIAN_POINT ( 'NONE',  ( -7.739006755302186846, 7.923262724141010516, 0.7998128361456462443 ) ) ;
#173679 = CARTESIAN_POINT ( 'NONE',  ( 9.240045382913317340, 10.73880668727576015, -1.199719254218446718 ) ) ;
#173680 = CARTESIAN_POINT ( 'NONE',  ( 6.029140723994201423, 5.928419020948356710, -0.7090443702179377583 ) ) ;
#173681 = CARTESIAN_POINT ( 'NONE',  ( 0.6323695665565836066, 1.111747700424435159, -1.853661729306683936 ) ) ;
#173682 = CARTESIAN_POINT ( 'NONE',  ( 7.679767667498067496, 7.924426798361372093, 0.000000000000000000 ) ) ;
#173683 = CARTESIAN_POINT ( 'NONE',  ( 5.424307079040114665, 1.017280057988108499, 1.803113764695261523 ) ) ;
#173684 = CARTESIAN_POINT ( 'NONE',  ( 1.364683531249986537, -0.03229166632525094088, -0.7879004041258309554 ) ) ;
#173685 = CARTESIAN_POINT ( 'NONE',  ( 4.095124908492456584, 1.828510582809875107, -1.152538879107746439 ) ) ;
#173686 = CARTESIAN_POINT ( 'NONE',  ( -4.634775730458505549, 8.344889633747440527, 0.3497604727749434872 ) ) ;
#173688 = CARTESIAN_POINT ( 'NONE',  ( 2.137090596337941406, -0.09316805448006218460, -1.959763546484971197 ) ) ;
#173687 = CARTESIAN_POINT ( 'NONE',  ( 2.631515421131935817, -0.1955963300145530936, 2.010161875231412765 ) ) ;
#173689 = CARTESIAN_POINT ( 'NONE',  ( 6.620655732516625314, 7.629137130509059617, 2.773739711112707340 ) ) ;
#173692 = CARTESIAN_POINT ( 'NONE',  ( 7.131225611108100715, 7.422110755822004968, 0.7216878364870317197 ) ) ;
#173691 = CARTESIAN_POINT ( 'NONE',  ( 0.000000000000000000, -2.187499999999998668, -4.012584370867899430 ) ) ;
#173690 =( NAMED_UNIT ( * ) SI_UNIT ( $, .STERADIAN. ) SOLID_ANGLE_UNIT ( ) );
#173693 = CARTESIAN_POINT ( 'NONE',  ( -7.632314129850253259, 7.869064337772231355, 0.7998128361456341429 ) ) ;
#173694 = CARTESIAN_POINT ( 'NONE',  ( 1.270720652900014791, -0.3006520276036573902, -1.993892820393451615 ) ) ;
#173696 = CARTESIAN_POINT ( 'NONE',  ( 6.163654587501778970, 1.125051486859941718, 1.880622087419632882 ) ) ;
#173695 = CARTESIAN_POINT ( 'NONE',  ( -5.066996723205291708, 6.934582148538044777, 1.599625672291267398 ) ) ;
#173697 = CARTESIAN_POINT ( 'NONE',  ( -3.741063380996889620, 7.355675534244899616, 0.6276085112526242904 ) ) ;
#173698 = CARTESIAN_POINT ( 'NONE',  ( 5.449440537890919423, -1.726199344983204043, 0.8234401749890254418 ) ) ;
#173699 = CARTESIAN_POINT ( 'NONE',  ( -4.302014814237876017, 3.913438792899272212, 0.7998128361456341429 ) ) ;
#173700 = ADVANCED_FACE ( 'NONE', ( #32449 ), #83309, .T. ) ;
#173701 = CARTESIAN_POINT ( 'NONE',  ( 5.626270559546821204, 6.626699076635176766, 1.082531754730560403 ) ) ;
#173703 = CARTESIAN_POINT ( 'NONE',  ( 3.515250061227533696, -1.862011288300661871, 0.7743320027404425598 ) ) ;
#173702 = CARTESIAN_POINT ( 'NONE',  ( -6.832946231163084860, 10.91559500309152675, 0.000000000000000000 ) ) ;
#173704 = CARTESIAN_POINT ( 'NONE',  ( -1.201851678989727383E-14, 3.462500000000019895, 1.732050807568877637 ) ) ;
#173705 = CARTESIAN_POINT ( 'NONE',  ( -1.364683531250014514, 13.15104166700806410, -0.7879004041258335089 ) ) ;
#173706 = CARTESIAN_POINT ( 'NONE',  ( 6.633849695589691287, -1.131556152058693865, -1.301821263952767316 ) ) ;
#173707 = CARTESIAN_POINT ( 'NONE',  ( 7.876360894896227371, 8.153785563659219804, -0.7998128361456341429 ) ) ;
#173708 = CARTESIAN_POINT ( 'NONE',  ( 8.975134502566660899, 10.53370701015836275, -1.082531754730543083 ) ) ;
#173709 = CARTESIAN_POINT ( 'NONE',  ( 2.275391796764376640, 5.643962577969389827, -0.5307291018262025872 ) ) ;
#173710 = CARTESIAN_POINT ( 'NONE',  ( 4.850782132498069998, -1.503350029756752804, 1.112868480285071460 ) ) ;
#173711 = DIRECTION ( 'NONE',  ( 0.000000000000000000, 0.4363663110634622977, 0.8997691051424613340 ) ) ;
#173713 = AXIS2_PLACEMENT_3D ( 'NONE', #186310, #152757, #135456 ) ;
#173712 = CARTESIAN_POINT ( 'NONE',  ( 2.694261129275489886, 0.9798316074655871732, -1.823736424811234658 ) ) ;
#173714 = CARTESIAN_POINT ( 'NONE',  ( -6.075462232255183892, 10.10214001435745246, 0.000000000000000000 ) ) ;
#173715 = ORIENTED_EDGE ( 'NONE', *, *, #130897, .T. ) ;
#173716 = CARTESIAN_POINT ( 'NONE',  ( 2.891631901464575272, 6.595597328342462262, 0.000000000000000000 ) ) ;
#173717 = CARTESIAN_POINT ( 'NONE',  ( 0.3338568476279568653, -0.9693210200989417213, -1.530242633214883963 ) ) ;
#173718 = CARTESIAN_POINT ( 'NONE',  ( 4.462041952228939401, 6.299077925724123617, -1.443375672974068769 ) ) ;
#173719 = CARTESIAN_POINT ( 'NONE',  ( -3.557915510932114334, 4.150901429420823519, 2.420000000000010587 ) ) ;
#173720 = ORIENTED_EDGE ( 'NONE', *, *, #101206, .F. ) ;
#173722 = CARTESIAN_POINT ( 'NONE',  ( 8.749089199520284410, 9.101692242395490240, 0.7998128361456481317 ) ) ;
#173721 = CARTESIAN_POINT ( 'NONE',  ( 1.855835942623608181, -0.6640040153468586004, 1.846199708051485811 ) ) ;
#173723 = CARTESIAN_POINT ( 'NONE',  ( 5.747645016999404888, 1.886384853835708642, -0.3323884645628824019 ) ) ;
#173724 = CARTESIAN_POINT ( 'NONE',  ( -11.35569630219380777, 13.61268439291364274, 3.554478010595060411 ) ) ;
#173725 = DIRECTION ( 'NONE',  ( 0.2684563758389248433, 0.000000000000000000, -0.9632918427306597087 ) ) ;
#173726 = ADVANCED_FACE ( 'NONE', ( #978 ), #133181, .T. ) ;
#173728 = ORIENTED_EDGE ( 'NONE', *, *, #50025, .F. ) ;
#173727 = CARTESIAN_POINT ( 'NONE',  ( 5.531363484695522637, 5.555604941673978558, -0.7216878364870207285 ) ) ;
#173729 = CARTESIAN_POINT ( 'NONE',  ( -7.483737605063437215, 10.71448239167390604, 1.082531754730549967 ) ) ;
#173730 = CARTESIAN_POINT ( 'NONE',  ( 2.729541802387557059, -2.017400560480298033, 0.7770373237434914371 ) ) ;
#173731 = CARTESIAN_POINT ( 'NONE',  ( -6.943184063974175757, 9.193743722760251202, -1.443375672974066548 ) ) ;
#173732 = CARTESIAN_POINT ( 'NONE',  ( 4.927462483923885195, 4.713404084191450849, -0.7998128361456481317 ) ) ;
#173733 = CARTESIAN_POINT ( 'NONE',  ( -0.06985027309261250539, -2.078401542846250116, 0.4200961532789050379 ) ) ;
#173734 = CARTESIAN_POINT ( 'NONE',  ( 5.280226139177822908, -1.012770463184736736, 1.518683248463777113 ) ) ;
#173735 = CARTESIAN_POINT ( 'NONE',  ( 9.053228077256719075, 12.24160320938252333, 7.401071681518285317 ) ) ;
#173736 = CARTESIAN_POINT ( 'NONE',  ( 1.405477211469996934, -0.4828617686813937993, 1.911177332403845464 ) ) ;
#173737 = CARTESIAN_POINT ( 'NONE',  ( 3.445477555875466891, -1.765175379189663607, 0.7362804355328657069 ) ) ;
#173738 = EDGE_LOOP ( 'NONE', ( #76581, #96662, #125868, #70156 ) ) ;
#173739 = APPLICATION_CONTEXT ( 'automotive_design' ) ;
#173740 = DIRECTION ( 'NONE',  ( -0.6724985119639490527, 0.7071067811865536790, 0.2185080122244163481 ) ) ;
#173741 = CARTESIAN_POINT ( 'NONE',  ( 5.037540015474098354, 1.838441386810828693, -0.7070908002782918533 ) ) ;
#173742 = ORIENTED_EDGE ( 'NONE', *, *, #180914, .T. ) ;
#173743 = CARTESIAN_POINT ( 'NONE',  ( 6.321825213571911739, 1.114395046473240392, -1.590342819258899532 ) ) ;
#173744 = EDGE_LOOP ( 'NONE', ( #39171, #42132, #7174, #48506, #107715, #142545, #61186, #13112, #151299, #192330, #82569, #143696, #50285, #111702, #12049, #162529 ) ) ;
#173745 = CARTESIAN_POINT ( 'NONE',  ( -6.283277845290492714, 6.295188672452495915, -0.7998128361456362523 ) ) ;
#173747 = CARTESIAN_POINT ( 'NONE',  ( 6.433838290133602200, -2.056603270127650429, 0.5165238393732355382 ) ) ;
#173746 = CARTESIAN_POINT ( 'NONE',  ( -5.795184315198522285, 5.725746220678519904, -0.7998128361456362523 ) ) ;
#173748 = CARTESIAN_POINT ( 'NONE',  ( 6.278834536460164983, 9.379038488295265097, -1.082531754730548412 ) ) ;
#173750 = ORIENTED_EDGE ( 'NONE', *, *, #183912, .T. ) ;
#173749 = CARTESIAN_POINT ( 'NONE',  ( 4.090413894173472009, -1.098427525215146749, 1.565146720495188104 ) ) ;
#173751 = CARTESIAN_POINT ( 'NONE',  ( 0.8860939741733677710, 1.483344945610004073, 1.634051305214024641 ) ) ;
#173752 = TOROIDAL_SURFACE ( 'NONE', #187481, 0.8300000000000010703, 0.08000000000000000167 ) ;
#173753 = CARTESIAN_POINT ( 'NONE',  ( 7.583532603600732003, -5.197284395437371529, 7.968353659517134702 ) ) ;
#173754 = CARTESIAN_POINT ( 'NONE',  ( 6.024093331079843239, -1.997604944964962437, 0.2488386476607491182 ) ) ;
#173755 = DIRECTION ( 'NONE',  ( 0.000000000000000000, -1.000000000000000000, 0.000000000000000000 ) ) ;
#173756 = CARTESIAN_POINT ( 'NONE',  ( 5.988856447087389512, -0.2726756491404982441, -1.805090154579996442 ) ) ;
#173757 = CARTESIAN_POINT ( 'NONE',  ( 2.418496320782090869, 0.8830982243829659240, 1.872697815963566992 ) ) ;
#173758 = CARTESIAN_POINT ( 'NONE',  ( -6.901263884555985051, 8.010228272525461435, 1.199719254218450271 ) ) ;
#173759 = CARTESIAN_POINT ( 'NONE',  ( -6.202194133424988820, 6.954874670134298498, -0.8734430727420500196 ) ) ;
#173760 = CARTESIAN_POINT ( 'NONE',  ( -1.225000000000006084, 2.041666667349461672, -0.7072540797572977045 ) ) ;
#173761 = CARTESIAN_POINT ( 'NONE',  ( 6.737182200980119440, -1.669782060861616291, 0.8434366901180423426 ) ) ;
#173762 = CARTESIAN_POINT ( 'NONE',  ( 4.638861114170084399, 8.563755066507100722, 0.7998128361456462443 ) ) ;
#173763 = CARTESIAN_POINT ( 'NONE',  ( -11.63101921567910324, 8.358080680206626312, -2.966213382291108758 ) ) ;
#173764 = CARTESIAN_POINT ( 'NONE',  ( 5.424670859243587273, 5.501406555305196733, -0.7216878364870458196 ) ) ;
#173765 = DIRECTION ( 'NONE',  ( 0.000000000000000000, 0.000000000000000000, 1.000000000000000000 ) ) ;
#173766 = CARTESIAN_POINT ( 'NONE',  ( 1.620863580070950327, 0.5000000000000004441, -1.903365770102947385 ) ) ;
#173767 = CARTESIAN_POINT ( 'NONE',  ( 1.364683531249996529, 12.02604166700806765, 0.7879004041258405033 ) ) ;
#173769 = CARTESIAN_POINT ( 'NONE',  ( -5.824109505522200081, 8.952488968821326054, -1.199719254218452047 ) ) ;
#173768 = CARTESIAN_POINT ( 'NONE',  ( 6.925078400183550364, 2.979478345347879031, 2.309228228758605450 ) ) ;
#173770 = CARTESIAN_POINT ( 'NONE',  ( 5.150864522821732017, 0.8611363216781149355, 1.505151585408972981 ) ) ;
#173771 = AXIS2_PLACEMENT_3D ( 'NONE', #170133, #82749, #54264 ) ;
#173772 = CARTESIAN_POINT ( 'NONE',  ( -5.427341564172148303, 5.226320001155936090, 0.000000000000000000 ) ) ;
#173773 = CIRCLE ( 'NONE', #21557, 1.829047314007942848 ) ;
#173774 = CARTESIAN_POINT ( 'NONE',  ( 2.483334644719075168, -0.004358110040847408898, 2.070434559716929357 ) ) ;
#173775 = CARTESIAN_POINT ( 'NONE',  ( 3.585668865097063840, -0.6122912394212923770, 2.026781372153120930 ) ) ;
#173776 = CARTESIAN_POINT ( 'NONE',  ( 5.764187864104357573, 9.876636274763768597, 1.040834085586084257E-14 ) ) ;
#173777 = CARTESIAN_POINT ( 'NONE',  ( -1.123270288250339366, 3.283552654332833054, 0.7749999999993804067 ) ) ;
#173778 = CARTESIAN_POINT ( 'NONE',  ( 1.182395473146230946, 1.177546377092754337, -1.578453288034264990 ) ) ;
#173779 = CARTESIAN_POINT ( 'NONE',  ( 5.344703475446304530, 6.534489784648752853, 1.338571508491542383 ) ) ;
#173781 = CARTESIAN_POINT ( 'NONE',  ( -0.1054227091227821350, -1.855472971956134920, -0.4628026090111520552 ) ) ;
#173780 = CARTESIAN_POINT ( 'NONE',  ( 3.475000000000000533, -1.574999999999999956, 0.000000000000000000 ) ) ;
#173782 = CARTESIAN_POINT ( 'NONE',  ( 3.240441643373017211, 0.5569673610456173929, 2.223450396423230391 ) ) ;
#173783 = CARTESIAN_POINT ( 'NONE',  ( 1.330379832379691818, 1.758967509726565792, 0.4888242021733391618 ) ) ;
#173784 = CARTESIAN_POINT ( 'NONE',  ( 5.825163275726873202, 6.825053905550038991, 1.199719254218452047 ) ) ;
#173785 = CARTESIAN_POINT ( 'NONE',  ( 6.927853306458752414, 7.184843067064434763, 0.7216878364870317197 ) ) ;
#173786 = CARTESIAN_POINT ( 'NONE',  ( -7.507464373665155399, 9.781794407407920389, 1.599625672291295375 ) ) ;
#173787 = CARTESIAN_POINT ( 'NONE',  ( 2.865492421389451039, -1.648320183868864364, -1.155634683092461978 ) ) ;
#173788 = CARTESIAN_POINT ( 'NONE',  ( 3.625789200213443753, 1.914935786268581852, -0.4253726038727227432 ) ) ;
#173789 = CARTESIAN_POINT ( 'NONE',  ( -8.670602931139386627, 10.07445716020612103, 1.199719254218462483 ) ) ;
#173790 = CARTESIAN_POINT ( 'NONE',  ( -5.065942953000576843, 9.062017211809330064, -0.7998128361456231517 ) ) ;
#173791 = CYLINDRICAL_SURFACE ( 'NONE', #147454, 0.08000000000000020983 ) ;
#173793 = CARTESIAN_POINT ( 'NONE',  ( 4.768267862989370443, -1.154894395163852616, 1.341171105668465646 ) ) ;
#173792 = CARTESIAN_POINT ( 'NONE',  ( 5.613254157830992241, -2.039858995719573631, 0.4571984828403846124 ) ) ;
#173794 = CARTESIAN_POINT ( 'NONE',  ( -9.348561386651960348, 4.000000000000000888, 7.001914024036570261 ) ) ;
#173795 = CARTESIAN_POINT ( 'NONE',  ( 0.7092355107721182161, -0.3178641103029449799, 2.168156088950490723 ) ) ;
#173796 = CARTESIAN_POINT ( 'NONE',  ( 5.577983363897286218, -1.699187140184825751, -0.3753857801653339710 ) ) ;
#173797 = CARTESIAN_POINT ( 'NONE',  ( 7.214910300766615769, 11.56914578420308715, -0.7998128361456291469 ) ) ;
#173798 = CARTESIAN_POINT ( 'NONE',  ( 6.188148266813070286, 1.908752161701723571, 1.280650486962619627 ) ) ;
#173799 = CARTESIAN_POINT ( 'NONE',  ( 0.1333692844072802142, 0.2389375359408679178, -2.087895146362698906 ) ) ;
#173800 = CARTESIAN_POINT ( 'NONE',  ( 5.800041802258188106, -1.566351721726914725, 0.7437187281235900782 ) ) ;
#173801 = CARTESIAN_POINT ( 'NONE',  ( 5.898927382237683759, 0.4177183949424836396, 2.130464630886391486 ) ) ;
#173802 = CARTESIAN_POINT ( 'NONE',  ( -2.494940289813118994, 4.000000000000003553, 11.73777120880565583 ) ) ;
#173803 = CARTESIAN_POINT ( 'NONE',  ( 0.4623062725150044461, -1.170719190667910414, 1.764065175548671593 ) ) ;
#173804 = CARTESIAN_POINT ( 'NONE',  ( 3.093750000000001776, -1.895863743164152071, -0.7852924748298234503 ) ) ;
#173805 = CARTESIAN_POINT ( 'NONE',  ( 6.727182134110234024, 0.5746707207614526469, 2.142055518182262475 ) ) ;
#173806 = CARTESIAN_POINT ( 'NONE',  ( 4.155238220467009747, -1.601147421941846227, -1.070839854175157813 ) ) ;
#173807 = CARTESIAN_POINT ( 'NONE',  ( -1.500000000000001110, 11.30208333401612997, 0.8660254037844419273 ) ) ;
#173808 = CARTESIAN_POINT ( 'NONE',  ( 0.9970955524637573619, -2.168350899310825586, -0.4814931055744512411 ) ) ;
#173809 = ORIENTED_EDGE ( 'NONE', *, *, #70476, .T. ) ;
#173810 = CARTESIAN_POINT ( 'NONE',  ( 1.499999999999987121, 4.295833333333352044, -0.8660254037844323793 ) ) ;
#173811 = CARTESIAN_POINT ( 'NONE',  ( 3.811813743736467419, 7.598866467667865443, 1.040834085586084257E-14 ) ) ;
#173812 = CARTESIAN_POINT ( 'NONE',  ( 6.819914962873951936, 7.915321197229798322, -1.199719254218446718 ) ) ;
#173813 = CARTESIAN_POINT ( 'NONE',  ( 3.123905467589927820, -0.4314640245299468657, 2.178836924841739631 ) ) ;
#173814 = CARTESIAN_POINT ( 'NONE',  ( -9.354762803749327560, 10.01623748057011376, 0.7216878364870438212 ) ) ;
#173816 = EDGE_CURVE ( 'NONE', #197822, #30182, #197879, .T. ) ;
#173815 = CARTESIAN_POINT ( 'NONE',  ( -0.02900071798683095947, 5.719935618195115978, -2.767867108847458901 ) ) ;
#173817 = CARTESIAN_POINT ( 'NONE',  ( 7.131225611108100715, 7.422110755822004968, 0.7216878364870317197 ) ) ;
#173818 = CARTESIAN_POINT ( 'NONE',  ( -8.093854517234044366, 11.42628545587295186, 1.082531754730549967 ) ) ;
#173819 = CARTESIAN_POINT ( 'NONE',  ( 6.617788377246179188, 8.814115421577600529, -1.443375672974078761 ) ) ;
#173820 = CARTESIAN_POINT ( 'NONE',  ( 0.7037502660087076034, 1.864169469917423161, 0.7691187473759173443 ) ) ;
#173822 = CARTESIAN_POINT ( 'NONE',  ( 6.549293068304288923, 1.796493013226226232, -1.013385894242497809 ) ) ;
#173821 = CARTESIAN_POINT ( 'NONE',  ( 8.215351014876830504, 11.67199438640995801, -1.199719254218446718 ) ) ;
#173823 = PRESENTATION_STYLE_ASSIGNMENT (( #174888 ) ) ;
#173824 = CARTESIAN_POINT ( 'NONE',  ( 5.506019780481205217, 9.437790487287811558, 0.000000000000000000 ) ) ;
#173825 = CARTESIAN_POINT ( 'NONE',  ( -1.364683531250014514, 1.488541667008084435, -0.7879004041258289570 ) ) ;
#173826 = CARTESIAN_POINT ( 'NONE',  ( 0.9129390864682377371, -0.2673504635808711671, 1.749312949811430373 ) ) ;
#173827 = CARTESIAN_POINT ( 'NONE',  ( 0.3521856818783953846, 0.1948384997633167970, -2.006960225185448810 ) ) ;
#173828 = CARTESIAN_POINT ( 'NONE',  ( 6.093256065386793985, -0.5776499228958801302, 1.641946315008017576 ) ) ;
#173829 = CARTESIAN_POINT ( 'NONE',  ( 3.738036193864560541, 2.281383974799616521, 0.2239769770701737495 ) ) ;
#173830 = CARTESIAN_POINT ( 'NONE',  ( -1.402160292154681736E-14, -0.3031249996585801965, -1.575800808251665908 ) ) ;
#173831 = CARTESIAN_POINT ( 'NONE',  ( 2.062219658421380775, -1.683061746929171321, -0.7467898329211534181 ) ) ;
#173832 = CARTESIAN_POINT ( 'NONE',  ( 9.911173986789782120, 11.52179005846497972, -1.199719254218440723 ) ) ;
#173833 = CARTESIAN_POINT ( 'NONE',  ( 3.575057022766346737, 0.04566639709948847742, -1.825179878808772305 ) ) ;
#173834 = CARTESIAN_POINT ( 'NONE',  ( 3.832657856672664565, 0.6767144645295587457, -1.899618369658891748 ) ) ;
#173835 = CARTESIAN_POINT ( 'NONE',  ( -9.612894607289142357, 11.17379744904754801, -1.199719254218441611 ) ) ;
#173837 = CARTESIAN_POINT ( 'NONE',  ( 4.911989969715248705, 4.726297878971393196, -2.420000000000000373 ) ) ;
#173836 = CARTESIAN_POINT ( 'NONE',  ( 2.114515676104791186, -1.066955051536956356, -1.995125387583786214 ) ) ;
#173838 = CARTESIAN_POINT ( 'NONE',  ( 4.893641883129576264, 1.558557130586870398, 1.416501212539149845 ) ) ;
#173839 = CARTESIAN_POINT ( 'NONE',  ( 8.738814790737972515, 15.13806168530491902, 7.596998062084875158 ) ) ;
#173840 = CARTESIAN_POINT ( 'NONE',  ( 2.840353284027045344, -1.066491845456703835, 1.774417039089710935 ) ) ;
#173841 = CARTESIAN_POINT ( 'NONE',  ( 5.542585869888291938, 5.360771691158120689, -0.7998128361456211532 ) ) ;
#173842 = CARTESIAN_POINT ( 'NONE',  ( 0.6801582343749952297, 1.088541667008086078, -1.178068619123883165 ) ) ;
#173843 = CARTESIAN_POINT ( 'NONE',  ( 5.004590575528129470, -2.104527602236761386, -0.2589986953433416894 ) ) ;
#173844 = SHAPE_DEFINITION_REPRESENTATION ( #57414, #11178 ) ;
#173846 = CARTESIAN_POINT ( 'NONE',  ( 1.189925737956001095, -0.8670580458889056708, 1.720419655784347412 ) ) ;
#173845 = CARTESIAN_POINT ( 'NONE',  ( -10.64045162862669081, 11.30828174301964140, -0.7998128361456221525 ) ) ;
#173847 = CARTESIAN_POINT ( 'NONE',  ( -3.318713740295064163, 7.093859473644694269, 0.000000000000000000 ) ) ;
#173848 = CARTESIAN_POINT ( 'NONE',  ( 8.235688245297327015, 11.69572115523387268, -1.199719254218446718 ) ) ;
#173849 = CARTESIAN_POINT ( 'NONE',  ( 5.139949632912227173, 8.050339434155988627, -1.082531754730548412 ) ) ;
#173850 = CARTESIAN_POINT ( 'NONE',  ( 5.150161082644886257, 6.468739049537000518, 1.195298158575591074 ) ) ;
#173851 = CARTESIAN_POINT ( 'NONE',  ( -0.2116396714000057522, 2.800000000000025135, -1.427100650709098417 ) ) ;
#173852 = CARTESIAN_POINT ( 'NONE',  ( -3.958090780185743451, 6.705190779270287393, -1.199719254218452047 ) ) ;
#173853 = CARTESIAN_POINT ( 'NONE',  ( 0.7037666293719077037, 1.955508453885120401, -1.053950084065604864 ) ) ;
#173854 = CARTESIAN_POINT ( 'NONE',  ( 1.712088352014268899, -2.090129137712465557, 0.2570578816783394283 ) ) ;
#173855 = CARTESIAN_POINT ( 'NONE',  ( -5.503684012504701961, 5.385662534202396934, 0.000000000000000000 ) ) ;
#173856 = CARTESIAN_POINT ( 'NONE',  ( 8.762647353133951711, 9.117510088278095282, 1.040834085586084257E-14 ) ) ;
#173857 = CARTESIAN_POINT ( 'NONE',  ( 6.491040186595096628, 0.1814514006053032646, 1.852032668777810587 ) ) ;
#173858 = CARTESIAN_POINT ( 'NONE',  ( 6.856673000209174695, 9.022537805042615489, 1.599625672291281386 ) ) ;
#173859 =( BOUNDED_CURVE ( )  B_SPLINE_CURVE ( 1, ( #87077, #189910 ),
 .UNSPECIFIED., .F., .T. ) 
 B_SPLINE_CURVE_WITH_KNOTS ( ( 2, 2 ),
 ( 0.000000000000000000, 6.249999999999832079E-05 ),
 .UNSPECIFIED. ) 
 CURVE ( )  GEOMETRIC_REPRESENTATION_ITEM ( )  RATIONAL_B_SPLINE_CURVE ( ( 0.9345202395942817652, 0.9345202395942817652 ) ) 
 REPRESENTATION_ITEM ( '' )  );
#173860 = CARTESIAN_POINT ( 'NONE',  ( -6.780486220610184134, 9.003929572168926754, -1.443375672974066548 ) ) ;
#173861 = CARTESIAN_POINT ( 'NONE',  ( -8.839552966430007430, 11.33589776563360019, -1.443375672974059665 ) ) ;
#173862 = CIRCLE ( 'NONE', #135806, 2.080000000000000071 ) ;
#173863 = CARTESIAN_POINT ( 'NONE',  ( -7.015401035077363900, 6.062865449010541141, 2.437084766375292144 ) ) ;
#173864 = CARTESIAN_POINT ( 'NONE',  ( -15.75000000000000000, 12.29999999999998295, 3.199999999999997957 ) ) ;
#173866 = CARTESIAN_POINT ( 'NONE',  ( 2.910546574502240968, 0.6583626327048962557, 1.848246418561696913 ) ) ;
#173865 = CARTESIAN_POINT ( 'NONE',  ( 1.224999999999969225, -0.3541666666666576369, -0.7072540797573098059 ) ) ;
#173867 = CARTESIAN_POINT ( 'NONE',  ( 1.674925575805393585, -2.052671086741376882, -0.6780288057936025847 ) ) ;
#173868 = MECHANICAL_DESIGN_GEOMETRIC_PRESENTATION_REPRESENTATION (  '', ( #187588 ), #121973 ) ;
#173870 = CARTESIAN_POINT ( 'NONE',  ( -5.609265928939476176, 6.186647267178685183, -0.8691123025580966832 ) ) ;
#173869 = CARTESIAN_POINT ( 'NONE',  ( -5.795184315198522285, 5.725746220678519904, -0.7998128361456362523 ) ) ;
#173872 = EDGE_CURVE ( 'NONE', #211004, #33851, #23193, .T. ) ;
#173871 = CARTESIAN_POINT ( 'NONE',  ( -1.364683531250012516, 2.280208333674751842, 0.7879004041258379498 ) ) ;
#173873 = CARTESIAN_POINT ( 'NONE',  ( 3.116877616926060135, -1.676954032530679761, 0.4650628940853319682 ) ) ;
#173874 = CARTESIAN_POINT ( 'NONE',  ( 5.612712406377503349, 8.531619659873665995, -1.082531754730543083 ) ) ;
#173875 = CARTESIAN_POINT ( 'NONE',  ( -11.15867860892636365, 6.757705308438493041, -5.812542620506402358 ) ) ;
#173876 = EDGE_LOOP ( 'NONE', ( #9978, #119296, #46908, #137110 ) ) ;
#173877 = CARTESIAN_POINT ( 'NONE',  ( 2.794295885581669747, -1.882186412485300719, 0.7230279869864174591 ) ) ;
#173878 = CARTESIAN_POINT ( 'NONE',  ( 6.825078400183546279, 2.419143596098617621, 2.525240329153962904 ) ) ;
#173879 = CARTESIAN_POINT ( 'NONE',  ( -3.984117037569407938, 5.741498858621315371, 1.599625672291270506 ) ) ;
#173880 = CARTESIAN_POINT ( 'NONE',  ( 2.395336953769642729, 1.522948423943527363, 1.251906274522778251 ) ) ;
#173881 = EDGE_CURVE ( 'NONE', #122713, #67094, #155807, .T. ) ;
#173883 = ORIENTED_EDGE ( 'NONE', *, *, #151553, .F. ) ;
#173882 = CARTESIAN_POINT ( 'NONE',  ( -5.045042558060949034, 6.018876084893449274, 1.082531754730549078 ) ) ;
#173885 = ADVANCED_FACE ( 'NONE', ( #69180 ), #151541, .T. ) ;
#173884 = CARTESIAN_POINT ( 'NONE',  ( -4.773879485343255347, 8.583626809626847987, 0.000000000000000000 ) ) ;
#173886 = CARTESIAN_POINT ( 'NONE',  ( 7.062871678076271920, 7.204714810702593120, -0.7998128361456341429 ) ) ;
#173887 = CARTESIAN_POINT ( 'NONE',  ( -5.794130544993808307, 7.853181283949808744, 1.599625672291263179 ) ) ;
#173888 = CARTESIAN_POINT ( 'NONE',  ( 1.928384432292037598, -0.9539229595667864103, -1.780212580967098335 ) ) ;
#173889 = CARTESIAN_POINT ( 'NONE',  ( -1.396038594575822467, 4.344678208267337638, 0.1345620919992577547 ) ) ;
#173890 = CARTESIAN_POINT ( 'NONE',  ( 5.280430876874616430, -1.287285901688420608, 1.914989055045878352 ) ) ;
#173891 = CARTESIAN_POINT ( 'NONE',  ( 6.795372052238223048, -1.752927774724974297, 0.8811163259476795240 ) ) ;
#173892 = CARTESIAN_POINT ( 'NONE',  ( 2.483191118468269565, -0.005009705968514814069, 1.961936380092830223 ) ) ;
#173893 = CARTESIAN_POINT ( 'NONE',  ( 7.913155211870404493, 12.38376484715752213, 0.7998128361456462443 ) ) ;
#173894 = CARTESIAN_POINT ( 'NONE',  ( 1.072888940501380839, -0.9041080511620370741, 1.802418165037560138 ) ) ;
#173895 = ORIENTED_EDGE ( 'NONE', *, *, #160720, .T. ) ;
#173896 = CARTESIAN_POINT ( 'NONE',  ( 2.097004163592118164, 1.893647498693065589, 0.9473067498170744116 ) ) ;
#173898 = CARTESIAN_POINT ( 'NONE',  ( -6.344325816190970357, 9.489131654609717970, 1.199719254218452047 ) ) ;
#173897 = CARTESIAN_POINT ( 'NONE',  ( -4.135400547368138113, 4.783387712472935149, 1.199719254218462483 ) ) ;
#173899 = CARTESIAN_POINT ( 'NONE',  ( 2.220424023188283247, -0.0004634451795330202239, 1.841320589463534052 ) ) ;
#173900 = ORIENTED_EDGE ( 'NONE', *, *, #188786, .T. ) ;
#173901 = CARTESIAN_POINT ( 'NONE',  ( 3.116422982138194353, 1.968445132739887748, 0.4370783100892047801 ) ) ;
#173902 = CARTESIAN_POINT ( 'NONE',  ( -10.45741655484220267, 11.09474082360439873, -0.7998128361456221525 ) ) ;
#173903 = CARTESIAN_POINT ( 'NONE',  ( 10.24561425425348382, 10.82119614928647877, 6.253163089680928266 ) ) ;
#173904 = CARTESIAN_POINT ( 'NONE',  ( 3.340189922722580196, -1.266226476691566738, -1.700888996046201029 ) ) ;
#173905 = CARTESIAN_POINT ( 'NONE',  ( 0.6910384644343779970, -0.6650364481293036256, 1.717017257891314097 ) ) ;
#173906 = CARTESIAN_POINT ( 'NONE',  ( -1.001543065824772872E-14, 4.493750000682820378, 1.732050807568877637 ) ) ;
#173907 = CARTESIAN_POINT ( 'NONE',  ( 8.046927864910717432, 9.346836249606042202, 1.199719254218462483 ) ) ;
#173909 = CARTESIAN_POINT ( 'NONE',  ( 6.339319342841494453, 9.553567112360518365, -1.199719254218452047 ) ) ;
#173908 = B_SPLINE_CURVE_WITH_KNOTS ( 'NONE', 3,
 ( #131387, #33819, #18627, #150793 ),
 .UNSPECIFIED., .F., .F.,
 ( 4, 4 ),
 ( 0.003007768841253834029, 0.003753604288505242494 ),
 .UNSPECIFIED. ) ;
#173910 = CARTESIAN_POINT ( 'NONE',  ( 4.464173201700037730, 0.9678196394932538915, 1.819351253882226516 ) ) ;
#173911 = VECTOR ( 'NONE', #70839, 1000.000000000000000 ) ;
#173913 = CARTESIAN_POINT ( 'NONE',  ( 1.188719773494644860, 1.394467456127197025, 1.202481090285527632 ) ) ;
#173912 = CARTESIAN_POINT ( 'NONE',  ( -9.176171038350775078, 9.599954387697719582, -0.7998128361456291469 ) ) ;
#173914 = CARTESIAN_POINT ( 'NONE',  ( -1.364683531250010295, 4.530208333674754506, 0.7879004041258379498 ) ) ;
#173915 = DIRECTION ( 'NONE',  ( -3.330669073875478496E-16, 1.665334536937734318E-16, 1.000000000000000000 ) ) ;
#173916 = CARTESIAN_POINT ( 'NONE',  ( -1.566565198595248676, 8.754658464388056061, 2.463935442259440833 ) ) ;
#173917 = CARTESIAN_POINT ( 'NONE',  ( -11.97929049433705373, 11.37999999999999901, 0.7046979865771783036 ) ) ;
#173918 =( BOUNDED_SURFACE ( )  B_SPLINE_SURFACE ( 3, 2, ( 
 ( #166754, #33545, #201350 ),
 ( #164619, #199221, #67080 ),
 ( #213345, #82286, #49799 ),
 ( #116990, #182990, #115925 ),
 ( #118065, #34607, #133215 ),
 ( #113813, #17273, #131122 ) ),
 .UNSPECIFIED., .F., .F., .T. ) 
 B_SPLINE_SURFACE_WITH_KNOTS ( ( 4, 2, 4 ),
 ( 3, 3 ),
 ( 0.000000000000000000, 0.0003766405729503174787, 0.0007532811459006349573 ),
 ( 0.000000000000000000, 1.000000000000000000 ),
 .UNSPECIFIED. ) 
 GEOMETRIC_REPRESENTATION_ITEM ( )  RATIONAL_B_SPLINE_SURFACE ( (
 ( 1.000000000000000000, 0.7071067811865551223, 1.000000000000000000),
 ( 1.000000000000000000, 0.7211294902953824248, 1.000000000000000000),
 ( 1.000000000000000000, 0.7311181975230335306, 1.000000000000000000),
 ( 1.000000000000000000, 0.7429553055061443034, 1.000000000000000000),
 ( 1.000000000000000000, 0.7451698531058310593, 1.000000000000000000),
 ( 1.000000000000000000, 0.7452309222762957264, 1.000000000000000000) ) ) 
 REPRESENTATION_ITEM ( '' )  SURFACE ( )  );
#173919 = CARTESIAN_POINT ( 'NONE',  ( 1.155211076828046579, -1.737760091701185505, 1.360235214042208263 ) ) ;
#173920 = CARTESIAN_POINT ( 'NONE',  ( 3.269090859574837804, -2.088958473869072741, -0.8692115097446629912 ) ) ;
#173921 = CARTESIAN_POINT ( 'NONE',  ( -8.676855123066022912, 10.18571440074093282, -1.082531754730543971 ) ) ;
#173922 = CARTESIAN_POINT ( 'NONE',  ( 3.339928375916663139, -1.083189831351333954, -1.451890931963683684 ) ) ;
#173923 = CARTESIAN_POINT ( 'NONE',  ( 2.712013535993620383, 1.060242027361221862, -1.595356271853585195 ) ) ;
#173924 = CARTESIAN_POINT ( 'NONE',  ( 4.404779037558821386, 0.5491149005726041477, 1.996164414091922135 ) ) ;
#173925 = CARTESIAN_POINT ( 'NONE',  ( -1.364683531249997417, 2.821875000341422801, 1.214306433183764966E-14 ) ) ;
#173926 = CARTESIAN_POINT ( 'NONE',  ( 2.377750047251852017, 1.211369778508808448, 1.555330764497768303 ) ) ;
#173927 = CARTESIAN_POINT ( 'NONE',  ( 1.026247228566424363, 1.149774913616221417, -1.545494133055951069 ) ) ;
#173928 = CARTESIAN_POINT ( 'NONE',  ( 4.381629165553334815, 1.221847395770376377, 1.416585496670008659 ) ) ;
#173929 = CARTESIAN_POINT ( 'NONE',  ( 1.981525833354264243, -0.1160811445666837666, -2.304894087891403487 ) ) ;
#173930 = CARTESIAN_POINT ( 'NONE',  ( 3.824516763807362274, -1.251359258362509497, 1.377693585838150936 ) ) ;
#173931 = CARTESIAN_POINT ( 'NONE',  ( 1.364683531249990311, 4.863541667008084879, 0.7879004041258500513 ) ) ;
#173932 = AXIS2_PLACEMENT_3D ( 'NONE', #188320, #104969, #153707 ) ;
#173933 = CARTESIAN_POINT ( 'NONE',  ( -3.425406365747000859, 7.148057860013469877, 1.040834085586084257E-14 ) ) ;
#173934 = CARTESIAN_POINT ( 'NONE',  ( 5.829115978871627135, 8.888053511070525659, 1.199719254218462483 ) ) ;
#173935 = CARTESIAN_POINT ( 'NONE',  ( 0.4019237886466816012, 8.957585450998170273, -1.499999999999998668 ) ) ;
#173936 = CARTESIAN_POINT ( 'NONE',  ( 0.8386649464857205416, 2.075244960028700181, 0.3580382472886770584 ) ) ;
#173938 = LINE ( 'NONE', #106826, #191130 ) ;
#173937 = CARTESIAN_POINT ( 'NONE',  ( 0.6823417656249917140, 3.405208333674754506, 1.181850606188765695 ) ) ;
#173939 = CARTESIAN_POINT ( 'NONE',  ( 6.696550776676711614, -0.5693818166121329405, -2.085215994158528208 ) ) ;
#173940 = CARTESIAN_POINT ( 'NONE',  ( 2.232824136269210502, 1.381628265877183903, -1.608862310199298928 ) ) ;
#173941 = CARTESIAN_POINT ( 'NONE',  ( 1.248313549685893475, 0.9916667988653109500, -1.759473928524292630 ) ) ;
#173942 = CARTESIAN_POINT ( 'NONE',  ( 0.6823417656249882723, 0.1760416670080894308, -1.181850606188749264 ) ) ;
#173943 = CARTESIAN_POINT ( 'NONE',  ( -4.284013352238262407, 6.021101549076499637, -1.443375672974053447 ) ) ;
#173944 = CARTESIAN_POINT ( 'NONE',  ( 6.498435699651741615, 6.475929825882159818, -0.7998128361456281477 ) ) ;
#173945 = CARTESIAN_POINT ( 'NONE',  ( 1.335488691732108046, -1.954760257947166568, 0.9229496955955732718 ) ) ;
#173948 = CARTESIAN_POINT ( 'NONE',  ( 3.795919822146273326, 5.451659097302528068, -1.443375672974051449 ) ) ;
#173947 = DIRECTION ( 'NONE',  ( 0.000000000000000000, 0.000000000000000000, -1.000000000000000000 ) ) ;
#173946 = CARTESIAN_POINT ( 'NONE',  ( 4.064412189046650248, 7.963840997188264659, 0.7998128361456271485 ) ) ;
#173949 = CARTESIAN_POINT ( 'NONE',  ( 6.210172754313918908, 1.157103754073171675, -1.651340222398114843 ) ) ;
#173951 = CARTESIAN_POINT ( 'NONE',  ( -6.577113915960841162, 7.806292669110006521, -1.082531754730549967 ) ) ;
#173950 = CARTESIAN_POINT ( 'NONE',  ( -9.164948653157990677, 11.71552606681625619, -1.443375672974059665 ) ) ;
#173952 = DIRECTION ( 'NONE',  ( 0.000000000000000000, 0.000000000000000000, -1.000000000000000000 ) ) ;
#173954 = CARTESIAN_POINT ( 'NONE',  ( -0.6823417656250039265, 10.31770833367473550, -1.181850606188755259 ) ) ;
#173953 = CARTESIAN_POINT ( 'NONE',  ( 0.2161854901324336276, -2.218109922327567318, 0.4452641707137113825 ) ) ;
#173955 = CARTESIAN_POINT ( 'NONE',  ( -10.64723070543352712, 11.31619066596094392, 0.7998128361456462443 ) ) ;
#173956 = ADVANCED_FACE ( 'NONE', ( #5240 ), #119092, .F. ) ;
#173958 = CARTESIAN_POINT ( 'NONE',  ( 0.1224727961543301408, 0.3280879897031144798, 1.887133295268013766 ) ) ;
#173957 = CARTESIAN_POINT ( 'NONE',  ( -6.060131475184148186, 6.172500930577367484, 0.7216878364870317197 ) ) ;
#173959 = CARTESIAN_POINT ( 'NONE',  ( -1.364683531250014514, 0.5510416670080878765, -0.7879004041258289570 ) ) ;
#173960 = CARTESIAN_POINT ( 'NONE',  ( 11.92619526913699879, 10.19999999999998153, 1.328859060402684644 ) ) ;
#173961 = CARTESIAN_POINT ( 'NONE',  ( 1.499999999999997113, 8.645833333333337478, -0.8660254037844378194 ) ) ;
#173962 = CARTESIAN_POINT ( 'NONE',  ( 3.035487670047633202, -1.158914029964135395, -1.277714875195012700 ) ) ;
#173963 = CARTESIAN_POINT ( 'NONE',  ( 4.706615602599436343, 5.520081620234675412, 1.199719254218452935 ) ) ;
#173964 = CARTESIAN_POINT ( 'NONE',  ( 7.191674137406095291, 7.354984346587396082, 0.000000000000000000 ) ) ;
#173965 = CARTESIAN_POINT ( 'NONE',  ( 1.264531387369687065, -1.596916444607907382, -0.7631234423778727738 ) ) ;
#173966 = CARTESIAN_POINT ( 'NONE',  ( 1.453772141523026251, -1.459646937795316068, -1.386592938616920678 ) ) ;
#173967 = DIRECTION ( 'NONE',  ( 0.000000000000000000, 0.000000000000000000, -1.000000000000000000 ) ) ;
#173968 = CARTESIAN_POINT ( 'NONE',  ( 4.401547605996741552, 1.770323140634282311, 1.317293360403009927 ) ) ;
#173969 = ORIENTED_EDGE ( 'NONE', *, *, #6898, .T. ) ;
#173970 = CARTESIAN_POINT ( 'NONE',  ( 7.741342523278692767, 11.01502146292508044, 1.082531754730558626 ) ) ;
#173972 = CARTESIAN_POINT ( 'NONE',  ( 3.216422893352603563, 1.967893637826668263, 0.4390085219014849827 ) ) ;
#173971 = CARTESIAN_POINT ( 'NONE',  ( 3.791739704763209318, 1.996120715041304061, -0.7158466834289513026 ) ) ;
#173974 = VERTEX_POINT ( 'NONE', #4178 ) ;
#173973 = CARTESIAN_POINT ( 'NONE',  ( 3.322321318109163979, -0.7387318680696324247, -1.654322230785286063 ) ) ;
#173975 = CARTESIAN_POINT ( 'NONE',  ( 4.115782150200256950, 6.959440387612411349, 1.199719254218452047 ) ) ;
#173976 = EDGE_LOOP ( 'NONE', ( #66428, #170762, #143498, #38934 ) ) ;
#173977 = CARTESIAN_POINT ( 'NONE',  ( 1.832664747978371533, 0.1804508633567840359, 1.861920966532565336 ) ) ;
#173978 = CARTESIAN_POINT ( 'NONE',  ( 3.246287715468270108, 5.874753870433235825, 1.199719254218450271 ) ) ;
#173979 = EDGE_CURVE ( 'NONE', #133087, #194227, #204293, .T. ) ;
#173980 = CARTESIAN_POINT ( 'NONE',  ( 6.006453938882227561, -0.6616566355047011072, -1.701761020394356283 ) ) ;
#173982 = CARTESIAN_POINT ( 'NONE',  ( 2.676846564686267804, 1.640678131122888406, -0.9888057999517668728 ) ) ;
#173981 = CARTESIAN_POINT ( 'NONE',  ( -4.115063316947640715, 4.759660943649018705, 1.199719254218462483 ) ) ;
#173983 = CARTESIAN_POINT ( 'NONE',  ( -9.917242840447775265, 4.174869238508773783, -6.172972641688763140 ) ) ;
#173984 = CARTESIAN_POINT ( 'NONE',  ( -2.788906526875773208E-15, 8.468750000682796042, -1.499999999999998446 ) ) ;
#173985 = CARTESIAN_POINT ( 'NONE',  ( 0.6823417656249882723, 1.238541667008083547, -1.181850606188749264 ) ) ;
#173986 = CARTESIAN_POINT ( 'NONE',  ( 2.157015650737173384, 3.934209603697786495, -11.36298392073394226 ) ) ;
#173987 = CARTESIAN_POINT ( 'NONE',  ( 5.858531774880875176, 9.849054480754103835, -0.7216878364870458196 ) ) ;
#173988 = EDGE_CURVE ( 'NONE', #79400, #152913, #212223, .T. ) ;
#173989 = CARTESIAN_POINT ( 'NONE',  ( -3.634994582239682526, 6.294558541704648569, 1.082531754730549967 ) ) ;
#173990 = CARTESIAN_POINT ( 'NONE',  ( -5.427006627220116286, 9.553534508390610469, -0.7998128361456362523 ) ) ;
#173991 = CARTESIAN_POINT ( 'NONE',  ( 3.357788437482766675, -1.608272433257527556, -1.382313803475518244 ) ) ;
#173993 = CARTESIAN_POINT ( 'NONE',  ( -12.36781821011106963, 9.649948393628900334, 1.413879826568002152 ) ) ;
#173992 = CARTESIAN_POINT ( 'NONE',  ( -0.02968770228140017037, 2.049257630910449990, -2.243713227073070637 ) ) ;
#173994 = CARTESIAN_POINT ( 'NONE',  ( 3.866447834861338695, -1.326295688514609550, 1.458626262776492544 ) ) ;
#173995 = CARTESIAN_POINT ( 'NONE',  ( -0.1403655429255863119, -1.558841978801903894, -1.273620833657141072 ) ) ;
#173996 = VERTEX_POINT ( 'NONE', #89758 ) ;
#173997 = CARTESIAN_POINT ( 'NONE',  ( 6.385961957380775544, -2.116826826188836552, 0.05405687909286471110 ) ) ;
#173998 =( LENGTH_UNIT ( ) NAMED_UNIT ( * ) SI_UNIT ( .MILLI., .METRE. ) );
#173999 = CARTESIAN_POINT ( 'NONE',  ( 1.522023487246677798, 2.040062638832959241, -0.3519594530456415793 ) ) ;
#174000 = CARTESIAN_POINT ( 'NONE',  ( 7.126746022638799971, 8.343567110280638133, 1.199719254218452047 ) ) ;
#174001 = ORIENTED_EDGE ( 'NONE', *, *, #207616, .T. ) ;
#174002 = CARTESIAN_POINT ( 'NONE',  ( 4.532168488718122390, 8.509556680138327778, 0.7998128361456271485 ) ) ;
#174003 = CARTESIAN_POINT ( 'NONE',  ( 7.198453214212898743, 7.362893269528701268, 0.7998128361456291469 ) ) ;
#174005 = CARTESIAN_POINT ( 'NONE',  ( 4.143988507271280319, 7.986403691791820414, -0.7998128361456221525 ) ) ;
#174004 = CARTESIAN_POINT ( 'NONE',  ( 4.101575158799015242, -2.085053422979638693, 0.1536182331017873492 ) ) ;
#174006 = CARTESIAN_POINT ( 'NONE',  ( 4.706088717274906408, 5.623429937309770921, 1.082531754730549078 ) ) ;
#174008 = ORIENTED_EDGE ( 'NONE', *, *, #94862, .T. ) ;
#174007 = CARTESIAN_POINT ( 'NONE',  ( 0.1174177504974990710, -0.4853618992130321885, 1.745175170155540245 ) ) ;
#174009 = CARTESIAN_POINT ( 'NONE',  ( 5.619807753665406302, -2.153844256707802440, 0.4802137346974973409 ) ) ;
#174010 = FILL_AREA_STYLE ('',( #206466 ) ) ;
#174011 = CARTESIAN_POINT ( 'NONE',  ( 4.753059971535213535, -1.774748228059085164, 1.311344899593884561 ) ) ;
#174012 = CARTESIAN_POINT ( 'NONE',  ( 8.633844893804129228, 8.967240552393299424, -0.7998128361456211532 ) ) ;
#174013 = CARTESIAN_POINT ( 'NONE',  ( 0.5773502691896192918, -2.500000000000002220, 1.000000000000004441 ) ) ;
#174014 = CARTESIAN_POINT ( 'NONE',  ( 2.789602095257078584, 1.815147277589121533, -0.6018686165152677958 ) ) ;
#174015 = CIRCLE ( 'NONE', #177393, 1.850000000000000089 ) ;
#174016 = CARTESIAN_POINT ( 'NONE',  ( 9.585778300061798873, 11.14216175728232550, -1.199719254218440723 ) ) ;
#174017 = CARTESIAN_POINT ( 'NONE',  ( 5.477033855465498924, 1.911541192706748715, 0.7957256658025003704 ) ) ;
#174018 = AXIS2_PLACEMENT_3D ( 'NONE', #184553, #14585, #181365 ) ;
#174020 = CARTESIAN_POINT ( 'NONE',  ( 3.098656953246520906, -0.6260995091542166380, -2.069055637940686143 ) ) ;
#174019 = CARTESIAN_POINT ( 'NONE',  ( -3.031102536865480701, 6.452456358313791718, 0.6335066767141804833 ) ) ;
#174021 = CARTESIAN_POINT ( 'NONE',  ( 5.214472588068230330, 2.024700573814151028, 0.8392323156421463981 ) ) ;
#174022 = CARTESIAN_POINT ( 'NONE',  ( 1.737500000000001155, -1.983333333333333393, 3.009438278150922130 ) ) ;
#174023 = DIRECTION ( 'NONE',  ( -0.3321398189114301847, 0.9432301631592802105, 8.628166150854816622E-32 ) ) ;
#174024 = CARTESIAN_POINT ( 'NONE',  ( 3.413620815590684199, 7.204584394822967752, 0.7998128361456281477 ) ) ;
#174025 = FACE_OUTER_BOUND ( 'NONE', #181321, .T. ) ;
#174026 = FACE_OUTER_BOUND ( 'NONE', #206730, .T. ) ;
#174027 = CARTESIAN_POINT ( 'NONE',  ( -6.561783159334121152, 10.59923808595773664, -0.7216878364870278340 ) ) ;
#174028 = CARTESIAN_POINT ( 'NONE',  ( 4.213551878797002992, 8.137837301896977849, 0.000000000000000000 ) ) ;
#174029 = CARTESIAN_POINT ( 'NONE',  ( 5.647352632913819726, 1.828451368696734747, -0.9708816006866529680 ) ) ;
#174030 = CARTESIAN_POINT ( 'NONE',  ( 4.371652425709642742, 1.868346805267994570, -0.4693074334855638630 ) ) ;
#174031 = CARTESIAN_POINT ( 'NONE',  ( 0.2105648349144396136, 1.930425396462841725, 0.5826343419270895163 ) ) ;
#174032 =( NAMED_UNIT ( * ) SI_UNIT ( $, .STERADIAN. ) SOLID_ANGLE_UNIT ( ) );
#174033 = CARTESIAN_POINT ( 'NONE',  ( 5.643937085038755797, 9.806620042512378177, -0.7998128361456481317 ) ) ;
#174034 = CARTESIAN_POINT ( 'NONE',  ( 0.2999999999999686806, 3.975028841772344723, -0.9637995837462834947 ) ) ;
#174035 = CARTESIAN_POINT ( 'NONE',  ( 0.6916816545035618935, -0.7852976098030055585, 2.046091368998310678 ) ) ;
#174036 = CARTESIAN_POINT ( 'NONE',  ( 5.566980414702134894, -1.652319403193935887, -0.7768266693391965294 ) ) ;
#174037 = CARTESIAN_POINT ( 'NONE',  ( 4.909461021924231616, 8.741805268971372556, 0.7216878364870317197 ) ) ;
#174038 = CARTESIAN_POINT ( 'NONE',  ( 3.348500752450937590, 5.890039396959305229, 1.082531754730558626 ) ) ;
#174039 = CARTESIAN_POINT ( 'NONE',  ( -5.387385936583832802, 7.378645907471495846, -1.599625672291271394 ) ) ;
#174040 = CARTESIAN_POINT ( 'NONE',  ( 6.039231080244466199, 6.010467446565510130, 0.7998128361456352531 ) ) ;
#174041 = ORIENTED_EDGE ( 'NONE', *, *, #61508, .T. ) ;
#174043 = CARTESIAN_POINT ( 'NONE',  ( 6.363545146358847937, -1.619577101098391925, -1.195656717203520403 ) ) ;
#174042 = CARTESIAN_POINT ( 'NONE',  ( 2.612652284633736777, -0.1782932461553646819, 1.832575692395449485 ) ) ;
#174044 = CARTESIAN_POINT ( 'NONE',  ( 1.353307579497017965, -1.032721833433938530, 2.053394521917959015 ) ) ;
#174045 = CARTESIAN_POINT ( 'NONE',  ( 6.192239757033616065, 0.9699301198475211994, -1.705161095427814466 ) ) ;
#174046 = CARTESIAN_POINT ( 'NONE',  ( -6.891622154448065807, 6.934647356477856128, 1.040834085586084257E-14 ) ) ;
#174047 = CARTESIAN_POINT ( 'NONE',  ( -7.100579091573050228, -6.583980363594990948, 6.484567079770452658 ) ) ;
#174048 = CARTESIAN_POINT ( 'NONE',  ( -2.761056838677368397, 6.372983411765559048, 0.7998128361456341429 ) ) ;
#174049 = DIRECTION ( 'NONE',  ( 1.000000000000000000, 0.000000000000000000, 0.000000000000000000 ) ) ;
#174050 = CARTESIAN_POINT ( 'NONE',  ( -5.659602779061863487, 5.567567761852417085, 0.7998128361456281477 ) ) ;
#174052 = CARTESIAN_POINT ( 'NONE',  ( 1.393192293617943944, 1.414286473764417185, 1.224485199485196629 ) ) ;
#174051 = CARTESIAN_POINT ( 'NONE',  ( 2.243796185194739223, 2.090353954619321275, 0.04827919579214814960 ) ) ;
#174053 = CARTESIAN_POINT ( 'NONE',  ( 2.337267334706777611, -1.242538083881424837, 1.587593183769491878 ) ) ;
#174054 = ORIENTED_EDGE ( 'NONE', *, *, #210348, .F. ) ;
#174055 = CARTESIAN_POINT ( 'NONE',  ( 0.6823417656249899377, 4.238541667008085767, -1.181850606188754593 ) ) ;
#174056 = CARTESIAN_POINT ( 'NONE',  ( 2.419155098189431641, -1.003372571555812831, -1.421874531148322740 ) ) ;
#174057 = AXIS2_PLACEMENT_3D ( 'NONE', #49343, #197701, #79697 ) ;
#174058 = CARTESIAN_POINT ( 'NONE',  ( 5.066996723205273057, 6.934582148538044777, 1.599625672291267398 ) ) ;
#174060 = CARTESIAN_POINT ( 'NONE',  ( -11.33772463945036968, 10.19999999999999929, -3.680000000000002824 ) ) ;
#174059 = CARTESIAN_POINT ( 'NONE',  ( -6.979380938965681125, -8.233137084989706977, 6.445605026751805688 ) ) ;
#174061 = CARTESIAN_POINT ( 'NONE',  ( 2.806937704738516448, 1.457146550840708210, 0.9226662414157487113 ) ) ;
#174062 = CARTESIAN_POINT ( 'NONE',  ( 2.349409277133751139, 0.5813161652389825518, -2.113004480973964760 ) ) ;
#174063 = CARTESIAN_POINT ( 'NONE',  ( 4.688207069967821106, -1.042061291317699423, 1.945354640606362873 ) ) ;
#174064 = CARTESIAN_POINT ( 'NONE',  ( -11.69084473744764097, 4.401359152538248054, -5.144113628910231384 ) ) ;
#174065 = CARTESIAN_POINT ( 'NONE',  ( 2.641674518982541020, 1.986514366401496590, -0.8763142005700165216 ) ) ;
#174066 = CARTESIAN_POINT ( 'NONE',  ( 1.347985785199314668, 1.823511463271022093, 0.09156768404049858701 ) ) ;
#174067 = CARTESIAN_POINT ( 'NONE',  ( 3.116528361068672481, 2.066776279341679956, 0.4593686614828630943 ) ) ;
#174068 = CARTESIAN_POINT ( 'NONE',  ( 3.719872605471106208, 6.605953636083950364, 7.500000000000000000 ) ) ;
#174069 = EDGE_CURVE ( 'NONE', #205917, #127875, #71316, .T. ) ;
#174070 = EDGE_LOOP ( 'NONE', ( #61305, #164737, #24385 ) ) ;
#174072 = CARTESIAN_POINT ( 'NONE',  ( 1.364683531249986537, 0.9260416670080896528, 0.7879004041258500513 ) ) ;
#174071 = CARTESIAN_POINT ( 'NONE',  ( 3.632637656275085281, 0.3374270351050281946, 2.267304333945507011 ) ) ;
#174073 = CARTESIAN_POINT ( 'NONE',  ( 11.33772463945037146, 10.89999999999998259, 3.599999999999999201 ) ) ;
#174074 = CARTESIAN_POINT ( 'NONE',  ( 4.552840656090682891, 4.206068941727564514, 1.214306433183764966E-14 ) ) ;
#174075 = CARTESIAN_POINT ( 'NONE',  ( 6.463560548549353690, -1.782115098378980855, -1.325830300435285825 ) ) ;
#174076 = CARTESIAN_POINT ( 'NONE',  ( -6.575341312947811545, 6.773579074634973551, 1.040834085586084257E-14 ) ) ;
#174077 = CARTESIAN_POINT ( 'NONE',  ( 2.887523530030648988, 6.312601851770308414, 0.000000000000000000 ) ) ;
#174078 = VECTOR ( 'NONE', #20937, 1000.000000000000000 ) ;
#174079 = CARTESIAN_POINT ( 'NONE',  ( -5.978782553502159480, 8.958701498185728695, 1.082531754730548412 ) ) ;
#174080 = CARTESIAN_POINT ( 'NONE',  ( 2.929970594329034395, 6.432399770110250437, -0.7216878364870338292 ) ) ;
#174081 = ORIENTED_EDGE ( 'NONE', *, *, #163457, .T. ) ;
#174082 = CARTESIAN_POINT ( 'NONE',  ( 4.078750125433938223, -0.7691220382576718917, 1.864168106189521890 ) ) ;
#174084 = CARTESIAN_POINT ( 'NONE',  ( 2.834894798709301611, -1.972450601023918448, -0.6029180858937719378 ) ) ;
#174083 = CARTESIAN_POINT ( 'NONE',  ( 6.745345117998789775, 7.828323044875442172, 1.199719254218462483 ) ) ;
#174085 = CARTESIAN_POINT ( 'NONE',  ( -3.994719869312852278, 3.988629890494022057, 0.6383152452940714650 ) ) ;
#174086 = CARTESIAN_POINT ( 'NONE',  ( 3.675669042636310557, 6.342012078834061484, -1.082531754730549967 ) ) ;
#174087 = CARTESIAN_POINT ( 'NONE',  ( -1.642778471874998480, -2.501041666188707158, 2.845375778867863303 ) ) ;
#174088 = CARTESIAN_POINT ( 'NONE',  ( -1.326716514427061987E-15, 2.999999999999988454, -1.225000000000003864 ) ) ;
#174089 = CARTESIAN_POINT ( 'NONE',  ( 6.087848540548081999, -2.180536604488235941, -0.2183335821156970336 ) ) ;
#174090 = CARTESIAN_POINT ( 'NONE',  ( 3.498672800139957406, -1.986100699840901651, 0.3474671148789992836 ) ) ;
#174091 = CARTESIAN_POINT ( 'NONE',  ( 2.823586671956069605, 1.020774559177588081, -1.532180179759069283 ) ) ;
#174092 = EDGE_CURVE ( 'NONE', #188860, #145094, #21448, .T. ) ;
#174093 = CARTESIAN_POINT ( 'NONE',  ( 7.481401836642521452, 7.622723652371411696, 1.040834085586084257E-14 ) ) ;
#174094 = CARTESIAN_POINT ( 'NONE',  ( 6.229513028222847026, -1.717969363144413952, 0.6179237509907066217 ) ) ;
#174095 = CIRCLE ( 'NONE', #208676, 0.07999999999999998779 ) ;
#174096 = CARTESIAN_POINT ( 'NONE',  ( -6.418895661066105873, 9.576129806964074120, -1.199719254218440723 ) ) ;
#174097 = CARTESIAN_POINT ( 'NONE',  ( 0.4919812829822337030, 1.677557865031731765, 1.518126404548009178 ) ) ;
#174098 = CARTESIAN_POINT ( 'NONE',  ( 1.840588936376737372, 2.083348874589638466, 0.3076409294043966902 ) ) ;
#174099 = CARTESIAN_POINT ( 'NONE',  ( -4.749098946536820520, 8.762642214260091933, 0.7998128361456281477 ) ) ;
#174100 = CARTESIAN_POINT ( 'NONE',  ( 7.079328764629950754, 11.41096732537697633, 0.7998128361456462443 ) ) ;
#174101 = CARTESIAN_POINT ( 'NONE',  ( 7.973603738168424826, 8.475161580717541554, 0.000000000000000000 ) ) ;
#174102 = CARTESIAN_POINT ( 'NONE',  ( 8.378074386687003994, 11.50815134976859078, 15.76159487570644124 ) ) ;
#174103 = B_SPLINE_CURVE_WITH_KNOTS ( 'NONE', 3,
 ( #37283, #185651, #70819, #172636, #90313, #206174 ),
 .UNSPECIFIED., .F., .F.,
 ( 4, 2, 4 ),
 ( 0.000000000000000000, 0.0006788971861661711581, 0.001357794372332342316 ),
 .UNSPECIFIED. ) ;
#174104 = CARTESIAN_POINT ( 'NONE',  ( -8.525379664894808585, 8.840697785332414682, -0.7998128361456291469 ) ) ;
#174105 = CARTESIAN_POINT ( 'NONE',  ( 7.769310276573728302, -5.221243112839674794, 7.769310276573704321 ) ) ;
#174106 = CARTESIAN_POINT ( 'NONE',  ( 7.958272981097359811, 9.347368568444167636, -1.082531754730537976 ) ) ;
#174107 = CARTESIAN_POINT ( 'NONE',  ( 4.026147685736890303, 7.792003671190927960, 0.3652107146706294882 ) ) ;
#174108 = CARTESIAN_POINT ( 'NONE',  ( -3.927058049452637700, 7.733318157670055371, -0.7998128361456281477 ) ) ;
#174109 = CARTESIAN_POINT ( 'NONE',  ( 4.166425639909420831, 2.220860392705526820, -0.05667459126444325535 ) ) ;
#174110 = CARTESIAN_POINT ( 'NONE',  ( 1.623246906879351581, -2.062630869249089116, 0.7406334225198917265 ) ) ;
#174111 = CARTESIAN_POINT ( 'NONE',  ( 0.2763675079364875664, 1.274320874971252460, 1.801605125401319007 ) ) ;
#174112 = CARTESIAN_POINT ( 'NONE',  ( -5.822300622425855110, 5.757381912443740646, 0.7998128361456281477 ) ) ;
#174113 = CARTESIAN_POINT ( 'NONE',  ( 4.773855682050706761, -1.924389145058275963, 0.3807478752155256663 ) ) ;
#174114 = CARTESIAN_POINT ( 'NONE',  ( 8.028399517586572998, 12.51821653715971472, -0.7998128361456352531 ) ) ;
#174115 = CARTESIAN_POINT ( 'NONE',  ( -5.357213605067637552, 6.353687308821166724, 1.098221101205157035 ) ) ;
#174116 = CARTESIAN_POINT ( 'NONE',  ( -3.946537740501743219, 2.817530495241825417, -0.7749999999999944711 ) ) ;
#174117 = CARTESIAN_POINT ( 'NONE',  ( -0.6823417656250246877, 0.05104166700808931978, 1.181850606188755259 ) ) ;
#174118 = FACE_OUTER_BOUND ( 'NONE', #172268, .T. ) ;
#174120 = ORIENTED_EDGE ( 'NONE', *, *, #7244, .F. ) ;
#174119 = CARTESIAN_POINT ( 'NONE',  ( -5.585596099150191840, 7.539614753807099667, -1.443375672974052559 ) ) ;
#174121 = CARTESIAN_POINT ( 'NONE',  ( 3.955424862866574021, -1.843446357660895041, 1.048082435718917571 ) ) ;
#174122 = CARTESIAN_POINT ( 'NONE',  ( -4.767627293860968507, 5.591261926706423857, -1.199719254218453823 ) ) ;
#174123 = CARTESIAN_POINT ( 'NONE',  ( 5.243122039519461097, -1.856066598825537373, 1.107904190987746063 ) ) ;
#174124 = CARTESIAN_POINT ( 'NONE',  ( 4.265079090171526310, 1.784866007061826298, -0.4516350764028759235 ) ) ;
#174125 = UNCERTAINTY_MEASURE_WITH_UNIT (LENGTH_MEASURE( 1.000000000000000082E-05 ), #67169, 'distance_accuracy_value', 'NONE');
#174126 = CARTESIAN_POINT ( 'NONE',  ( -5.724176140219916498, 6.114206214821067853, 0.7043541215260868960 ) ) ;
#174127 = CARTESIAN_POINT ( 'NONE',  ( -0.6823417656250003738, 1.280208333674752508, -1.181850606188749264 ) ) ;
#174128 = CARTESIAN_POINT ( 'NONE',  ( -0.006821830062568761018, -1.739981233400577088, -0.04623622425214619219 ) ) ;
#174129 = CARTESIAN_POINT ( 'NONE',  ( 6.727182134110205602, 7.053355583909074689, 2.409100679957976165 ) ) ;
#174130 = CARTESIAN_POINT ( 'NONE',  ( 2.562127843302666186, 5.932973550587659517, 0.000000000000000000 ) ) ;
#174131 = CARTESIAN_POINT ( 'NONE',  ( 11.83929459711652932, 6.804233087161206228, -1.971914732669066472 ) ) ;
#174132 = CARTESIAN_POINT ( 'NONE',  ( 4.399409362686744096, 1.734418756986338295, 1.290045131933370781 ) ) ;
#174133 = CARTESIAN_POINT ( 'NONE',  ( 5.272814466252145671, -2.006652483137221665, 0.1948127969565379425 ) ) ;
#174134 = CARTESIAN_POINT ( 'NONE',  ( -7.334597914868727919, 10.54048608644677465, -1.082531754730543083 ) ) ;
#174135 = CARTESIAN_POINT ( 'NONE',  ( 3.538091169922503276, 0.9737216987566952309, -1.930062384640649054 ) ) ;
#174136 = CARTESIAN_POINT ( 'NONE',  ( 3.760970446608974171, -1.736958583363076736, -0.9323722252271587907 ) ) ;
#174137 = ADVANCED_FACE ( 'NONE', ( #20444 ), #198666, .F. ) ;
#174138 = CARTESIAN_POINT ( 'NONE',  ( 1.062054608305310177, 0.4471719227481777414, -2.263690193671878514 ) ) ;
#174139 = CARTESIAN_POINT ( 'NONE',  ( 2.688805810584052658, -0.3489404079633807165, -2.030846992095108217 ) ) ;
#174140 = CARTESIAN_POINT ( 'NONE',  ( 5.653840721119872903, 0.7909470656678599942, 1.773883556849734644 ) ) ;
#174142 = ORIENTED_EDGE ( 'NONE', *, *, #189986, .T. ) ;
#174141 = CARTESIAN_POINT ( 'NONE',  ( -8.473482818416682605, 8.988077497682020578, -0.7216878364870267237 ) ) ;
#174144 = EDGE_CURVE ( 'NONE', #75675, #170253, #184755, .T. ) ;
#174143 = CARTESIAN_POINT ( 'NONE',  ( -5.121948170912633991, 9.197632976031879792, -0.7998128361456362523 ) ) ;
#174145 = CARTESIAN_POINT ( 'NONE',  ( -1.420000000000001039, 6.216000000000048153, -2.921333333333328675 ) ) ;
#174147 = VERTEX_POINT ( 'NONE', #64667 ) ;
#174146 = CARTESIAN_POINT ( 'NONE',  ( -3.806807270387036368, 7.663301925418665839, 0.000000000000000000 ) ) ;
#174148 = CARTESIAN_POINT ( 'NONE',  ( -8.202319746143382773, 9.632089794331152532, 1.082531754730558626 ) ) ;
#174149 = CARTESIAN_POINT ( 'NONE',  ( 1.887996149947854807, 1.521953097117642706, 1.598203399828190152 ) ) ;
#174150 = CARTESIAN_POINT ( 'NONE',  ( 0.000000000000000000, -3.784374999522044369, -3.793834371823813001 ) ) ;
#174151 = CARTESIAN_POINT ( 'NONE',  ( 6.825062041929172985, -1.792332737533608666, -0.7979697884207545000 ) ) ;
#174152 = CARTESIAN_POINT ( 'NONE',  ( 6.539320575229278454, 2.035006821797652687, 2.408631514295301645 ) ) ;
#174153 = CARTESIAN_POINT ( 'NONE',  ( -0.7500000000000215383, 3.722916667349487785, 1.299038105676671107 ) ) ;
#174154 = CARTESIAN_POINT ( 'NONE',  ( 4.581598608702507569, 7.168929433314090716, -1.325851593340146461 ) ) ;
#174155 = CARTESIAN_POINT ( 'NONE',  ( -6.402982088906444602, 6.898597865962027065, -0.7910698893406533649 ) ) ;
#174156 = CARTESIAN_POINT ( 'NONE',  ( 4.874869531740305462, 1.716800804850382223, -0.6655867697097292979 ) ) ;
#174157 = ORIENTED_EDGE ( 'NONE', *, *, #154365, .T. ) ;
#174159 = CARTESIAN_POINT ( 'NONE',  ( 2.114203836804037007, -0.9703286663178596338, -1.818149309968750016 ) ) ;
#174158 = ADVANCED_BREP_SHAPE_REPRESENTATION ( '', ( #26340, #200407 ), #27579 ) ;
#174160 = CARTESIAN_POINT ( 'NONE',  ( 1.360316468749985575, 0.2864583336747233422, -0.7853790794158961308 ) ) ;
#174161 = UNCERTAINTY_MEASURE_WITH_UNIT (LENGTH_MEASURE( 1.000000000000000082E-05 ), #185150, 'distance_accuracy_value', 'NONE');
#174162 = CARTESIAN_POINT ( 'NONE',  ( -7.867809214632013770, 8.073532260025807261, 1.040834085586084257E-14 ) ) ;
#174163 = CARTESIAN_POINT ( 'NONE',  ( 0.000000000000000000, 0.4000000000000010214, 0.000000000000000000 ) ) ;
#174164 = CARTESIAN_POINT ( 'NONE',  ( 11.95359438121989371, 11.10421899708699200, 1.059536798430487314 ) ) ;
#174165 = CARTESIAN_POINT ( 'NONE',  ( 5.335297142177534369, 6.183267073083954735, -1.199719254218452047 ) ) ;
#174166 = CARTESIAN_POINT ( 'NONE',  ( 0.4618819262211275034, 2.038552468250200533, -0.3016747405163843765 ) ) ;
#174168 = CARTESIAN_POINT ( 'NONE',  ( 4.476008884455379366, -1.787108923542475525, -0.4427587100873929815 ) ) ;
#174167 = CARTESIAN_POINT ( 'NONE',  ( 4.879351199879441658, 4.945478990385278273, 0.6233296712930589401 ) ) ;
#174169 = CARTESIAN_POINT ( 'NONE',  ( 7.416473721875251890, 8.611306416064660851, 1.199719254218462483 ) ) ;
#174170 = CARTESIAN_POINT ( 'NONE',  ( -4.911522990386917975, 4.699272633198016358, 0.3641131004739307508 ) ) ;
#174171 = CARTESIAN_POINT ( 'NONE',  ( -6.317173229324657413, 6.334733287159020954, 0.000000000000000000 ) ) ;
#174173 = ORIENTED_EDGE ( 'NONE', *, *, #75043, .T. ) ;
#174172 = CARTESIAN_POINT ( 'NONE',  ( 6.610000000000008313, 7.629137130509070275, 2.600000000000001421 ) ) ;
#174174 =( GEOMETRIC_REPRESENTATION_CONTEXT ( 3 ) GLOBAL_UNCERTAINTY_ASSIGNED_CONTEXT ( ( #195144 ) ) GLOBAL_UNIT_ASSIGNED_CONTEXT ( ( #111671, #57524, #179805 ) ) REPRESENTATION_CONTEXT ( 'NONE', 'WORKASPACE' ) );
#174175 = CARTESIAN_POINT ( 'NONE',  ( 4.301547675229603129, 1.771612934706376707, 1.315755017190944676 ) ) ;
#174176 = CARTESIAN_POINT ( 'NONE',  ( 0.8433209000573947955, -1.854398715148808385, 1.110445933987347367 ) ) ;
#174177 = CARTESIAN_POINT ( 'NONE',  ( -4.880572111239580124, 7.677455982212699759, 1.082531754730560403 ) ) ;
#174178 = CARTESIAN_POINT ( 'NONE',  ( 0.2110004604562870645, 1.588762659912812403, -1.064147093309028680 ) ) ;
#174179 = CARTESIAN_POINT ( 'NONE',  ( 6.491422787562372676, -0.4091076066058823013, 1.878265147811091662 ) ) ;
#174180 = CARTESIAN_POINT ( 'NONE',  ( -3.022498986271247023, 2.800000000000024691, -2.500000000000000444 ) ) ;
#174181 = CYLINDRICAL_SURFACE ( 'NONE', #135866, 0.08000000000000020983 ) ;
#174182 = CARTESIAN_POINT ( 'NONE',  ( 5.707647354773449422, 1.450964518888698596, 1.245719642194928589 ) ) ;
#174183 =( NAMED_UNIT ( * ) SI_UNIT ( $, .STERADIAN. ) SOLID_ANGLE_UNIT ( ) );
#174185 = AXIS2_PLACEMENT_3D ( 'NONE', #46261, #209788, #177318 ) ;
#174184 = CARTESIAN_POINT ( 'NONE',  ( 0.4791068267422092797, 1.747065859276742072, -0.6691465683838908607 ) ) ;
#174186 = CARTESIAN_POINT ( 'NONE',  ( 2.694546298722868549, 1.457235452327232395, -1.394086077981852911 ) ) ;
#174188 = CARTESIAN_POINT ( 'NONE',  ( 4.389357127182037743, 1.881541760944308139, -0.9463713395347850277 ) ) ;
#174187 = CARTESIAN_POINT ( 'NONE',  ( -6.842061076390810292, 11.13415502243129218, 0.000000000000000000 ) ) ;
#174189 = CARTESIAN_POINT ( 'NONE',  ( 7.609150525767641504, 9.900428251527500834, -1.599625672291262513 ) ) ;
#174191 = CARTESIAN_POINT ( 'NONE',  ( -7.527801604085656351, 9.805521176231838609, 1.599625672291295375 ) ) ;
#174190 = CARTESIAN_POINT ( 'NONE',  ( 0.7499999999999885647, 0.2333333333333562076, 1.299038105676657340 ) ) ;
#174192 = CARTESIAN_POINT ( 'NONE',  ( 11.52901446936746588, 9.805744725324114341, 3.330874149801137829 ) ) ;
#174193 = CARTESIAN_POINT ( 'NONE',  ( 3.779560859189102562, 0.2429267963163626032, -2.005027992008329818 ) ) ;
#174194 = CARTESIAN_POINT ( 'NONE',  ( 0.6823417656249899377, 5.426041667008087543, -1.181850606188754593 ) ) ;
#174195 = CARTESIAN_POINT ( 'NONE',  ( 9.246297574839980271, 10.85006392781057905, 1.082531754730549967 ) ) ;
#174196 = CARTESIAN_POINT ( 'NONE',  ( 4.112696061561730509, 1.531809107248631507, -1.525399859652858847 ) ) ;
#174197 = CARTESIAN_POINT ( 'NONE',  ( 5.664274315459256748, 9.830346811336296398, -0.7998128361456481317 ) ) ;
#174198 = CARTESIAN_POINT ( 'NONE',  ( -1.201851678989727383E-14, 4.837500000000018119, -1.732050807568863648 ) ) ;
#174200 = DIRECTION ( 'NONE',  ( -0.04888523518676889112, 8.339466111204228823E-16, -0.9988044021632737079 ) ) ;
#174199 = CARTESIAN_POINT ( 'NONE',  ( 5.180097208873055692, 8.201141289397330780, -1.199719254218450271 ) ) ;
#174201 = CARTESIAN_POINT ( 'NONE',  ( 8.392133896734662812, 10.81390885098904420, 1.443375672974076540 ) ) ;
#174203 = CARTESIAN_POINT ( 'NONE',  ( -1.992711204631002198E-15, 2.999999999999989342, 1.224999999999989875 ) ) ;
#174202 = CARTESIAN_POINT ( 'NONE',  ( 2.260437933566094681, -2.170709518246512815, 0.05174924654302060639 ) ) ;
#174205 = CARTESIAN_POINT ( 'NONE',  ( 1.206327419354651820, 1.623952629372883427, 0.8676893986077349741 ) ) ;
#174204 = CARTESIAN_POINT ( 'NONE',  ( -7.063434843039784639, 7.343021526408956667, 1.040834085586084257E-14 ) ) ;
#174206 = CARTESIAN_POINT ( 'NONE',  ( -0.6823417656250003738, 1.467708333674752730, -1.181850606188749264 ) ) ;
#174207 = CARTESIAN_POINT ( 'NONE',  ( 2.911879292414458309, -1.082406496695037301, -1.905547650945007776 ) ) ;
#174208 = CARTESIAN_POINT ( 'NONE',  ( 6.313255789627134185, 6.931427761816202349, -0.8697005975955690582 ) ) ;
#174209 = CARTESIAN_POINT ( 'NONE',  ( 3.766728628225763043, -1.521468805364207144, 1.674700015324230407 ) ) ;
#174210 = CARTESIAN_POINT ( 'NONE',  ( -8.044065211609668253, 8.279164256499745633, 0.7998128361456602331 ) ) ;
#174211 = CARTESIAN_POINT ( 'NONE',  ( 4.663296154398564042, 1.879804967172087782, -0.7303043177912388328 ) ) ;
#174212 = CARTESIAN_POINT ( 'NONE',  ( 1.364683531249990311, 4.676041667008083103, 0.7879004041258500513 ) ) ;
#174213 = CARTESIAN_POINT ( 'NONE',  ( 6.469672735924913987, 6.762149564967588233, 0.2594904213018677797 ) ) ;
#174214 = CARTESIAN_POINT ( 'NONE',  ( 1.500000000000001332, 12.12499999999999645, 0.000000000000000000 ) ) ;
#174215 = CARTESIAN_POINT ( 'NONE',  ( 7.214347136247488912, 7.589362211809770997, -0.7216878364870317197 ) ) ;
#174216 = CARTESIAN_POINT ( 'NONE',  ( 4.657331418887999064, 0.3884847549131437705, -1.726375946583807774 ) ) ;
#174217 = CARTESIAN_POINT ( 'NONE',  ( 9.433775957010412938, 9.900493459467314850, 0.000000000000000000 ) ) ;
#174218 = CARTESIAN_POINT ( 'NONE',  ( 1.237491679122425969, -1.904027454836676014, 0.9001316648933003206 ) ) ;
#174220 = CARTESIAN_POINT ( 'NONE',  ( -1.201851678989727383E-14, 1.212500000000025002, 1.732050807568877637 ) ) ;
#174219 = CARTESIAN_POINT ( 'NONE',  ( 1.364683531250000303, 11.25520833367473550, -0.7879004041258355073 ) ) ;
#174221 = CARTESIAN_POINT ( 'NONE',  ( 0.9241884870439884825, 0.9676023207046909880, 1.715383555584276909 ) ) ;
#174222 = CARTESIAN_POINT ( 'NONE',  ( -5.469788628470539926, 5.346117919495872783, -0.7998128361456362523 ) ) ;
#174223 = CARTESIAN_POINT ( 'NONE',  ( 5.800407700000974387, 1.352143934286989868, -1.496062775417882129 ) ) ;
#174224 = ORIENTED_EDGE ( 'NONE', *, *, #207104, .T. ) ;
#174225 = CARTESIAN_POINT ( 'NONE',  ( 7.293923454472087897, 8.572294120714675003, 1.082531754730558626 ) ) ;
#174226 = CARTESIAN_POINT ( 'NONE',  ( 4.381629165553334815, 1.221847395770376377, 1.416585496670008659 ) ) ;
#174227 = CIRCLE ( 'NONE', #122346, 4.000000000000000000 ) ;
#174228 = CARTESIAN_POINT ( 'NONE',  ( 4.047765473330780850, 1.496028175931501947, 1.431257568052332729 ) ) ;
#174229 = COLOUR_RGB ( '', 0.66274510, 0.83137255, 0.94901961) ;
#174230 = CARTESIAN_POINT ( 'NONE',  ( -1.225000000000046052, 2.520833333333404092, 0.7072540797572777205 ) ) ;
#174231 = CARTESIAN_POINT ( 'NONE',  ( -5.682275777458886346, 7.722684055159061423, 1.443375672974058777 ) ) ;
#174232 = CARTESIAN_POINT ( 'NONE',  ( -11.04536101718726293, 10.90000000000000036, -1.100000000000002087 ) ) ;
#174233 = CARTESIAN_POINT ( 'NONE',  ( 8.697719238366680372, 10.10609285197134533, 1.199719254218462483 ) ) ;
#174234 = CARTESIAN_POINT ( 'NONE',  ( -10.31505594189871111, 10.92865344183699428, -0.7998128361456291469 ) ) ;
#174235 = CARTESIAN_POINT ( 'NONE',  ( 5.996449078994045223, 10.21788403546024782, 0.7998128361456331437 ) ) ;
#174236 = CIRCLE ( 'NONE', #115508, 11.29999999999998828 ) ;
#174237 = CARTESIAN_POINT ( 'NONE',  ( 1.836970198721030181E-16, 13.49999999999999822, 1.500000000000000222 ) ) ;
#174238 = CARTESIAN_POINT ( 'NONE',  ( -0.6823417656250212460, 5.613541667008087543, 1.181850606188767472 ) ) ;
#174239 = CARTESIAN_POINT ( 'NONE',  ( 4.141029529442549872, -0.1900441490861082827, -1.952618137025011746 ) ) ;
#174240 = CARTESIAN_POINT ( 'NONE',  ( 1.862657450031137474, -0.6818942500997280387, 1.897406292459068222 ) ) ;
#174241 = CARTESIAN_POINT ( 'NONE',  ( -3.311934663488232733, 7.085950550703385531, -0.7998128361456481317 ) ) ;
#174242 = VECTOR ( 'NONE', #34882, 1000.000000000000000 ) ;
#174243 = CARTESIAN_POINT ( 'NONE',  ( 6.639320575229252341, 2.457876053485750223, 2.280608551775892501 ) ) ;
#174244 = CARTESIAN_POINT ( 'NONE',  ( 1.387741975113141235, -0.8460221195879283895, 1.668388151239764028 ) ) ;
#174245 = CARTESIAN_POINT ( 'NONE',  ( -1.201851678989727383E-14, 4.071875000341425022, 1.575800808251672791 ) ) ;
#174246 = CARTESIAN_POINT ( 'NONE',  ( 3.093996842688331750, 1.280297628565935097, 1.553616095213964154 ) ) ;
#174248 = CARTESIAN_POINT ( 'NONE',  ( 3.902059883959855924, -1.090250183479730461, -1.814828101457645060 ) ) ;
#174247 = CARTESIAN_POINT ( 'NONE',  ( -5.910991785878170646, 7.919243054989755670, -1.443375672974059665 ) ) ;
#174249 = DIRECTION ( 'NONE',  ( 0.000000000000000000, 0.000000000000000000, 1.000000000000000000 ) ) ;
#174250 = CARTESIAN_POINT ( 'NONE',  ( 5.230950013807261101, -1.948248037745937022, -0.7008574099531189594 ) ) ;
#174251 = CARTESIAN_POINT ( 'NONE',  ( 7.452141709366786770, 8.723195411463290583, 1.199719254218452047 ) ) ;
#174253 = DIRECTION ( 'NONE',  ( 0.000000000000000000, 0.000000000000000000, -1.000000000000000000 ) ) ;
#174252 = CARTESIAN_POINT ( 'NONE',  ( 0.2399332258718233080, 2.085444179493881389, 0.1495565104911322774 ) ) ;
#174255 = ORIENTED_EDGE ( 'NONE', *, *, #114444, .T. ) ;
#174254 = CARTESIAN_POINT ( 'NONE',  ( 5.526323803393728085, 1.085782926936417425, -1.467421699745217412 ) ) ;
#174256 = CARTESIAN_POINT ( 'NONE',  ( 8.239604668803105270, 10.63595808506888396, -1.599625672291268286 ) ) ;
#174257 = DIRECTION ( 'NONE',  ( 0.8079921913670625733, 0.000000000000000000, -0.5891931930104522541 ) ) ;
#174258 = CARTESIAN_POINT ( 'NONE',  ( 2.855963913973019963, 6.483708332943829866, 0.000000000000000000 ) ) ;
#174259 = CARTESIAN_POINT ( 'NONE',  ( -10.67000816626867810, 5.238978589329153834, 6.814456324518622488 ) ) ;
#174260 = CARTESIAN_POINT ( 'NONE',  ( 0.6823417656249934904, 12.25520833367473017, 1.181850606188764807 ) ) ;
#174261 = CARTESIAN_POINT ( 'NONE',  ( 6.481121912432155519, -1.750430003815309998, -0.7703581994758443852 ) ) ;
#174262 = CARTESIAN_POINT ( 'NONE',  ( -9.508345801885592863, 9.987491611821676329, 0.7998128361456462443 ) ) ;
#174263 = CARTESIAN_POINT ( 'NONE',  ( 6.063521013809720195, 8.097193820909906137, 1.599625672291281386 ) ) ;
#174264 = CARTESIAN_POINT ( 'NONE',  ( 1.360316468749978469, 2.296875000341369599, -4.857225732735059864E-14 ) ) ;
#174265 = DIRECTION ( 'NONE',  ( 1.014813233446432150E-15, 1.000000000000000000, -4.583713267641621330E-32 ) ) ;
#174266 = CARTESIAN_POINT ( 'NONE',  ( 5.834086172582112262, 5.700855377634248100, 1.040834085586084257E-14 ) ) ;
#174267 = ORIENTED_EDGE ( 'NONE', *, *, #100809, .T. ) ;
#174268 = CARTESIAN_POINT ( 'NONE',  ( -5.803772275101700906, 8.928762199997411386, -1.199719254218452047 ) ) ;
#174269 = EDGE_CURVE ( 'NONE', #210464, #92865, #49173, .T. ) ;
#174270 = CARTESIAN_POINT ( 'NONE',  ( 5.325796065338770369, 0.8146125389149364571, -1.844717355016491478 ) ) ;
#174271 = DIRECTION ( 'NONE',  ( 0.7071067811865462405, 0.000000000000000000, -0.7071067811865489050 ) ) ;
#174272 = CARTESIAN_POINT ( 'NONE',  ( -6.457230086593013674, 6.786253674495239530, 0.3580049749655131452 ) ) ;
#174273 = CARTESIAN_POINT ( 'NONE',  ( -6.263503779833496488, 6.409768619334935913, 0.7216878364870317197 ) ) ;
#174274 = CARTESIAN_POINT ( 'NONE',  ( 4.871457266011829823, 4.577788319968905562, -0.7998128361456221525 ) ) ;
#174275 = CARTESIAN_POINT ( 'NONE',  ( 2.711712322018722698, 0.5300763513187057852, -1.896665901777684127 ) ) ;
#174276 = CARTESIAN_POINT ( 'NONE',  ( 3.761342352588430860, 1.897692735847063661, -0.6820134568972098243 ) ) ;
#174277 = CARTESIAN_POINT ( 'NONE',  ( -6.886651960737580680, 10.12184548991413457, -1.199719254218440723 ) ) ;
#174278 = CARTESIAN_POINT ( 'NONE',  ( 6.827182134110224787, 2.015384445464900587, 2.492173930675382731 ) ) ;
#174279 = CARTESIAN_POINT ( 'NONE',  ( 3.820431320580887302, 2.080737768064028437, 0.6879518193209921417 ) ) ;
#174280 = CARTESIAN_POINT ( 'NONE',  ( 1.607015867998825343, 0.9165151389911689872, 1.199999999999999734 ) ) ;
#174281 = CARTESIAN_POINT ( 'NONE',  ( 2.291906413246731944, -0.8257142216546548008, 1.740595036569925647 ) ) ;
#174282 = CARTESIAN_POINT ( 'NONE',  ( -8.565000355531095622, 11.01558638625153286, -1.599625672291263179 ) ) ;
#174283 = CARTESIAN_POINT ( 'NONE',  ( -0.1296875068447916890, 6.948706544289747988, -2.421546651465163347 ) ) ;
#174284 = CARTESIAN_POINT ( 'NONE',  ( 0.2329586101569892376, 6.948071080078905837, -2.440796105365902857 ) ) ;
#174285 = SURFACE_STYLE_USAGE ( .BOTH. , #203528 ) ;
#174286 = CARTESIAN_POINT ( 'NONE',  ( 8.308449207076147758, 8.587612251210650527, -0.7998128361456281477 ) ) ;
#174287 = CARTESIAN_POINT ( 'NONE',  ( 5.497994985541524215, 6.373081223675282736, -1.199719254218445830 ) ) ;
#174288 = CARTESIAN_POINT ( 'NONE',  ( -6.984891963202824350, -8.199734048663005481, 6.439526774796434871 ) ) ;
#174289 = CARTESIAN_POINT ( 'NONE',  ( 5.560252395380215873, 6.619954228432645138, 1.082531754730549078 ) ) ;
#174290 = ORIENTED_EDGE ( 'NONE', *, *, #72253, .F. ) ;
#174292 = CARTESIAN_POINT ( 'NONE',  ( 3.018229385809416687, -2.010681777978724494, 0.1011178238035769505 ) ) ;
#174291 = CARTESIAN_POINT ( 'NONE',  ( 5.565905774130330386, -1.163279849954502287, 1.427249551226833502 ) ) ;
#174293 = CARTESIAN_POINT ( 'NONE',  ( 4.710533686004090725, -1.772996550310073971, -1.462542180504990075 ) ) ;
#174295 = CARTESIAN_POINT ( 'NONE',  ( 2.729178580549945110, 0.09652143117058623045, -1.858595261477024918 ) ) ;
#174294 = CARTESIAN_POINT ( 'NONE',  ( -0.1290005225502398323, 0.2247172878383028038, -2.207197350255707402 ) ) ;
#174296 = CARTESIAN_POINT ( 'NONE',  ( -3.285556943750000514, -1.188541666188710044, -1.896917185911906500 ) ) ;
#174297 = CARTESIAN_POINT ( 'NONE',  ( -4.827315259302275230, 8.191461316972679541, -0.9557250891021950023 ) ) ;
#174298 = FACE_OUTER_BOUND ( 'NONE', #193968, .T. ) ;
#174299 = CARTESIAN_POINT ( 'NONE',  ( -7.802881099864745984, 9.062115023719057305, -1.199719254218446718 ) ) ;
#174300 = CARTESIAN_POINT ( 'NONE',  ( -5.153507786970276783, 6.145418851954329575, -1.082531754730549967 ) ) ;
#174301 = CARTESIAN_POINT ( 'NONE',  ( 6.023005994326640078, -1.968326514718239828, 0.7052485104920204195 ) ) ;
#174302 = CARTESIAN_POINT ( 'NONE',  ( 6.480434237652132445, 7.623223367758051872, 1.082531754730558626 ) ) ;
#174303 = EDGE_LOOP ( 'NONE', ( #149557, #63565, #97657, #109465 ) ) ;
#174304 = DIRECTION ( 'NONE',  ( 0.000000000000000000, 0.000000000000000000, 1.000000000000000000 ) ) ;
#174305 = DIRECTION ( 'NONE',  ( 0.9486832980505138790, -0.3162277660168376636, -3.312310031615527152E-15 ) ) ;
#174306 = CARTESIAN_POINT ( 'NONE',  ( 6.721331452548120922, -0.1233026559786208343, 1.696394328608492819 ) ) ;
#174307 = CARTESIAN_POINT ( 'NONE',  ( -4.401593425930945713, 8.286942763561420122, 1.040834085586084257E-14 ) ) ;
#174308 = TOROIDAL_SURFACE ( 'NONE', #25539, 8.300000000000000711, 0.2000000000000000111 ) ;
#174309 = CARTESIAN_POINT ( 'NONE',  ( 1.459138885926267504, -1.646488293146914472, -0.5446327844310631106 ) ) ;
#174310 = CARTESIAN_POINT ( 'NONE',  ( -8.120005463787672184, 14.55205930359461242, 8.786303532376779302 ) ) ;
#174311 = DIRECTION ( 'NONE',  ( 0.000000000000000000, 1.000000000000000000, 0.000000000000000000 ) ) ;
#174312 = CARTESIAN_POINT ( 'NONE',  ( -5.796211742350026341, 6.069872996917573538, -0.5622600474562855499 ) ) ;
#174313 = CARTESIAN_POINT ( 'NONE',  ( 6.368071955308375998, -2.155667716570781156, 0.2575352064990812928 ) ) ;
#174314 = CARTESIAN_POINT ( 'NONE',  ( 4.195794211080963620, -0.6966935528937777677, 1.687730213881050600 ) ) ;
#174315 = CARTESIAN_POINT ( 'NONE',  ( 2.360140415366945188, -1.961439503465340239, 0.04308618615556784187 ) ) ;
#174316 = CARTESIAN_POINT ( 'NONE',  ( 10.62873463776380056, 9.799999999999982947, 3.199999999999997957 ) ) ;
#174317 = CARTESIAN_POINT ( 'NONE',  ( -8.805130697071332335, 12.36007068230351358, 1.199719254218462483 ) ) ;
#174318 = CARTESIAN_POINT ( 'NONE',  ( 8.239604668803105270, 10.63595808506888396, -1.599625672291268286 ) ) ;
#174319 = CARTESIAN_POINT ( 'NONE',  ( 3.211701520346501582, 1.672844727185973657, 1.303009041611735030 ) ) ;
#174320 = CARTESIAN_POINT ( 'NONE',  ( 1.637338291174485510E-15, -6.530144695498204754, 11.00000000000000178 ) ) ;
#174321 = DIRECTION ( 'NONE',  ( -1.000000000000000000, -2.664535259100375697E-15, 0.000000000000000000 ) ) ;
#174322 = CARTESIAN_POINT ( 'NONE',  ( -4.989408424308831691, 6.622959204541034595, -1.241733208710007696 ) ) ;
#174323 = CARTESIAN_POINT ( 'NONE',  ( 0.8837443060279138729, -1.967007789996034095, 0.6459356165888497925 ) ) ;
#174325 = CARTESIAN_POINT ( 'NONE',  ( -0.7500000000000006661, 14.73958333401613530, -1.299038105676657340 ) ) ;
#174324 = CARTESIAN_POINT ( 'NONE',  ( -11.07693626658230990, 1.970899860167826700, 4.005980692924094200 ) ) ;
#174327 = VERTEX_POINT ( 'NONE', #65700 ) ;
#174326 = CARTESIAN_POINT ( 'NONE',  ( 3.686370400671713732, 1.234840205895268328, 1.846255301073204791 ) ) ;
#174328 = CARTESIAN_POINT ( 'NONE',  ( 1.653414166010831243, 1.186659091926351106, 1.968620417403597944 ) ) ;
#174330 = CARTESIAN_POINT ( 'NONE',  ( 6.596538677256176264, 2.039275035945103731, 0.3085339683557372092 ) ) ;
#174329 = CARTESIAN_POINT ( 'NONE',  ( 9.327646496521982300, 11.90534021740758064, -1.443375672974057666 ) ) ;
#174332 = CARTESIAN_POINT ( 'NONE',  ( 1.642778471875001811, -3.842708332855375275, 2.845375778867859751 ) ) ;
#174331 = CARTESIAN_POINT ( 'NONE',  ( 3.230585741806197841, 6.991043475407723307, 0.7998128361456271485 ) ) ;
#174333 = DIRECTION ( 'NONE',  ( -0.000000000000000000, -1.000000000000000000, -0.000000000000000000 ) ) ;
#174334 = CARTESIAN_POINT ( 'NONE',  ( -10.97113184882213766, -5.223163831703878657, 0.3618152180564682685 ) ) ;
#174335 = CARTESIAN_POINT ( 'NONE',  ( -5.631423255934748795, 6.172511151708975241, -0.8413464574193817436 ) ) ;
#174336 = ADVANCED_FACE ( 'NONE', ( #131848 ), #159712, .T. ) ;
#174337 = CARTESIAN_POINT ( 'NONE',  ( -0.1106727585415837045, 2.871245121144291090, -2.491938459964110120 ) ) ;
#174338 = CARTESIAN_POINT ( 'NONE',  ( 2.766273355629506714, -1.191139867243676598, 1.247637197061921555 ) ) ;
#174339 = CARTESIAN_POINT ( 'NONE',  ( 2.800017839408690090, -0.9981255096969069429, -1.752139039461996006 ) ) ;
#174340 = CARTESIAN_POINT ( 'NONE',  ( 3.270466940867942984, 2.077131924838520050, -0.9849289250120364381 ) ) ;
#174341 = CARTESIAN_POINT ( 'NONE',  ( 3.058202344463755828, 2.251794067479270911, -0.2186341555679652271 ) ) ;
#174342 = CARTESIAN_POINT ( 'NONE',  ( 4.828798294617491216, 2.015104956129540881, 0.6122756557535751210 ) ) ;
#174343 = CARTESIAN_POINT ( 'NONE',  ( -5.153507786970262572, 9.026526494858359229, -0.7216878364870338292 ) ) ;
#174344 = CARTESIAN_POINT ( 'NONE',  ( 3.848697245170757508, -1.448060206101034808, 1.017097547381773159 ) ) ;
#174346 = CARTESIAN_POINT ( 'NONE',  ( 5.864811835480173485, 0.1724426041235416485, -2.285918041817245783 ) ) ;
#174345 = CARTESIAN_POINT ( 'NONE',  ( 6.003228155800906407, 10.22579295840155744, 0.000000000000000000 ) ) ;
#174347 = CARTESIAN_POINT ( 'NONE',  ( 5.191278274421009975, -0.6593680717656666967, 1.719199333795925710 ) ) ;
#174348 = CARTESIAN_POINT ( 'NONE',  ( -2.449219305563052895, 6.009172956465517856, 1.040834085586084257E-14 ) ) ;
#174349 = CARTESIAN_POINT ( 'NONE',  ( 3.999292125906894313, 7.609665213625947722, 0.7216878364870317197 ) ) ;
#174350 = CARTESIAN_POINT ( 'NONE',  ( -0.7500000000000215383, 3.191666666666689967, 1.299038105676671107 ) ) ;
#174351 = CARTESIAN_POINT ( 'NONE',  ( 4.945371362016416583, 0.6893947036107104243, -2.080263006054481334 ) ) ;
#174352 = CARTESIAN_POINT ( 'NONE',  ( -3.379006598303881059, 4.965260336153046516, -1.599625672291256295 ) ) ;
#174353 = CARTESIAN_POINT ( 'NONE',  ( -5.556597592091960358, 15.44691531748820168, 10.59560191213078717 ) ) ;
#174354 = EDGE_CURVE ( 'NONE', #182393, #170502, #46687, .T. ) ;
#174355 = CARTESIAN_POINT ( 'NONE',  ( 5.898901817742318698, 0.4001337562283372451, 2.031160294743330486 ) ) ;
#174356 = CARTESIAN_POINT ( 'NONE',  ( -0.06521966986864842497, -1.616690375843790051, 1.205047459138554045 ) ) ;
#174357 = CARTESIAN_POINT ( 'NONE',  ( 1.364683531249990311, 4.884375000341417916, 1.214306433183764966E-14 ) ) ;
#174358 = CARTESIAN_POINT ( 'NONE',  ( 3.018101299323606046, -0.9500872288037317537, -1.675862364343786215 ) ) ;
#174359 = CARTESIAN_POINT ( 'NONE',  ( -1.364683531250000748, 9.859375000341398021, 0.000000000000000000 ) ) ;
#174360 = DIRECTION ( 'NONE',  ( -1.000000000000000000, -3.451266460341925773E-31, -8.638326563840809144E-31 ) ) ;
#174361 = CARTESIAN_POINT ( 'NONE',  ( 6.486587849989844834, -1.303813291173651301, 1.673118453357678392 ) ) ;
#174362 = EDGE_LOOP ( 'NONE', ( #74316, #29617, #148469, #51972, #137451 ) ) ;
#174364 = DIRECTION ( 'NONE',  ( -0.000000000000000000, 1.000000000000000000, -0.000000000000000000 ) ) ;
#174363 = CARTESIAN_POINT ( 'NONE',  ( -3.689227196694346400, 6.357829925235092716, -1.082531754730546636 ) ) ;
#174365 = CARTESIAN_POINT ( 'NONE',  ( 5.379888026524302980, 5.170957540566797128, -0.7998128361456211532 ) ) ;
#174366 = CARTESIAN_POINT ( 'NONE',  ( 7.735357998705605809, -5.759585062615364848, -7.724608556409205740 ) ) ;
#174367 = CARTESIAN_POINT ( 'NONE',  ( 11.92619526913699524, 11.02780024161490324, -1.328859060402685976 ) ) ;
#174368 = CARTESIAN_POINT ( 'NONE',  ( 11.22789937895645096, 8.808731784781956620, -4.106656770659993683 ) ) ;
#174369 = DIRECTION ( 'NONE',  ( -0.6783731810844091381, 3.929830605827845711E-15, -0.7347175152297782397 ) ) ;
#174370 = CARTESIAN_POINT ( 'NONE',  ( 1.012071980069820132, 1.959787197952606252, -0.09269708818125663163 ) ) ;
#174371 = CARTESIAN_POINT ( 'NONE',  ( 1.364683531249986537, 0.9677083336747538400, -0.7879004041258239610 ) ) ;
#174372 = CARTESIAN_POINT ( 'NONE',  ( 11.88168329227127096, 12.21999999999998288, 1.685799833707125606 ) ) ;
#174373 = CARTESIAN_POINT ( 'NONE',  ( 5.969191311310417802, 1.729517061547349632, 0.9261464158661563140 ) ) ;
#174374 = CARTESIAN_POINT ( 'NONE',  ( -9.321394304595349567, 10.83371376257142416, 1.199719254218462483 ) ) ;
#174375 = CARTESIAN_POINT ( 'NONE',  ( -4.677199806590235376, 7.440188293455128665, 1.082531754730560403 ) ) ;
#174376 = CARTESIAN_POINT ( 'NONE',  ( 0.09312846265441956928, -0.5046389715205062965, -2.214118724221309620 ) ) ;
#174378 = ORIENTED_EDGE ( 'NONE', *, *, #43445, .F. ) ;
#174377 = CARTESIAN_POINT ( 'NONE',  ( -3.475000000000000533, 0.000000000000000000, 0.000000000000000000 ) ) ;
#174379 = CARTESIAN_POINT ( 'NONE',  ( 0.6823417656249917140, 5.092708333674749177, 1.181850606188765695 ) ) ;
#174380 = CARTESIAN_POINT ( 'NONE',  ( 0.3681424317822541425, -1.226883886190757611, 1.412057460252094554 ) ) ;
#174381 = CARTESIAN_POINT ( 'NONE',  ( 5.641838915941918664, -0.04494510194943436565, -1.733422878500885167 ) ) ;
#174382 = VECTOR ( 'NONE', #139305, 1000.000000000000000 ) ;
#174383 = ADVANCED_FACE ( 'NONE', ( #34292 ), #214074, .T. ) ;
#174385 = CARTESIAN_POINT ( 'NONE',  ( 3.263397454411249399, 2.137687552337414587, -0.4822058812353549606 ) ) ;
#174384 = CARTESIAN_POINT ( 'NONE',  ( -1.360316468750040642, 1.161458333674751486, 0.7853790794158861388 ) ) ;
#174386 = CARTESIAN_POINT ( 'NONE',  ( 4.296143005555221883, -0.8870401112092487494, 2.130475988740585080 ) ) ;
#174387 = CARTESIAN_POINT ( 'NONE',  ( 6.520785525839065677, 1.921145329286999326, 0.7461220883302563944 ) ) ;
#174388 = CARTESIAN_POINT ( 'NONE',  ( 1.956878712445113244, 0.3320500349934927820, -1.913199751371328361 ) ) ;
#174389 = CARTESIAN_POINT ( 'NONE',  ( -5.219525951136856357, 6.152163700156858539, -1.082531754730543971 ) ) ;
#174390 = EDGE_CURVE ( 'NONE', #169074, #181560, #66289, .T. ) ;
#174391 = CARTESIAN_POINT ( 'NONE',  ( 11.80248046418316044, 11.29999999999998117, 1.695421849633139466 ) ) ;
#174392 = CARTESIAN_POINT ( 'NONE',  ( 4.658503719480325600, 2.115088938745744329, 0.1532479335744421078 ) ) ;
#174393 = CARTESIAN_POINT ( 'NONE',  ( 3.147111449167848019, 0.9091449406319618287, 1.799922684605055556 ) ) ;
#174394 = CARTESIAN_POINT ( 'NONE',  ( -4.189106276498259618, 6.870745841681152655, 1.082531754730560403 ) ) ;
#174395 = CARTESIAN_POINT ( 'NONE',  ( -8.106849506328558164, 8.422688943663599659, 0.000000000000000000 ) ) ;
#174396 = CARTESIAN_POINT ( 'NONE',  ( 10.18233705906309972, 11.83814697611718714, 1.199719254218450271 ) ) ;
#174397 = CARTESIAN_POINT ( 'NONE',  ( 1.172165686010542274, -1.159919637379997814, 1.409874495853599141 ) ) ;
#174398 = CARTESIAN_POINT ( 'NONE',  ( -5.586841817283045408, 8.675676665875643678, 1.199719254218454489 ) ) ;
#174399 = CARTESIAN_POINT ( 'NONE',  ( 4.853455804012215324, 6.685451076146141425, 1.443375672974062551 ) ) ;
#174400 = DIRECTION ( 'NONE',  ( -5.578564026256490882E-16, -1.000000000000000000, -9.066213480720158442E-32 ) ) ;
#174401 = ORIENTED_EDGE ( 'NONE', *, *, #123768, .T. ) ;
#174402 = CARTESIAN_POINT ( 'NONE',  ( 6.139539385720709674, -1.490912338237950108, -1.423074965643542411 ) ) ;
#174403 = CARTESIAN_POINT ( 'NONE',  ( -6.251718229232846369, 9.347402796530044355, -1.082531754730549967 ) ) ;
#174404 = UNCERTAINTY_MEASURE_WITH_UNIT (LENGTH_MEASURE( 1.000000000000000082E-05 ), #188796, 'distance_accuracy_value', 'NONE');
#174405 = CARTESIAN_POINT ( 'NONE',  ( 7.987161891782087686, 8.490979426600148372, -0.7216878364870317197 ) ) ;
#174406 = CARTESIAN_POINT ( 'NONE',  ( -2.740719608256871442, 6.349256642941639051, 0.7998128361456341429 ) ) ;
#174407 = CARTESIAN_POINT ( 'NONE',  ( -4.516801452008150086, 5.298631777878131111, 1.199719254218452935 ) ) ;
#174408 = CARTESIAN_POINT ( 'NONE',  ( 4.354169037430507316, 0.8614980693376246279, -1.826848373156648497 ) ) ;
#174410 = VERTEX_POINT ( 'NONE', #1771 ) ;
#174409 = CARTESIAN_POINT ( 'NONE',  ( 5.268325480127796112, 2.218825861875061811, -0.1076023827350883894 ) ) ;
#174412 = CARTESIAN_POINT ( 'NONE',  ( 8.676855123066012254, 11.14608361504227574, -1.443375672974052559 ) ) ;
#174411 = CARTESIAN_POINT ( 'NONE',  ( -5.178288325776719603, 5.006034233019745372, 0.000000000000000000 ) ) ;
#174413 = CARTESIAN_POINT ( 'NONE',  ( 6.765682348419287173, 7.852049813699357728, 1.199719254218462483 ) ) ;
#174414 = CARTESIAN_POINT ( 'NONE',  ( 4.434483769945627429, 2.020730376925969018, 0.4039503012724340869 ) ) ;
#174415 = CARTESIAN_POINT ( 'NONE',  ( 2.426407915648312930, -1.496052118593782287, -1.352154011671408362 ) ) ;
#174416 = ORIENTED_EDGE ( 'NONE', *, *, #199668, .T. ) ;
#174417 = SURFACE_STYLE_FILL_AREA ( #170113 ) ;
#174418 = CARTESIAN_POINT ( 'NONE',  ( 5.529027716274630855, 5.344953845275508542, 1.040834085586084257E-14 ) ) ;
#174420 = ORIENTED_EDGE ( 'NONE', *, *, #57845, .T. ) ;
#174419 = CARTESIAN_POINT ( 'NONE',  ( -0.09868764650532374505, 7.157731444430473822, -1.998865700660849010 ) ) ;
#174421 = CARTESIAN_POINT ( 'NONE',  ( 5.170590401584001405, 7.751911629329717002, -1.182414590771277085 ) ) ;
#174422 = CARTESIAN_POINT ( 'NONE',  ( 3.128279665134887644, 0.2985813455266342342, -1.993766061640166232 ) ) ;
#174423 = CARTESIAN_POINT ( 'NONE',  ( 2.220424023188283247, -0.0004634451795330202239, 1.841320589463534052 ) ) ;
#174424 = CARTESIAN_POINT ( 'NONE',  ( 0.9620547613307988133, 0.4452262838200848893, -2.264189643979396482 ) ) ;
#174425 = CARTESIAN_POINT ( 'NONE',  ( 3.790386463472274148, 6.579812086429759788, 1.199719254218452047 ) ) ;
#174426 = CARTESIAN_POINT ( 'NONE',  ( 3.989662644735529451, 1.562606173494068829, 1.493797087085822595 ) ) ;
#174427 = CARTESIAN_POINT ( 'NONE',  ( -5.442708600882160574, 8.437244903416123876, -1.199719254218446718 ) ) ;
#174428 = EDGE_LOOP ( 'NONE', ( #173720, #94610, #8745, #74426, #66392, #89559, #78206 ) ) ;
#174429 = DIRECTION ( 'NONE',  ( -0.2684563758389304500, 0.000000000000000000, -0.9632918427306581544 ) ) ;
#174430 = CARTESIAN_POINT ( 'NONE',  ( 1.199835987674138460, -1.870836310881810682, -0.003643258294119822160 ) ) ;
#174431 = EDGE_LOOP ( 'NONE', ( #110981, #133542 ) ) ;
#174432 =( BOUNDED_CURVE ( )  B_SPLINE_CURVE ( 3, ( #184834, #138261, #36464, #204274 ),
 .UNSPECIFIED., .F., .T. ) 
 B_SPLINE_CURVE_WITH_KNOTS ( ( 4, 4 ),
 ( 1.570796326794895892, 2.200856270443528828 ),
 .UNSPECIFIED. ) 
 CURVE ( )  GEOMETRIC_REPRESENTATION_ITEM ( )  RATIONAL_B_SPLINE_CURVE ( ( 1.000000000000000000, 0.9671913951481023730, 0.9671913951481023730, 1.000000000000000000 ) ) 
 REPRESENTATION_ITEM ( '' )  );
#174433 = CARTESIAN_POINT ( 'NONE',  ( 5.823112234018508637, -0.04902082458170010926, 1.971020750367402430 ) ) ;
#174434 = VECTOR ( 'NONE', #113692, 1000.000000000000000 ) ;
#174436 = CARTESIAN_POINT ( 'NONE',  ( 7.415946836550703303, 11.59576237604377091, 0.7216878364870438212 ) ) ;
#174435 = CARTESIAN_POINT ( 'NONE',  ( -1.201851678989727383E-14, 5.196875000341422357, -1.575800808251660134 ) ) ;
#174438 = CARTESIAN_POINT ( 'NONE',  ( 0.7509353727821498348, 0.6442623716619542140, 2.110749664216593047 ) ) ;
#174437 = CARTESIAN_POINT ( 'NONE',  ( -5.925076824372040640, 6.871343368977510302, 1.199719254218450271 ) ) ;
#174439 = CARTESIAN_POINT ( 'NONE',  ( -1.440240048130672079, 7.355731858843376436, -4.317885097515330450 ) ) ;
#174440 = CARTESIAN_POINT ( 'NONE',  ( 5.518332215962025167, 6.396807992499198292, -1.199719254218445830 ) ) ;
#174441 = CARTESIAN_POINT ( 'NONE',  ( -5.656776405399756236, 7.622658444431597680, -1.599625672291256295 ) ) ;
#174442 = CARTESIAN_POINT ( 'NONE',  ( 0.3769810270647828698, 3.049942316455306113, 0.4288785890452298522 ) ) ;
#174443 = CARTESIAN_POINT ( 'NONE',  ( 5.049669536805332370, 0.6190787695102616395, -1.871797661314599015 ) ) ;
#174444 = CARTESIAN_POINT ( 'NONE',  ( 5.373738807407080209, 2.225351779437909183, -0.6107155785605354881 ) ) ;
#174445 = CARTESIAN_POINT ( 'NONE',  ( 5.600015889513015210, 0.7539677941885476464, -1.701683582386106952 ) ) ;
#174446 = CARTESIAN_POINT ( 'NONE',  ( 3.520431386055590917, 0.9232258726861832798, 1.844449542969233358 ) ) ;
#174447 = CARTESIAN_POINT ( 'NONE',  ( 7.158341918335438869, 7.453746447587225710, -0.7216878364870257245 ) ) ;
#174448 = CARTESIAN_POINT ( 'NONE',  ( 8.005163354226054295, 8.304055099544019214, 0.000000000000000000 ) ) ;
#174449 = CARTESIAN_POINT ( 'NONE',  ( 7.578644679914713578, 8.904468883731073703, 1.082531754730558626 ) ) ;
#174450 = CARTESIAN_POINT ( 'NONE',  ( -1.201851678989727383E-14, 2.384375000341416584, 1.575800808251672791 ) ) ;
#174451 = CARTESIAN_POINT ( 'NONE',  ( -4.723354487065243745, 14.48146267970840384, 11.04057532931312835 ) ) ;
#174452 = CARTESIAN_POINT ( 'NONE',  ( 6.616015773344440021, 6.821032611764393572, 1.040834085586084257E-14 ) ) ;
#174453 = CARTESIAN_POINT ( 'NONE',  ( 5.301315566676442437, -1.864821911710778490, 1.111730659606048111 ) ) ;
#174455 = CARTESIAN_POINT ( 'NONE',  ( 4.511176471348508521, -1.804767551675333204, 0.3638508048048467169 ) ) ;
#174454 = DIRECTION ( 'NONE',  ( 3.330669073875478989E-16, -3.540251991789410786E-16, -1.000000000000000000 ) ) ;
#174457 = CARTESIAN_POINT ( 'NONE',  ( 6.620655732516673275, 1.290356161719278028, 1.942653802560645460 ) ) ;
#174456 = CARTESIAN_POINT ( 'NONE',  ( -11.88172094500854037, 11.37999994398404269, 1.685553348215819369 ) ) ;
#174458 = CARTESIAN_POINT ( 'NONE',  ( 6.339412547452306868, 0.8406370108028878851, -2.024118718474729128 ) ) ;
#174459 = CARTESIAN_POINT ( 'NONE',  ( -11.00593736619310725, 11.11000507135410409, -1.443925800506596469 ) ) ;
#174460 = CARTESIAN_POINT ( 'NONE',  ( 0.5095019425028306514, 1.969206903598280212, 1.113800330609107103 ) ) ;
#174461 = CARTESIAN_POINT ( 'NONE',  ( -3.975569122714607495, 7.849474212055944200, 0.02231197147695325456 ) ) ;
#174462 = CARTESIAN_POINT ( 'NONE',  ( 0.000000000000000000, 0.08000000000000020983, 0.000000000000000000 ) ) ;
#174463 = CARTESIAN_POINT ( 'NONE',  ( 6.044612043767858545, 7.151903759757407109, 1.166429756139725660 ) ) ;
#174464 = CARTESIAN_POINT ( 'NONE',  ( -4.299344108864953995, 7.069632989434141201, -1.082531754730551743 ) ) ;
#174465 = CARTESIAN_POINT ( 'NONE',  ( -1.396252044512855672, 3.354846891984019752, -0.1338139928737557549 ) ) ;
#174466 = CARTESIAN_POINT ( 'NONE',  ( 0.2503970875498504056, -1.425519035090598852, 1.048718885610238294 ) ) ;
#174467 = CARTESIAN_POINT ( 'NONE',  ( 5.584640334855505373, -1.275214923639787834, 1.557698558565046243 ) ) ;
#174468 = CARTESIAN_POINT ( 'NONE',  ( 6.681470773436232413, 6.689470745297396270, -0.7998128361456281477 ) ) ;
#174469 = CARTESIAN_POINT ( 'NONE',  ( 4.542079205076994697, 0.9026690382304535243, -1.902845716346044158 ) ) ;
#174470 = CARTESIAN_POINT ( 'NONE',  ( 3.480013654308728555, -1.913576260228011749, -0.09060460826773930609 ) ) ;
#174471 = DIRECTION ( 'NONE',  ( -0.000000000000000000, -1.000000000000000000, -0.000000000000000000 ) ) ;
#174472 = B_SPLINE_CURVE_WITH_KNOTS ( 'NONE', 3,
 ( #127689, #156915, #43174, #206704, #90851, #107145 ),
 .UNSPECIFIED., .F., .F.,
 ( 4, 2, 4 ),
 ( 0.000000000000000000, 0.0003239988925529257036, 0.0006479977851058514073 ),
 .UNSPECIFIED. ) ;
#174473 = CARTESIAN_POINT ( 'NONE',  ( 4.510180775305682843, 1.969176117969779982, -0.04608634298608124680 ) ) ;
#174474 = CARTESIAN_POINT ( 'NONE',  ( 5.379167904621746210, -1.827783419154908273, -0.8597544005511729148 ) ) ;
#174475 = CARTESIAN_POINT ( 'NONE',  ( 3.028041890241763401, 1.040506211802554981, -1.554362669439563360 ) ) ;
#174478 = ORIENTED_EDGE ( 'NONE', *, *, #3774, .F. ) ;
#174477 = CARTESIAN_POINT ( 'NONE',  ( 0.7735182334044669039, 0.3705173918269571431, -1.875978362188877036 ) ) ;
#174476 = CARTESIAN_POINT ( 'NONE',  ( 4.881344157179084320, 1.607756147011094150, -0.6252594192169037557 ) ) ;
#174480 = CARTESIAN_POINT ( 'NONE',  ( 3.226477370372293763, 6.708047998835573900, 0.7216878364870317197 ) ) ;
#174479 = CARTESIAN_POINT ( 'NONE',  ( 2.631697372267821855, -2.058793095894187353, 0.7952504953367269813 ) ) ;
#174481 = CARTESIAN_POINT ( 'NONE',  ( 1.364683531249988757, 1.696875000341414808, 0.000000000000000000 ) ) ;
#174482 = CARTESIAN_POINT ( 'NONE',  ( 0.1392228125525768467, -0.1412503886474673342, -2.030206775815279308 ) ) ;
#174483 = CARTESIAN_POINT ( 'NONE',  ( 7.938462636001388795, 9.220293482545153907, -1.199719254218441611 ) ) ;
#174484 = CARTESIAN_POINT ( 'NONE',  ( -10.32861409551237486, 10.94447128771960287, 1.040834085586084257E-14 ) ) ;
#174485 = DIRECTION ( 'NONE',  ( 1.224646797963766027E-16, -4.396526966619892032E-05, 0.9999999990335275424 ) ) ;
#174486 = CARTESIAN_POINT ( 'NONE',  ( -4.904298879841297421, 6.744767997946720328, 1.599625672291267175 ) ) ;
#174487 = CLOSED_SHELL ( 'NONE', ( #197236, #12593, #124848, #104589, #131806, #140035, #177268, #94801 ) ) ;
#174488 = CARTESIAN_POINT ( 'NONE',  ( 0.000000000000000000, 0.02011834319527033843, -6.938893903907228378E-15 ) ) ;
#174489 = ORIENTED_EDGE ( 'NONE', *, *, #142352, .T. ) ;
#174490 = CARTESIAN_POINT ( 'NONE',  ( 2.137250951388528275, -0.09934309608320915363, -2.068088366144354318 ) ) ;
#174491 = CARTESIAN_POINT ( 'NONE',  ( -1.499999999999997780, 2.650000000000020339, 1.214306433183764966E-14 ) ) ;
#174492 = CARTESIAN_POINT ( 'NONE',  ( 6.661133543015731462, 6.665743976473484267, -0.7998128361456281477 ) ) ;
#174493 = CARTESIAN_POINT ( 'NONE',  ( -5.716734326456539783, 9.821273814174633188, -0.7998128361456231517 ) ) ;
#174494 = CARTESIAN_POINT ( 'NONE',  ( 5.401997860402196316, 5.267028690082820930, 0.000000000000000000 ) ) ;
#174495 = CARTESIAN_POINT ( 'NONE',  ( 6.270199134133584096, 2.114857618286110075, -0.1555134818699496213 ) ) ;
#174496 = DIRECTION ( 'NONE',  ( -0.01745240643728004568, 0.000000000000000000, -0.9998476951563912696 ) ) ;
#174497 = CARTESIAN_POINT ( 'NONE',  ( -1.364683531250012516, 2.738541667008090208, -0.7879004041258289570 ) ) ;
#174499 = CARTESIAN_POINT ( 'NONE',  ( 9.897088948295943212, 11.60932053017587506, 1.082531754730548412 ) ) ;
#174498 = CARTESIAN_POINT ( 'NONE',  ( 0.07479286986302942364, 7.629137130509078268, -2.455503679634089220 ) ) ;
#174500 = EDGE_CURVE ( 'NONE', #83422, #30243, #28289, .T. ) ;
#174501 = CARTESIAN_POINT ( 'NONE',  ( 5.589220178194088895, 1.203167956798111060, -1.617571559180859486 ) ) ;
#174502 = CARTESIAN_POINT ( 'NONE',  ( 5.067565384200278800, 1.291559945344708638, 1.415018661930996569 ) ) ;
#174503 = CARTESIAN_POINT ( 'NONE',  ( 0.000000000000000000, 15.00000000000000000, 0.000000000000000000 ) ) ;
#174504 = CARTESIAN_POINT ( 'NONE',  ( 2.366952063387484095, 0.1042156695447923470, -2.189191704635709890 ) ) ;
#174505 = CARTESIAN_POINT ( 'NONE',  ( 1.907519672996849103, 3.236073672982398008, 0.4612874649729346022 ) ) ;
#174506 = CARTESIAN_POINT ( 'NONE',  ( -1.500000000000013101, 1.660416667349487119, -0.8660254037844313801 ) ) ;
#174507 = CARTESIAN_POINT ( 'NONE',  ( 5.765890645310551399, 0.5801508929094216782, -1.927831218222434195 ) ) ;
#174508 = CARTESIAN_POINT ( 'NONE',  ( 0.7383556378116812313, 1.137082172773289379, -1.537495029474859276 ) ) ;
#174509 = CARTESIAN_POINT ( 'NONE',  ( -4.869349725602420520, 8.832658446511480577, 1.040834085586084257E-14 ) ) ;
#174511 = CARTESIAN_POINT ( 'NONE',  ( 0.3511856949766634095, 0.1948183440376727305, -2.006963311255556714 ) ) ;
#174510 = CARTESIAN_POINT ( 'NONE',  ( -4.134873662487946966, 3.926366815765101936, 1.214306433183764966E-14 ) ) ;
#174512 = CARTESIAN_POINT ( 'NONE',  ( -0.6823417656250003738, 9.463541667008065872, 1.181850606188754593 ) ) ;
#174514 = CARTESIAN_POINT ( 'NONE',  ( -7.306918443122272677, 7.489436036589583345, 0.7998128361456341429 ) ) ;
#174513 = CARTESIAN_POINT ( 'NONE',  ( 3.966417678127855950, -1.951510144350139919, -0.7507201541567410930 ) ) ;
#174516 = ORIENTED_EDGE ( 'NONE', *, *, #10280, .T. ) ;
#174515 = CARTESIAN_POINT ( 'NONE',  ( 2.045521581634631048, 0.6637456736250256784, -1.592148833096140192 ) ) ;
#174517 = CARTESIAN_POINT ( 'NONE',  ( 5.976833544478475702, -1.498421880457675215, 1.500811427713820478 ) ) ;
#174518 = CARTESIAN_POINT ( 'NONE',  ( 6.972971076130050072, 7.029554431773520129, 1.040834085586084257E-14 ) ) ;
#174519 = EDGE_CURVE ( 'NONE', #184190, #140464, #7634, .T. ) ;
#174520 = CARTESIAN_POINT ( 'NONE',  ( 0.2737812321212430566, -1.924752420120953822, 0.3788971555385572954 ) ) ;
#174521 = CARTESIAN_POINT ( 'NONE',  ( -11.81905481421901705, 9.842643443827332916, -1.592167362352180593 ) ) ;
#174522 = CARTESIAN_POINT ( 'NONE',  ( 5.198661835836162481, 8.152523677529138979, 1.199719254218462483 ) ) ;
#174524 =( BOUNDED_SURFACE ( )  B_SPLINE_SURFACE ( 3, 2, ( 
 ( #188818, #22012, #122857 ),
 ( #74003, #205047, #3629 ),
 ( #70766, #186673, #137948 ),
 ( #38300, #154192, #121771 ) ),
 .UNSPECIFIED., .F., .F., .F. ) 
 B_SPLINE_SURFACE_WITH_KNOTS ( ( 4, 4 ),
 ( 3, 3 ),
 ( 0.000000000000000000, 9.170893476616523974E-05 ),
 ( 0.000000000000000000, 1.000000000000000000 ),
 .UNSPECIFIED. ) 
 GEOMETRIC_REPRESENTATION_ITEM ( )  RATIONAL_B_SPLINE_SURFACE ( (
 ( 1.000000000000000000, 0.7100530722026879848, 1.000000000000000000),
 ( 1.000000000000000000, 0.6998898451682321609, 1.000000000000000000),
 ( 1.000000000000000000, 0.6894756946157196698, 1.000000000000000000),
 ( 1.000000000000000000, 0.6787756258917869712, 1.000000000000000000) ) ) 
 REPRESENTATION_ITEM ( '' )  SURFACE ( )  );
#174523 = CARTESIAN_POINT ( 'NONE',  ( -11.91826848676326378, 13.50833707238768078, -1.400000051401918855 ) ) ;
#174525 = CARTESIAN_POINT ( 'NONE',  ( 3.264119686811095988, 1.811656971725349896, -0.002766503545040265976 ) ) ;
#174526 = ORIENTED_EDGE ( 'NONE', *, *, #41738, .T. ) ;
#174527 = CARTESIAN_POINT ( 'NONE',  ( 2.218730694130720771, 5.740269576461138890, 0.7998128361456462443 ) ) ;
#174528 = CARTESIAN_POINT ( 'NONE',  ( 4.386945222473598527, 7.275797305264619652, -1.199719254218452047 ) ) ;
#174529 = CARTESIAN_POINT ( 'NONE',  ( 3.457467740999135231, -1.373635607365558453, -1.181027286383716124 ) ) ;
#174530 = CARTESIAN_POINT ( 'NONE',  ( 0.6386894617478928726, 3.364476098278418092, -0.1366332986426504470 ) ) ;
#174531 = CARTESIAN_POINT ( 'NONE',  ( 5.681948419994366617, 6.106813310819505070, 0.7427411415691799190 ) ) ;
#174532 = ORIENTED_EDGE ( 'NONE', *, *, #90702, .F. ) ;
#174533 = EDGE_CURVE ( 'NONE', #59826, #53788, #28443, .T. ) ;
#174534 = CARTESIAN_POINT ( 'NONE',  ( 4.545250530879026307, 1.662896905596674468, -0.8357390809586220382 ) ) ;
#174535 = EDGE_CURVE ( 'NONE', #175693, #142172, #153056, .T. ) ;
#174536 = CARTESIAN_POINT ( 'NONE',  ( 2.073720586576404568, -0.8169873708120840572, 1.732773573125611088 ) ) ;
#174537 = CARTESIAN_POINT ( 'NONE',  ( 1.078802750678783395, -0.04027803099338270881, -1.825304540826321542 ) ) ;
#174538 = VECTOR ( 'NONE', #163900, 1000.000000000000000 ) ;
#174539 = CARTESIAN_POINT ( 'NONE',  ( 4.833798585616123411, 8.091670711168742258, 0.8834425186924599327 ) ) ;
#174540 = CARTESIAN_POINT ( 'NONE',  ( -3.945059511896602089, 7.546393830613923548, 1.040834085586084257E-14 ) ) ;
#174541 = CARTESIAN_POINT ( 'NONE',  ( 5.028717893731355026, 7.888467461587344687, 1.094519599958807765 ) ) ;
#174542 = CARTESIAN_POINT ( 'NONE',  ( -11.45846087878765296, 10.00688399218595492, 3.566076377698180089 ) ) ;
#174543 = CARTESIAN_POINT ( 'NONE',  ( 1.734723475976807094E-15, 14.99962766111844736, 11.68000013863625774 ) ) ;
#174544 = CARTESIAN_POINT ( 'NONE',  ( -5.886439722289627419, 6.118937485343679761, -0.7679415244158314113 ) ) ;
#174545 = AXIS2_PLACEMENT_3D ( 'NONE', #72191, #121056, #188089 ) ;
#174546 = CARTESIAN_POINT ( 'NONE',  ( 6.317736394288122170, 10.31451686007074997, 0.7216878364870438212 ) ) ;
#174547 = CARTESIAN_POINT ( 'NONE',  ( 5.278159644759479185, -1.050164822159710853, -1.665878549478349013 ) ) ;
#174548 = CARTESIAN_POINT ( 'NONE',  ( -4.416205349749324327, 6.175325546172740765, 1.599625672291267398 ) ) ;
#174549 = CARTESIAN_POINT ( 'NONE',  ( -3.855349344377450027, 7.344262544186459074, -0.7342876487609185654 ) ) ;
#174550 = CARTESIAN_POINT ( 'NONE',  ( 0.04111360010001801485, -1.617408405202691135, -1.324400026677017728 ) ) ;
#174551 = CARTESIAN_POINT ( 'NONE',  ( 5.702155557734973179, -1.926566265495327723, 0.0002483051060025303638 ) ) ;
#174552 = CARTESIAN_POINT ( 'NONE',  ( -4.706651882238427120, 8.642844295920152575, 1.040834085586084257E-14 ) ) ;
#174553 = CARTESIAN_POINT ( 'NONE',  ( 0.9205982885796895054, 1.684962172289593996, 0.7030880920091547859 ) ) ;
#174554 = CARTESIAN_POINT ( 'NONE',  ( 2.543839704335303153, -1.636039663378138886, -1.481301067789652537 ) ) ;
#174555 = CARTESIAN_POINT ( 'NONE',  ( -0.4382560683119304801, -7.666862915010147717, 10.99126615174920119 ) ) ;
#174556 = CARTESIAN_POINT ( 'NONE',  ( 1.072351618572921605, 0.7776387867773439933, 1.747342548420704800 ) ) ;
#174557 = ORIENTED_EDGE ( 'NONE', *, *, #193710, .T. ) ;
#174558 = AXIS2_PLACEMENT_3D ( 'NONE', #33949, #130470, #97911 ) ;
#174559 = CARTESIAN_POINT ( 'NONE',  ( 0.3968417698968416674, 0.3330189415953662690, 1.941018003364772593 ) ) ;
#174560 = CARTESIAN_POINT ( 'NONE',  ( 2.841277192181762334, 0.6965426786647112012, -1.813031058463436818 ) ) ;
#174561 = ORIENTED_EDGE ( 'NONE', *, *, #32706, .F. ) ;
#174562 = CARTESIAN_POINT ( 'NONE',  ( 1.159529582462547781, -0.4871260124716703110, -1.956262300040665814 ) ) ;
#174564 = CARTESIAN_POINT ( 'NONE',  ( 6.772303520102497920, -0.8766781706108403016, -1.641457522745570996 ) ) ;
#174563 = CARTESIAN_POINT ( 'NONE',  ( -6.303615075710993665, 6.318915441276411471, -0.7998128361456362523 ) ) ;
#174565 = CARTESIAN_POINT ( 'NONE',  ( 4.492547798081839794, 6.334668079219206049, 1.599625672291262513 ) ) ;
#174566 = CARTESIAN_POINT ( 'NONE',  ( -11.52888687719588745, 13.79423125105035730, -3.331331986263487366 ) ) ;
#174567 = CARTESIAN_POINT ( 'NONE',  ( 8.550388431712704573, 13.12720360364021133, 0.000000000000000000 ) ) ;
#174568 = CARTESIAN_POINT ( 'NONE',  ( -4.990283058281743678, 7.979691447040783814, -1.199719254218453823 ) ) ;
#174569 = CARTESIAN_POINT ( 'NONE',  ( 2.806388347806953121, 1.585463108415147149, -1.513251884624075672 ) ) ;
#174570 = CARTESIAN_POINT ( 'NONE',  ( 4.039966587192267866, 4.776011108888172707, 1.082531754730560403 ) ) ;
#174571 = CARTESIAN_POINT ( 'NONE',  ( 7.862802741282558294, 8.137967717776607657, 0.000000000000000000 ) ) ;
#174572 = DIRECTION ( 'NONE',  ( 1.000000000000000000, -0.000000000000000000, -0.000000000000000000 ) ) ;
#174573 = CARTESIAN_POINT ( 'NONE',  ( 2.683998146737070378, -0.9385614705539682134, 1.565816405032012470 ) ) ;
#174574 = CARTESIAN_POINT ( 'NONE',  ( 1.734723475976807094E-15, 0.7598076211376182387, -11.09999999999959996 ) ) ;
#174575 = CARTESIAN_POINT ( 'NONE',  ( -4.437596350374534815, 4.071617251725375475, -0.7998128361456221525 ) ) ;
#174576 = CARTESIAN_POINT ( 'NONE',  ( -4.780157383859068077, 8.266535928781179265, -0.8537241328121815132 ) ) ;
#174577 = DIRECTION ( 'NONE',  ( -1.000000000000000000, 0.000000000000000000, 0.000000000000000000 ) ) ;
#174578 = CIRCLE ( 'NONE', #18967, 4.899999999999999467 ) ;
#174579 = CARTESIAN_POINT ( 'NONE',  ( 8.426556166093362776, 9.789735934319136135, -1.199719254218446718 ) ) ;
#174580 = CARTESIAN_POINT ( 'NONE',  ( 1.541497387563552479, -1.395045264726347600, -1.328863961831990181 ) ) ;
#174581 = CARTESIAN_POINT ( 'NONE',  ( 5.594571816639393624, 1.932094781187740917, 0.3390067100078468232 ) ) ;
#174582 = CARTESIAN_POINT ( 'NONE',  ( -1.500000000000001110, 14.77083333333333570, 0.8660254037844419273 ) ) ;
#174583 = CARTESIAN_POINT ( 'NONE',  ( -6.632963465583701534, 8.761543347979550589, -1.599625672291263179 ) ) ;
#174584 = CARTESIAN_POINT ( 'NONE',  ( 5.931855901178834323, 6.879252291918818152, 1.199719254218462483 ) ) ;
#174585 = CARTESIAN_POINT ( 'NONE',  ( 4.634432875810733599, 0.3748786239917039631, 2.159109584303263940 ) ) ;
#174586 = CARTESIAN_POINT ( 'NONE',  ( 0.000000000000000000, 13.49999999999999822, 0.000000000000000000 ) ) ;
#174587 = CARTESIAN_POINT ( 'NONE',  ( 5.489151832033660305, 0.1466973765328460355, 2.065091666743318122 ) ) ;
#174589 = CARTESIAN_POINT ( 'NONE',  ( 1.364683531249988535, 2.176041667008087543, 0.7879004041258500513 ) ) ;
#174588 = CARTESIAN_POINT ( 'NONE',  ( -2.093037498677872144, 1.000000000000000888, 11.70868840297834446 ) ) ;
#174590 = VERTEX_POINT ( 'NONE', #182670 ) ;
#174591 = CARTESIAN_POINT ( 'NONE',  ( 4.694093285409329575, 1.999278280869060342, 1.134256664920972213 ) ) ;
#174592 = CARTESIAN_POINT ( 'NONE',  ( 5.490689023854504747, 9.349628261231513804, 1.040834085586084257E-14 ) ) ;
#174593 = CARTESIAN_POINT ( 'NONE',  ( 4.245111494854632461, 7.966730820723463502, 0.000000000000000000 ) ) ;
#174594 = CARTESIAN_POINT ( 'NONE',  ( 0.4984804791418595560, -0.7777643670432095035, -2.156416217022334436 ) ) ;
#174595 = CARTESIAN_POINT ( 'NONE',  ( -7.518896314322850216, -5.199789852011974745, -8.029456579251602832 ) ) ;
#174596 = CARTESIAN_POINT ( 'NONE',  ( -7.774674742793745708, 8.035151719539642912, 0.7998128361456341429 ) ) ;
#174597 = CARTESIAN_POINT ( 'NONE',  ( 4.787022420419578594, 1.440143517293355879, 1.302930595787118895 ) ) ;
#174598 = ORIENTED_EDGE ( 'NONE', *, *, #72494, .T. ) ;
#174600 = CARTESIAN_POINT ( 'NONE',  ( 9.693716643646601128, 10.41168362711695750, 0.7216878364870438212 ) ) ;
#174599 = STYLED_ITEM ( 'NONE', ( #206772 ), #157787 ) ;
#174601 = EDGE_CURVE ( 'NONE', #103667, #173148, #59668, .T. ) ;
#174602 = EDGE_LOOP ( 'NONE', ( #34762, #159261, #29534, #86030, #8903 ) ) ;
#174603 = CARTESIAN_POINT ( 'NONE',  ( 4.693567934957057375, 1.782326746607498791, -0.6936623114904352239 ) ) ;
#174604 = CARTESIAN_POINT ( 'NONE',  ( 6.475633750228043439, 1.648727237068832396, -0.5065655092456061714 ) ) ;
#174605 = CARTESIAN_POINT ( 'NONE',  ( 5.313685493615880162, -1.282986534165726944, -1.555701818360885280 ) ) ;
#174607 = PLANE ( 'NONE',  #112556 ) ;
#174606 = CARTESIAN_POINT ( 'NONE',  ( -8.371269781434001800, 11.85389961405997816, -1.199719254218446718 ) ) ;
#174608 = CARTESIAN_POINT ( 'NONE',  ( 3.285556943749998737, -1.742708332855374076, -1.896917185911906500 ) ) ;
#174610 = CARTESIAN_POINT ( 'NONE',  ( 0.5492016079408028606, 0.5613503750152969429, -1.678537049539428727 ) ) ;
#174609 = CARTESIAN_POINT ( 'NONE',  ( 1.570382428225084226, -1.985578813138744403, -0.6546124938694962703 ) ) ;
#174611 = CARTESIAN_POINT ( 'NONE',  ( 5.449842333688053486, -1.824117940560719298, -0.8596331684956670660 ) ) ;
#174613 = CARTESIAN_POINT ( 'NONE',  ( 3.152547991667663307, -1.735656589536422212, 1.497406435017712756 ) ) ;
#174612 = CARTESIAN_POINT ( 'NONE',  ( 3.549202351727371862, 7.362762853649070571, -0.7998128361456362523 ) ) ;
#174614 = CARTESIAN_POINT ( 'NONE',  ( 1.868729199028572596, 1.665863247900209121, -0.5035742270650641617 ) ) ;
#174615 = CARTESIAN_POINT ( 'NONE',  ( 2.918346969001627045, -2.117983955170518851, 0.1081942149789016649 ) ) ;
#174616 = CARTESIAN_POINT ( 'NONE',  ( -4.913752204202785023, 4.881785571126718182, -0.5639616748225815268 ) ) ;
#174617 = CARTESIAN_POINT ( 'NONE',  ( 2.161130077686782336, -0.4579326675830681093, -1.672196941802698733 ) ) ;
#174618 = CARTESIAN_POINT ( 'NONE',  ( -6.760415694317216410E-14, 2.234375000341476625, 1.570758158831744078 ) ) ;
#174619 = CARTESIAN_POINT ( 'NONE',  ( 2.066652149400012295, 1.381653119961171239, -1.247030302550973468 ) ) ;
#174620 = CARTESIAN_POINT ( 'NONE',  ( 2.418641202038225302, 0.9268156738743680290, 1.963535311701142483 ) ) ;
#174621 = CARTESIAN_POINT ( 'NONE',  ( 3.186732694495420848, 1.586669336078951664, -1.244385354607212335 ) ) ;
#174622 = CARTESIAN_POINT ( 'NONE',  ( 4.125000000000001776, -2.052068128417945392, 2.349217982248014418E-13 ) ) ;
#174623 = CARTESIAN_POINT ( 'NONE',  ( -0.7500000000000006661, 1.389583334016154748, -1.299038105676652011 ) ) ;
#174624 = CARTESIAN_POINT ( 'NONE',  ( 1.289925581193847925, -0.8688078642279849495, 1.719429354455022096 ) ) ;
#174625 = CARTESIAN_POINT ( 'NONE',  ( -8.012344526598182026E-15, 14.04687500034139624, -1.575800808251669460 ) ) ;
#174626 = CARTESIAN_POINT ( 'NONE',  ( 3.832468605949594043, -1.144296635937601669, -1.903904886208422909 ) ) ;
#174627 = VERTEX_POINT ( 'NONE', #211969 ) ;
#174628 = DIRECTION ( 'NONE',  ( -4.440892098500630106E-16, -3.330669073875473073E-16, -1.000000000000000000 ) ) ;
#174629 = CARTESIAN_POINT ( 'NONE',  ( -1.500000000000013101, 0.4208333333333572068, 0.8660254037844403729 ) ) ;
#174630 = CARTESIAN_POINT ( 'NONE',  ( 7.588813295347141441, 9.876701482703580837, -1.599625672291262513 ) ) ;
#174631 = CARTESIAN_POINT ( 'NONE',  ( -1.402160292154681736E-14, -0.1781249996585796136, 1.575800808251672791 ) ) ;
#174632 = CARTESIAN_POINT ( 'NONE',  ( 5.660436988733716035, 2.218808146451553220, 0.1093606849192785280 ) ) ;
#174633 = CARTESIAN_POINT ( 'NONE',  ( 4.457442142980160504, 1.574409630067734156, 1.170308293268598643 ) ) ;
#174635 = CARTESIAN_POINT ( 'NONE',  ( -6.588899466561478846, 6.789396920517583922, 0.7216878364870317197 ) ) ;
#174634 = CARTESIAN_POINT ( 'NONE',  ( 8.541273586929342798, 11.94827437051752206, -1.082531754730543083 ) ) ;
#174636 = CARTESIAN_POINT ( 'NONE',  ( 6.063815651355930036, 2.230472738441360292, -0.3779872977145922741 ) ) ;
#174637 = CIRCLE ( 'NONE', #81220, 0.08000000000000020983 ) ;
#174638 = CARTESIAN_POINT ( 'NONE',  ( 2.313000242259897199, -1.596077997345384247, 1.306617308116851062 ) ) ;
#174639 = CARTESIAN_POINT ( 'NONE',  ( -4.543954038874438162, 8.453030145328826350, 1.040834085586084257E-14 ) ) ;
#174640 = ORIENTED_EDGE ( 'NONE', *, *, #58112, .T. ) ;
#174641 = CARTESIAN_POINT ( 'NONE',  ( -1.201851678989727383E-14, 2.868750000682821266, -1.732050807568863648 ) ) ;
#174642 = CARTESIAN_POINT ( 'NONE',  ( 1.364683531249988535, 4.717708333674756283, -0.7879004041258300672 ) ) ;
#174643 = CARTESIAN_POINT ( 'NONE',  ( 4.235518730357812345, -1.288231833625707701, -1.356488508162751128 ) ) ;
#174644 = CARTESIAN_POINT ( 'NONE',  ( 2.443678673881148011, -1.509841515647825094, -0.8527992262679043867 ) ) ;
#174645 = EDGE_CURVE ( 'NONE', #85656, #156566, #73422, .T. ) ;
#174646 = CARTESIAN_POINT ( 'NONE',  ( 0.09973926083830295108, -0.6030689337076476919, 2.211586693686658389 ) ) ;
#174647 = CARTESIAN_POINT ( 'NONE',  ( 1.589210545419886378, -0.3244246349418925535, -2.182665228674217861 ) ) ;
#174648 = CARTESIAN_POINT ( 'NONE',  ( 4.089459622424143070, -0.7983975988373869237, 1.932503512935821011 ) ) ;
#174649 = CARTESIAN_POINT ( 'NONE',  ( 5.314377360232536596, 1.795021767651948208, 0.7414505486388212052 ) ) ;
#174650 = CARTESIAN_POINT ( 'NONE',  ( 6.928203230275514990, 15.51887838114830309, 9.797958971132707973 ) ) ;
#174651 = CARTESIAN_POINT ( 'NONE',  ( 0.4062500000042400528, 1.895863743059760909, -0.7852924748300097457 ) ) ;
#174652 = ADVANCED_FACE ( 'NONE', ( #113497 ), #97199, .T. ) ;
#174653 = CARTESIAN_POINT ( 'NONE',  ( 0.4576579978108759050, -1.899619568183811058, -0.6767110947205197125 ) ) ;
#174654 = SURFACE_SIDE_STYLE ('',( #108626 ) ) ;
#174655 = CARTESIAN_POINT ( 'NONE',  ( -1.734723475976807094E-14, 4.000000000000003553, -1.734723475976807094E-14 ) ) ;
#174656 = CARTESIAN_POINT ( 'NONE',  ( -9.664264568442742842, 10.16939683947169115, -0.7998128361456291469 ) ) ;
#174657 = CARTESIAN_POINT ( 'NONE',  ( 7.983053520348166288, 8.207983950027992748, -0.7998128361456281477 ) ) ;
#174659 = ADVANCED_FACE ( 'NONE', ( #32174 ), #154460, .F. ) ;
#174658 = CARTESIAN_POINT ( 'NONE',  ( 4.441915170580639227, 0.7783198120194650960, -1.651611053696280695 ) ) ;
#174660 = CARTESIAN_POINT ( 'NONE',  ( 2.468050989216635127, 2.164326253657654853, -0.4298898877757306725 ) ) ;
#174661 = ORIENTED_EDGE ( 'NONE', *, *, #22794, .T. ) ;
#174662 = CARTESIAN_POINT ( 'NONE',  ( -6.084577077482911101, 10.32070003369722144, 0.000000000000000000 ) ) ;
#174663 = UNCERTAINTY_MEASURE_WITH_UNIT (LENGTH_MEASURE( 1.000000000000000082E-05 ), #124382, 'distance_accuracy_value', 'NONE');
#174664 = CARTESIAN_POINT ( 'NONE',  ( -3.285556943749998737, -1.567708332855375142, 1.896917185911908499 ) ) ;
#174665 = CARTESIAN_POINT ( 'NONE',  ( -8.453672473320708036, 9.821371626084353323, -1.199719254218446718 ) ) ;
#174666 = CARTESIAN_POINT ( 'NONE',  ( 1.177996693904998615, 1.989173073321507612, -0.3494277517126374577 ) ) ;
#174667 = FACE_OUTER_BOUND ( 'NONE', #159459, .T. ) ;
#174668 = ORIENTED_EDGE ( 'NONE', *, *, #173439, .T. ) ;
#174669 = CARTESIAN_POINT ( 'NONE',  ( -4.984557751679625781, 5.844347460828191565, 1.199719254218452935 ) ) ;
#174670 = CARTESIAN_POINT ( 'NONE',  ( 3.467479172597370596, -0.3673618142193516012, 1.824136687861827921 ) ) ;
#174671 = CARTESIAN_POINT ( 'NONE',  ( 4.729096653068339151, 4.411700938201493116, -0.7998128361456211532 ) ) ;
#174672 = CARTESIAN_POINT ( 'NONE',  ( 11.48806469435255551, 9.769102271275494687, 3.468902948106700190 ) ) ;
#174673 = ORIENTED_EDGE ( 'NONE', *, *, #169884, .F. ) ;
#174674 = ORIENTED_EDGE ( 'NONE', *, *, #5122, .T. ) ;
#174675 = CARTESIAN_POINT ( 'NONE',  ( -4.554649539187067830, 7.401175998105142817, 1.199719254218464037 ) ) ;
#174676 = CARTESIAN_POINT ( 'NONE',  ( -7.323375529675950624, 11.69568855126397011, -0.7998128361456291469 ) ) ;
#174677 = CARTESIAN_POINT ( 'NONE',  ( 4.143042835627613663, -1.587387879459275286, 0.9017181768668989239 ) ) ;
#174679 = CARTESIAN_POINT ( 'NONE',  ( -5.356222800695524811, 6.520424213373273936, -1.360004217313095953 ) ) ;
#174678 = CARTESIAN_POINT ( 'NONE',  ( -5.002032328799064231, 4.800402236545811441, -0.7998128361456362523 ) ) ;
#174680 = CARTESIAN_POINT ( 'NONE',  ( 5.544801429207002030, 7.539493339695484408, -1.337888636821100041 ) ) ;
#174681 = CARTESIAN_POINT ( 'NONE',  ( 0.5789038866980666942, 1.201919051685101270, -1.249903294292388667 ) ) ;
#174682 = CARTESIAN_POINT ( 'NONE',  ( 5.718664505737725001, -0.04093049815006092468, 1.840854889930729765 ) ) ;
#174683 = CARTESIAN_POINT ( 'NONE',  ( 3.879734811474966794, 2.173438607767137043, -0.7759833549572618949 ) ) ;
#174684 = CARTESIAN_POINT ( 'NONE',  ( 5.727393547130178675, 5.646656991265468939, 0.000000000000000000 ) ) ;
#174685 = CARTESIAN_POINT ( 'NONE',  ( 0.1927530690809010350, -0.4471281949963988867, -2.018758496260419921 ) ) ;
#174686 = CARTESIAN_POINT ( 'NONE',  ( 5.413504136812340661, 0.6594720349357428013, 2.201770641885878899 ) ) ;
#174687 = DIRECTION ( 'NONE',  ( 1.000000000000000000, 3.451266460341927087E-31, 0.000000000000000000 ) ) ;
#174689 = AXIS2_PLACEMENT_3D ( 'NONE', #3508, #102107, #39243 ) ;
#174688 = CARTESIAN_POINT ( 'NONE',  ( -6.563028877466991595, 9.814561569423593923, 1.199719254218452935 ) ) ;
#174690 = ADVANCED_FACE ( 'NONE', ( #120970 ), #71037, .F. ) ;
#174691 = CARTESIAN_POINT ( 'NONE',  ( 5.963714631206167738, 1.842656449598079060, -0.3214700631931910468 ) ) ;
#174692 = ORIENTED_EDGE ( 'NONE', *, *, #170147, .F. ) ;
#174693 = VECTOR ( 'NONE', #144206, 1000.000000000000114 ) ;
#174695 = CARTESIAN_POINT ( 'NONE',  ( -4.176793841461789114, 7.030620694084159794, -1.199719254218455378 ) ) ;
#174694 = CARTESIAN_POINT ( 'NONE',  ( 2.320441991784210067, -0.7354482596747033973, -1.765520077574176394 ) ) ;
#174696 = CARTESIAN_POINT ( 'NONE',  ( 3.774219598512587037, 1.225428716765289749, 1.835190637982798023 ) ) ;
#174697 = CARTESIAN_POINT ( 'NONE',  ( -4.557020949502716471E-14, 0.2500000006828292376, -1.414508159514595409 ) ) ;
#174698 = CARTESIAN_POINT ( 'NONE',  ( 6.983263157960370116, 7.052597238847845063, 2.544342084569085838 ) ) ;
#174699 = CARTESIAN_POINT ( 'NONE',  ( 5.356880090730872013, 6.382686539675070492, 1.082531754730549078 ) ) ;
#174700 = CARTESIAN_POINT ( 'NONE',  ( -4.773879485343255347, 8.583626809626847987, 0.000000000000000000 ) ) ;
#174701 = CARTESIAN_POINT ( 'NONE',  ( 2.626355190031507192, -1.328241637659173247, -1.886819894403545028 ) ) ;
#174702 = CARTESIAN_POINT ( 'NONE',  ( 2.646866301197240645, -0.3325320220872363675, -1.933311746529025266 ) ) ;
#174703 = CARTESIAN_POINT ( 'NONE',  ( -3.023105066167323329, 5.702484939155337607, -2.420000000000000373 ) ) ;
#174704 = CARTESIAN_POINT ( 'NONE',  ( 6.385603471572667722, -1.944119864917488893, 0.6893456996763939193 ) ) ;
#174705 = CARTESIAN_POINT ( 'NONE',  ( 2.846849069189655967, 5.304779099821139710, -1.082531754730543083 ) ) ;
#174706 = CARTESIAN_POINT ( 'NONE',  ( 3.925017756809038527, -1.752140073516525565, 0.9981236898717813499 ) ) ;
#174707 = CARTESIAN_POINT ( 'NONE',  ( 3.932747076415766596, 6.745899468197171345, 1.199719254218451159 ) ) ;
#174708 = ORIENTED_EDGE ( 'NONE', *, *, #146979, .F. ) ;
#174709 = CARTESIAN_POINT ( 'NONE',  ( 5.014861385384292269, 0.1531656238677771009, 2.010801456750747285 ) ) ;
#174710 =( BOUNDED_CURVE ( )  B_SPLINE_CURVE ( 3, ( #7519, #190542, #124582, #56296, #207860, #106161, #105065 ),
 .UNSPECIFIED., .F., .T. ) 
 B_SPLINE_CURVE_WITH_KNOTS ( ( 4, 3, 4 ),
 ( 0.001053980190856398762, 0.001563073325492780842, 0.001563600248854528623 ),
 .UNSPECIFIED. ) 
 CURVE ( )  GEOMETRIC_REPRESENTATION_ITEM ( )  RATIONAL_B_SPLINE_CURVE ( ( 0.5394211213094468604, 0.6067365765767515073, 0.7602628694736025539, 1.000000000000000000, 0.9997518664343353345, 0.9995038252240703303, 0.9992558763692048762 ) ) 
 REPRESENTATION_ITEM ( '' )  );
#174711 = CARTESIAN_POINT ( 'NONE',  ( -8.188234707649510113, 11.64035869464474082, -1.199719254218446718 ) ) ;
#174712 = CARTESIAN_POINT ( 'NONE',  ( -4.497580221328687067, 8.250285843153577048, -0.1439893610950530312 ) ) ;
#174713 = CARTESIAN_POINT ( 'NONE',  ( -10.78227258717170578, 6.269840026405313793, 4.500979083849748541 ) ) ;
#174714 = CARTESIAN_POINT ( 'NONE',  ( 2.521453382017309952, 5.885520012421409319, 0.000000000000000000 ) ) ;
#174715 = CARTESIAN_POINT ( 'NONE',  ( 1.464000922811282468, -0.5298712919106687291, 2.105275420227727956 ) ) ;
#174716 = CARTESIAN_POINT ( 'NONE',  ( 5.987861119090863049, 7.014868056141362551, 1.199719254218452047 ) ) ;
#174717 =( NAMED_UNIT ( * ) PLANE_ANGLE_UNIT ( ) SI_UNIT ( $, .RADIAN. ) );
#174718 = CARTESIAN_POINT ( 'NONE',  ( 5.464131616080136311, 6.363286244674468684, 1.171972476768274429 ) ) ;
#174719 = CARTESIAN_POINT ( 'NONE',  ( 2.301827437220682171, -1.870247568056710774, 0.04138213060620592881 ) ) ;
#174720 = CARTESIAN_POINT ( 'NONE',  ( 0.1809649437218979473, -0.1514441579043615538, -2.027393396774066936 ) ) ;
#174722 = CARTESIAN_POINT ( 'NONE',  ( 6.727182134110201162, 1.271184308336456015, 2.025152302351560518 ) ) ;
#174721 = CARTESIAN_POINT ( 'NONE',  ( -0.02244404828157658613, 7.629137130509074716, -2.789100637983293662 ) ) ;
#174723 = CARTESIAN_POINT ( 'NONE',  ( 0.6823417656249882723, 0.3427083336747516196, 1.181850606188755259 ) ) ;
#174724 = CARTESIAN_POINT ( 'NONE',  ( -15.75000000000000000, 12.29999999999998295, 1.799999999999999600 ) ) ;
#174725 = ORIENTED_EDGE ( 'NONE', *, *, #123817, .F. ) ;
#174726 = CARTESIAN_POINT ( 'NONE',  ( 2.982959643696237784, -1.767753630637520779, -0.7297678730374329570 ) ) ;
#174727 = B_SPLINE_CURVE_WITH_KNOTS ( 'NONE', 3,
 ( #152362, #3939, #170741, #23404, #103618, #202137, #70007, #56996 ),
 .UNSPECIFIED., .F., .F.,
 ( 4, 2, 2, 4 ),
 ( 0.000000000000000000, 0.001495953190030211788, 0.002991906380060423577, 0.005983812760120847153 ),
 .UNSPECIFIED. ) ;
#174728 = CARTESIAN_POINT ( 'NONE',  ( 4.662845455860040289, -1.581648675543185334, -0.7943582009959786472 ) ) ;
#174729 = CARTESIAN_POINT ( 'NONE',  ( 1.453610327690219473, -1.385809040371610346, -1.317956379189986871 ) ) ;
#174730 = CARTESIAN_POINT ( 'NONE',  ( -3.418627288940168096, 7.140148937072163804, -0.7998128361456281477 ) ) ;
#174732 = CARTESIAN_POINT ( 'NONE',  ( 0.02247297916271525850, 0.3300846716227764932, 1.886903735308493424 ) ) ;
#174731 = DIRECTION ( 'NONE',  ( -1.561251128379126077E-17, -1.301042606982605475E-17, -1.000000000000000000 ) ) ;
#174733 = CARTESIAN_POINT ( 'NONE',  ( 1.499999999999985123, -0.2041666666666457353, -0.8660254037844323793 ) ) ;
#174734 = CARTESIAN_POINT ( 'NONE',  ( 0.8892259839063383353, 0.1505779921940515187, 2.064926437897919964 ) ) ;
#174735 = CARTESIAN_POINT ( 'NONE',  ( 0.7499999999999902300, 5.566666666666685082, -1.299038105676658228 ) ) ;
#174736 = CARTESIAN_POINT ( 'NONE',  ( 5.770339134078734666, -1.185559297855027561, 1.446973003893243348 ) ) ;
#174737 = CARTESIAN_POINT ( 'NONE',  ( 1.558932953716257730, -1.564965500463588732, -0.9399777662534372080 ) ) ;
#174739 = CARTESIAN_POINT ( 'NONE',  ( 4.594558193676899549, 8.374302254291812631, 0.02480325318809234458 ) ) ;
#174738 = CARTESIAN_POINT ( 'NONE',  ( 5.567066847960510323, -1.993696164035433371, -0.9465883713010987410 ) ) ;
#174740 = CARTESIAN_POINT ( 'NONE',  ( -0.6823417656250003738, -0.2822916663252489355, -1.181850606188749264 ) ) ;
#174741 = CARTESIAN_POINT ( 'NONE',  ( 3.051292873657907023, 1.770411945740796966, -1.058192539780268282 ) ) ;
#174742 = CARTESIAN_POINT ( 'NONE',  ( -6.418895661066105873, 9.576129806964074120, -1.199719254218440723 ) ) ;
#174743 = CARTESIAN_POINT ( 'NONE',  ( 8.106885785967500979, 11.54545161934907682, 1.199719254218460707 ) ) ;
#174744 = CARTESIAN_POINT ( 'NONE',  ( 1.443845971921564386, 3.571381292232905125, -0.4218533236949457144 ) ) ;
#174745 = CARTESIAN_POINT ( 'NONE',  ( 0.4390364970160882119, 0.3691015439823106536, 2.129678967336546602 ) ) ;
#174746 = CARTESIAN_POINT ( 'NONE',  ( 7.289443866002793371, 8.533381260871966134, 1.199719254218452047 ) ) ;
#174747 = B_SPLINE_CURVE_WITH_KNOTS ( 'NONE', 3,
 ( #96075, #148009, #192463, #77659 ),
 .UNSPECIFIED., .F., .F.,
 ( 4, 4 ),
 ( 0.000000000000000000, 8.045963024324400998E-05 ),
 .UNSPECIFIED. ) ;
#174748 = CARTESIAN_POINT ( 'NONE',  ( 4.914543119725925280, 0.7892175071393169317, 1.914236960262293508 ) ) ;
#174749 = CARTESIAN_POINT ( 'NONE',  ( -1.364683531250000748, 0.5718750003414208027, 0.000000000000000000 ) ) ;
#174750 = CARTESIAN_POINT ( 'NONE',  ( 3.093221446634909721, 1.855696356685032633, -1.108285163885482039 ) ) ;
#174751 = CARTESIAN_POINT ( 'NONE',  ( -4.820236115778962827, 8.125194398966316456, -0.8510355349711593576 ) ) ;
#174753 = CARTESIAN_POINT ( 'NONE',  ( 1.996468121258226924, 1.940055844723225009, 0.2909814450420752929 ) ) ;
#174752 = CARTESIAN_POINT ( 'NONE',  ( 3.563153132451855054, -1.649810593967064865, 1.164694042050371303 ) ) ;
#174754 = CARTESIAN_POINT ( 'NONE',  ( 6.620655732516684822, 7.052296306484477029, 2.671890196246820004 ) ) ;
#174755 = AXIS2_PLACEMENT_3D ( 'NONE', #71411, #200350, #18410 ) ;
#174758 = CARTESIAN_POINT ( 'NONE',  ( 7.185458225562760148, 8.445751353653788485, -1.082531754730543083 ) ) ;
#174757 = CARTESIAN_POINT ( 'NONE',  ( -3.474999999999998312, -1.370833333333331350, 2.006292185433951047 ) ) ;
#174756 = PRESENTATION_STYLE_ASSIGNMENT (( #160612 ) ) ;
#174759 = ADVANCED_FACE ( 'NONE', ( #203176 ), #87991, .F. ) ;
#174760 = CARTESIAN_POINT ( 'NONE',  ( -6.770317605177755382, 8.992066187497757213, 1.599625672291269396 ) ) ;
#174761 = CARTESIAN_POINT ( 'NONE',  ( 0.9894706735516716201, -0.4852629857438545691, 1.957171443305204761 ) ) ;
#174763 = CARTESIAN_POINT ( 'NONE',  ( 5.812113132715003516, 1.472855484078567923, -1.623034594306454137 ) ) ;
#174762 = CARTESIAN_POINT ( 'NONE',  ( -5.311043488251275591, 7.219303374425030562, -1.599625672291256295 ) ) ;
#174764 = CARTESIAN_POINT ( 'NONE',  ( 0.000000000000000000, 0.9000000000000014655, 0.000000000000000000 ) ) ;
#174765 = CARTESIAN_POINT ( 'NONE',  ( 5.713130151434068438, 1.559639147136464343, -1.106415316399149473 ) ) ;
#174766 = LINE ( 'NONE', #72949, #187923 ) ;
#174768 = CARTESIAN_POINT ( 'NONE',  ( 3.023064714212614135, -1.777003028299545484, 0.9530295004822467719 ) ) ;
#174767 = CARTESIAN_POINT ( 'NONE',  ( -9.449669878600625239, 10.12696240122997082, -0.7216878364870267237 ) ) ;
#174769 = CARTESIAN_POINT ( 'NONE',  ( 0.6823417656249934904, 14.00520833367473195, 1.181850606188764807 ) ) ;
#174770 = CARTESIAN_POINT ( 'NONE',  ( 4.823137214860290456, -0.08221903636504260260, 1.722948775904736385 ) ) ;
#174771 = CARTESIAN_POINT ( 'NONE',  ( 5.189738938980948291, 9.276722205444929870, 0.000000000000000000 ) ) ;
#174772 = CARTESIAN_POINT ( 'NONE',  ( 10.05978679165993483, 11.79913468076720306, 1.082531754730548412 ) ) ;
#174773 = CARTESIAN_POINT ( 'NONE',  ( 4.112460492241882370, 1.324567223757302292, -1.321038939096484066 ) ) ;
#174774 = FACE_OUTER_BOUND ( 'NONE', #142031, .T. ) ;
#174775 = CARTESIAN_POINT ( 'NONE',  ( 0.7431355771655088205, -0.2497938498803170537, -2.055034051290441255 ) ) ;
#174776 = CARTESIAN_POINT ( 'NONE',  ( 6.602015318333181781, 0.7961593463888805289, -1.911361562896146671 ) ) ;
#174777 = VERTEX_POINT ( 'NONE', #161972 ) ;
#174778 = CARTESIAN_POINT ( 'NONE',  ( 5.011674058906918638, 5.875983152593414971, 1.199719254218452047 ) ) ;
#174779 = FACE_OUTER_BOUND ( 'NONE', #54386, .T. ) ;
#174780 = CARTESIAN_POINT ( 'NONE',  ( -0.03528172390533482194, -1.455059732361897895, 1.078909735853793794 ) ) ;
#174781 = CARTESIAN_POINT ( 'NONE',  ( 5.438229012412886476, 7.437962829272074750, -1.443375672974078761 ) ) ;
#174782 = CARTESIAN_POINT ( 'NONE',  ( 9.844850794264569771, 11.91743369232944616, -6.864440167955208949 ) ) ;
#174783 = ORIENTED_EDGE ( 'NONE', *, *, #18312, .T. ) ;
#174784 = ADVANCED_FACE ( 'NONE', ( #11422 ), #29808, .T. ) ;
#174785 = CARTESIAN_POINT ( 'NONE',  ( 9.097157884645296733, 10.67606762258344055, -1.082531754730543083 ) ) ;
#174787 = CARTESIAN_POINT ( 'NONE',  ( 7.130698725783555680, 10.40656671580112658, 1.199719254218460707 ) ) ;
#174786 = CARTESIAN_POINT ( 'NONE',  ( 0.5550359226569913096, 1.633180182981083028, -1.086726831054436682 ) ) ;
#174788 = COLOUR_RGB ( '', 0.31764706, 0.68627451, 0.89019608) ;
#174789 = CARTESIAN_POINT ( 'NONE',  ( 4.991753579581297728, -1.905966813954384387, 0.1920618708746626713 ) ) ;
#174790 = CYLINDRICAL_SURFACE ( 'NONE', #207998, 1.500000000000000222 ) ;
#174791 = CARTESIAN_POINT ( 'NONE',  ( -1.814759087649955749, 3.975067388631681187, 0.4606438099578266665 ) ) ;
#174792 = CARTESIAN_POINT ( 'NONE',  ( 3.469446951953614189E-15, 6.400000000000023448, 1.214306433183764966E-14 ) ) ;
#174794 = ORIENTED_EDGE ( 'NONE', *, *, #199649, .F. ) ;
#174793 = CARTESIAN_POINT ( 'NONE',  ( 5.178851490740205676, 6.104710163027444736, 1.082531754730558626 ) ) ;
#174795 = CARTESIAN_POINT ( 'NONE',  ( -6.399085315970132193, 10.40942393536641397, -0.7216878364870278340 ) ) ;
#174796 = CARTESIAN_POINT ( 'NONE',  ( 2.114359756454447847, -1.018641858927371135, -1.906637348776268004 ) ) ;
#174797 = CARTESIAN_POINT ( 'NONE',  ( -4.065465959251405081, 5.836405933916976707, -1.599625672291271394 ) ) ;
#174798 = CARTESIAN_POINT ( 'NONE',  ( 5.722950238744187956, 9.690876021928001904, 0.7216878364870317197 ) ) ;
#174799 = CARTESIAN_POINT ( 'NONE',  ( -3.277320446201389181, 4.846626492033466072, 1.599625672291267398 ) ) ;
#174800 = CARTESIAN_POINT ( 'NONE',  ( 4.788025880137685597, -0.8597811773201522456, 1.610451283527076116 ) ) ;
#174801 = EDGE_CURVE ( 'NONE', #99756, #11614, #64051, .T. ) ;
#174802 = CARTESIAN_POINT ( 'NONE',  ( 12.32921881676780806, 6.000999082531765616, -1.082566570140983675 ) ) ;
#174803 = CARTESIAN_POINT ( 'NONE',  ( 0.8781228960479293688, -1.098726114091676198, 1.636593336376483743 ) ) ;
#174804 = CARTESIAN_POINT ( 'NONE',  ( 3.779479514802902340, 0.2291398179169491789, -1.898525689255560422 ) ) ;
#174805 = VERTEX_POINT ( 'NONE', #199350 ) ;
#174806 = CARTESIAN_POINT ( 'NONE',  ( 0.3999999999999802047, 3.950000000000008171, 0.8338124244295502807 ) ) ;
#174807 = CARTESIAN_POINT ( 'NONE',  ( 4.703538277703087189, -1.521029056438701232, -1.251204274914043957 ) ) ;
#174808 = ORIENTED_EDGE ( 'NONE', *, *, #99577, .T. ) ;
#174809 = CARTESIAN_POINT ( 'NONE',  ( 5.987830644705256056, -1.933104919717167025, -0.1861817195589876295 ) ) ;
#174810 = ORIENTED_EDGE ( 'NONE', *, *, #64219, .T. ) ;
#174811 = CARTESIAN_POINT ( 'NONE',  ( -5.204350862799341115, 7.165104988056252289, -1.599625672291271394 ) ) ;
#174813 = CARTESIAN_POINT ( 'NONE',  ( 6.099870585610251084, 1.463495690422533579, 1.534846084132005961 ) ) ;
#174812 = CARTESIAN_POINT ( 'NONE',  ( -5.041653019435350380, 6.975290837464928728, -1.599625672291271394 ) ) ;
#174814 = CARTESIAN_POINT ( 'NONE',  ( 6.495764994278795612, 9.632124022417032805, 1.082531754730549078 ) ) ;
#174816 = EDGE_LOOP ( 'NONE', ( #145857, #89927, #16300, #64804, #204864, #11463 ) ) ;
#174815 = CARTESIAN_POINT ( 'NONE',  ( 4.055252259792781366, -1.662250449027093735, 0.9452659147194606426 ) ) ;
#174817 = CARTESIAN_POINT ( 'NONE',  ( -1.790873115444854946, 15.44822087383597875, -11.85388518076883457 ) ) ;
#174818 = CARTESIAN_POINT ( 'NONE',  ( 0.08333923026508995024, -0.1592477204843331384, -2.171661519566956855 ) ) ;
#174819 = CARTESIAN_POINT ( 'NONE',  ( 7.573156686838095730, -5.230039540835552891, 7.978162878861390084 ) ) ;
#174820 = CARTESIAN_POINT ( 'NONE',  ( 4.934244218189309805, -1.078892596291732398, -1.699401429059212765 ) ) ;
#174821 = DIRECTION ( 'NONE',  ( 0.000000000000000000, 1.000000000000000000, 1.496258514059622730E-16 ) ) ;
#174822 = CARTESIAN_POINT ( 'NONE',  ( 6.147073579019600054, -1.539581890156189292, 0.9809480439507823890 ) ) ;
#174823 = CARTESIAN_POINT ( 'NONE',  ( 6.727182134110202050, 0.5964276595885747989, 1.864301751488647962 ) ) ;
#174824 = CARTESIAN_POINT ( 'NONE',  ( 1.522023487246677798, 2.040062638832959241, -0.3519594530456415793 ) ) ;
#174825 = CARTESIAN_POINT ( 'NONE',  ( -6.735703387890906946, 6.752742128827836865, -0.7998128361456291469 ) ) ;
#174826 = CARTESIAN_POINT ( 'NONE',  ( -6.259328228163411723, 6.916251825828671151, -0.7980491773402348388 ) ) ;
#174827 = CARTESIAN_POINT ( 'NONE',  ( 2.672702088255949078E-15, 1.937500000000013323, -1.225000000000018074 ) ) ;
#174828 = CARTESIAN_POINT ( 'NONE',  ( 6.582647274634798151, 7.638508894284114170, 1.199719254218462483 ) ) ;
#174829 = CARTESIAN_POINT ( 'NONE',  ( 4.367134877377630175, 7.148722219365612141, -1.082531754730548412 ) ) ;
#174830 = CARTESIAN_POINT ( 'NONE',  ( 4.241003122976366058, 3.842258486427521103, -0.7998128361456211532 ) ) ;
#174831 = CARTESIAN_POINT ( 'NONE',  ( 0.6823417656249934904, 12.25520833367473017, 1.181850606188764807 ) ) ;
#174833 = CARTESIAN_POINT ( 'NONE',  ( -6.414942957921379474, 7.513130201443591005, -1.199719254218452047 ) ) ;
#174832 = CARTESIAN_POINT ( 'NONE',  ( 6.925078400183531713, 7.629137130509067610, 2.355651831298340326 ) ) ;
#174835 = CARTESIAN_POINT ( 'NONE',  ( 4.605968593894432139, -0.07825817699743177480, 1.732511586087708499 ) ) ;
#174834 = CIRCLE ( 'NONE', #102140, 0.08000000000000050127 ) ;
#174836 = CARTESIAN_POINT ( 'NONE',  ( -5.766295404513795297, 5.621766148221195358, 0.7998128361456341429 ) ) ;
#174837 = CARTESIAN_POINT ( 'NONE',  ( 2.940353189855488658, -1.068159618217549234, 1.773299548953041871 ) ) ;
#174838 = CARTESIAN_POINT ( 'NONE',  ( 3.075892445452293344, -0.8556518723831849638, 1.936791289764336010 ) ) ;
#174839 = AXIS2_PLACEMENT_3D ( 'NONE', #135680, #2430, #68507 ) ;
#174840 = CARTESIAN_POINT ( 'NONE',  ( 6.428537391173986038, 10.65171072301167854, 0.7998128361456462443 ) ) ;
#174841 = CARTESIAN_POINT ( 'NONE',  ( -0.6823417656249969321, 3.467708333674754506, -1.181850606188749264 ) ) ;
#174842 = CARTESIAN_POINT ( 'NONE',  ( 1.621857603371698708, 1.941177911247515375, -0.3314221829187612989 ) ) ;
#174843 = CARTESIAN_POINT ( 'NONE',  ( 5.882017484636844706, 6.163768100491378910, 0.8443116549854499109 ) ) ;
#174844 = CARTESIAN_POINT ( 'NONE',  ( 3.226477370372302644, 5.747678784534228313, 1.082531754730546636 ) ) ;
#174846 = CARTESIAN_POINT ( 'NONE',  ( -10.91944002402978775, -9.900000000000005684, 0.1905873483556694836 ) ) ;
#174845 = CARTESIAN_POINT ( 'NONE',  ( -3.475000000000000533, -2.100000000000000977, 0.000000000000000000 ) ) ;
#174847 = CARTESIAN_POINT ( 'NONE',  ( 3.873197071204284914, 2.158828169701370037, -0.7710026823131793661 ) ) ;
#174848 = CARTESIAN_POINT ( 'NONE',  ( 2.015964598666186269, -0.8597642540715648707, -1.610575774528985704 ) ) ;
#174849 = CARTESIAN_POINT ( 'NONE',  ( 5.722423353419669567, 8.833855124701747386, 1.199719254218451159 ) ) ;
#174850 = CARTESIAN_POINT ( 'NONE',  ( 5.409340101728155936, 8.294351971116089572, -1.082531754730543971 ) ) ;
#174851 = CARTESIAN_POINT ( 'NONE',  ( -6.645467848992654858, 10.90479625713344625, 0.7998128361456481317 ) ) ;
#174852 = ADVANCED_FACE ( 'NONE', ( #15275 ), #17396, .T. ) ;
#174853 = CARTESIAN_POINT ( 'NONE',  ( 2.760023647720879492, 0.7205980239477025595, -1.880007780590841282 ) ) ;
#174854 = CARTESIAN_POINT ( 'NONE',  ( 2.131626046773547500, 1.878804184644796926, -0.5645400877590660560 ) ) ;
#174855 = CARTESIAN_POINT ( 'NONE',  ( -7.458957065812611198, 11.85386701009007204, 0.7998128361456481317 ) ) ;
#174856 = CARTESIAN_POINT ( 'NONE',  ( -7.223796917982883592, 7.322184580601816428, -0.7998128361456291469 ) ) ;
#174857 = CARTESIAN_POINT ( 'NONE',  ( 0.07536363704233400851, 2.864322694550157866, -2.632457840217194089 ) ) ;
#174859 = CARTESIAN_POINT ( 'NONE',  ( 3.010364070732887143, 1.283045204736869671, -1.219329851163194922 ) ) ;
#174858 = CARTESIAN_POINT ( 'NONE',  ( 5.208965158259858619, -0.3072975092734456237, 2.067794563079519143 ) ) ;
#174860 = CARTESIAN_POINT ( 'NONE',  ( 1.050790385995008513, 16.00000000000000000, 12.64745918785790302 ) ) ;
#174861 = CARTESIAN_POINT ( 'NONE',  ( 6.087847202767847854, -2.280615992951875448, -0.2307264670357595804 ) ) ;
#174862 = CARTESIAN_POINT ( 'NONE',  ( 5.929613673486688441, 0.8517357041802063877, -1.517590187452934281 ) ) ;
#174863 = CARTESIAN_POINT ( 'NONE',  ( 6.903072767652295383, 11.20533532890304684, 1.040834085586084257E-14 ) ) ;
#174864 = CARTESIAN_POINT ( 'NONE',  ( 5.801499429514798578, 1.546190052965769057, -1.701143905309614679 ) ) ;
#174865 = CARTESIAN_POINT ( 'NONE',  ( 0.1333692844072559003, 2.872395615372814515, -2.542035612928101873 ) ) ;
#174866 = CARTESIAN_POINT ( 'NONE',  ( 5.272643526055802887, -1.725312034932389382, 0.1713184177872198732 ) ) ;
#174867 = CARTESIAN_POINT ( 'NONE',  ( 5.371592247264787900, -0.3238957681546798528, 2.146784808600268324 ) ) ;
#174868 = CARTESIAN_POINT ( 'NONE',  ( -1.162044386198238738E-15, 2.937500000000009326, -1.225000000000010303 ) ) ;
#174869 = CARTESIAN_POINT ( 'NONE',  ( 0.3216855292715998793, -1.502087118449943137, -1.492529068308690920 ) ) ;
#174870 = CARTESIAN_POINT ( 'NONE',  ( 5.875000000000001776, 2.052068128417940951, -3.214650538869141380E-13 ) ) ;
#174871 = CARTESIAN_POINT ( 'NONE',  ( -0.1639926229446835304, 8.277376109547587291, -1.999401122995872138 ) ) ;
#174872 = CARTESIAN_POINT ( 'NONE',  ( 4.067344539004444037, 0.2368424065766552566, -1.911724265930745847 ) ) ;
#174873 = CARTESIAN_POINT ( 'NONE',  ( -1.500000000000015099, 11.76041666734946922, -0.8660254037844309360 ) ) ;
#174874 = CARTESIAN_POINT ( 'NONE',  ( 6.240512348869785342, 1.279970183950808860, -1.815422973897186543 ) ) ;
#174875 = EDGE_LOOP ( 'NONE', ( #8755, #45655, #114949, #121190 ) ) ;
#174876 = CARTESIAN_POINT ( 'NONE',  ( 0.7499999999999902300, 4.316666666666691299, -1.299038105676658228 ) ) ;
#174877 = CARTESIAN_POINT ( 'NONE',  ( 3.472859903394816872, 7.203420320602605287, -0.7998128361456291469 ) ) ;
#174878 = CARTESIAN_POINT ( 'NONE',  ( 6.632963465583686435, 8.761543347979550589, -1.599625672291262513 ) ) ;
#174879 = CARTESIAN_POINT ( 'NONE',  ( 2.789914007569836318, 2.108506539658880907, -0.6989939510357189301 ) ) ;
#174880 = DIRECTION ( 'NONE',  ( -1.276756478318932585E-15, 1.000000000000000000, -1.665334536937738262E-16 ) ) ;
#174881 = CARTESIAN_POINT ( 'NONE',  ( 7.158341918335438869, 7.453746447587225710, -0.7216878364870257245 ) ) ;
#174882 = CARTESIAN_POINT ( 'NONE',  ( -9.612367721964622191, 10.31677655182129527, -0.7216878364870267237 ) ) ;
#174883 = CARTESIAN_POINT ( 'NONE',  ( 6.129694847154206983, 8.244672969803623630, -1.443375672974078761 ) ) ;
#174884 = AXIS2_PLACEMENT_3D ( 'NONE', #7459, #121313, #185140 ) ;
#174885 = CARTESIAN_POINT ( 'NONE',  ( 0.4400775573648734174, -1.704940109561555950, -1.076314675215600314 ) ) ;
#174887 = CARTESIAN_POINT ( 'NONE',  ( 5.002416047594211435, 2.056911163480923843, 0.1552035700525862538 ) ) ;
#174886 = CARTESIAN_POINT ( 'NONE',  ( 8.914649696185335870, 10.35917838609310593, -1.199719254218446718 ) ) ;
#174888 = SURFACE_STYLE_USAGE ( .BOTH. , #108862 ) ;
#174889 = CARTESIAN_POINT ( 'NONE',  ( -2.764973262183167968, 5.313220341600567664, 1.199719254218462483 ) ) ;
#174890 = CARTESIAN_POINT ( 'NONE',  ( 6.902509602688803980, 9.146290184594002781, -1.443375672974064550 ) ) ;
#174891 = CARTESIAN_POINT ( 'NONE',  ( 0.6823417656249882723, 1.426041667008083547, -1.181850606188749264 ) ) ;
#174892 = CARTESIAN_POINT ( 'NONE',  ( 1.563349520526525538, 1.744638119327382553, -0.2959517217632592900 ) ) ;
#174893 = CARTESIAN_POINT ( 'NONE',  ( 0.1060925565549031974, -0.09613213100253051313, 2.014232862735332308 ) ) ;
#174894 = CARTESIAN_POINT ( 'NONE',  ( 5.741712943377584644, 1.738890731700697412, 0.07666446624409603561 ) ) ;
#174895 = EDGE_CURVE ( 'NONE', #79803, #186977, #45380, .T. ) ;
#174896 = CARTESIAN_POINT ( 'NONE',  ( 3.615000845857639256, -0.1676676331447447266, 2.286275989141072440 ) ) ;
#174897 = CARTESIAN_POINT ( 'NONE',  ( -0.6823417656250003738, -0.2822916663252489355, -1.181850606188749264 ) ) ;
#174898 = CARTESIAN_POINT ( 'NONE',  ( 1.868857239601273923, 1.762127240619456803, -0.5335365013287919345 ) ) ;
#174899 = CARTESIAN_POINT ( 'NONE',  ( 9.154780037725547714, 11.70366268214508487, 1.599625672291279388 ) ) ;
#174900 = CARTESIAN_POINT ( 'NONE',  ( 11.46478114675041127, 7.823431138067391544, 3.656553153322682714 ) ) ;
#174901 = CARTESIAN_POINT ( 'NONE',  ( 2.871877888313049354, 0.9750061419492547232, 1.543211660213184899 ) ) ;
#174902 = CARTESIAN_POINT ( 'NONE',  ( 3.709611425391425854, 1.915599900965975433, 0.6298755557959597740 ) ) ;
#174903 = CARTESIAN_POINT ( 'NONE',  ( -9.022061154889962964, 12.61315621642528129, -1.199719254218446718 ) ) ;
#174904 = DIRECTION ( 'NONE',  ( 0.000000000000000000, 0.000000000000000000, -1.000000000000000000 ) ) ;
#174905 = CARTESIAN_POINT ( 'NONE',  ( 5.139724016738759005, -1.487180916556319454, -1.491360876250556800 ) ) ;
#174906 = CARTESIAN_POINT ( 'NONE',  ( 8.493624849120759990, 15.84268045232546918, 9.435489967669033362 ) ) ;
#174907 = ADVANCED_FACE ( 'NONE', ( #31561 ), #132222, .T. ) ;
#174908 = CARTESIAN_POINT ( 'NONE',  ( 2.559107912120599071, 1.664280205102614429, -1.231313097332722872 ) ) ;
#174909 = CARTESIAN_POINT ( 'NONE',  ( 3.354752944377597856, 6.001296637494123232, -1.199719254218446718 ) ) ;
#174910 = CARTESIAN_POINT ( 'NONE',  ( 1.360316468749971808, 1.026041667008142921, 0.7853790794158540534 ) ) ;
#174911 = CARTESIAN_POINT ( 'NONE',  ( 5.074906250706387567, -1.535530725987072298, 1.462626433913247093 ) ) ;
#174913 = ADVANCED_FACE ( 'NONE', ( #165813 ), #84554, .F. ) ;
#174912 = CARTESIAN_POINT ( 'NONE',  ( 1.102032671262738850, -1.926676517669764443, -0.0008590682252854196007 ) ) ;
#174914 = CARTESIAN_POINT ( 'NONE',  ( -4.817943484809863008, 6.714296380401858499, 1.599625672291263179 ) ) ;
#174915 = CARTESIAN_POINT ( 'NONE',  ( 9.284636267260101050, 9.726497154758602548, -0.7998128361456281477 ) ) ;
#174916 = CARTESIAN_POINT ( 'NONE',  ( 4.814553946184248368, 7.670711132973337065, -1.082531754730548412 ) ) ;
#174917 = CARTESIAN_POINT ( 'NONE',  ( -3.475000000000000533, -1.006249999044084298, 0.000000000000000000 ) ) ;
#174918 = CARTESIAN_POINT ( 'NONE',  ( -5.525111292768871252, 6.404716915440499037, -1.199719254218446718 ) ) ;
#174919 = CARTESIAN_POINT ( 'NONE',  ( 5.783468009189684622, 0.1541500780414573890, -2.115021274163720211 ) ) ;
#174920 = CARTESIAN_POINT ( 'NONE',  ( 2.010898292529788467, 1.560970962663108752, -1.413861550561988922 ) ) ;
#174921 = CARTESIAN_POINT ( 'NONE',  ( -5.330290668828105538, 6.247702530834755130, 1.199719254218452935 ) ) ;
#174922 = CARTESIAN_POINT ( 'NONE',  ( 7.995557903757111617, 10.35123685918189729, 1.599625672291281386 ) ) ;
#174923 = CARTESIAN_POINT ( 'NONE',  ( 6.192234700126073577, 0.9181466042854893317, -1.618627059862162376 ) ) ;
#174924 = CARTESIAN_POINT ( 'NONE',  ( 6.401421083946654100, 10.62007503124645957, -0.7998128361456291469 ) ) ;
#174925 = FACE_OUTER_BOUND ( 'NONE', #68, .T. ) ;
#174926 = CARTESIAN_POINT ( 'NONE',  ( -5.334207092333882017, 5.187939460669764635, 0.7998128361456281477 ) ) ;
#174927 = CARTESIAN_POINT ( 'NONE',  ( -9.503902493499651882, 10.19023378527882784, 1.040834085586084257E-14 ) ) ;
#174928 = CARTESIAN_POINT ( 'NONE',  ( 0.2641366190093488164, 0.6592694798918593557, -2.015615888626711705 ) ) ;
#174929 = CARTESIAN_POINT ( 'NONE',  ( 0.5773502691896192918, -4.295408888568413630, 1.000000000000004441 ) ) ;
#174931 = CARTESIAN_POINT ( 'NONE',  ( 3.455471728117681440, 1.544996161402897528, 1.208956721487665087 ) ) ;
#174930 = CARTESIAN_POINT ( 'NONE',  ( 1.225000000000001199, -0.1041666666666644925, -0.7072540797572898219 ) ) ;
#174932 = CARTESIAN_POINT ( 'NONE',  ( 0.4972265960483426284, 1.796464302094663346, -1.202062886709959422 ) ) ;
#174934 = CARTESIAN_POINT ( 'NONE',  ( -6.104320841615721527, 6.016881168963393200, -0.3405398961462170471 ) ) ;
#174933 = CARTESIAN_POINT ( 'NONE',  ( -5.581116510680924847, 6.540332679663050541, -1.199719254218453823 ) ) ;
#174935 = CARTESIAN_POINT ( 'NONE',  ( 1.364683531249988535, 1.863541667008086211, 0.7879004041258500513 ) ) ;
#174936 = CARTESIAN_POINT ( 'NONE',  ( 2.448798285840974476, 0.4648185774855151942, -1.677030037339591217 ) ) ;
#174937 = CARTESIAN_POINT ( 'NONE',  ( 6.805829924380118356, 7.042482454639357847, 0.7216878364870317197 ) ) ;
#174938 = CARTESIAN_POINT ( 'NONE',  ( -10.91435215633265621, 5.922423255477170301, -6.337208484649258899 ) ) ;
#174939 = CARTESIAN_POINT ( 'NONE',  ( 2.741564358335503382, -1.928455994415989139, -0.5879317209081732498 ) ) ;
#174940 = CARTESIAN_POINT ( 'NONE',  ( 6.825078400183572036, 2.942104585519232263, 2.696255528691358982 ) ) ;
#174941 = CARTESIAN_POINT ( 'NONE',  ( -4.821859908315634158, 5.654533310236863564, 1.199719254218452935 ) ) ;
#174942 = ADVANCED_FACE ( 'NONE', ( #150643 ), #42385, .T. ) ;
#174943 = CARTESIAN_POINT ( 'NONE',  ( 2.430492692261185805, 1.911874441976011640, 0.4805678379448170001 ) ) ;
#174945 = CARTESIAN_POINT ( 'NONE',  ( -6.455090533882206216, 7.663932056684933158, -1.082531754730549967 ) ) ;
#174944 = CARTESIAN_POINT ( 'NONE',  ( 6.222915752822945734, 1.412394824171304908, -1.289504995239741714 ) ) ;
#174946 = CARTESIAN_POINT ( 'NONE',  ( -5.356880090730904875, 7.343055753976412525, 1.443375672974058777 ) ) ;
#174947 = CARTESIAN_POINT ( 'NONE',  ( 6.200875153403774043, 8.327716660428123419, -1.599625672291283607 ) ) ;
#174948 = CARTESIAN_POINT ( 'NONE',  ( -6.805266759416629618, 6.904175738932996964, 0.000000000000000000 ) ) ;
#174949 = CARTESIAN_POINT ( 'NONE',  ( 0.9088601047923352549, -0.4930153254206064428, -1.958433058913966018 ) ) ;
#174950 = CARTESIAN_POINT ( 'NONE',  ( 0.3999999999999889200, 3.949999999999988187, -0.4999999999999987232 ) ) ;
#174951 = CARTESIAN_POINT ( 'NONE',  ( 5.491387719013633983, 2.038315193044057505, -1.081779828593228521 ) ) ;
#174952 = DIRECTION ( 'NONE',  ( 1.000000000000000000, -0.000000000000000000, -0.000000000000000000 ) ) ;
#174953 = CARTESIAN_POINT ( 'NONE',  ( 2.711707638535421960, 0.5279276851305572116, -1.889291386287835550 ) ) ;
#174954 = CARTESIAN_POINT ( 'NONE',  ( 8.748035429315576650, 11.22912730566677553, -1.599625672291255185 ) ) ;
#174955 = CARTESIAN_POINT ( 'NONE',  ( 0.1236729436712938751, 0.3474707636354073537, 1.986100063511665237 ) ) ;
#174956 = EDGE_LOOP ( 'NONE', ( #67779, #42543, #27441, #145528 ) ) ;
#174957 = CARTESIAN_POINT ( 'NONE',  ( 0.7611333729100393519, -0.05844121263920940695, -2.116714853662078344 ) ) ;
#174959 = CARTESIAN_POINT ( 'NONE',  ( -7.555971681517696936, 7.709721804725773175, 0.7998128361456462443 ) ) ;
#174958 = CARTESIAN_POINT ( 'NONE',  ( -2.761056838677368397, 6.372983411765559048, 0.7998128361456341429 ) ) ;
#174960 = CARTESIAN_POINT ( 'NONE',  ( 1.675478281319711549, -0.9859397310463119402, 1.554705294492392254 ) ) ;
#174961 = EDGE_LOOP ( 'NONE', ( #177324, #194620, #194887 ) ) ;
#174962 = CARTESIAN_POINT ( 'NONE',  ( 9.501543970383670157, 13.11825151260853417, 7.330405911628732341 ) ) ;
#174963 = CARTESIAN_POINT ( 'NONE',  ( 3.498385214435925317, -1.041973313016024472, 1.846846941210858351 ) ) ;
#174964 = CARTESIAN_POINT ( 'NONE',  ( -1.500000000000011324, 3.952083334016153415, 0.8660254037844403729 ) ) ;
#174965 = CARTESIAN_POINT ( 'NONE',  ( 8.372323551638698902, 9.726464550788689323, 1.199719254218462483 ) ) ;
#174966 = CARTESIAN_POINT ( 'NONE',  ( 8.025500584646550806, 8.327781868367935658, 0.000000000000000000 ) ) ;
#174967 = CARTESIAN_POINT ( 'NONE',  ( 4.218082229858637788, -1.055972844705153291, -1.769506188133779467 ) ) ;
#174969 = CARTESIAN_POINT ( 'NONE',  ( 0.8371598888798935656, 0.7463826720714299423, -1.683355135116317847 ) ) ;
#174968 = CARTESIAN_POINT ( 'NONE',  ( -6.692921386640485082, 10.96015871772258521, -0.7998128361456291469 ) ) ;
#174970 = CARTESIAN_POINT ( 'NONE',  ( -0.6823417656250212460, 4.801041667008086655, 1.181850606188767472 ) ) ;
#174971 =( LENGTH_UNIT ( ) NAMED_UNIT ( * ) SI_UNIT ( .MILLI., .METRE. ) );
#174972 = CARTESIAN_POINT ( 'NONE',  ( -5.346851039111045978, 6.199209027673974859, 1.173132900504408438 ) ) ;
#174973 = CARTESIAN_POINT ( 'NONE',  ( 2.865460964793633991, 6.435730012307613990, -0.3240538301300336377 ) ) ;
#174974 = CARTESIAN_POINT ( 'NONE',  ( 1.489210700298746692, -0.3264265768355456010, -2.182489157894373033 ) ) ;
#174975 = CARTESIAN_POINT ( 'NONE',  ( 2.460583821258513382, 0.9655243699240693145, 2.046139933455006776 ) ) ;
#174976 = CARTESIAN_POINT ( 'NONE',  ( -9.178506806771670412, 9.810605484096178941, 1.040834085586084257E-14 ) ) ;
#174977 = CARTESIAN_POINT ( 'NONE',  ( 1.915983733309385872, -1.811150802387480274, 0.04719988836864030118 ) ) ;
#174978 = CARTESIAN_POINT ( 'NONE',  ( 2.536237933002471134, 0.6498936893539140058, 1.802224345963408192 ) ) ;
#174979 = CARTESIAN_POINT ( 'NONE',  ( 4.527825515032589898, 2.008996319933327612, -0.4998958796476050681 ) ) ;
#174980 = CARTESIAN_POINT ( 'NONE',  ( -0.6823417656250212460, 3.363541667008085323, 1.181850606188767472 ) ) ;
#174981 = CARTESIAN_POINT ( 'NONE',  ( 3.133621081638960693, -1.322844378366348606, -1.461937730511401190 ) ) ;
#174982 = CARTESIAN_POINT ( 'NONE',  ( 6.358035567807713839, 1.921127907539350810, -0.1446545421508997620 ) ) ;
#174983 = CARTESIAN_POINT ( 'NONE',  ( 4.293723057671197552, -0.7160966649314598476, 1.728361679364013748 ) ) ;
#174985 = CARTESIAN_POINT ( 'NONE',  ( 5.303225773876714122, 7.631601692149430072, -1.229104931163179426 ) ) ;
#174984 = CARTESIAN_POINT ( 'NONE',  ( 1.911159365042811809, 1.708073263224022975, -1.551933148444275989 ) ) ;
#174986 = CARTESIAN_POINT ( 'NONE',  ( 3.490524873212813795, 1.815147244032933038, 0.4099927795770376693 ) ) ;
#174987 = CARTESIAN_POINT ( 'NONE',  ( 0.6823417656249917140, 4.342708333674755394, 1.181850606188765695 ) ) ;
#174988 = CARTESIAN_POINT ( 'NONE',  ( -5.298539104842322267, 5.076050465271134016, 0.7998128361456341429 ) ) ;
#174989 = CARTESIAN_POINT ( 'NONE',  ( 6.043183783389218355, 8.073467052085995022, 1.599625672291267398 ) ) ;
#174990 = CARTESIAN_POINT ( 'NONE',  ( 11.06297021485807264, 9.843306985125275688, 0.9089447062504968367 ) ) ;
#174991 = CARTESIAN_POINT ( 'NONE',  ( 0.5222713366250474332, -1.128438999127111098, -1.778050165696586360 ) ) ;
#174992 = VECTOR ( 'NONE', #26272, 1000.000000000000000 ) ;
#174993 = CARTESIAN_POINT ( 'NONE',  ( 1.364683531249988535, 4.176041667008081326, 0.7879004041258500513 ) ) ;
#174994 = CARTESIAN_POINT ( 'NONE',  ( 5.677088005223024147, -0.04676544374488526834, -2.161250967910962828 ) ) ;
#174995 = CARTESIAN_POINT ( 'NONE',  ( 2.531617689938488791, -0.2033970545941807817, 2.110794199748195599 ) ) ;
#174996 = CARTESIAN_POINT ( 'NONE',  ( 6.182287216677275765, 1.039997956529638889, 1.731187096421077376 ) ) ;
#174997 = CARTESIAN_POINT ( 'NONE',  ( 1.364683531249986537, -0.09479166632524321789, -0.7879004041258309554 ) ) ;
#174998 = CARTESIAN_POINT ( 'NONE',  ( -4.121315508874262790, 6.791656612786516334, -1.082531754730549967 ) ) ;
#174999 = CARTESIAN_POINT ( 'NONE',  ( 1.229993901927586286, -1.370328181169593096, -1.671761099108048265 ) ) ;
#175002 = CARTESIAN_POINT ( 'NONE',  ( 2.738383840280320669, 6.138605547061593448, 0.7216878364870338292 ) ) ;
#175001 = CARTESIAN_POINT ( 'NONE',  ( 1.001543065824772753E-15, -0.3718749995220430038, 3.793834371823811669 ) ) ;
#175000 = CARTESIAN_POINT ( 'NONE',  ( 5.352436782344940802, 9.466536356036257871, 0.000000000000000000 ) ) ;
#175003 = CARTESIAN_POINT ( 'NONE',  ( -4.085803189671902480, 5.860132702740892263, -1.599625672291271394 ) ) ;
#175004 = CARTESIAN_POINT ( 'NONE',  ( 5.208220363674559650, 1.197307938467083055, -1.622483861274232719 ) ) ;
#175006 = CARTESIAN_POINT ( 'NONE',  ( -7.065207446052813367, 8.375735120883982532, -1.082531754730549967 ) ) ;
#175005 = CARTESIAN_POINT ( 'NONE',  ( -7.700668062882059850, 11.92793714009701311, -0.7216878364870267237 ) ) ;
#175007 = CARTESIAN_POINT ( 'NONE',  ( -9.367496997601184816, 15.42330868760440410, -7.413898975931886959 ) ) ;
#175009 = CARTESIAN_POINT ( 'NONE',  ( -0.6823417656250003738, 10.15104166700806587, 1.181850606188754593 ) ) ;
#175008 = CARTESIAN_POINT ( 'NONE',  ( 6.209879897626497502, -2.145988306206991325, 0.2596296833028768347 ) ) ;
#175011 = CARTESIAN_POINT ( 'NONE',  ( -0.08845379458875551881, -1.178863245278682026, -1.510317944339079732 ) ) ;
#175010 = CARTESIAN_POINT ( 'NONE',  ( -4.392478580703220281, 8.068382744221649361, 1.040834085586084257E-14 ) ) ;
#175012 = CARTESIAN_POINT ( 'NONE',  ( -1.364683531250000748, 0.5718750003414208027, 0.000000000000000000 ) ) ;
#175013 = CARTESIAN_POINT ( 'NONE',  ( 6.883263157960364254, 2.431740398616466070, 2.435552827938294751 ) ) ;
#175014 = DIRECTION ( 'NONE',  ( 1.000000000000000000, 0.000000000000000000, 0.000000000000000000 ) ) ;
#175015 = CARTESIAN_POINT ( 'NONE',  ( 3.123388959964632949, -1.662097631915793183, 0.4608284732507839654 ) ) ;
#175016 = CARTESIAN_POINT ( 'NONE',  ( 7.343676480457483002, 8.596652644402405841, -1.199719254218452047 ) ) ;
#175017 = CARTESIAN_POINT ( 'NONE',  ( 6.527324610336440180, 6.579909898339485252, 0.7998128361456331437 ) ) ;
#175018 = CARTESIAN_POINT ( 'NONE',  ( -0.6823417656250246877, -0.6364583329919113464, 1.181850606188755259 ) ) ;
#175019 = CARTESIAN_POINT ( 'NONE',  ( 1.088686764528872919, 1.564356141470560679, -0.8274751086292527757 ) ) ;
#175020 = CARTESIAN_POINT ( 'NONE',  ( 2.033841672972019676, -1.952135521142538854, 0.4911360252713212193 ) ) ;
#175021 = FACE_OUTER_BOUND ( 'NONE', #41161, .T. ) ;
#175023 = COLOUR_RGB ( '', 0.72549020, 0.75294118, 0.79215686) ;
#175022 = CARTESIAN_POINT ( 'NONE',  ( 4.612475435721691497, -0.9401552641563456492, -1.996616816212187340 ) ) ;
#175024 = CARTESIAN_POINT ( 'NONE',  ( 4.997030173247643425, 0.3645372836193886967, 2.140096573681660619 ) ) ;
#175025 = VERTEX_POINT ( 'NONE', #166885 ) ;
#175026 = CARTESIAN_POINT ( 'NONE',  ( 4.947799714344386146, 4.737130853015369958, -0.7998128361456481317 ) ) ;
#175027 = CARTESIAN_POINT ( 'NONE',  ( 7.253248993186713456, 11.40594822545244824, 0.7216878364870438212 ) ) ;
#175029 = CARTESIAN_POINT ( 'NONE',  ( 2.390250109419411295, -0.7743331304885041622, -1.862010821188607945 ) ) ;
#175028 = CARTESIAN_POINT ( 'NONE',  ( 3.739029402251158984, 2.014021593674422572, 0.6637135986873595739 ) ) ;
#175031 = ORIENTED_EDGE ( 'NONE', *, *, #128539, .F. ) ;
#175030 = CARTESIAN_POINT ( 'NONE',  ( 3.761794061002172729, 0.6050747832711267371, -1.707706662339498749 ) ) ;
#175032 = CARTESIAN_POINT ( 'NONE',  ( 6.038177310039780643, 8.137902509836795417, -1.599625672291283607 ) ) ;
#175033 = ORIENTED_EDGE ( 'NONE', *, *, #106403, .T. ) ;
#175034 = EDGE_CURVE ( 'NONE', #108790, #166283, #149503, .T. ) ;
#175035 = CARTESIAN_POINT ( 'NONE',  ( -10.67870335800436798, -6.148216694138041838, 1.725267604293023217E-15 ) ) ;
#175036 = CARTESIAN_POINT ( 'NONE',  ( 5.883392091387671385, 1.685093539698417242, -0.7030590484573000509 ) ) ;
#175038 = CARTESIAN_POINT ( 'NONE',  ( 1.833070758936614864, -1.541008679516321589, -1.137915016233618015 ) ) ;
#175037 = CARTESIAN_POINT ( 'NONE',  ( -3.952365473583647315, 4.569846793057691592, 1.199719254218462483 ) ) ;
#175039 = CARTESIAN_POINT ( 'NONE',  ( 1.217323170181689784, 3.219494316908636300, 0.7750000000000135669 ) ) ;
#175040 = CARTESIAN_POINT ( 'NONE',  ( -1.500000000000015099, 8.760416667349462116, -0.8660254037844309360 ) ) ;
#175041 = CARTESIAN_POINT ( 'NONE',  ( 1.364683531249988757, 1.946875000341415030, 0.000000000000000000 ) ) ;
#175042 = DIRECTION ( 'NONE',  ( 0.000000000000000000, 1.000000000000000000, 0.000000000000000000 ) ) ;
#175043 = AXIS2_PLACEMENT_3D ( 'NONE', #106384, #90098, #156163 ) ;
#175044 = CARTESIAN_POINT ( 'NONE',  ( 6.211043768836170820, 9.299949259400630552, 1.082531754730549967 ) ) ;
#175045 = CARTESIAN_POINT ( 'NONE',  ( -4.163762573172648196, 7.871823745427799501, 0.000000000000000000 ) ) ;
#175046 = CARTESIAN_POINT ( 'NONE',  ( -6.831329296439251131, 9.063246493969506545, -1.599625672291271394 ) ) ;
#175047 = CARTESIAN_POINT ( 'NONE',  ( 2.514065211524143084, -0.6609878990531635745, 2.015050547854141172 ) ) ;
#175049 = CARTESIAN_POINT ( 'NONE',  ( -11.50715376448619764, 7.744667295756731740, 4.958460396591308772 ) ) ;
#175048 = CARTESIAN_POINT ( 'NONE',  ( -4.803422538100232231, 4.881709431271958444, 0.4436329477108340025 ) ) ;
#175050 = CARTESIAN_POINT ( 'NONE',  ( 4.182859841474963147, -0.1902271694152017079, -1.962134583082324024 ) ) ;
#175051 = CARTESIAN_POINT ( 'NONE',  ( 6.222915752822945734, 1.412394824171304908, -1.289504995239741714 ) ) ;
#175052 = ORIENTED_EDGE ( 'NONE', *, *, #159688, .T. ) ;
#175053 = CARTESIAN_POINT ( 'NONE',  ( 6.139883455347572294, 2.111525295599859575, -0.1581134299761654260 ) ) ;
#175054 = CARTESIAN_POINT ( 'NONE',  ( 0.1021010164683408550, 6.360493866598974755, -3.113991822131910059 ) ) ;
#175055 = CARTESIAN_POINT ( 'NONE',  ( 1.820844063133007396, -1.465591517063179028, 1.462601037713284535 ) ) ;
#175056 = CARTESIAN_POINT ( 'NONE',  ( 3.169799299931614911, -1.156099248863748485, 1.560184043245048890 ) ) ;
#175057 = ORIENTED_EDGE ( 'NONE', *, *, #78925, .F. ) ;
#175058 = CARTESIAN_POINT ( 'NONE',  ( 4.179656494762836516, 8.098292687190454586, -0.7998128361456362523 ) ) ;
#175059 = CARTESIAN_POINT ( 'NONE',  ( 5.580062740476173566, 8.667767742934335828, 1.199719254218451159 ) ) ;
#175061 = CARTESIAN_POINT ( 'NONE',  ( 4.632082037363250748, 8.555846143565791095, -0.7998128361456231517 ) ) ;
#175060 = CARTESIAN_POINT ( 'NONE',  ( 3.240259679068544507, 0.5084995621511109176, 2.027717503869540749 ) ) ;
#175062 = CARTESIAN_POINT ( 'NONE',  ( 6.003228155800906407, 10.22579295840155744, 0.000000000000000000 ) ) ;
#175064 = ORIENTED_EDGE ( 'NONE', *, *, #194941, .F. ) ;
#175063 = CARTESIAN_POINT ( 'NONE',  ( 0.5042037957796470238, -1.797571035118279870, -0.2231917716723781087 ) ) ;
#175065 = CARTESIAN_POINT ( 'NONE',  ( 5.356176587289051660, 2.204499490778097481, -0.1052899746726426722 ) ) ;
#175066 = DIRECTION ( 'NONE',  ( 0.000000000000000000, 0.000000000000000000, 1.000000000000000000 ) ) ;
#175067 = CARTESIAN_POINT ( 'NONE',  ( 2.995379075007987613, 1.893430763284314811, -1.133229021217339483 ) ) ;
#175068 = DIRECTION ( 'NONE',  ( 1.000000000000000000, 1.725633230170963762E-31, 8.638326563840814399E-31 ) ) ;
#175069 = CARTESIAN_POINT ( 'NONE',  ( 1.998553653897700011, -1.875654816251038248, -0.3715787057524469472 ) ) ;
#175070 = CARTESIAN_POINT ( 'NONE',  ( 9.610031953988080744, 10.10612545594124967, -0.7998128361456281477 ) ) ;
#175071 = CARTESIAN_POINT ( 'NONE',  ( 5.090316257491098284, 1.067296284200716983, -1.773933887923849984 ) ) ;
#175073 = CARTESIAN_POINT ( 'NONE',  ( 2.413140945657660907, 1.930630709398067246, 0.9725960170764782475 ) ) ;
#175072 = CARTESIAN_POINT ( 'NONE',  ( 9.590330253158084517, -9.597646708343965827, -0.1673998372498815279 ) ) ;
#175074 = CARTESIAN_POINT ( 'NONE',  ( 5.108995794240286159, -0.3219066699026683631, 2.167653318578148358 ) ) ;
#175075 = ORIENTED_EDGE ( 'NONE', *, *, #93285, .T. ) ;
#175076 = ORIENTED_EDGE ( 'NONE', *, *, #49744, .T. ) ;
#175077 = CARTESIAN_POINT ( 'NONE',  ( -0.1294898018152357277, -0.0008549345193623123906, -1.926395771554182179 ) ) ;
#175078 = CARTESIAN_POINT ( 'NONE',  ( -3.701012746406287413, 6.301303389907177532, 1.082531754730560403 ) ) ;
#175079 = CARTESIAN_POINT ( 'NONE',  ( -4.702146809683723561, 5.356480858934594025, -2.500000000000000444 ) ) ;
#175080 = CARTESIAN_POINT ( 'NONE',  ( 4.441177836928239309, 7.339068688795062911, 1.199719254218452047 ) ) ;
#175081 = CARTESIAN_POINT ( 'NONE',  ( -3.285556943749998737, -2.617708332855374742, 1.896917185911908721 ) ) ;
#175082 = DIRECTION ( 'NONE',  ( 0.000000000000000000, 0.000000000000000000, -1.000000000000000000 ) ) ;
#175083 = CARTESIAN_POINT ( 'NONE',  ( -9.517460647113315630, 10.20605163116143821, 0.7216878364870438212 ) ) ;
#175084 = CARTESIAN_POINT ( 'NONE',  ( 6.398522151006641678, 6.429640362454684954, 0.000000000000000000 ) ) ;
#175085 = CARTESIAN_POINT ( 'NONE',  ( 6.244996659533327943, -0.2978818936431072983, -2.048576297084458098 ) ) ;
#175086 = CARTESIAN_POINT ( 'NONE',  ( 4.002502541323429419, -0.6052661472178870739, -1.829015351804675005 ) ) ;
#175087 = CARTESIAN_POINT ( 'NONE',  ( 6.521125090989952078, -1.891168486443073116, 0.9521521135891182208 ) ) ;
#175088 = DIRECTION ( 'NONE',  ( 1.000000000000000000, -0.000000000000000000, -0.000000000000000000 ) ) ;
#175089 = CARTESIAN_POINT ( 'NONE',  ( 6.145923705696426431, 6.064665832934283962, 0.7998128361456341429 ) ) ;
#175090 = CARTESIAN_POINT ( 'NONE',  ( -1.499999999999997780, 3.431250000682818602, 1.214306433183764966E-14 ) ) ;
#175091 = CARTESIAN_POINT ( 'NONE',  ( 5.541845313694261144, 1.319919544752303331, 1.461889559981154108 ) ) ;
#175092 = CARTESIAN_POINT ( 'NONE',  ( 0.3049557181189038180, 1.908793570626087455, 1.076422248949958638 ) ) ;
#175093 = CARTESIAN_POINT ( 'NONE',  ( 5.690036971771410101, -0.8169618954828453683, 1.632782195682795257 ) ) ;
#175094 = PRODUCT_DEFINITION_SHAPE ( 'NONE', 'NONE',  #214426 ) ;
#175095 = CARTESIAN_POINT ( 'NONE',  ( 5.858531774880875176, 9.849054480754103835, -0.7216878364870458196 ) ) ;
#175096 = CARTESIAN_POINT ( 'NONE',  ( 3.185802909086945967, 5.700225246367978116, 1.082531754730546636 ) ) ;
#175097 = CARTESIAN_POINT ( 'NONE',  ( -6.252245114557387851, 7.323316050852266557, -1.199719254218453823 ) ) ;
#175098 = CARTESIAN_POINT ( 'NONE',  ( 4.716257332707354699, 6.595662536282280719, -1.599625672291269396 ) ) ;
#175099 = ORIENTED_EDGE ( 'NONE', *, *, #102005, .F. ) ;
#175101 = CARTESIAN_POINT ( 'NONE',  ( 5.871345457035325843, -1.728819661934883678, -1.031334786431532313 ) ) ;
#175100 = CARTESIAN_POINT ( 'NONE',  ( 2.155570461979210428, 0.7887370375637430264, 1.663910549085621415 ) ) ;
#175102 = CARTESIAN_POINT ( 'NONE',  ( 0.4744793627779358980, 2.001106834215804042, 1.130494720166761891 ) ) ;
#175103 = CARTESIAN_POINT ( 'NONE',  ( 6.016451032921247055, 0.7918200671565789328, 1.795022358689958963 ) ) ;
#175104 = CARTESIAN_POINT ( 'NONE',  ( -6.389970470742427189, 6.349387058821269747, -0.7998128361456291469 ) ) ;
#175105 = CARTESIAN_POINT ( 'NONE',  ( 9.183873789516525221, -7.868711957286002701, 9.269928574751062911E-15 ) ) ;
#175106 = VECTOR ( 'NONE', #189924, 1000.000000000000000 ) ;
#175107 = CARTESIAN_POINT ( 'NONE',  ( -2.611917148927046295, 6.198987107056845858, 1.040834085586084257E-14 ) ) ;
#175108 = CARTESIAN_POINT ( 'NONE',  ( 0.8892259839063383353, 0.1505779921940515187, 2.064926437897919964 ) ) ;
#175109 = CARTESIAN_POINT ( 'NONE',  ( -4.664887371553763096, 7.600063145858131364, -1.199719254218453823 ) ) ;
#175111 = CARTESIAN_POINT ( 'NONE',  ( 0.3911966820569385828, 1.383097094795827209, 1.259704262696823118 ) ) ;
#175110 = CARTESIAN_POINT ( 'NONE',  ( 1.874669627338154454, -0.1056657526060876956, -2.088216114563210102 ) ) ;
#175112 = CARTESIAN_POINT ( 'NONE',  ( 1.405624810022429561, 0.3905361843517705100, 1.977748161624798939 ) ) ;
#175113 = CARTESIAN_POINT ( 'NONE',  ( -0.2104748580754166321, -0.006608320950486632102, -2.103482951484026309 ) ) ;
#175114 = CARTESIAN_POINT ( 'NONE',  ( 2.278492620635372390, 1.590801041788017178, -0.7064735415249421280 ) ) ;
#175115 = CARTESIAN_POINT ( 'NONE',  ( 4.635998460869027227, 7.496083073400806818, -1.199719254218452047 ) ) ;
#175117 = DIRECTION ( 'NONE',  ( -0.000000000000000000, -1.000000000000000000, 0.000000000000000000 ) ) ;
#175116 = DIRECTION ( 'NONE',  ( -1.276756478318932585E-15, 1.000000000000000000, -1.665334536937738262E-16 ) ) ;
#175118 = CARTESIAN_POINT ( 'NONE',  ( 3.017853972043908151, -0.8504761986376055960, -1.500546066986796490 ) ) ;
#175119 =( BOUNDED_SURFACE ( )  B_SPLINE_SURFACE ( 3, 2, ( 
 ( #52406, #168289, #100088 ),
 ( #184516, #38287, #199698 ),
 ( #118533, #134748, #200757 ),
 ( #54537, #132623, #53466 ),
 ( #101138, #51343, #18812 ),
 ( #150986, #166149, #68625 ) ),
 .UNSPECIFIED., .F., .F., .F. ) 
 B_SPLINE_SURFACE_WITH_KNOTS ( ( 4, 2, 4 ),
 ( 3, 3 ),
 ( 0.000000000000000000, 0.0003754689591423961527, 0.0007509379182847923054 ),
 ( 0.000000000000000000, 1.000000000000000000 ),
 .UNSPECIFIED. ) 
 GEOMETRIC_REPRESENTATION_ITEM ( )  RATIONAL_B_SPLINE_SURFACE ( (
 ( 1.000000000000000000, 0.7071067811865475727, 1.000000000000000000),
 ( 1.000000000000000000, 0.7018599272024023117, 1.000000000000000000),
 ( 1.000000000000000000, 0.6927733177260293473, 1.000000000000000000),
 ( 1.000000000000000000, 0.6772007068873806546, 1.000000000000000000),
 ( 1.000000000000000000, 0.6709974581636959368, 1.000000000000000000),
 ( 1.000000000000000000, 0.6711954675835484219, 1.000000000000000000) ) ) 
 REPRESENTATION_ITEM ( '' )  SURFACE ( )  );
#175120 = CARTESIAN_POINT ( 'NONE',  ( 2.507599501126521524, -2.167277876680247850, 0.3246147914140809498 ) ) ;
#175121 = CARTESIAN_POINT ( 'NONE',  ( 5.637410271038987730, -1.996576301129053377, 0.9405272304151901519 ) ) ;
#175122 = CARTESIAN_POINT ( 'NONE',  ( -10.24056286296518614, 5.004077596833054642, -7.476959758773280562 ) ) ;
#175123 = CARTESIAN_POINT ( 'NONE',  ( 2.799877792657178066, -1.606015216909290277, -1.461049007858437054 ) ) ;
#175124 = CARTESIAN_POINT ( 'NONE',  ( 0.7502976729042536430, 0.5272139720400963459, 1.747899773703022408 ) ) ;
#175125 = CARTESIAN_POINT ( 'NONE',  ( 3.591103737854687061, 1.818103999434977025, 1.084929287856269742 ) ) ;
#175126 = DIRECTION ( 'NONE',  ( 0.000000000000000000, 0.000000000000000000, 1.000000000000000000 ) ) ;
#175127 = ORIENTED_EDGE ( 'NONE', *, *, #4291, .T. ) ;
#175129 = CARTESIAN_POINT ( 'NONE',  ( -1.364683531250012516, 1.842708333674749843, 0.7879004041258379498 ) ) ;
#175128 = CARTESIAN_POINT ( 'NONE',  ( 3.316269524717931017, 1.452881069417772730, -1.773186822121583184 ) ) ;
#175130 = CARTESIAN_POINT ( 'NONE',  ( 1.224999999999967004, 0.1041666666667366015, 0.7072540797572677285 ) ) ;
#175131 = CARTESIAN_POINT ( 'NONE',  ( 3.354752944377597856, 6.001296637494123232, -1.199719254218446718 ) ) ;
#175132 = CARTESIAN_POINT ( 'NONE',  ( 6.340512354315207766, 1.281540423541355223, -1.814176132805396691 ) ) ;
#175133 = CARTESIAN_POINT ( 'NONE',  ( -6.236387472606158333, 7.338502141871059870, -1.082531754730544860 ) ) ;
#175134 = AXIS2_PLACEMENT_3D ( 'NONE', #148621, #189, #211463 ) ;
#175135 = CARTESIAN_POINT ( 'NONE',  ( 3.551873057100283226, 6.127307085716883428, 1.082531754730558626 ) ) ;
#175136 = CARTESIAN_POINT ( 'NONE',  ( -7.063434842595444962, 8.303390740191881392, 1.082531754730549967 ) ) ;
#175137 = FACE_OUTER_BOUND ( 'NONE', #24839, .T. ) ;
#175139 = VERTEX_POINT ( 'NONE', #117117 ) ;
#175138 = AXIS2_PLACEMENT_3D ( 'NONE', #41651, #25367, #140226 ) ;
#175140 = CARTESIAN_POINT ( 'NONE',  ( 4.412732527109735514, -1.242725882911545510, -1.587838301257207041 ) ) ;
#175142 = CARTESIAN_POINT ( 'NONE',  ( 3.485269120655315689, 0.04592427588026624929, 2.062205569330832766 ) ) ;
#175141 = CARTESIAN_POINT ( 'NONE',  ( 5.937581207780954884, 9.014596278131406848, -1.199719254218440723 ) ) ;
#175143 = CARTESIAN_POINT ( 'NONE',  ( -3.070003471035267939, 6.451017196056028524, -0.6895117023006979151 ) ) ;
#175144 = CARTESIAN_POINT ( 'NONE',  ( 5.058600711230250013, 5.074324715956299414, -0.7216878364870458196 ) ) ;
#175145 = CARTESIAN_POINT ( 'NONE',  ( 1.001543065824772753E-15, -3.521874999522041083, 3.793834371823811669 ) ) ;
#175146 = CARTESIAN_POINT ( 'NONE',  ( 0.6823417656249899377, 5.426041667008087543, -1.181850606188754593 ) ) ;
#175147 = CARTESIAN_POINT ( 'NONE',  ( 6.228506716250251429, 0.2110190803071687604, 2.181275323772186692 ) ) ;
#175148 = CARTESIAN_POINT ( 'NONE',  ( 4.043592392309851569, -1.492256208629010761, 1.356298961253152413 ) ) ;
#175149 = CARTESIAN_POINT ( 'NONE',  ( 2.296224312773272658, 1.477747569344042278, -1.098160524033331642 ) ) ;
#175150 = CARTESIAN_POINT ( 'NONE',  ( 7.305145839664861640, 7.417091655897478653, 0.7998128361456341429 ) ) ;
#175151 = CARTESIAN_POINT ( 'NONE',  ( 5.877927443470423619, 1.089437568142386015, 1.464738158297604453 ) ) ;
#175152 = CARTESIAN_POINT ( 'NONE',  ( 0.3000039258060793745, 1.578900123410318823, -1.670874907869798864 ) ) ;
#175153 = CARTESIAN_POINT ( 'NONE',  ( -7.039708073993679704, 9.236078724457858158, 1.599625672291283607 ) ) ;
#175155 = CARTESIAN_POINT ( 'NONE',  ( -5.061990249855848667, 6.999017606288844284, -1.599625672291271394 ) ) ;
#175154 = CARTESIAN_POINT ( 'NONE',  ( 6.209908689894510836, -2.246332978858367468, 0.2696892186580777673 ) ) ;
#175156 = CARTESIAN_POINT ( 'NONE',  ( 1.682391906368089662, -1.125439293035620292, 1.779948400507038953 ) ) ;
#175157 = CARTESIAN_POINT ( 'NONE',  ( -5.261446130555064826, 8.296048364692991228, 1.199719254218452935 ) ) ;
#175158 = CARTESIAN_POINT ( 'NONE',  ( 7.239163954692881653, 10.53310948286200599, -1.199719254218441611 ) ) ;
#175159 = CARTESIAN_POINT ( 'NONE',  ( 6.333067150914805765, 9.442309871825708356, 1.082531754730549967 ) ) ;
#175161 = EDGE_CURVE ( 'NONE', #190182, #164527, #184117, .T. ) ;
#175160 = CARTESIAN_POINT ( 'NONE',  ( -6.353967546298838087, 10.56471257065732416, 0.000000000000000000 ) ) ;
#175162 = DIRECTION ( 'NONE',  ( -5.551115123125765446E-17, 0.000000000000000000, 1.000000000000000000 ) ) ;
#175163 = CARTESIAN_POINT ( 'NONE',  ( 5.924549939047454750, 9.855799328956630134, -0.7216878364870267237 ) ) ;
#175164 = CARTESIAN_POINT ( 'NONE',  ( 4.075930520424391190, 7.726065465775651120, -0.5982635945973235891 ) ) ;
#175165 = CARTESIAN_POINT ( 'NONE',  ( -4.089755892816631544, 7.923132308261379819, -0.7998128361456281477 ) ) ;
#175166 = CARTESIAN_POINT ( 'NONE',  ( 3.252379014334851437, 0.9957207747773239026, -1.985791214296761087 ) ) ;
#175167 = CARTESIAN_POINT ( 'NONE',  ( 0.2236267563471248943, -0.1037379595543522215, 2.204571545119632603 ) ) ;
#175168 = CARTESIAN_POINT ( 'NONE',  ( -6.069210040772897052, 7.109775131437022999, -1.199719254218453823 ) ) ;
#175169 = CARTESIAN_POINT ( 'NONE',  ( 6.471319392424407901, 6.444294134116939077, 0.7998128361456341429 ) ) ;
#175170 = CARTESIAN_POINT ( 'NONE',  ( 4.193769882565239193, -1.351282707657221582, -1.422545440481419510 ) ) ;
#175171 = CARTESIAN_POINT ( 'NONE',  ( 8.646349277213076334, 11.11049346154719508, 1.599625672291281386 ) ) ;
#175172 = CARTESIAN_POINT ( 'NONE',  ( -4.638859928512265363, 6.918491158249495676, 1.209939204767721987 ) ) ;
#175173 = CARTESIAN_POINT ( 'NONE',  ( -1.402160292154681736E-14, 1.196875000341419026, -1.575800808251659024 ) ) ;
#175174 = CARTESIAN_POINT ( 'NONE',  ( -5.153507786970275006, 7.105788066255672497, -1.443375672974066548 ) ) ;
#175177 = ORIENTED_EDGE ( 'NONE', *, *, #179502, .F. ) ;
#175176 = CARTESIAN_POINT ( 'NONE',  ( -5.070386261830872598, 8.859275038870594088, 0.7216878364870458196 ) ) ;
#175175 = COLOUR_RGB ( '', 0.08235294, 0.09019608, 0.10196078) ;
#175178 =( BOUNDED_SURFACE ( )  B_SPLINE_SURFACE ( 1, 2, ( 
 ( #80320, #66161, #132307, #47855, #49954, #99772, #17423, #83506, #149588, #97661, #51023, #29451, #79259, #211374, #195148, #63000, #64077, #30521, #46782, #112896, #178907, #113966, #170089, #72584, #169028, #204702, #37970, #166910, #138685, #117144, #203636, #200442, #54221, #183148, #120360, #86714, #100825, #84583, #88869, #150670, #2231, #167967, #87785, #36888, #68308, #104044, #19573, #202570, #153859, #185264, #134439, #151733, #53149, #71508, #69373, #137618, #55287, #121437, #187406, #52088, #135481, #118215, #39037, #105122, #171162, #201503, #22751, #13582, #115420, #149995, #146821, #494, #50355, #161992, #147871, #29856, #30928, #82845, #15702, #1566, #165166, #97004, #67628, #179307, #81788, #132704, #116477, #16761, #95936, #79655, #198710, #163057, #182467, #14637, #66562, #114365, #34096, #196611, #113300, #148921, #180359, #213887, #181412, #178240, #129562, #31985, #100167, #98063, #80731, #48250, #65509, #131655, #164119, #197658, #49304, #166232, #212841, #64478, #17822, #83905, #130619, #133773, #33039, #47187, #211773, #99117, #195549, #199781, #51427, #145772, #63411, #186742, #171560, #102295, #135877, #118611, #117547, #101224, #185667, #184599, #36216, #167307, #139085, #201897, #134827, #136950, #168369, #105526, #55678, #37296, #35148, #88188, #19964, #84978, #169431, #86048, #119680, #5835, #152124, #68705, #121834, #3694, #69771, #18894, #151070, #53549, #23158, #187805, #183541, #104443, #103369, #21015, #52482, #200831, #2632, #87113, #153183, #154261, #39433, #89272, #38364, #202975, #205112, #4757, #70833, #54616, #120764, #170492, #22076, #71906, #138015, #204030, #155321, #6905, #72982, #206188, #157471, #208318, #42664, #12255, #176909, #108773, #109842, #59948, #192064, #126104, #94615, #123978, #27445, #93543, #25309, #174798, #189946, #159587, #26374, #9066, #92487, #11186, #43727, #77265, #143379, #190998, #160659, #78332, #158526, #10123, #7983, #76198, #107706, #41595, #209377, #125043, #61021, #142308, #175856, #144454, #127180, #56755, #193148, #106622, #122920 ),
 ( #44798, #173732, #74072, #110903, #91411, #75141, #40519, #172651, #141250, #28524, #188878, #24226, #90328, #207259, #58888, #57816, #140165, #156397, #79404, #130372, #32791, #248, #66320, #131410, #15449, #83657, #210457, #114120, #95685, #31736, #14381, #81537, #180112, #177986, #129321, #17573, #65264, #147619, #45862, #213638, #182222, #179052, #98866, #82594, #194217, #97809, #62095, #63156, #115171, #48002, #33845, #197410, #195298, #99926, #211520, #163872, #164918, #148680, #49051, #128254, #111983, #16511, #46928, #132464, #113046, #198466, #146572, #50111, #80473, #145521, #181166, #212591, #116231, #165988, #29599, #161739, #64229, #13330, #196362, #30671, #96754, #162804, #202726, #154012, #200591, #5578, #2385, #18654, #183295, #52239, #167062, #84734, #53304, #187560, #134591, #4514, #203790, #118367, #168123, #150822, #149747, #133525, #3457, #68463, #184355, #199532, #171313, #19724, #35977, #169183, #102058, #137772, #87938, #69527, #67385, #120516, #85803, #117298, #201655, #151883, #135634, #38125, #119436, #100973, #71658, #185423, #37041, #51175, #34901, #103125, #55436, #121588, #1324, #136702, #20775, #86871, #152937, #70587, #54378, #186494, #104198, #170245, #39187, #105276, #21830, #22908, #179579, #89024, #209916, #191539, #127719, #110378, #111442, #61554, #59421, #10656, #113577, #161194, #177446, #141789, #29061, #63685, #60480, #128770, #178512, #75679, #193679, #155077, #159060, #210981, #143919, #129841, #78855, #76729, #195822, #93017, #45322, #46384, #30124, #144976, #9602, #207793, #112502, #142845, #96213, #208850, #194746, #27989, #162264, #176383, #26910, #62608, #94085, #95144, #12782, #125577, #43204, #160123, #13851, #11724, #126639, #77800, #79927, #192604, #44257, #47462, #146034, #109317, #212043, #175327, #149201, #18111, #34375, #116758, #48519, #117839, #180633, #131928, #182757, #17042, #201127, #151351, #83121, #84197, #100448, #166521, #150287, #68993, #98325, #1854, #67914, #214152, #776, #164390, #134060, #66842, #197938, #132986, #200068, #51719, #183831 ) ),
 .UNSPECIFIED., .F., .F., .T. ) 
 B_SPLINE_SURFACE_WITH_KNOTS ( ( 2, 2 ),
 ( 3, 2, 2, 2, 2, 2, 2, 2, 2, 2, 2, 2, 2, 2, 2, 2, 2, 2, 2, 2, 2, 2, 2, 2, 2, 2, 2, 2, 2, 2, 2, 2, 2, 2, 2, 2, 2, 2, 2, 2, 2, 2, 2, 2, 2, 2, 2, 2, 2, 2, 2, 2, 2, 2, 2, 2, 2, 2, 2, 2, 2, 2, 2, 2, 2, 2, 2, 2, 2, 2, 2, 2, 2, 2, 2, 2, 2, 2, 2, 2, 2, 2, 2, 2, 2, 2, 2, 2, 2, 2, 2, 2, 2, 2, 2, 2, 2, 2, 2, 2, 2, 2, 2, 2, 2, 2, 2, 2, 2, 2, 2, 2, 2, 2, 2, 2, 2, 2, 2, 2, 3 ),
 ( 0.000000000000000000, 1.000000000000000000 ),
 ( 0.000000000000000000, 0.008333333333333333218, 0.01666666666666666644, 0.02500000000000000139, 0.03333333333333333287, 0.04166666666666666435, 0.05000000000000000278, 0.05833333333333333426, 0.06666666666666666574, 0.07499999999999999722, 0.08333333333333332871, 0.09166666666666666019, 0.1000000000000000056, 0.1083333333333333370, 0.1166666666666666685, 0.1250000000000000000, 0.1333333333333333315, 0.1416666666666666630, 0.1499999999999999944, 0.1583333333333333259, 0.1666666666666666574, 0.1749999999999999889, 0.1833333333333333204, 0.1916666666666666796, 0.2000000000000000111, 0.2083333333333333426, 0.2166666666666666741, 0.2250000000000000056, 0.2333333333333333370, 0.2416666666666666685, 0.2500000000000000000, 0.2583333333333333592, 0.2666666666666666630, 0.2750000000000000222, 0.2833333333333333259, 0.2916666666666666852, 0.2999999999999999889, 0.3083333333333333481, 0.3166666666666666519, 0.3250000000000000111, 0.3333333333333333148, 0.3416666666666666741, 0.3499999999999999778, 0.3583333333333333370, 0.3666666666666666408, 0.3750000000000000000, 0.3833333333333333592, 0.3916666666666666630, 0.4000000000000000222, 0.4083333333333333259, 0.4166666666666666852, 0.4249999999999999889, 0.4333333333333333481, 0.4416666666666666519, 0.4500000000000000111, 0.4583333333333333148, 0.4666666666666666741, 0.4749999999999999778, 0.4833333333333333370, 0.4916666666666666408, 0.5000000000000000000, 0.5083333333333333037, 0.5166666666666667185, 0.5250000000000000222, 0.5333333333333333259, 0.5416666666666666297, 0.5500000000000000444, 0.5583333333333333481, 0.5666666666666666519, 0.5749999999999999556, 0.5833333333333333703, 0.5916666666666666741, 0.5999999999999999778, 0.6083333333333332815, 0.6166666666666666963, 0.6250000000000000000, 0.6333333333333333037, 0.6416666666666667185, 0.6500000000000000222, 0.6583333333333333259, 0.6666666666666666297, 0.6750000000000000444, 0.6833333333333333481, 0.6916666666666666519, 0.6999999999999999556, 0.7083333333333333703, 0.7166666666666666741, 0.7249999999999999778, 0.7333333333333332815, 0.7416666666666666963, 0.7500000000000000000, 0.7583333333333333037, 0.7666666666666667185, 0.7750000000000000222, 0.7833333333333333259, 0.7916666666666666297, 0.8000000000000000444, 0.8083333333333333481, 0.8166666666666666519, 0.8249999999999999556, 0.8333333333333333703, 0.8416666666666666741, 0.8499999999999999778, 0.8583333333333332815, 0.8666666666666666963, 0.8750000000000000000, 0.8833333333333333037, 0.8916666666666667185, 0.9000000000000000222, 0.9083333333333333259, 0.9166666666666666297, 0.9250000000000000444, 0.9333333333333333481, 0.9416666666666666519, 0.9499999999999999556, 0.9583333333333333703, 0.9666666666666666741, 0.9749999999999999778, 0.9833333333333332815, 0.9916666666666666963, 1.000000000000000000 ),
 .UNSPECIFIED. ) 
 GEOMETRIC_REPRESENTATION_ITEM ( )  RATIONAL_B_SPLINE_SURFACE ( (
 ( 1.000000000000000000, 0.8660254037844387076, 1.000000000000000000, 0.8660254037844387076, 1.000000000000000000, 0.8660254037844387076, 1.000000000000000000, 0.8660254037844387076, 1.000000000000000000, 0.8660254037844387076, 1.000000000000000000, 0.8660254037844387076, 1.000000000000000000, 0.8660254037844387076, 1.000000000000000000, 0.8660254037844387076, 1.000000000000000000, 0.8660254037844387076, 1.000000000000000000, 0.8660254037844387076, 1.000000000000000000, 0.8660254037844387076, 1.000000000000000000, 0.8660254037844387076, 1.000000000000000000, 0.8660254037844387076, 1.000000000000000000, 0.8660254037844387076, 1.000000000000000000, 0.8660254037844387076, 1.000000000000000000, 0.8660254037844387076, 1.000000000000000000, 0.8660254037844387076, 1.000000000000000000, 0.8660254037844387076, 1.000000000000000000, 0.8660254037844387076, 1.000000000000000000, 0.8660254037844387076, 1.000000000000000000, 0.8660254037844387076, 1.000000000000000000, 0.8660254037844387076, 1.000000000000000000, 0.8660254037844387076, 1.000000000000000000, 0.8660254037844387076, 1.000000000000000000, 0.8660254037844387076, 1.000000000000000000, 0.8660254037844387076, 1.000000000000000000, 0.8660254037844387076, 1.000000000000000000, 0.8660254037844387076, 1.000000000000000000, 0.8660254037844387076, 1.000000000000000000, 0.8660254037844387076, 1.000000000000000000, 0.8660254037844387076, 1.000000000000000000, 0.8660254037844387076, 1.000000000000000000, 0.8660254037844387076, 1.000000000000000000, 0.8660254037844387076, 1.000000000000000000, 0.8660254037844387076, 1.000000000000000000, 0.8660254037844387076, 1.000000000000000000, 0.8660254037844387076, 1.000000000000000000, 0.8660254037844387076, 1.000000000000000000, 0.8660254037844387076, 1.000000000000000000, 0.8660254037844387076, 1.000000000000000000, 0.8660254037844387076, 1.000000000000000000, 0.8660254037844387076, 1.000000000000000000, 0.8660254037844387076, 1.000000000000000000, 0.8660254037844387076, 1.000000000000000000, 0.8660254037844387076, 1.000000000000000000, 0.8660254037844387076, 1.000000000000000000, 0.8660254037844387076, 1.000000000000000000, 0.8660254037844387076, 1.000000000000000000, 0.8660254037844387076, 1.000000000000000000, 0.8660254037844387076, 1.000000000000000000, 0.8660254037844387076, 1.000000000000000000, 0.8660254037844387076, 1.000000000000000000, 0.8660254037844387076, 1.000000000000000000, 0.8660254037844387076, 1.000000000000000000, 0.8660254037844387076, 1.000000000000000000, 0.8660254037844387076, 1.000000000000000000, 0.8660254037844387076, 1.000000000000000000, 0.8660254037844387076, 1.000000000000000000, 0.8660254037844387076, 1.000000000000000000, 0.8660254037844387076, 1.000000000000000000, 0.8660254037844387076, 1.000000000000000000, 0.8660254037844387076, 1.000000000000000000, 0.8660254037844387076, 1.000000000000000000, 0.8660254037844387076, 1.000000000000000000, 0.8660254037844387076, 1.000000000000000000, 0.8660254037844387076, 1.000000000000000000, 0.8660254037844387076, 1.000000000000000000, 0.8660254037844387076, 1.000000000000000000, 0.8660254037844387076, 1.000000000000000000, 0.8660254037844387076, 1.000000000000000000, 0.8660254037844387076, 1.000000000000000000, 0.8660254037844387076, 1.000000000000000000, 0.8660254037844387076, 1.000000000000000000, 0.8660254037844387076, 1.000000000000000000, 0.8660254037844387076, 1.000000000000000000, 0.8660254037844387076, 1.000000000000000000, 0.8660254037844387076, 1.000000000000000000, 0.8660254037844387076, 1.000000000000000000, 0.8660254037844387076, 1.000000000000000000, 0.8660254037844387076, 1.000000000000000000, 0.8660254037844387076, 1.000000000000000000, 0.8660254037844387076, 1.000000000000000000, 0.8660254037844387076, 1.000000000000000000, 0.8660254037844387076, 1.000000000000000000, 0.8660254037844387076, 1.000000000000000000, 0.8660254037844387076, 1.000000000000000000, 0.8660254037844387076, 1.000000000000000000, 0.8660254037844387076, 1.000000000000000000, 0.8660254037844387076, 1.000000000000000000, 0.8660254037844387076, 1.000000000000000000, 0.8660254037844387076, 1.000000000000000000, 0.8660254037844387076, 1.000000000000000000, 0.8660254037844387076, 1.000000000000000000, 0.8660254037844387076, 1.000000000000000000, 0.8660254037844387076, 1.000000000000000000, 0.8660254037844387076, 1.000000000000000000, 0.8660254037844387076, 1.000000000000000000, 0.8660254037844387076, 1.000000000000000000, 0.8660254037844387076, 1.000000000000000000, 0.8660254037844387076, 1.000000000000000000, 0.8660254037844387076, 1.000000000000000000, 0.8660254037844387076, 1.000000000000000000, 0.8660254037844387076, 1.000000000000000000, 0.8660254037844387076, 1.000000000000000000, 0.8660254037844387076, 1.000000000000000000, 0.8660254037844387076, 1.000000000000000000, 0.8660254037844387076, 1.000000000000000000, 0.8660254037844387076, 1.000000000000000000, 0.8660254037844387076, 1.000000000000000000, 0.8660254037844387076, 1.000000000000000000, 0.8660254037844387076, 1.000000000000000000, 0.8660254037844387076, 1.000000000000000000, 0.8660254037844387076, 1.000000000000000000, 0.8660254037844387076, 1.000000000000000000, 0.8660254037844387076, 1.000000000000000000, 0.8660254037844387076, 1.000000000000000000, 0.8660254037844387076, 1.000000000000000000, 0.8660254037844387076, 1.000000000000000000, 0.8660254037844387076, 1.000000000000000000, 0.8660254037844387076, 1.000000000000000000),
 ( 1.000000000000000000, 0.8660254037844387076, 1.000000000000000000, 0.8660254037844387076, 1.000000000000000000, 0.8660254037844387076, 1.000000000000000000, 0.8660254037844387076, 1.000000000000000000, 0.8660254037844387076, 1.000000000000000000, 0.8660254037844387076, 1.000000000000000000, 0.8660254037844387076, 1.000000000000000000, 0.8660254037844387076, 1.000000000000000000, 0.8660254037844387076, 1.000000000000000000, 0.8660254037844387076, 1.000000000000000000, 0.8660254037844387076, 1.000000000000000000, 0.8660254037844387076, 1.000000000000000000, 0.8660254037844387076, 1.000000000000000000, 0.8660254037844387076, 1.000000000000000000, 0.8660254037844387076, 1.000000000000000000, 0.8660254037844387076, 1.000000000000000000, 0.8660254037844387076, 1.000000000000000000, 0.8660254037844387076, 1.000000000000000000, 0.8660254037844387076, 1.000000000000000000, 0.8660254037844387076, 1.000000000000000000, 0.8660254037844387076, 1.000000000000000000, 0.8660254037844387076, 1.000000000000000000, 0.8660254037844387076, 1.000000000000000000, 0.8660254037844387076, 1.000000000000000000, 0.8660254037844387076, 1.000000000000000000, 0.8660254037844387076, 1.000000000000000000, 0.8660254037844387076, 1.000000000000000000, 0.8660254037844387076, 1.000000000000000000, 0.8660254037844387076, 1.000000000000000000, 0.8660254037844387076, 1.000000000000000000, 0.8660254037844387076, 1.000000000000000000, 0.8660254037844387076, 1.000000000000000000, 0.8660254037844387076, 1.000000000000000000, 0.8660254037844387076, 1.000000000000000000, 0.8660254037844387076, 1.000000000000000000, 0.8660254037844387076, 1.000000000000000000, 0.8660254037844387076, 1.000000000000000000, 0.8660254037844387076, 1.000000000000000000, 0.8660254037844387076, 1.000000000000000000, 0.8660254037844387076, 1.000000000000000000, 0.8660254037844387076, 1.000000000000000000, 0.8660254037844387076, 1.000000000000000000, 0.8660254037844387076, 1.000000000000000000, 0.8660254037844387076, 1.000000000000000000, 0.8660254037844387076, 1.000000000000000000, 0.8660254037844387076, 1.000000000000000000, 0.8660254037844387076, 1.000000000000000000, 0.8660254037844387076, 1.000000000000000000, 0.8660254037844387076, 1.000000000000000000, 0.8660254037844387076, 1.000000000000000000, 0.8660254037844387076, 1.000000000000000000, 0.8660254037844387076, 1.000000000000000000, 0.8660254037844387076, 1.000000000000000000, 0.8660254037844387076, 1.000000000000000000, 0.8660254037844387076, 1.000000000000000000, 0.8660254037844387076, 1.000000000000000000, 0.8660254037844387076, 1.000000000000000000, 0.8660254037844387076, 1.000000000000000000, 0.8660254037844387076, 1.000000000000000000, 0.8660254037844387076, 1.000000000000000000, 0.8660254037844387076, 1.000000000000000000, 0.8660254037844387076, 1.000000000000000000, 0.8660254037844387076, 1.000000000000000000, 0.8660254037844387076, 1.000000000000000000, 0.8660254037844387076, 1.000000000000000000, 0.8660254037844387076, 1.000000000000000000, 0.8660254037844387076, 1.000000000000000000, 0.8660254037844387076, 1.000000000000000000, 0.8660254037844387076, 1.000000000000000000, 0.8660254037844387076, 1.000000000000000000, 0.8660254037844387076, 1.000000000000000000, 0.8660254037844387076, 1.000000000000000000, 0.8660254037844387076, 1.000000000000000000, 0.8660254037844387076, 1.000000000000000000, 0.8660254037844387076, 1.000000000000000000, 0.8660254037844387076, 1.000000000000000000, 0.8660254037844387076, 1.000000000000000000, 0.8660254037844387076, 1.000000000000000000, 0.8660254037844387076, 1.000000000000000000, 0.8660254037844387076, 1.000000000000000000, 0.8660254037844387076, 1.000000000000000000, 0.8660254037844387076, 1.000000000000000000, 0.8660254037844387076, 1.000000000000000000, 0.8660254037844387076, 1.000000000000000000, 0.8660254037844387076, 1.000000000000000000, 0.8660254037844387076, 1.000000000000000000, 0.8660254037844387076, 1.000000000000000000, 0.8660254037844387076, 1.000000000000000000, 0.8660254037844387076, 1.000000000000000000, 0.8660254037844387076, 1.000000000000000000, 0.8660254037844387076, 1.000000000000000000, 0.8660254037844387076, 1.000000000000000000, 0.8660254037844387076, 1.000000000000000000, 0.8660254037844387076, 1.000000000000000000, 0.8660254037844387076, 1.000000000000000000, 0.8660254037844387076, 1.000000000000000000, 0.8660254037844387076, 1.000000000000000000, 0.8660254037844387076, 1.000000000000000000, 0.8660254037844387076, 1.000000000000000000, 0.8660254037844387076, 1.000000000000000000, 0.8660254037844387076, 1.000000000000000000, 0.8660254037844387076, 1.000000000000000000, 0.8660254037844387076, 1.000000000000000000, 0.8660254037844387076, 1.000000000000000000, 0.8660254037844387076, 1.000000000000000000, 0.8660254037844387076, 1.000000000000000000, 0.8660254037844387076, 1.000000000000000000, 0.8660254037844387076, 1.000000000000000000, 0.8660254037844387076, 1.000000000000000000, 0.8660254037844387076, 1.000000000000000000, 0.8660254037844387076, 1.000000000000000000, 0.8660254037844387076, 1.000000000000000000, 0.8660254037844387076, 1.000000000000000000, 0.8660254037844387076, 1.000000000000000000, 0.8660254037844387076, 1.000000000000000000, 0.8660254037844387076, 1.000000000000000000, 0.8660254037844387076, 1.000000000000000000, 0.8660254037844387076, 1.000000000000000000, 0.8660254037844387076, 1.000000000000000000, 0.8660254037844387076, 1.000000000000000000) ) ) 
 REPRESENTATION_ITEM ( '' )  SURFACE ( )  );
#175179 = CARTESIAN_POINT ( 'NONE',  ( 3.972980863544761654, -1.569110274459505350, 1.426624754300914510 ) ) ;
#175180 = CARTESIAN_POINT ( 'NONE',  ( -4.423703259808839938, 8.383013913077441259, 0.7998128361456352531 ) ) ;
#175181 = CARTESIAN_POINT ( 'NONE',  ( 4.434552454296070145, 2.119417814153037316, 0.4246342833542292028 ) ) ;
#175182 = CARTESIAN_POINT ( 'NONE',  ( 4.528748383445759806, -1.681502307688139908, 0.7506017836093890061 ) ) ;
#175183 = CARTESIAN_POINT ( 'NONE',  ( -5.266216980226317013, 6.417262052691032004, 1.151019644853501944 ) ) ;
#175184 = CARTESIAN_POINT ( 'NONE',  ( 0.6823417656249899377, 1.655208333674752730, 1.181850606188755259 ) ) ;
#175185 = CARTESIAN_POINT ( 'NONE',  ( 6.158121301954061266, -1.225565299391921936, 1.235896697784558906 ) ) ;
#175186 = CARTESIAN_POINT ( 'NONE',  ( 6.727182134110198497, 4.703735537933666500, 2.273690654489219032 ) ) ;
#175187 = CARTESIAN_POINT ( 'NONE',  ( 2.236732156574683827, 5.553345249405011508, 1.040834085586084257E-14 ) ) ;
#175188 = FACE_OUTER_BOUND ( 'NONE', #194233, .T. ) ;
#175189 = CARTESIAN_POINT ( 'NONE',  ( 3.608425205800522839, -0.8741791752944136906, -1.977237025433141504 ) ) ;
#175190 = CARTESIAN_POINT ( 'NONE',  ( 5.220077296912079667, -1.701688162634030999, -1.080898591909580597 ) ) ;
#175191 = CARTESIAN_POINT ( 'NONE',  ( -9.286972035236635392, 9.937148250638648150, -0.7216878364870267237 ) ) ;
#175192 = CARTESIAN_POINT ( 'NONE',  ( 2.307699607974790901, -0.4742087202370263155, 2.108885336910087283 ) ) ;
#175193 = ADVANCED_FACE ( 'NONE', ( #52064 ), #34727, .F. ) ;
#175194 = CARTESIAN_POINT ( 'NONE',  ( 3.796128654474308028, -1.968949637145664955, -0.1001596523246932047 ) ) ;
#175195 = CARTESIAN_POINT ( 'NONE',  ( 2.852750215419812108, -1.865046845876184189, -0.7672916333427428626 ) ) ;
#175196 = CARTESIAN_POINT ( 'NONE',  ( -0.3388969742604198143, -7.666862915010146828, 10.99522790877599654 ) ) ;
#175197 = CARTESIAN_POINT ( 'NONE',  ( 1.255362601414770296, -1.817582055312426004, 1.421667062125511860 ) ) ;
#175198 = CARTESIAN_POINT ( 'NONE',  ( 4.054194213510796452, -1.436945492307143635, 1.306602268835421077 ) ) ;
#175201 = EDGE_LOOP ( 'NONE', ( #81294, #168106, #199834, #37207 ) ) ;
#175200 = CARTESIAN_POINT ( 'NONE',  ( -6.901817412891860570, -6.554751173179683477, 6.500815856195042208 ) ) ;
#175199 = CARTESIAN_POINT ( 'NONE',  ( -8.419250203962027612, 11.80591375705560608, 1.082531754730549967 ) ) ;
#175202 = AXIS2_PLACEMENT_3D ( 'NONE', #170058, #204675, #5397 ) ;
#175203 = CARTESIAN_POINT ( 'NONE',  ( -6.957269102468015554, 8.145844036748005834, 1.199719254218452047 ) ) ;
#175204 = CARTESIAN_POINT ( 'NONE',  ( -11.89829993707161471, 12.27080771748872046, 1.561606677374347552 ) ) ;
#175206 = ORIENTED_EDGE ( 'NONE', *, *, #89413, .T. ) ;
#175205 = CARTESIAN_POINT ( 'NONE',  ( -4.817943484809863008, 6.714296380401858499, 1.599625672291263179 ) ) ;
#175207 = CARTESIAN_POINT ( 'NONE',  ( -7.876924059415400414, 9.252461493148505411, 1.082531754730558626 ) ) ;
#175208 = CARTESIAN_POINT ( 'NONE',  ( 2.661379449941482012, -1.919611247835448342, -1.088434722066232485 ) ) ;
#175209 = CARTESIAN_POINT ( 'NONE',  ( 3.285556943750000070, -0.2843749995220419269, 0.000000000000000000 ) ) ;
#175210 = CARTESIAN_POINT ( 'NONE',  ( 6.016451032921247055, 0.7918200671565789328, 1.795022358689958963 ) ) ;
#175211 = CARTESIAN_POINT ( 'NONE',  ( -1.500000000000001110, 9.020833333333330373, 0.8660254037844418162 ) ) ;
#175212 = CARTESIAN_POINT ( 'NONE',  ( -0.7499999999999972244, 4.139583334016149863, -1.299038105676652899 ) ) ;
#175213 = CARTESIAN_POINT ( 'NONE',  ( -15.75000000000000000, 10.90000000000000036, -1.800000000000001155 ) ) ;
#175215 = DIRECTION ( 'NONE',  ( 0.05872483221476467591, 7.952201780260630618E-17, 0.9982742078614211811 ) ) ;
#175214 = DIRECTION ( 'NONE',  ( 0.6507913734559641616, -0.7592566023653004592, 0.000000000000000000 ) ) ;
#175216 = CARTESIAN_POINT ( 'NONE',  ( 5.859284738525260217, 1.813109059707292747, -0.3191327317438249489 ) ) ;
#175217 = ORIENTED_EDGE ( 'NONE', *, *, #23157, .T. ) ;
#175218 = CARTESIAN_POINT ( 'NONE',  ( -0.6801582343750213200, -0.3177083329919394572, 1.178068619123815663 ) ) ;
#175219 = CARTESIAN_POINT ( 'NONE',  ( -6.008234629150358330, 10.16135750065076060, 0.000000000000000000 ) ) ;
#175220 = CYLINDRICAL_SURFACE ( 'NONE', #75711, 11.49999999999998934 ) ;
#175221 = CARTESIAN_POINT ( 'NONE',  ( 6.258074605086497932, 0.8102346573028992305, -1.959903593942226685 ) ) ;
#175222 = CARTESIAN_POINT ( 'NONE',  ( 11.70600796652113829, 7.005607364824809835, -2.416925703268587355 ) ) ;
#175223 = CARTESIAN_POINT ( 'NONE',  ( 4.310602774141044868, 7.116454772218158809, -1.199719254218452047 ) ) ;
#175224 = CARTESIAN_POINT ( 'NONE',  ( 0.3739917644934092067, 1.186169308094830344, 1.685110605438163045 ) ) ;
#175227 = CARTESIAN_POINT ( 'NONE',  ( 4.300242120186610784, 1.420457692841030850, -1.171515996850613694 ) ) ;
#175226 = CARTESIAN_POINT ( 'NONE',  ( 2.312761410774709425, -1.440873624601293423, 1.177899742917737358 ) ) ;
#175225 = CARTESIAN_POINT ( 'NONE',  ( -10.52211811376581707, 5.354010262649191887, 5.769489279399182102 ) ) ;
#175228 = CARTESIAN_POINT ( 'NONE',  ( 5.933664784275179294, 10.07435934829639912, -0.7998128361456291469 ) ) ;
#175229 = CARTESIAN_POINT ( 'NONE',  ( -9.333041836230190569, 14.55305236562365145, -7.472413793097476109 ) ) ;
#175230 = CARTESIAN_POINT ( 'NONE',  ( -6.303615075710993665, 6.318915441276411471, -0.7998128361456362523 ) ) ;
#175232 = VERTEX_POINT ( 'NONE', #23809 ) ;
#175231 = CARTESIAN_POINT ( 'NONE',  ( -9.765991159989196646, -7.287292132423887736, 1.138412281109779656E-15 ) ) ;
#175233 = CARTESIAN_POINT ( 'NONE',  ( 4.319099500008596770, 2.017107695584336557, 0.8957252843501888329 ) ) ;
#175234 = CARTESIAN_POINT ( 'NONE',  ( 6.028679731477588177, 2.178036183261321757, 0.6118574502519974478 ) ) ;
#175235 = CARTESIAN_POINT ( 'NONE',  ( -4.772106882330227506, 7.550913215151819458, -1.082531754730549967 ) ) ;
#175236 = CARTESIAN_POINT ( 'NONE',  ( 0.1055216070770526038, 1.418477292093557329, 1.282857148695019989 ) ) ;
#175237 = CARTESIAN_POINT ( 'NONE',  ( 6.174997428096934193, 1.663181612469267101, -0.9506077395253130780 ) ) ;
#175238 = CARTESIAN_POINT ( 'NONE',  ( 4.853455804012222430, 5.725081861844796727, 1.082531754730560403 ) ) ;
#175239 = CARTESIAN_POINT ( 'NONE',  ( 4.572363442555127833, 8.499999999999996447, 0.3169179603640607246 ) ) ;
#175240 = CARTESIAN_POINT ( 'NONE',  ( 5.373660369522260005, 0.3689257714810100230, -1.876182517032434438 ) ) ;
#175241 = DIRECTION ( 'NONE',  ( 0.000000000000000000, 8.546850786086437571E-32, 1.000000000000000000 ) ) ;
#175242 = CARTESIAN_POINT ( 'NONE',  ( 0.4439547499465161251, 1.865322535695708606, 0.1421067652795371117 ) ) ;
#175243 = CARTESIAN_POINT ( 'NONE',  ( 1.956267901341804283, -1.236798062192035363, 1.592663274815858676 ) ) ;
#175245 = CARTESIAN_POINT ( 'NONE',  ( 4.195997148085639061, -0.8063668458072065226, 1.945788449171739876 ) ) ;
#175244 = CARTESIAN_POINT ( 'NONE',  ( -8.859363311525973117, 12.42334206583395328, -1.199719254218446718 ) ) ;
#175246 = CARTESIAN_POINT ( 'NONE',  ( 6.611572464958476836, 10.86525164242692298, 0.7998128361456462443 ) ) ;
#175248 = CARTESIAN_POINT ( 'NONE',  ( -6.665805079413154921, 10.92852302595736447, 0.7998128361456481317 ) ) ;
#175247 = CARTESIAN_POINT ( 'NONE',  ( 1.499999999999985123, -0.4541666666666469010, -0.8660254037844323793 ) ) ;
#175249 = DIRECTION ( 'NONE',  ( 0.000000000000000000, 7.254698431505021095E-17, -1.000000000000000000 ) ) ;
#175250 = CARTESIAN_POINT ( 'NONE',  ( 2.549087187268097576, 0.2513027392179004171, 2.004046050866041817 ) ) ;
#175251 = CARTESIAN_POINT ( 'NONE',  ( -1.201851678989727383E-14, 3.946875000341423689, -1.575800808251660134 ) ) ;
#175252 = CARTESIAN_POINT ( 'NONE',  ( 8.595506201384008449, 11.05117653974661529, 1.443375672974076540 ) ) ;
#175253 = CARTESIAN_POINT ( 'NONE',  ( 4.903692054014650026, -0.5817465652163296141, 2.081756923971528117 ) ) ;
#175254 = CARTESIAN_POINT ( 'NONE',  ( 6.230854113932139171, 9.427024345299638952, 1.199719254218452047 ) ) ;
#175255 = CARTESIAN_POINT ( 'NONE',  ( 0.7499999999999920064, 5.483333333333353821, 1.299038105676669330 ) ) ;
#175257 = PRESENTATION_STYLE_ASSIGNMENT (( #125505 ) ) ;
#175256 = CARTESIAN_POINT ( 'NONE',  ( 7.828907357248368726, 8.098423103070084395, 0.7998128361456281477 ) ) ;
#175258 = CARTESIAN_POINT ( 'NONE',  ( 7.076992996209058973, 11.20031622897851165, 1.040834085586084257E-14 ) ) ;
#175260 = CARTESIAN_POINT ( 'NONE',  ( 8.733437601049905297, 14.92147133172287354, -8.230922393287746885 ) ) ;
#175259 = CARTESIAN_POINT ( 'NONE',  ( 1.697964449562241018, -1.571978469985369831, -1.497844480664213052 ) ) ;
#175262 = CARTESIAN_POINT ( 'NONE',  ( 1.012948470060770934, -1.796336717620912626, 0.4034172393945419377 ) ) ;
#175261 = CARTESIAN_POINT ( 'NONE',  ( -7.104109303880803417, 8.350844278358124484, 1.082531754730549967 ) ) ;
#175263 = CARTESIAN_POINT ( 'NONE',  ( 1.364683531249986537, 2.655208333674754062, -0.7879004041258239610 ) ) ;
#175264 = CARTESIAN_POINT ( 'NONE',  ( 1.558417602779540889, -1.546676288433556756, 1.552911753681482487 ) ) ;
#175265 = CARTESIAN_POINT ( 'NONE',  ( 6.883263157960364254, 4.694764272337425659, 2.516417202187768432 ) ) ;
#175266 = CARTESIAN_POINT ( 'NONE',  ( 3.204270770158343939, -2.259979215032235977, 0.1094169825565076415 ) ) ;
#175267 = CARTESIAN_POINT ( 'NONE',  ( -7.531718027591449705, 8.745758106066849891, 1.199719254218462483 ) ) ;
#175268 = CARTESIAN_POINT ( 'NONE',  ( -1.364683531249997417, 4.321875000341417028, 1.214306433183764966E-14 ) ) ;
#175269 = CARTESIAN_POINT ( 'NONE',  ( 4.990887655837901171, 7.926359819171765686, 1.063311220390166234 ) ) ;
#175270 = CARTESIAN_POINT ( 'NONE',  ( -0.7500000000000006661, 11.95833333333333393, -1.299038105676657340 ) ) ;
#175271 = CARTESIAN_POINT ( 'NONE',  ( 7.038091139269835317, 7.383730215335837954, 0.000000000000000000 ) ) ;
#175272 = CARTESIAN_POINT ( 'NONE',  ( 4.376060336092471026, -1.020005645217741064, 1.445989269263460386 ) ) ;
#175273 = CARTESIAN_POINT ( 'NONE',  ( 7.397945374551106568, 11.78268670361832093, -0.7998128361456291469 ) ) ;
#175274 = CARTESIAN_POINT ( 'NONE',  ( 0.3937647135470741522, 1.560644430845319119, 1.414193795423605904 ) ) ;
#175276 = CARTESIAN_POINT ( 'NONE',  ( -0.7500000000000215383, 1.441666666666688190, 1.299038105676659116 ) ) ;
#175275 = CARTESIAN_POINT ( 'NONE',  ( -1.364683531250010295, 10.13020833367472839, 0.7879004041258445001 ) ) ;
#175277 = CARTESIAN_POINT ( 'NONE',  ( -4.984557751679625781, 5.844347460828191565, 1.199719254218452935 ) ) ;
#175278 = CARTESIAN_POINT ( 'NONE',  ( 6.011342256177333532, -1.897693555989588887, 0.6820111564242032909 ) ) ;
#175279 = ORIENTED_EDGE ( 'NONE', *, *, #128500, .T. ) ;
#175280 = CARTESIAN_POINT ( 'NONE',  ( 7.510853912290742507, 8.825379654836435606, -1.082531754730537976 ) ) ;
#175281 = EDGE_CURVE ( 'NONE', #108269, #86684, #139737, .T. ) ;
#175282 = CARTESIAN_POINT ( 'NONE',  ( 9.531545685607134999, 11.07889037375188401, 1.199719254218450271 ) ) ;
#175284 = CARTESIAN_POINT ( 'NONE',  ( 3.660894226558962128, -1.649352935060313552, -0.8826137995501317501 ) ) ;
#175283 = AXIS2_PLACEMENT_3D ( 'NONE', #87022, #150973, #52394 ) ;
#175285 = CARTESIAN_POINT ( 'NONE',  ( 4.205968427668831389, 0.7022645179026367757, -1.947615878368731623 ) ) ;
#175286 = CARTESIAN_POINT ( 'NONE',  ( -6.414416072596849538, 7.616478518518682073, -1.082531754730549967 ) ) ;
#175287 = CARTESIAN_POINT ( 'NONE',  ( -1.500000000000015099, 10.76041666734946212, -0.8660254037844309360 ) ) ;
#175288 = CARTESIAN_POINT ( 'NONE',  ( 7.377608144130607393, 11.75895993479440982, -0.7998128361456291469 ) ) ;
#175289 = CARTESIAN_POINT ( 'NONE',  ( -4.568734577680894304, 5.392907097791561633, -1.082531754730543971 ) ) ;
#175290 = CARTESIAN_POINT ( 'NONE',  ( 6.424584688029230328, 8.588711117491191871, 1.599625672291268286 ) ) ;
#175291 = CARTESIAN_POINT ( 'NONE',  ( -4.910702663797468226, 4.682374061739900561, -0.3233530799688824064 ) ) ;
#175292 = CARTESIAN_POINT ( 'NONE',  ( -1.364683531249997417, 5.321875000341417916, 1.214306433183764966E-14 ) ) ;
#175293 = EDGE_CURVE ( 'NONE', #130778, #24109, #60537, .T. ) ;
#175294 = CARTESIAN_POINT ( 'NONE',  ( 3.982823771651412770, 1.862158852298421152, 0.6176278068941787325 ) ) ;
#175295 = CARTESIAN_POINT ( 'NONE',  ( 2.249374845261054467, -1.976652949091894707, -0.3960421909960794018 ) ) ;
#175296 = CARTESIAN_POINT ( 'NONE',  ( -11.92619526913699879, 12.69999999999999929, -1.328859060402686199 ) ) ;
#175297 = CARTESIAN_POINT ( 'NONE',  ( -4.948362879307902418, 4.875437568721725512, 1.214306433183764966E-14 ) ) ;
#175298 = CARTESIAN_POINT ( 'NONE',  ( 1.000990332655056436, 1.525750722454706443, 1.081861512215509524 ) ) ;
#175299 = CARTESIAN_POINT ( 'NONE',  ( 0.6823417656249899377, 4.426041667008086655, -1.181850606188754593 ) ) ;
#175300 = CARTESIAN_POINT ( 'NONE',  ( 3.340093095703601023, -1.202498264213421209, -1.614455356613291093 ) ) ;
#175302 = CARTESIAN_POINT ( 'NONE',  ( 3.427469813117941744, -1.604901852541072760, -1.381049200617268102 ) ) ;
#175301 = CARTESIAN_POINT ( 'NONE',  ( -6.290620087060847965, 7.401773525401500464, 1.082531754730549967 ) ) ;
#175303 = CARTESIAN_POINT ( 'NONE',  ( 4.967269779104159788, 1.799668380515653920, 1.023422521214325309 ) ) ;
#175304 = CARTESIAN_POINT ( 'NONE',  ( 4.004454267989866700, 5.765225627445230927, 1.599625672291262513 ) ) ;
#175306 = CARTESIAN_POINT ( 'NONE',  ( 2.218730694130720771, 5.740269576461138890, 0.7998128361456462443 ) ) ;
#175305 = CARTESIAN_POINT ( 'NONE',  ( 0.4157161284131759005, -1.121801286243618190, -1.764121917367883263 ) ) ;
#175308 = ORIENTED_EDGE ( 'NONE', *, *, #189945, .T. ) ;
#175307 = CARTESIAN_POINT ( 'NONE',  ( 5.702125722003772879, -1.825762228975034596, 0.002264948092654816680 ) ) ;
#175309 = CARTESIAN_POINT ( 'NONE',  ( 9.589694723567584234, 10.08239868711733855, -0.7998128361456281477 ) ) ;
#175310 = DIRECTION ( 'NONE',  ( -1.000000000000000000, 0.000000000000000000, 0.000000000000000000 ) ) ;
#175311 = CARTESIAN_POINT ( 'NONE',  ( 10.81425746553161460, 10.30853785568457326, -6.489671246970442731 ) ) ;
#175312 = CARTESIAN_POINT ( 'NONE',  ( -10.71692179555930302, 5.308633586712264041, 6.728550107195007790 ) ) ;
#175313 = CARTESIAN_POINT ( 'NONE',  ( 1.364683531249997417, 12.04687500034139980, 2.602085213965210642E-15 ) ) ;
#175314 = CARTESIAN_POINT ( 'NONE',  ( 6.463533315534490065, -1.538886664202097965, -1.134999244291827747 ) ) ;
#175316 = CARTESIAN_POINT ( 'NONE',  ( -8.727698198895085469, 11.20540053684285553, -1.599625672291263179 ) ) ;
#175315 = CIRCLE ( 'NONE', #43906, 3.475000000000000089 ) ;
#175317 = CARTESIAN_POINT ( 'NONE',  ( 6.928380191783277908, 8.041863964290678624, 1.199719254218462483 ) ) ;
#175318 = CARTESIAN_POINT ( 'NONE',  ( -1.360316468750058849, 2.692708333674814991, 0.7853790794158641564 ) ) ;
#175319 = CARTESIAN_POINT ( 'NONE',  ( 3.172244755473273781, 6.644776614786712443, 0.000000000000000000 ) ) ;
#175320 = EDGE_CURVE ( 'NONE', #193052, #102754, #74076, .T. ) ;
#175321 = CARTESIAN_POINT ( 'NONE',  ( -1.115562610750309283E-14, 9.812500000000000000, 1.500000000000001554 ) ) ;
#175322 = CARTESIAN_POINT ( 'NONE',  ( 5.009901455449552010, 5.803638771901306725, -1.199719254218452047 ) ) ;
#175323 = ORIENTED_EDGE ( 'NONE', *, *, #15931, .T. ) ;
#175324 = PRESENTATION_LAYER_ASSIGNMENT (  '', '', ( #19612 ) ) ;
#175325 = CARTESIAN_POINT ( 'NONE',  ( -5.855142236255304944, 7.924361590421551860, -1.599625672291271394 ) ) ;
#175327 = CARTESIAN_POINT ( 'NONE',  ( 5.643937085038755797, 9.806620042512378177, -0.7998128361456481317 ) ) ;
#175326 = CARTESIAN_POINT ( 'NONE',  ( -15.75000000000000000, 12.69999999999998153, 3.599999999999999201 ) ) ;
#175328 = CARTESIAN_POINT ( 'NONE',  ( 1.872228381520318896, 3.299999999999997158, 0.3999999999999958589 ) ) ;
#175329 = CARTESIAN_POINT ( 'NONE',  ( 0.1394461523057501928, 1.435241935670927171, -1.984817279021661829 ) ) ;
#175330 = CARTESIAN_POINT ( 'NONE',  ( -5.422898255786193111, 8.310169817517122581, -1.082531754730544860 ) ) ;
#175331 = CARTESIAN_POINT ( 'NONE',  ( 5.020596955762157698, 4.751784624677624080, 1.040834085586084257E-14 ) ) ;
#175332 = CARTESIAN_POINT ( 'NONE',  ( 2.448051270322794348, -0.8465065455745772738, 1.778409512993859076 ) ) ;
#175333 = EDGE_CURVE ( 'NONE', #29327, #33454, #177185, .T. ) ;
#175334 = CARTESIAN_POINT ( 'NONE',  ( 3.163685574146878565, 1.281377625384312324, 1.556896677758594416 ) ) ;
#175335 = CARTESIAN_POINT ( 'NONE',  ( -8.681298431451969222, 9.022603012982438386, 1.040834085586084257E-14 ) ) ;
#175336 = CARTESIAN_POINT ( 'NONE',  ( 6.827182134110198142, 3.677047352536796154, 2.802821765677898203 ) ) ;
#175337 = STYLED_ITEM ( 'NONE', ( #183116 ), #143840 ) ;
#175338 = CARTESIAN_POINT ( 'NONE',  ( 3.205210054081304438, -0.4271916898582402422, 2.149238826137919389 ) ) ;
#175339 = CARTESIAN_POINT ( 'NONE',  ( 0.000000000000000000, 4.000000000000003553, 0.000000000000000000 ) ) ;
#175340 = CARTESIAN_POINT ( 'NONE',  ( 2.397378046164869936, 1.487928659643242169, 1.223526803071661950 ) ) ;
#175341 = CARTESIAN_POINT ( 'NONE',  ( -8.239604668803112375, 10.63595808506888396, -1.599625672291263179 ) ) ;
#175342 = EDGE_CURVE ( 'NONE', #114519, #83117, #20602, .T. ) ;
#175343 = SURFACE_SIDE_STYLE ('',( #93032 ) ) ;
#175344 = CARTESIAN_POINT ( 'NONE',  ( 0.2331563151865486683, 7.629137130509099585, -2.545728013813946422 ) ) ;
#175345 = CARTESIAN_POINT ( 'NONE',  ( -3.531379743775235003, 15.51966450452909640, -11.47742191263038336 ) ) ;
#175346 = CARTESIAN_POINT ( 'NONE',  ( 6.825640269476072497, 10.05066518344239412, 1.199719254218460707 ) ) ;
#175347 = CARTESIAN_POINT ( 'NONE',  ( 6.145923705696426431, 6.064665832934283962, 0.7998128361456341429 ) ) ;
#175348 = CARTESIAN_POINT ( 'NONE',  ( 0.09916492693110359746, -9.919999999999998153, 9.499482423651659957 ) ) ;
#175349 = CARTESIAN_POINT ( 'NONE',  ( 5.939880696562888751, 7.062853913145737295, -1.082531754730548412 ) ) ;
#175350 = ORIENTED_EDGE ( 'NONE', *, *, #123006, .F. ) ;
#175352 = CARTESIAN_POINT ( 'NONE',  ( 2.912746486309669258, -0.5863433081114779455, -1.925794048158388394 ) ) ;
#175351 = CARTESIAN_POINT ( 'NONE',  ( 6.462460624273299814, -1.686435539877573220, -0.7394478613861471539 ) ) ;
#175353 = CARTESIAN_POINT ( 'NONE',  ( 4.394144163123720581, 0.1076087731387373875, 2.295966082354545801 ) ) ;
#175355 = CARTESIAN_POINT ( 'NONE',  ( 2.483057756668010541, -0.005615179255674587061, 1.861131632832468963 ) ) ;
#175354 = CARTESIAN_POINT ( 'NONE',  ( -0.02900071798685525254, 1.326456003635017922, -2.425894103910302135 ) ) ;
#175356 = CARTESIAN_POINT ( 'NONE',  ( 8.188198428010544205, 8.517596018959260107, 0.000000000000000000 ) ) ;
#175357 = CARTESIAN_POINT ( 'NONE',  ( -4.586165880992525423, 5.350526861157986147, -7.499999999999997335 ) ) ;
#175358 = CARTESIAN_POINT ( 'NONE',  ( 6.293217207623316156, -0.1008467329366956045, -1.909883259500498198 ) ) ;
#175359 = CARTESIAN_POINT ( 'NONE',  ( -6.482770005628665011, 10.71498210654212002, 0.7998128361456481317 ) ) ;
#175360 = CARTESIAN_POINT ( 'NONE',  ( -6.468648687495877958, 6.719380688266201496, 0.000000000000000000 ) ) ;
#175361 = CARTESIAN_POINT ( 'NONE',  ( 6.339408610606328764, 0.7995911543839243629, -1.932009116241965252 ) ) ;
#175362 = CARTESIAN_POINT ( 'NONE',  ( 5.504247177468175600, 8.405076892812779477, 1.082531754730558626 ) ) ;
#175363 = ORIENTED_EDGE ( 'NONE', *, *, #190193, .T. ) ;
#175364 = CARTESIAN_POINT ( 'NONE',  ( 2.974019135304241335, 6.526997603303817286, -0.5344409224624764310 ) ) ;
#175365 = FACE_OUTER_BOUND ( 'NONE', #85284, .T. ) ;
#175366 = CARTESIAN_POINT ( 'NONE',  ( 5.725168984891365831, -0.03570264050535218447, 1.724697241110892509 ) ) ;
#175367 = CARTESIAN_POINT ( 'NONE',  ( -6.749261541504576911, 6.768559974710451677, 1.040834085586084257E-14 ) ) ;
#175368 = CARTESIAN_POINT ( 'NONE',  ( 2.004178618920505972, -1.681731546479984463, 0.4224366712483189623 ) ) ;
#175369 = CARTESIAN_POINT ( 'NONE',  ( -6.518203450479854943, 5.167241622962448488, 2.437504649502892473 ) ) ;
#175370 = CARTESIAN_POINT ( 'NONE',  ( -2.725000000000000089, 0.000000000000000000, 0.000000000000000000 ) ) ;
#175371 = CARTESIAN_POINT ( 'NONE',  ( 5.471592230178073279, -0.3258623020658823477, 2.146390899824067056 ) ) ;
#175372 = CARTESIAN_POINT ( 'NONE',  ( 4.002439121739418404, -0.5745171773131328985, -1.733004836422600725 ) ) ;
#175373 = CARTESIAN_POINT ( 'NONE',  ( 1.780054392102415672, -1.085390340960286082, -1.633940563308281968 ) ) ;
#175374 = CARTESIAN_POINT ( 'NONE',  ( -10.50487009249003378, 11.15010328419353947, 0.7998128361456462443 ) ) ;
#175375 = CARTESIAN_POINT ( 'NONE',  ( 7.832860060393120882, 10.16142270859057462, 1.599625672291281386 ) ) ;
#175376 = CARTESIAN_POINT ( 'NONE',  ( 1.998837940877351116, -2.080155006269391205, -0.4107514010402503746 ) ) ;
#175377 = CARTESIAN_POINT ( 'NONE',  ( -3.226477370372317743, 4.787309570232886280, 1.443375672974064550 ) ) ;
#175378 = CYLINDRICAL_SURFACE ( 'NONE', #128995, 0.3999999999999997446 ) ;
#175379 = CARTESIAN_POINT ( 'NONE',  ( -5.552734181323573992, 6.223089306236814444, -0.9332588772281782408 ) ) ;
#175380 = CARTESIAN_POINT ( 'NONE',  ( 1.077107760077404830, 1.911388382048292645, 0.7958064784282170567 ) ) ;
#175382 = CARTESIAN_POINT ( 'NONE',  ( 1.499999999999993117, 13.38541666734946745, 0.8660254037844409281 ) ) ;
#175381 = CARTESIAN_POINT ( 'NONE',  ( -11.57407876878716557, 2.018041202054113636, 3.760646157730112016 ) ) ;
#175384 = VERTEX_POINT ( 'NONE', #54193 ) ;
#175383 = CARTESIAN_POINT ( 'NONE',  ( 3.194184678167404368, 1.410462778303589015, 1.716012817976236171 ) ) ;
#175385 = CARTESIAN_POINT ( 'NONE',  ( 1.073308018423566823, -1.027821916426611581, 2.056166664744577321 ) ) ;
#175387 = CARTESIAN_POINT ( 'NONE',  ( 6.983263157960404754, -0.005959781318053481922, 2.045923054782183392 ) ) ;
#175386 = CARTESIAN_POINT ( 'NONE',  ( 4.207107738942202246, 3.802713871720993399, 1.214306433183764966E-14 ) ) ;
#175389 = CARTESIAN_POINT ( 'NONE',  ( 1.001543065824772753E-15, -1.312499999999998224, 4.012584370867899430 ) ) ;
#175388 = CARTESIAN_POINT ( 'NONE',  ( 4.366607992053101128, 7.252070536440704096, -1.199719254218448494 ) ) ;
#175390 = LINE ( 'NONE', #78923, #64755 ) ;
#175391 = CARTESIAN_POINT ( 'NONE',  ( 5.864778394761136049, 0.1288883805774850844, -1.836796581567698539 ) ) ;
#175392 = DIRECTION ( 'NONE',  ( 1.000000000000000000, -0.000000000000000000, 1.224646799147353207E-16 ) ) ;
#175393 = CARTESIAN_POINT ( 'NONE',  ( -0.1102773484823937195, 1.994803768489497031, -2.617422746694163749 ) ) ;
#175394 = CARTESIAN_POINT ( 'NONE',  ( 3.100334465813825435, -0.4993057154734497072, -1.650917527159057707 ) ) ;
#175395 = CARTESIAN_POINT ( 'NONE',  ( 1.288296401830712368, -0.7303101666344159471, -1.879802715551846859 ) ) ;
#175396 = CARTESIAN_POINT ( 'NONE',  ( 2.778317543532899947, 1.969881296151472894, -1.184559908770227432 ) ) ;
#175397 = CARTESIAN_POINT ( 'NONE',  ( 1.862946185591638049, -1.600570176636705089, 1.599199478044037059 ) ) ;
#175398 = CARTESIAN_POINT ( 'NONE',  ( 5.408848747418643299, 1.595474064493606514, -1.374861248814135628 ) ) ;
#175399 = CARTESIAN_POINT ( 'NONE',  ( -5.628043163448566588, 9.580151100749725757, 0.000000000000000000 ) ) ;
#175400 = CARTESIAN_POINT ( 'NONE',  ( 3.971743243459349149, 0.9813984145389564873, 1.472460009610305320 ) ) ;
#175401 = AXIS2_PLACEMENT_3D ( 'NONE', #17936, #84022, #185776 ) ;
#175403 = CARTESIAN_POINT ( 'NONE',  ( 0.1118211671861284034, -2.246746504121981403, 0.4537721782011410188 ) ) ;
#175402 = CARTESIAN_POINT ( 'NONE',  ( 4.462041952228939401, 6.299077925724123617, -1.443375672974068769 ) ) ;
#175404 = CARTESIAN_POINT ( 'NONE',  ( 4.716662652015527257, -0.08744826293657045890, 1.839185557975311358 ) ) ;
#175406 = EDGE_CURVE ( 'NONE', #140029, #132973, #125470, .T. ) ;
#175405 = CARTESIAN_POINT ( 'NONE',  ( -4.517891501851816649, 6.293959390292322986, -1.599625672291256295 ) ) ;
#175407 = CARTESIAN_POINT ( 'NONE',  ( 6.127922243252466039, 6.251590159990418449, 1.040834085586084257E-14 ) ) ;
#175408 = CARTESIAN_POINT ( 'NONE',  ( 0.7499999999999902300, 3.983333333333352488, 1.299038105676669330 ) ) ;
#175409 = CARTESIAN_POINT ( 'NONE',  ( 4.822331674454460426, 2.096538211656114647, 0.6379635903819569354 ) ) ;
#175410 = DIRECTION ( 'NONE',  ( 0.7592566023653005702, -0.6507913734559639396, 0.000000000000000000 ) ) ;
#175411 = FACE_OUTER_BOUND ( 'NONE', #159824, .T. ) ;
#175412 = CARTESIAN_POINT ( 'NONE',  ( 4.826661161267837841, -1.354893614093263254, 1.565527137264411728 ) ) ;
#175413 = CARTESIAN_POINT ( 'NONE',  ( 0.2336117360935245635, 0.6279853779636718203, -1.916355031878452797 ) ) ;
#175414 = CARTESIAN_POINT ( 'NONE',  ( 1.364683531249988535, 4.155208333674753618, -0.7879004041258239610 ) ) ;
#175415 = CARTESIAN_POINT ( 'NONE',  ( 3.650929903551769939, -1.574478333125122864, 1.109889904662264115 ) ) ;
#175416 = CARTESIAN_POINT ( 'NONE',  ( 1.364683531249997417, 9.484375000341396245, 2.602085213965210642E-15 ) ) ;
#175417 = CARTESIAN_POINT ( 'NONE',  ( -3.633221978782299910, 5.261844946711204507, -1.443375672974053447 ) ) ;
#175418 = CARTESIAN_POINT ( 'NONE',  ( 0.4225341819744453664, -2.209939313495157265, 0.2258247597332131984 ) ) ;
#175419 = ORIENTED_EDGE ( 'NONE', *, *, #166876, .F. ) ;
#175421 = CARTESIAN_POINT ( 'NONE',  ( 3.947104627881218963, 8.980740528189222971, -0.7749999999999996891 ) ) ;
#175420 = CARTESIAN_POINT ( 'NONE',  ( 1.500000000000001554, 7.809273069926260469, -3.635729725621137831 ) ) ;
#175422 = CARTESIAN_POINT ( 'NONE',  ( 4.704842999142070603, 5.447737239542574272, -1.199719254218452047 ) ) ;
#175423 = DIRECTION ( 'NONE',  ( 0.7592566023652995710, 0.6507913734559652719, 0.000000000000000000 ) ) ;
#175424 = CARTESIAN_POINT ( 'NONE',  ( -1.772826578343124959, 3.950000000000009059, -0.4500000000000423661 ) ) ;
#175425 = CARTESIAN_POINT ( 'NONE',  ( -4.533519451513712717, 7.918419216724965182, -0.7681833670988020835 ) ) ;
#175426 = CARTESIAN_POINT ( 'NONE',  ( 1.521847698614446687, 1.933392594956625521, -0.3320675068423510345 ) ) ;
#175427 = CARTESIAN_POINT ( 'NONE',  ( -1.201851678989727383E-14, 0.8843750003414173610, 1.575800808251672791 ) ) ;
#175428 = CARTESIAN_POINT ( 'NONE',  ( 11.92046840572485777, 12.44747875205727894, 1.382231356234940867 ) ) ;
#175429 = CARTESIAN_POINT ( 'NONE',  ( 5.142999638377217408, -0.2383176028181442918, -1.947251298587366231 ) ) ;
#175430 = CARTESIAN_POINT ( 'NONE',  ( -9.297140650669053485, 11.86975006391249643, 1.599625672291281386 ) ) ;
#175431 = CARTESIAN_POINT ( 'NONE',  ( -5.626270559546828309, 7.587068290936515247, 1.443375672974064550 ) ) ;
#175432 = AXIS2_PLACEMENT_3D ( 'NONE', #7134, #140397, #88420 ) ;
#175433 = CARTESIAN_POINT ( 'NONE',  ( 6.350466702034289312, 0.6732396885240909956, 2.054270918568662729 ) ) ;
#175435 = ORIENTED_EDGE ( 'NONE', *, *, #186987, .F. ) ;
#175434 = CARTESIAN_POINT ( 'NONE',  ( -0.2104748580754391973, 0.7011259924453935310, -2.185273273056092425 ) ) ;
#175436 = CARTESIAN_POINT ( 'NONE',  ( -1.001543065824772872E-14, 4.571875000341418804, 1.575800808251672791 ) ) ;
#175437 = CARTESIAN_POINT ( 'NONE',  ( 6.661403070661808812, 0.3393488462513394310, -1.941789718247180607 ) ) ;
#175438 = CARTESIAN_POINT ( 'NONE',  ( 6.661516750719080449, -0.4673772157907078451, -1.669595843636323185 ) ) ;
#175440 = CARTESIAN_POINT ( 'NONE',  ( 2.700927432832851860, 1.852951201923001223, 1.169960570980829839 ) ) ;
#175439 = CARTESIAN_POINT ( 'NONE',  ( 1.360316468749969809, 1.036458333674743049, -0.7853790794158820310 ) ) ;
#175441 = CARTESIAN_POINT ( 'NONE',  ( 4.348838485402671594, 0.6111939248801941948, 2.225120539556017629 ) ) ;
#175442 = CARTESIAN_POINT ( 'NONE',  ( 5.764934849280819229, -1.861221615537820728, -0.8850300128313455250 ) ) ;
#175443 = CARTESIAN_POINT ( 'NONE',  ( 1.798672962244704410, 1.614485480382701565, 1.078883064099228628 ) ) ;
#175444 = CARTESIAN_POINT ( 'NONE',  ( -5.029711800545518585, 8.811821500704338561, 0.7216878364870458196 ) ) ;
#175445 = EDGE_CURVE ( 'NONE', #88459, #160735, #139142, .T. ) ;
#175446 = CARTESIAN_POINT ( 'NONE',  ( 5.583108480610128765, 5.824348371890765819, -0.7571734975398980438 ) ) ;
#175447 = CARTESIAN_POINT ( 'NONE',  ( 5.414351406770180120, -2.120778210838507150, 0.002142078463891750485 ) ) ;
#175448 = SURFACE_STYLE_USAGE ( .BOTH. , #191659 ) ;
#175449 = CARTESIAN_POINT ( 'NONE',  ( 2.479138880926802901, -2.011204309026824344, -0.1455328587063598189 ) ) ;
#175450 = CARTESIAN_POINT ( 'NONE',  ( -4.568734577680887199, 6.353276312092901890, -1.443375672974051449 ) ) ;
#175451 = CARTESIAN_POINT ( 'NONE',  ( 11.43209210103587914, 12.44403924016084240, -3.649125173352125273 ) ) ;
#175452 = CARTESIAN_POINT ( 'NONE',  ( 8.238550898598388628, 12.76339314834017102, 0.7998128361456462443 ) ) ;
#175453 = DIRECTION ( 'NONE',  ( -1.000000000000000000, 7.387867266669436732E-31, 0.000000000000000000 ) ) ;
#175454 = CARTESIAN_POINT ( 'NONE',  ( -5.315678745009726924, 8.359319748223434487, -1.199719254218453823 ) ) ;
#175456 = CARTESIAN_POINT ( 'NONE',  ( -5.468734858265826837, 7.473552982767156294, 1.599625672291263401 ) ) ;
#175455 = CARTESIAN_POINT ( 'NONE',  ( -4.725015201957559086, 8.329469486225510977, 0.7380969479929339050 ) ) ;
#175457 = CARTESIAN_POINT ( 'NONE',  ( -4.489157070319179432, 8.251450656689856444, 5.811111664500048210E-05 ) ) ;
#175458 = ORIENTED_EDGE ( 'NONE', *, *, #55489, .T. ) ;
#175459 = CARTESIAN_POINT ( 'NONE',  ( 6.121960869219821966, -1.142753529713343763, -1.714830629803126616 ) ) ;
#175460 = LINE ( 'NONE', #97417, #106331 ) ;
#175461 = CARTESIAN_POINT ( 'NONE',  ( -1.500000000000008216, 11.78125000068279427, 3.469446951953614189E-15 ) ) ;
#175462 = CARTESIAN_POINT ( 'NONE',  ( -3.144601563365788444, 5.756120026313656268, -1.199719254218452935 ) ) ;
#175463 = CARTESIAN_POINT ( 'NONE',  ( -2.979759899953417612, 6.698413326579433225, 0.7998128361456352531 ) ) ;
#175464 = CARTESIAN_POINT ( 'NONE',  ( 4.283856624473350472, 1.958454427565621048, -0.4929297443572661641 ) ) ;
#175466 = VERTEX_POINT ( 'NONE', #171136 ) ;
#175465 = CARTESIAN_POINT ( 'NONE',  ( -1.201851678989727383E-14, 0.9625000000000237810, 1.732050807568877637 ) ) ;
#175468 = CARTESIAN_POINT ( 'NONE',  ( 9.571693261567965294, 10.26932301469188857, 0.7216878364870438212 ) ) ;
#175467 = CARTESIAN_POINT ( 'NONE',  ( -5.517242166118370150, 5.401480380085008193, 0.7998128361456281477 ) ) ;
#175469 = CARTESIAN_POINT ( 'NONE',  ( 6.958359152311676787, 9.141171649162195934, -1.599625672291262513 ) ) ;
#175470 = CARTESIAN_POINT ( 'NONE',  ( 3.836836124264888959, 0.3005266716369097701, 2.038723765318616099 ) ) ;
#175471 = CARTESIAN_POINT ( 'NONE',  ( 2.373672848961404735, -0.3474683332905931232, -1.986100487175908258 ) ) ;
#175472 = ORIENTED_EDGE ( 'NONE', *, *, #93956, .F. ) ;
#175473 = CARTESIAN_POINT ( 'NONE',  ( 1.419999999999990603, 6.280000000000042881, 2.873333333333337070 ) ) ;
#175474 = CARTESIAN_POINT ( 'NONE',  ( 3.032219910950674890, 6.689340329417765574, 0.7998128361456321445 ) ) ;
#175475 = CIRCLE ( 'NONE', #12936, 0.08000000000000020983 ) ;
#175477 = ORIENTED_EDGE ( 'NONE', *, *, #160465, .F. ) ;
#175476 = CARTESIAN_POINT ( 'NONE',  ( -0.1495493664682910895, 8.232402834744856790, -1.999498275785964507 ) ) ;
#175478 = CARTESIAN_POINT ( 'NONE',  ( 3.251327214347735861, -1.985796489957316391, -0.3474142817363470304 ) ) ;
#175479 = CARTESIAN_POINT ( 'NONE',  ( 2.413779523973126118, 1.202770565240804279, -1.394052804434331216 ) ) ;
#175480 = CARTESIAN_POINT ( 'NONE',  ( 0.7159568421808035765, -0.3331041906398305441, 2.283425790780469811 ) ) ;
#175481 = CARTESIAN_POINT ( 'NONE',  ( 4.064412189046650248, 7.963840997188264659, 0.7998128361456271485 ) ) ;
#175482 = CARTESIAN_POINT ( 'NONE',  ( 3.216266648612066792, -1.062311135343798618, -1.882447817163131587 ) ) ;
#175483 = CARTESIAN_POINT ( 'NONE',  ( 9.759171643738394408, 10.28012176064996197, 0.000000000000000000 ) ) ;
#175484 = CARTESIAN_POINT ( 'NONE',  ( -5.388475986427523345, 8.373973519885682393, 1.199719254218452047 ) ) ;
#175485 = AXIS2_PLACEMENT_3D ( 'NONE', #19332, #151495, #137384 ) ;
#175486 = EDGE_CURVE ( 'NONE', #107993, #192999, #170363, .T. ) ;
#175487 = CARTESIAN_POINT ( 'NONE',  ( 3.023178501820302344, 2.287506772329782390, -0.2231754551033394429 ) ) ;
#175488 = ORIENTED_EDGE ( 'NONE', *, *, #76548, .F. ) ;
#175489 = FACE_OUTER_BOUND ( 'NONE', #194643, .T. ) ;
#175490 = CARTESIAN_POINT ( 'NONE',  ( 0.7955152940811484052, -0.6771210053572243037, 1.743984199989514927 ) ) ;
#175491 = CARTESIAN_POINT ( 'NONE',  ( 5.524284814141814159, 1.174771371627521876, -1.583071389104006244 ) ) ;
#175493 = CARTESIAN_POINT ( 'NONE',  ( 9.368320956918614328, 10.99242454023565507, 1.082531754730549967 ) ) ;
#175492 = CARTESIAN_POINT ( 'NONE',  ( -1.364683531250010295, 3.780208333674750953, 0.7879004041258379498 ) ) ;
#175495 = CARTESIAN_POINT ( 'NONE',  ( 0.5224629442122545875, -1.184049029929446828, -1.862174541895257995 ) ) ;
#175494 = CARTESIAN_POINT ( 'NONE',  ( -6.358937740009323214, 7.377514437221045718, -1.199719254218446718 ) ) ;
#175496 = CARTESIAN_POINT ( 'NONE',  ( 6.505214776458575265, 6.483838748823460563, 1.040834085586084257E-14 ) ) ;
#175497 = CARTESIAN_POINT ( 'NONE',  ( -3.899941742225307539, 7.701682465904834629, 0.7998128361456341429 ) ) ;
#175498 = CARTESIAN_POINT ( 'NONE',  ( 6.539320575229236709, 1.252639605590207150, 2.218328189723097754 ) ) ;
#175499 = CARTESIAN_POINT ( 'NONE',  ( 5.207875265678946874, -1.962022031532301369, 0.1926216461900862598 ) ) ;
#175500 = CARTESIAN_POINT ( 'NONE',  ( 5.039818274408326637, -1.629004898613298558, -1.634814698366208185 ) ) ;
#175501 = CARTESIAN_POINT ( 'NONE',  ( 2.887610015510627459, -1.926180996541780877, 0.7380674418178012619 ) ) ;
#175502 = CARTESIAN_POINT ( 'NONE',  ( 5.490689023854504747, 9.349628261231513804, 1.040834085586084257E-14 ) ) ;
#175503 = CARTESIAN_POINT ( 'NONE',  ( 5.071631979963703962, 8.074598522336444262, 1.199719254218451159 ) ) ;
#175504 = CARTESIAN_POINT ( 'NONE',  ( 3.223806664999388172, 6.983134552466421674, -0.7998128361456362523 ) ) ;
#175505 = CARTESIAN_POINT ( 'NONE',  ( -0.6823417656250003738, 2.280208333674753174, -1.181850606188749264 ) ) ;
#175506 = CARTESIAN_POINT ( 'NONE',  ( -7.085023742657587498, 14.52988328832284814, 9.695690332251523103 ) ) ;
#175507 = CARTESIAN_POINT ( 'NONE',  ( 6.493992390821439642, 7.639041213122241381, -1.082531754730543971 ) ) ;
#175508 = CARTESIAN_POINT ( 'NONE',  ( 4.844266001044335468, -1.027726779992131023, 1.912555630771580084 ) ) ;
#175510 = CARTESIAN_POINT ( 'NONE',  ( 3.632213977189250098, 0.2737156317273430894, 1.820677940640710979 ) ) ;
#175509 = CARTESIAN_POINT ( 'NONE',  ( -2.819732761962332024, 6.233512622357263666, -0.7216878364870267237 ) ) ;
#175512 = CARTESIAN_POINT ( 'NONE',  ( 11.86239285000045740, 12.21999999999998288, 1.812080536912751283 ) ) ;
#175511 = CARTESIAN_POINT ( 'NONE',  ( -11.87828357749969754, 11.30310252740409283, 1.708055325888841569 ) ) ;
#175513 = CARTESIAN_POINT ( 'NONE',  ( 5.214472588068230330, 2.024700573814151028, 0.8392323156421463981 ) ) ;
#175514 = LINE ( 'NONE', #193870, #143176 ) ;
#175515 = CARTESIAN_POINT ( 'NONE',  ( 6.772354121900423962, -1.399018086243536407, 1.779017302379340748 ) ) ;
#175516 = EDGE_CURVE ( 'NONE', #199311, #11347, #5403, .T. ) ;
#175517 = CARTESIAN_POINT ( 'NONE',  ( -4.301340604499551468, 7.447936736316801642, -1.117465989868490883 ) ) ;
#175518 = PRESENTATION_STYLE_ASSIGNMENT (( #125772 ) ) ;
#175519 = CARTESIAN_POINT ( 'NONE',  ( 5.355371708033295874, 7.701368364266228284, 1.317571137710125351 ) ) ;
#175520 = CARTESIAN_POINT ( 'NONE',  ( -3.296040741453672318, 6.859481608422314025, 0.7216878364870338292 ) ) ;
#175521 = CARTESIAN_POINT ( 'NONE',  ( 3.553645660557675612, 6.199651466408984568, -1.082531754730549967 ) ) ;
#175522 = CARTESIAN_POINT ( 'NONE',  ( 0.4261447845913856614, 1.691672268694037307, 0.5201907349937917591 ) ) ;
#175523 = CARTESIAN_POINT ( 'NONE',  ( 5.760407631487725055, 2.010880845746499279, 0.09660876809274536459 ) ) ;
#175524 = CARTESIAN_POINT ( 'NONE',  ( 5.309989718046547402, 9.346738437696316737, 0.7998128361456462443 ) ) ;
#175525 = CARTESIAN_POINT ( 'NONE',  ( 4.524511627872906061, 1.297711147994727865, -1.658517390945497549 ) ) ;
#175526 = CARTESIAN_POINT ( 'NONE',  ( 2.847180372343278254, 0.2781937080071684720, -1.895151957576347579 ) ) ;
#175527 = CARTESIAN_POINT ( 'NONE',  ( 0.07302493934787820939, 1.405922845961229184, -11.99988463978223407 ) ) ;
#175529 = EDGE_CURVE ( 'NONE', #169262, #57507, #156089, .T. ) ;
#175528 = CARTESIAN_POINT ( 'NONE',  ( 4.369560876907440772, -0.3388413995694672387, 1.940020671193002810 ) ) ;
#175530 = CARTESIAN_POINT ( 'NONE',  ( 5.660417604421997595, 2.017665076342503916, 0.09485465564632548918 ) ) ;
#175531 = CARTESIAN_POINT ( 'NONE',  ( 1.639302681421180852, -1.352760811461351187, -1.292285834730775074 ) ) ;
#175533 = CARTESIAN_POINT ( 'NONE',  ( 1.828231037913151447, -0.9045423626323212396, -1.684975973026317408 ) ) ;
#175532 = CARTESIAN_POINT ( 'NONE',  ( 4.617633504863215776, -1.690751803285206245, 0.3404669814689939011 ) ) ;
#175535 = CARTESIAN_POINT ( 'NONE',  ( 3.036663219780971978, 6.486598156479028709, -0.7216878364870267237 ) ) ;
#175534 = CARTESIAN_POINT ( 'NONE',  ( 2.649284799151204073, -1.834272514977531632, 1.226802785254533568 ) ) ;
#175536 = CARTESIAN_POINT ( 'NONE',  ( 1.364683531249986537, 1.717708333674749399, -0.7879004041258239610 ) ) ;
#175537 = CARTESIAN_POINT ( 'NONE',  ( 6.268018250734934682, -1.947192974725008963, 0.2387856323943157166 ) ) ;
#175538 = CARTESIAN_POINT ( 'NONE',  ( 7.293396569147545527, 10.59638086639245280, 1.199719254218460707 ) ) ;
#175539 = CARTESIAN_POINT ( 'NONE',  ( 11.86239285000045918, 11.37999999999998302, 1.812080536912751283 ) ) ;
#175540 = CARTESIAN_POINT ( 'NONE',  ( 10.25773349932952350, -6.796015482748906322, 1.760695953681369627E-15 ) ) ;
#175541 = CARTESIAN_POINT ( 'NONE',  ( 3.010962844182406783, 6.456614384947361174, 0.07536873999088607168 ) ) ;
#175542 = ORIENTED_EDGE ( 'NONE', *, *, #163282, .F. ) ;
#175543 = CARTESIAN_POINT ( 'NONE',  ( 7.728718841140392648, -6.124285369217659536, 7.728718841140364226 ) ) ;
#175544 = ORIENTED_EDGE ( 'NONE', *, *, #41171, .T. ) ;
#175545 = CARTESIAN_POINT ( 'NONE',  ( 1.908725956546155178, 0.6474277305483535638, 1.966616875269424192 ) ) ;
#175546 = CARTESIAN_POINT ( 'NONE',  ( -1.402160292154681736E-14, 2.587500000000023892, -1.732050807568863648 ) ) ;
#175547 = CARTESIAN_POINT ( 'NONE',  ( 6.205881626753210867, 8.263281202677319470, 1.599625672291281386 ) ) ;
#175548 = CARTESIAN_POINT ( 'NONE',  ( -6.690058733339450114, 9.892486724616283311, 1.199719254218452047 ) ) ;
#175549 = CARTESIAN_POINT ( 'NONE',  ( 5.578253857379852576, 5.472660686556754861, -0.7998128361456481317 ) ) ;
#175550 = CARTESIAN_POINT ( 'NONE',  ( 0.1881566102324930545, 1.164766123054150837, 1.649759867427439186 ) ) ;
#175551 = CYLINDRICAL_SURFACE ( 'NONE', #32200, 0.07999999999999998779 ) ;
#175552 = CARTESIAN_POINT ( 'NONE',  ( -1.364683531250012516, 2.780208333674754506, 0.7879004041258379498 ) ) ;
#175553 = EDGE_CURVE ( 'NONE', #106547, #175025, #83778, .T. ) ;
#175555 = CARTESIAN_POINT ( 'NONE',  ( 2.683624340501134853, 5.218313266304903664, -1.199719254218446718 ) ) ;
#175554 = FACE_OUTER_BOUND ( 'NONE', #50360, .T. ) ;
#175556 = CARTESIAN_POINT ( 'NONE',  ( 5.852888695852590750, -0.9090035733541059759, 1.799648235488074732 ) ) ;
#175557 = CARTESIAN_POINT ( 'NONE',  ( 4.540194369826378029, 0.7389084316076138803, 1.767693002002197034 ) ) ;
#175558 = CARTESIAN_POINT ( 'NONE',  ( 3.052458795248469414, -1.657928338269051505, 1.433322580492613296 ) ) ;
#175559 = CARTESIAN_POINT ( 'NONE',  ( -5.956409969451652131, 6.075908546082715134, -0.6293437877468227581 ) ) ;
#175560 = CARTESIAN_POINT ( 'NONE',  ( 1.499999999999989120, 0.05625000068281565957, 0.000000000000000000 ) ) ;
#175561 = CARTESIAN_POINT ( 'NONE',  ( 5.836195099138038245, -1.121959161234881819, -1.671398195203987136 ) ) ;
#175562 = CARTESIAN_POINT ( 'NONE',  ( 1.810667312839256304, -0.5133170510521027907, -1.842115474350584980 ) ) ;
#175563 = CARTESIAN_POINT ( 'NONE',  ( -6.449928391799210736, 8.548002428564306143, -1.599625672291263179 ) ) ;
#175565 = CARTESIAN_POINT ( 'NONE',  ( 6.468375645409351726, -2.076397406075684682, -0.4129765506453788038 ) ) ;
#175564 = CARTESIAN_POINT ( 'NONE',  ( -2.928197990871687306, 5.399686175116803710, 1.082531754730560403 ) ) ;
#175566 = CARTESIAN_POINT ( 'NONE',  ( 1.364683531249997417, 10.04687500034139802, 2.602085213965210642E-15 ) ) ;
#175568 = CARTESIAN_POINT ( 'NONE',  ( -5.661411662158206681, 8.762674818229999829, -1.199719254218452047 ) ) ;
#175567 = CARTESIAN_POINT ( 'NONE',  ( 3.825792374969799514, 1.116656699807290432, -1.767364921024146218 ) ) ;
#175570 = ORIENTED_EDGE ( 'NONE', *, *, #188595, .T. ) ;
#175569 = CARTESIAN_POINT ( 'NONE',  ( 1.869703332329395895, 0.8828569656042523084, 1.481527559500251501 ) ) ;
#175571 = DIRECTION ( 'NONE',  ( 0.000000000000000000, 0.000000000000000000, -1.000000000000000000 ) ) ;
#175572 = CARTESIAN_POINT ( 'NONE',  ( 6.335737856287750880, 6.286115675290828264, -0.7998128361456281477 ) ) ;
#175573 = CARTESIAN_POINT ( 'NONE',  ( -1.119339255005453736E-13, 13.28612805825129151, 1.454322456996997470 ) ) ;
#175574 = CARTESIAN_POINT ( 'NONE',  ( 0.1683002474503410839, -0.8351952195557797998, -1.773497582445908938 ) ) ;
#175575 = CARTESIAN_POINT ( 'NONE',  ( 7.037870247915987143, -8.199999999999986855, -6.381095703207948944 ) ) ;
#175576 = CARTESIAN_POINT ( 'NONE',  ( 5.738125327081736060, 7.717565519727259904, 1.599625672291267398 ) ) ;
#175577 = CARTESIAN_POINT ( 'NONE',  ( 3.094265954482837255, 2.800000000000017586, 2.490342512183689294 ) ) ;
#175578 = ORIENTED_EDGE ( 'NONE', *, *, #92189, .T. ) ;
#175579 = CARTESIAN_POINT ( 'NONE',  ( 3.369578772036628145, 0.4373610723380080834, -1.757749666579068171 ) ) ;
#175580 = ORIENTED_EDGE ( 'NONE', *, *, #115776, .T. ) ;
#175581 = CARTESIAN_POINT ( 'NONE',  ( 2.530568227245037605, 6.104080031761181857, 0.000000000000000000 ) ) ;
#175582 = VERTEX_POINT ( 'NONE', #85620 ) ;
#175583 = CARTESIAN_POINT ( 'NONE',  ( 5.408776937209000657, 5.274937613024121674, 0.7998128361456352531 ) ) ;
#175584 = CARTESIAN_POINT ( 'NONE',  ( 3.299258901807587741, 1.636513117289538188, -0.7770104639905143218 ) ) ;
#175585 = CARTESIAN_POINT ( 'NONE',  ( 6.639320575229255006, 4.696066290934245657, 2.559399261709224049 ) ) ;
#175586 = CARTESIAN_POINT ( 'NONE',  ( -10.99943592145024240, -8.241816521215563185, 0.1113975309873064257 ) ) ;
#175587 = CARTESIAN_POINT ( 'NONE',  ( 4.009017875521604601, 7.583074288825860876, 0.2480677224083651655 ) ) ;
#175588 = EDGE_LOOP ( 'NONE', ( #67457, #180838, #148539, #121040 ) ) ;
#175589 = CARTESIAN_POINT ( 'NONE',  ( 3.947575701020007877, 1.346737928234511106, 1.284688856454605732 ) ) ;
#175590 = CARTESIAN_POINT ( 'NONE',  ( 1.704550880262687640, 1.788078052428695219, 0.6877594758711459422 ) ) ;
#175591 = CARTESIAN_POINT ( 'NONE',  ( 0.5865807246496178573, -0.2182756592755269454, -1.812417144444453232 ) ) ;
#175592 = CARTESIAN_POINT ( 'NONE',  ( 0.7500000000000006661, 11.58333333333333393, 1.299038105676657340 ) ) ;
#175593 = CARTESIAN_POINT ( 'NONE',  ( -0.5000000000000108802, 3.950000000000001954, -0.5000000000000091038 ) ) ;
#175594 = CIRCLE ( 'NONE', #182503, 0.08000000000000001554 ) ;
#175595 = CARTESIAN_POINT ( 'NONE',  ( 5.590372323399994237, 7.390087136190794936, 1.241407824010079652 ) ) ;
#175596 = CARTESIAN_POINT ( 'NONE',  ( 8.518320732998095224, 14.76619040281040718, 9.398253358897362020 ) ) ;
#175597 = CARTESIAN_POINT ( 'NONE',  ( 3.212919216758630014, 6.692230152952963529, 0.000000000000000000 ) ) ;
#175598 = CARTESIAN_POINT ( 'NONE',  ( 8.785320351975350661, 9.351887953500479966, -0.7216878364870197293 ) ) ;
#175599 = CARTESIAN_POINT ( 'NONE',  ( 5.629738194587773137, 1.899041559284548208, -0.5217042529989719402 ) ) ;
#175600 = EDGE_CURVE ( 'NONE', #65129, #201530, #69344, .T. ) ;
#175601 = CARTESIAN_POINT ( 'NONE',  ( -3.554208825076827782, 7.298327395898266623, 0.7998128361456341429 ) ) ;
#175602 = DIRECTION ( 'NONE',  ( 1.776356839400250465E-14, 0.000000000000000000, -1.000000000000000000 ) ) ;
#175603 = CARTESIAN_POINT ( 'NONE',  ( 6.615165563918417924, -2.126712762998611783, 0.5283135293715838232 ) ) ;
#175604 = CARTESIAN_POINT ( 'NONE',  ( 7.313733799568044702, 10.62010763521636214, 1.199719254218460707 ) ) ;
#175605 = CARTESIAN_POINT ( 'NONE',  ( 5.456054696845579421, 1.924170334762603574, -0.09472988109167354565 ) ) ;
#175606 = CARTESIAN_POINT ( 'NONE',  ( -4.367698041896780126, 8.247398148854895084, 0.7998128361456481317 ) ) ;
#175607 = ADVANCED_FACE ( 'NONE', ( #119253 ), #191064, .T. ) ;
#175608 = CARTESIAN_POINT ( 'NONE',  ( 1.272165501999738435, -1.161393580401563375, 1.408505525491813515 ) ) ;
#175609 = CARTESIAN_POINT ( 'NONE',  ( 2.174722684859807575, -1.356406721008751814, 1.740749382485320629 ) ) ;
#175610 = CARTESIAN_POINT ( 'NONE',  ( 11.86145016429273191, 12.69999999999999929, 1.099999999999996980 ) ) ;
#175611 = CARTESIAN_POINT ( 'NONE',  ( 0.6153073421325053749, 1.564839666810373231, 1.099065937236625157 ) ) ;
#175612 = EDGE_LOOP ( 'NONE', ( #80026, #1474, #90502, #184524 ) ) ;
#175613 = CARTESIAN_POINT ( 'NONE',  ( 0.5902130973520075541, 1.015489506344388282, -1.687439782384107634 ) ) ;
#175614 = CARTESIAN_POINT ( 'NONE',  ( 2.243606950041766357, 1.941679294436208680, 0.04551257769231514122 ) ) ;
#175615 = VERTEX_POINT ( 'NONE', #92052 ) ;
#175616 = CARTESIAN_POINT ( 'NONE',  ( 0.4915642615439493879, 1.928455281639355867, 0.5879340682083398217 ) ) ;
#175618 = CARTESIAN_POINT ( 'NONE',  ( 6.684420909863875160, 1.071953792136259187, -1.520962823361602601 ) ) ;
#175617 = CARTESIAN_POINT ( 'NONE',  ( -5.306037014901836990, 7.283738832175834510, 1.599625672291263179 ) ) ;
#175619 = CARTESIAN_POINT ( 'NONE',  ( 5.143339171537801846, 7.093924681584509173, 1.599625672291269396 ) ) ;
#175620 = CARTESIAN_POINT ( 'NONE',  ( 11.41381675112453742, 19.00000000000000000, 3.704697986577180746 ) ) ;
#175621 = CARTESIAN_POINT ( 'NONE',  ( -7.462104991928524278, -5.166862915010159263, -8.081892667527526442 ) ) ;
#175622 = CARTESIAN_POINT ( 'NONE',  ( -3.730464822054482710, 7.503959392372201442, 1.040834085586084257E-14 ) ) ;
#175623 = CARTESIAN_POINT ( 'NONE',  ( -7.611976899429754084, 7.845337568948314022, 0.7998128361456341429 ) ) ;
#175624 = CARTESIAN_POINT ( 'NONE',  ( 2.314256413632868714, 1.428969747754246233, -1.661726224907192684 ) ) ;
#175625 = CARTESIAN_POINT ( 'NONE',  ( 2.901081683644319842, 5.368050483351580304, 1.082531754730548412 ) ) ;
#175626 = CARTESIAN_POINT ( 'NONE',  ( 6.851666526859736983, 9.086973262793417661, -1.599625672291269396 ) ) ;
#175627 = FACE_BOUND ( 'NONE', #140445, .T. ) ;
#175628 = CARTESIAN_POINT ( 'NONE',  ( 2.367563199519676420, 1.790531440309536926, -0.3556685536310541518 ) ) ;
#175629 = CARTESIAN_POINT ( 'NONE',  ( 3.945059511452237100, 6.586024615794168646, -1.082531754730548412 ) ) ;
#175630 = CARTESIAN_POINT ( 'NONE',  ( -3.307299406729781399, 5.945934176904983381, -1.199719254218452935 ) ) ;
#175631 = B_SPLINE_CURVE_WITH_KNOTS ( 'NONE', 3,
 ( #35367, #137165, #132912, #198917, #19112, #85191, #67841, #54835 ),
 .UNSPECIFIED., .F., .F.,
 ( 4, 2, 2, 4 ),
 ( 0.000000000000000000, 0.001552951981419670689, 0.003105903962839341378, 0.006211807925678680155 ),
 .UNSPECIFIED. ) ;
#175632 = CARTESIAN_POINT ( 'NONE',  ( -5.847422642759834588, 7.296647196851402839, -1.286413008881746256 ) ) ;
#175633 = DIRECTION ( 'NONE',  ( -3.330669073875479975E-16, 2.334947598634344260E-16, 1.000000000000000000 ) ) ;
#175634 = CARTESIAN_POINT ( 'NONE',  ( 9.378489572351044856, 11.96465713920816043, -1.599625672291262513 ) ) ;
#175635 = CARTESIAN_POINT ( 'NONE',  ( 0.9086680563264810662, 1.459560178543020559, -1.257504221390127519 ) ) ;
#175636 = CARTESIAN_POINT ( 'NONE',  ( 5.190269257085567745, 1.011813749630154691, -1.680575076195559792 ) ) ;
#175637 = CIRCLE ( 'NONE', #57958, 0.04999999999999883010 ) ;
#175638 = CARTESIAN_POINT ( 'NONE',  ( -1.500000000000015099, 15.22916666666666607, -0.8660254037844309360 ) ) ;
#175639 = CARTESIAN_POINT ( 'NONE',  ( -6.177711549321182716, 10.35908057418338402, 0.7998128361456481317 ) ) ;
#175640 = CARTESIAN_POINT ( 'NONE',  ( 4.150767584078112193, 7.994312614733129152, 0.7998128361456321445 ) ) ;
#175641 = CARTESIAN_POINT ( 'NONE',  ( 5.337503337980974649, 0.8888059580158399475, -2.003405333693850654 ) ) ;
#175642 = CARTESIAN_POINT ( 'NONE',  ( 3.174580523894165562, 6.855427711185177131, 0.7998128361456341429 ) ) ;
#175643 = CARTESIAN_POINT ( 'NONE',  ( 3.995033623311712301, 0.2988084191791628985, 2.048438004591215389 ) ) ;
#175644 = CARTESIAN_POINT ( 'NONE',  ( -1.364683531250014514, 1.301041667008083325, -0.7879004041258289570 ) ) ;
#175645 = ORIENTED_EDGE ( 'NONE', *, *, #81658, .F. ) ;
#175646 = CARTESIAN_POINT ( 'NONE',  ( 3.762538640753902097, 2.164199696370266324, -0.7750164773838670307 ) ) ;
#175647 = CARTESIAN_POINT ( 'NONE',  ( 6.588899466561449536, 9.670504563421618016, -1.082531754730537088 ) ) ;
#175649 = SPHERICAL_SURFACE ( 'NONE', #177617, 0.05000000000000000278 ) ;
#175648 = CARTESIAN_POINT ( 'NONE',  ( 6.400857919427532572, 6.640291458853147866, -0.7216878364870458196 ) ) ;
#175650 = CARTESIAN_POINT ( 'NONE',  ( 6.620655732516623537, 7.629137130509068498, 2.426260288887295058 ) ) ;
#175651 = CARTESIAN_POINT ( 'NONE',  ( -5.887983850084758330, 10.09134126839936840, 0.7998128361456291469 ) ) ;
#175652 = CARTESIAN_POINT ( 'NONE',  ( 4.997963218837587540, -0.6557800786283998207, -1.827999027568379509 ) ) ;
#175653 = EDGE_LOOP ( 'NONE', ( #81862, #165777, #211468, #149875 ) ) ;
#175654 = CARTESIAN_POINT ( 'NONE',  ( 8.392133896734655707, 11.77427806529038357, 1.082531754730546636 ) ) ;
#175655 = EDGE_LOOP ( 'NONE', ( #142314, #200459, #75137, #211594, #112837 ) ) ;
#175656 = CARTESIAN_POINT ( 'NONE',  ( 5.537344615273096515, -0.04053095765194079242, 1.912125305397804009 ) ) ;
#175657 = CARTESIAN_POINT ( 'NONE',  ( 6.633849695589691287, -1.131556152058693865, -1.301821263952767316 ) ) ;
#175658 = CARTESIAN_POINT ( 'NONE',  ( 4.065638850954083061, 1.320825628876612257, 1.523796413913918624 ) ) ;
#175660 = CARTESIAN_POINT ( 'NONE',  ( -4.340018570150322219, 5.196348098997705556, -1.082531754730551743 ) ) ;
#175659 = CARTESIAN_POINT ( 'NONE',  ( -9.073431116043565225, 11.60875560684942265, -1.599625672291263179 ) ) ;
#175661 = CARTESIAN_POINT ( 'NONE',  ( 1.642778471875000035, -3.113541666188709200, -2.845375778867859751 ) ) ;
#175663 = CARTESIAN_POINT ( 'NONE',  ( 0.4964904254905980197, 1.474999729349553590, -0.9777959528048956184 ) ) ;
#175662 = CARTESIAN_POINT ( 'NONE',  ( 1.201248573238463235, -0.5064915201186767080, 2.028225233004859351 ) ) ;
#175664 = CARTESIAN_POINT ( 'NONE',  ( 5.959611329766300258, -1.915599147091971544, -0.6298778581111733610 ) ) ;
#175666 = CARTESIAN_POINT ( 'NONE',  ( 2.519810532312277473, -1.321113963755312870, -1.873090484924363697 ) ) ;
#175665 = CARTESIAN_POINT ( 'NONE',  ( 4.061549535745618833, 6.896169004081968090, -1.199719254218452047 ) ) ;
#175667 = CARTESIAN_POINT ( 'NONE',  ( 1.657743431332364681, -1.232332549506355290, 1.229129442381997395 ) ) ;
#175668 = CARTESIAN_POINT ( 'NONE',  ( 6.559000000000036579, 7.629137130509070275, 2.600000000000001421 ) ) ;
#175669 = CARTESIAN_POINT ( 'NONE',  ( 0.5965333524920403141, 0.8982759108043871787, -1.482850294500896560 ) ) ;
#175670 = CARTESIAN_POINT ( 'NONE',  ( 1.360316468749987573, 1.817708333674738608, -0.7853790794158981292 ) ) ;
#175671 = CARTESIAN_POINT ( 'NONE',  ( 1.416206177014844192, 0.7498276349873562729, 1.703500622989342572 ) ) ;
#175672 = CARTESIAN_POINT ( 'NONE',  ( 2.699877945841188343, -1.607453219145397849, -1.459642119406568739 ) ) ;
#175673 = CARTESIAN_POINT ( 'NONE',  ( 3.925017756809038527, -1.752140073516525565, 0.9981236898717813499 ) ) ;
#175674 = CARTESIAN_POINT ( 'NONE',  ( 4.218750000000001776, -0.7852924748297752666, 1.895863743164170057 ) ) ;
#175675 = CARTESIAN_POINT ( 'NONE',  ( -1.500000000000013101, 1.910416667349488451, -0.8660254037844313801 ) ) ;
#175676 = CARTESIAN_POINT ( 'NONE',  ( 6.340456170274588743, 1.905924810476855580, 0.2800546826549690782 ) ) ;
#175677 = CARTESIAN_POINT ( 'NONE',  ( 1.364683531250000303, 14.00520833367473195, -0.7879004041258355073 ) ) ;
#175678 = CARTESIAN_POINT ( 'NONE',  ( 3.217226816143878398, 1.749018536054181672, -1.369387470038183396 ) ) ;
#175679 = VERTEX_POINT ( 'NONE', #43297 ) ;
#175680 = CARTESIAN_POINT ( 'NONE',  ( 1.224999999999963007, 2.458333334016087335, -0.7072540797572877125 ) ) ;
#175681 = CARTESIAN_POINT ( 'NONE',  ( -1.402160292154681736E-14, -0.7874999999999764411, 1.732050807568877637 ) ) ;
#175682 = CARTESIAN_POINT ( 'NONE',  ( 7.540305987494599016, 11.94877408538573427, -0.7998128361456291469 ) ) ;
#175683 = CARTESIAN_POINT ( 'NONE',  ( -1.402160292154681736E-14, 0.07187500034142156602, 1.575800808251672791 ) ) ;
#175684 = CARTESIAN_POINT ( 'NONE',  ( -0.07508257667859614959, -0.9546805890920804227, -2.003339222774684458 ) ) ;
#175685 = CARTESIAN_POINT ( 'NONE',  ( 4.387127823891323608, 0.09410986116351567621, 1.959716250186482434 ) ) ;
#175687 = CARTESIAN_POINT ( 'NONE',  ( -5.083944415444539899, 8.875092884753202682, 0.000000000000000000 ) ) ;
#175686 = CARTESIAN_POINT ( 'NONE',  ( 2.171277156482887882, 5.684907115872006145, -0.7998128361456291469 ) ) ;
#175688 = CARTESIAN_POINT ( 'NONE',  ( -4.260029445439560192, 7.236136616047151193, 2.499999999999999556 ) ) ;
#175689 = CARTESIAN_POINT ( 'NONE',  ( 6.134080777514242300, 1.123080384508338136, -1.963935940973794869 ) ) ;
#175690 = CARTESIAN_POINT ( 'NONE',  ( 2.400897505987206415, 0.4495084874868838232, 2.012960725780033489 ) ) ;
#175691 = CARTESIAN_POINT ( 'NONE',  ( -7.040761844198392794, 7.108643661186573759, -0.7998128361456291469 ) ) ;
#175692 =( BOUNDED_SURFACE ( )  B_SPLINE_SURFACE ( 1, 2, ( 
 ( #56622, #122787, #188746, #156268, #73937, #140031, #57691, #41461, #91278, #157337, #11846, #68040, #149329, #83244, #114760, #99518, #166648, #50757, #180757, #133115, #64870, #116886, #199112, #182885, #97401, #80055, #200187, #163456, #30253, #15036, #134179, #13970, #96337, #63807, #51840, #34502, #117959, #214275, #181809, #165576, #129967, #17170, #115821, #908, #146157, #213240, #65908, #212173, #162393, #81128, #31324, #100575, #195954, #47589, #48642, #18239, #66976, #84323, #150409, #1977, #113703, #16099, #164514, #179707, #147214, #131015, #82183, #32384, #197007, #98450, #132054, #148276, #198064, #49693, #33441, #89687, #119026, #72322, #85391, #202317, #139502, #183953, #152528, #6253, #73399, #53966, #120102, #22502, #153605, #138428, #151475, #35563, #136294, #7321, #88613, #154667, #186081, #38782, #105965, #204447, #37715, #56101, #4113, #122258, #188216, #39856, #36633, #19313, #205530, #102717, #101644, #168775, #57166, #167710, #3046, #69115, #135237, #171987, #201251, #5176, #121184, #104863, #52891, #170907, #55035, #23579, #185008, #70183, #71251, #20379, #86464, #103790, #169841, #155736, #21428, #87537, #137365, #187153, #203382, #92890, #93958, #156813, #74485, #110251, #58231, #140591, #206602, #190346, #43077, #11600, #45203, #142718, #207671, #158935, #124388, #109191, #143794, #193560, #8400, #208727, #127594, #111317, #40933, #42008, #108116, #159999, #177321, #125449, #59290, #174143, #176260, #107038, #12660, #78733, #28935, #95019, #25717, #26785, #60353, #77674, #91826, #126516, #157885, #9477, #75550, #141660, #24644, #191410, #175203, #210865, #10531, #76604, #144858, #192478, #44130, #209791, #161069, #189292, #27861, #61427, #123329, #173064, #90753, #198861, #100319, #132856, #179456, #115565, #646, #62491, #130766, #17977, #15852, #196761, #81938, #98212, #212989, #47338, #84064, #129719, #195703, #13731, #180511, #163209, #182624, #146972, #145916, #165320, #150153, #113452, #66711, #164263, #181561, #50508, #211928, #48403, #63562, #148022, #214032, #64627, #128655 ),
 ( #16914, #166385, #194621, #80882, #116630, #33189, #34248, #49446, #46264, #112381, #114515, #32131, #178393, #30005, #96088, #65657, #131804, #162143, #99272, #197813, #82994, #149069, #79804, #31080, #97154, #14791, #104600, #117707, #20116, #171714, #1723, #184746, #38522, #105687, #86201, #152274, #54769, #185815, #170646, #183698, #67780, #168517, #39584, #120917, #186890, #3846, #70987, #138169, #22232, #69920, #88344, #36373, #154408, #5987, #72058, #68858, #51582, #23313, #134978, #89422, #102450, #2787, #204178, #55834, #133930, #37447, #151218, #103524, #121990, #119836, #187956, #199935, #35305, #118761, #101382, #167457, #19051, #136030, #85131, #169583, #202043, #21166, #87270, #53704, #200987, #52633, #153337, #4910, #137100, #203127, #41747, #61171, #25460, #24374, #43880, #28677, #74229, #159739, #42819, #60100, #143533, #90487, #141404, #156551, #108924, #174946, #91567, #177061, #157620, #27598, #26528, #106775, #11337, #139231, #209529, #126258, #158677, #56903, #9217, #92636, #75289, #59031, #172803, #10275, #77418, #76350, #8146, #7056, #127332, #207412, #176006, #125189, #173884, #191151, #123077, #93698, #155471, #107858, #142457, #193301, #190093, #208465, #205262, #109994, #192217, #44946, #73129, #111054, #189034, #40672, #140323, #206341, #57968, #124132, #66462, #48151, #146720, #79553, #96902, #113195, #132603, #12402, #64373, #46011, #16660, #194368, #160811, #62242, #114265, #49199, #47077, #13477, #78483, #65406, #80628, #145671, #31885, #211668, #63304, #195448, #129465, #210615, #95833, #162953, #182363, #179200, #30825, #82745, #198609, #165068, #14531, #147767, #32937, #94764, #212737, #50255, #180261, #130519, #97962, #196509, #164020, #15594, #116375, #161890, #81681, #112131, #213783, #131553, #390, #197555, #178134, #115320, #144600, #181310, #99011, #148818, #128401, #29749, #117449, #19867, #183443, #135779, #53444, #184498, #55584, #36117, #120663, #201802, #199678, #38267, #17716, #88087, #153084, #37196, #149897, #102200, #119582, #168267, #152027, #51321, #185566 ) ),
 .UNSPECIFIED., .F., .F., .T. ) 
 B_SPLINE_SURFACE_WITH_KNOTS ( ( 2, 2 ),
 ( 3, 2, 2, 2, 2, 2, 2, 2, 2, 2, 2, 2, 2, 2, 2, 2, 2, 2, 2, 2, 2, 2, 2, 2, 2, 2, 2, 2, 2, 2, 2, 2, 2, 2, 2, 2, 2, 2, 2, 2, 2, 2, 2, 2, 2, 2, 2, 2, 2, 2, 2, 2, 2, 2, 2, 2, 2, 2, 2, 2, 2, 2, 2, 2, 2, 2, 2, 2, 2, 2, 2, 2, 2, 2, 2, 2, 2, 2, 2, 2, 2, 2, 2, 2, 2, 2, 2, 2, 2, 2, 2, 2, 2, 2, 2, 2, 2, 2, 2, 2, 2, 2, 2, 2, 2, 2, 2, 2, 2, 2, 2, 2, 2, 2, 2, 2, 2, 2, 2, 2, 3 ),
 ( 0.000000000000000000, 1.000000000000000000 ),
 ( 0.000000000000000000, 0.008333333333333333218, 0.01666666666666666644, 0.02500000000000000139, 0.03333333333333333287, 0.04166666666666666435, 0.05000000000000000278, 0.05833333333333333426, 0.06666666666666666574, 0.07499999999999999722, 0.08333333333333332871, 0.09166666666666666019, 0.1000000000000000056, 0.1083333333333333370, 0.1166666666666666685, 0.1250000000000000000, 0.1333333333333333315, 0.1416666666666666630, 0.1499999999999999944, 0.1583333333333333259, 0.1666666666666666574, 0.1749999999999999889, 0.1833333333333333204, 0.1916666666666666796, 0.2000000000000000111, 0.2083333333333333426, 0.2166666666666666741, 0.2250000000000000056, 0.2333333333333333370, 0.2416666666666666685, 0.2500000000000000000, 0.2583333333333333592, 0.2666666666666666630, 0.2750000000000000222, 0.2833333333333333259, 0.2916666666666666852, 0.2999999999999999889, 0.3083333333333333481, 0.3166666666666666519, 0.3250000000000000111, 0.3333333333333333148, 0.3416666666666666741, 0.3499999999999999778, 0.3583333333333333370, 0.3666666666666666408, 0.3750000000000000000, 0.3833333333333333592, 0.3916666666666666630, 0.4000000000000000222, 0.4083333333333333259, 0.4166666666666666852, 0.4249999999999999889, 0.4333333333333333481, 0.4416666666666666519, 0.4500000000000000111, 0.4583333333333333148, 0.4666666666666666741, 0.4749999999999999778, 0.4833333333333333370, 0.4916666666666666408, 0.5000000000000000000, 0.5083333333333333037, 0.5166666666666667185, 0.5250000000000000222, 0.5333333333333333259, 0.5416666666666666297, 0.5500000000000000444, 0.5583333333333333481, 0.5666666666666666519, 0.5749999999999999556, 0.5833333333333333703, 0.5916666666666666741, 0.5999999999999999778, 0.6083333333333332815, 0.6166666666666666963, 0.6250000000000000000, 0.6333333333333333037, 0.6416666666666667185, 0.6500000000000000222, 0.6583333333333333259, 0.6666666666666666297, 0.6750000000000000444, 0.6833333333333333481, 0.6916666666666666519, 0.6999999999999999556, 0.7083333333333333703, 0.7166666666666666741, 0.7249999999999999778, 0.7333333333333332815, 0.7416666666666666963, 0.7500000000000000000, 0.7583333333333333037, 0.7666666666666667185, 0.7750000000000000222, 0.7833333333333333259, 0.7916666666666666297, 0.8000000000000000444, 0.8083333333333333481, 0.8166666666666666519, 0.8249999999999999556, 0.8333333333333333703, 0.8416666666666666741, 0.8499999999999999778, 0.8583333333333332815, 0.8666666666666666963, 0.8750000000000000000, 0.8833333333333333037, 0.8916666666666667185, 0.9000000000000000222, 0.9083333333333333259, 0.9166666666666666297, 0.9250000000000000444, 0.9333333333333333481, 0.9416666666666666519, 0.9499999999999999556, 0.9583333333333333703, 0.9666666666666666741, 0.9749999999999999778, 0.9833333333333332815, 0.9916666666666666963, 1.000000000000000000 ),
 .UNSPECIFIED. ) 
 GEOMETRIC_REPRESENTATION_ITEM ( )  RATIONAL_B_SPLINE_SURFACE ( (
 ( 1.000000000000000000, 0.8660254037844387076, 1.000000000000000000, 0.8660254037844387076, 1.000000000000000000, 0.8660254037844387076, 1.000000000000000000, 0.8660254037844387076, 1.000000000000000000, 0.8660254037844387076, 1.000000000000000000, 0.8660254037844387076, 1.000000000000000000, 0.8660254037844387076, 1.000000000000000000, 0.8660254037844387076, 1.000000000000000000, 0.8660254037844387076, 1.000000000000000000, 0.8660254037844387076, 1.000000000000000000, 0.8660254037844387076, 1.000000000000000000, 0.8660254037844387076, 1.000000000000000000, 0.8660254037844387076, 1.000000000000000000, 0.8660254037844387076, 1.000000000000000000, 0.8660254037844387076, 1.000000000000000000, 0.8660254037844387076, 1.000000000000000000, 0.8660254037844387076, 1.000000000000000000, 0.8660254037844387076, 1.000000000000000000, 0.8660254037844387076, 1.000000000000000000, 0.8660254037844387076, 1.000000000000000000, 0.8660254037844387076, 1.000000000000000000, 0.8660254037844387076, 1.000000000000000000, 0.8660254037844387076, 1.000000000000000000, 0.8660254037844387076, 1.000000000000000000, 0.8660254037844387076, 1.000000000000000000, 0.8660254037844387076, 1.000000000000000000, 0.8660254037844387076, 1.000000000000000000, 0.8660254037844387076, 1.000000000000000000, 0.8660254037844387076, 1.000000000000000000, 0.8660254037844387076, 1.000000000000000000, 0.8660254037844387076, 1.000000000000000000, 0.8660254037844387076, 1.000000000000000000, 0.8660254037844387076, 1.000000000000000000, 0.8660254037844387076, 1.000000000000000000, 0.8660254037844387076, 1.000000000000000000, 0.8660254037844387076, 1.000000000000000000, 0.8660254037844387076, 1.000000000000000000, 0.8660254037844387076, 1.000000000000000000, 0.8660254037844387076, 1.000000000000000000, 0.8660254037844387076, 1.000000000000000000, 0.8660254037844387076, 1.000000000000000000, 0.8660254037844387076, 1.000000000000000000, 0.8660254037844387076, 1.000000000000000000, 0.8660254037844387076, 1.000000000000000000, 0.8660254037844387076, 1.000000000000000000, 0.8660254037844387076, 1.000000000000000000, 0.8660254037844387076, 1.000000000000000000, 0.8660254037844387076, 1.000000000000000000, 0.8660254037844387076, 1.000000000000000000, 0.8660254037844387076, 1.000000000000000000, 0.8660254037844387076, 1.000000000000000000, 0.8660254037844387076, 1.000000000000000000, 0.8660254037844387076, 1.000000000000000000, 0.8660254037844387076, 1.000000000000000000, 0.8660254037844387076, 1.000000000000000000, 0.8660254037844387076, 1.000000000000000000, 0.8660254037844387076, 1.000000000000000000, 0.8660254037844387076, 1.000000000000000000, 0.8660254037844387076, 1.000000000000000000, 0.8660254037844387076, 1.000000000000000000, 0.8660254037844387076, 1.000000000000000000, 0.8660254037844387076, 1.000000000000000000, 0.8660254037844387076, 1.000000000000000000, 0.8660254037844387076, 1.000000000000000000, 0.8660254037844387076, 1.000000000000000000, 0.8660254037844387076, 1.000000000000000000, 0.8660254037844387076, 1.000000000000000000, 0.8660254037844387076, 1.000000000000000000, 0.8660254037844387076, 1.000000000000000000, 0.8660254037844387076, 1.000000000000000000, 0.8660254037844387076, 1.000000000000000000, 0.8660254037844387076, 1.000000000000000000, 0.8660254037844387076, 1.000000000000000000, 0.8660254037844387076, 1.000000000000000000, 0.8660254037844387076, 1.000000000000000000, 0.8660254037844387076, 1.000000000000000000, 0.8660254037844387076, 1.000000000000000000, 0.8660254037844387076, 1.000000000000000000, 0.8660254037844387076, 1.000000000000000000, 0.8660254037844387076, 1.000000000000000000, 0.8660254037844387076, 1.000000000000000000, 0.8660254037844387076, 1.000000000000000000, 0.8660254037844387076, 1.000000000000000000, 0.8660254037844387076, 1.000000000000000000, 0.8660254037844387076, 1.000000000000000000, 0.8660254037844387076, 1.000000000000000000, 0.8660254037844387076, 1.000000000000000000, 0.8660254037844387076, 1.000000000000000000, 0.8660254037844387076, 1.000000000000000000, 0.8660254037844387076, 1.000000000000000000, 0.8660254037844387076, 1.000000000000000000, 0.8660254037844387076, 1.000000000000000000, 0.8660254037844387076, 1.000000000000000000, 0.8660254037844387076, 1.000000000000000000, 0.8660254037844387076, 1.000000000000000000, 0.8660254037844387076, 1.000000000000000000, 0.8660254037844387076, 1.000000000000000000, 0.8660254037844387076, 1.000000000000000000, 0.8660254037844387076, 1.000000000000000000, 0.8660254037844387076, 1.000000000000000000, 0.8660254037844387076, 1.000000000000000000, 0.8660254037844387076, 1.000000000000000000, 0.8660254037844387076, 1.000000000000000000, 0.8660254037844387076, 1.000000000000000000, 0.8660254037844387076, 1.000000000000000000, 0.8660254037844387076, 1.000000000000000000, 0.8660254037844387076, 1.000000000000000000, 0.8660254037844387076, 1.000000000000000000, 0.8660254037844387076, 1.000000000000000000, 0.8660254037844387076, 1.000000000000000000, 0.8660254037844387076, 1.000000000000000000, 0.8660254037844387076, 1.000000000000000000, 0.8660254037844387076, 1.000000000000000000, 0.8660254037844387076, 1.000000000000000000, 0.8660254037844387076, 1.000000000000000000, 0.8660254037844387076, 1.000000000000000000, 0.8660254037844387076, 1.000000000000000000, 0.8660254037844387076, 1.000000000000000000, 0.8660254037844387076, 1.000000000000000000, 0.8660254037844387076, 1.000000000000000000),
 ( 1.000000000000000000, 0.8660254037844387076, 1.000000000000000000, 0.8660254037844387076, 1.000000000000000000, 0.8660254037844387076, 1.000000000000000000, 0.8660254037844387076, 1.000000000000000000, 0.8660254037844387076, 1.000000000000000000, 0.8660254037844387076, 1.000000000000000000, 0.8660254037844387076, 1.000000000000000000, 0.8660254037844387076, 1.000000000000000000, 0.8660254037844387076, 1.000000000000000000, 0.8660254037844387076, 1.000000000000000000, 0.8660254037844387076, 1.000000000000000000, 0.8660254037844387076, 1.000000000000000000, 0.8660254037844387076, 1.000000000000000000, 0.8660254037844387076, 1.000000000000000000, 0.8660254037844387076, 1.000000000000000000, 0.8660254037844387076, 1.000000000000000000, 0.8660254037844387076, 1.000000000000000000, 0.8660254037844387076, 1.000000000000000000, 0.8660254037844387076, 1.000000000000000000, 0.8660254037844387076, 1.000000000000000000, 0.8660254037844387076, 1.000000000000000000, 0.8660254037844387076, 1.000000000000000000, 0.8660254037844387076, 1.000000000000000000, 0.8660254037844387076, 1.000000000000000000, 0.8660254037844387076, 1.000000000000000000, 0.8660254037844387076, 1.000000000000000000, 0.8660254037844387076, 1.000000000000000000, 0.8660254037844387076, 1.000000000000000000, 0.8660254037844387076, 1.000000000000000000, 0.8660254037844387076, 1.000000000000000000, 0.8660254037844387076, 1.000000000000000000, 0.8660254037844387076, 1.000000000000000000, 0.8660254037844387076, 1.000000000000000000, 0.8660254037844387076, 1.000000000000000000, 0.8660254037844387076, 1.000000000000000000, 0.8660254037844387076, 1.000000000000000000, 0.8660254037844387076, 1.000000000000000000, 0.8660254037844387076, 1.000000000000000000, 0.8660254037844387076, 1.000000000000000000, 0.8660254037844387076, 1.000000000000000000, 0.8660254037844387076, 1.000000000000000000, 0.8660254037844387076, 1.000000000000000000, 0.8660254037844387076, 1.000000000000000000, 0.8660254037844387076, 1.000000000000000000, 0.8660254037844387076, 1.000000000000000000, 0.8660254037844387076, 1.000000000000000000, 0.8660254037844387076, 1.000000000000000000, 0.8660254037844387076, 1.000000000000000000, 0.8660254037844387076, 1.000000000000000000, 0.8660254037844387076, 1.000000000000000000, 0.8660254037844387076, 1.000000000000000000, 0.8660254037844387076, 1.000000000000000000, 0.8660254037844387076, 1.000000000000000000, 0.8660254037844387076, 1.000000000000000000, 0.8660254037844387076, 1.000000000000000000, 0.8660254037844387076, 1.000000000000000000, 0.8660254037844387076, 1.000000000000000000, 0.8660254037844387076, 1.000000000000000000, 0.8660254037844387076, 1.000000000000000000, 0.8660254037844387076, 1.000000000000000000, 0.8660254037844387076, 1.000000000000000000, 0.8660254037844387076, 1.000000000000000000, 0.8660254037844387076, 1.000000000000000000, 0.8660254037844387076, 1.000000000000000000, 0.8660254037844387076, 1.000000000000000000, 0.8660254037844387076, 1.000000000000000000, 0.8660254037844387076, 1.000000000000000000, 0.8660254037844387076, 1.000000000000000000, 0.8660254037844387076, 1.000000000000000000, 0.8660254037844387076, 1.000000000000000000, 0.8660254037844387076, 1.000000000000000000, 0.8660254037844387076, 1.000000000000000000, 0.8660254037844387076, 1.000000000000000000, 0.8660254037844387076, 1.000000000000000000, 0.8660254037844387076, 1.000000000000000000, 0.8660254037844387076, 1.000000000000000000, 0.8660254037844387076, 1.000000000000000000, 0.8660254037844387076, 1.000000000000000000, 0.8660254037844387076, 1.000000000000000000, 0.8660254037844387076, 1.000000000000000000, 0.8660254037844387076, 1.000000000000000000, 0.8660254037844387076, 1.000000000000000000, 0.8660254037844387076, 1.000000000000000000, 0.8660254037844387076, 1.000000000000000000, 0.8660254037844387076, 1.000000000000000000, 0.8660254037844387076, 1.000000000000000000, 0.8660254037844387076, 1.000000000000000000, 0.8660254037844387076, 1.000000000000000000, 0.8660254037844387076, 1.000000000000000000, 0.8660254037844387076, 1.000000000000000000, 0.8660254037844387076, 1.000000000000000000, 0.8660254037844387076, 1.000000000000000000, 0.8660254037844387076, 1.000000000000000000, 0.8660254037844387076, 1.000000000000000000, 0.8660254037844387076, 1.000000000000000000, 0.8660254037844387076, 1.000000000000000000, 0.8660254037844387076, 1.000000000000000000, 0.8660254037844387076, 1.000000000000000000, 0.8660254037844387076, 1.000000000000000000, 0.8660254037844387076, 1.000000000000000000, 0.8660254037844387076, 1.000000000000000000, 0.8660254037844387076, 1.000000000000000000, 0.8660254037844387076, 1.000000000000000000, 0.8660254037844387076, 1.000000000000000000, 0.8660254037844387076, 1.000000000000000000, 0.8660254037844387076, 1.000000000000000000, 0.8660254037844387076, 1.000000000000000000, 0.8660254037844387076, 1.000000000000000000, 0.8660254037844387076, 1.000000000000000000, 0.8660254037844387076, 1.000000000000000000, 0.8660254037844387076, 1.000000000000000000, 0.8660254037844387076, 1.000000000000000000, 0.8660254037844387076, 1.000000000000000000, 0.8660254037844387076, 1.000000000000000000, 0.8660254037844387076, 1.000000000000000000, 0.8660254037844387076, 1.000000000000000000, 0.8660254037844387076, 1.000000000000000000, 0.8660254037844387076, 1.000000000000000000, 0.8660254037844387076, 1.000000000000000000, 0.8660254037844387076, 1.000000000000000000) ) ) 
 REPRESENTATION_ITEM ( '' )  SURFACE ( )  );
#175693 = VERTEX_POINT ( 'NONE', #44355 ) ;
#175694 = CARTESIAN_POINT ( 'NONE',  ( -0.7500000000000006661, 2.639583334016156080, -1.299038105676652011 ) ) ;
#175695 = CARTESIAN_POINT ( 'NONE',  ( 3.514787476322968285, 1.689724804184733253, 0.8026845837263293371 ) ) ;
#175696 = CARTESIAN_POINT ( 'NONE',  ( 2.197566421822871874, 1.549772363009613407, 0.7782106121714903457 ) ) ;
#175697 = CARTESIAN_POINT ( 'NONE',  ( 6.392125918040960642, -0.5824770489515176397, -2.112646119873210271 ) ) ;
#175698 = CARTESIAN_POINT ( 'NONE',  ( 1.026743138268666922, 1.313310656681260680, -1.773271738842125300 ) ) ;
#175699 = CARTESIAN_POINT ( 'NONE',  ( 4.047864428982482110, 0.7307185629543844207, -2.034579650689218866 ) ) ;
#175700 = CARTESIAN_POINT ( 'NONE',  ( 5.718683143142158087, -0.04558518807709806275, 1.941574535162658544 ) ) ;
#175701 = CARTESIAN_POINT ( 'NONE',  ( 7.217521757037772545, 15.46950125388860364, 9.593379878448720532 ) ) ;
#175702 = SURFACE_STYLE_FILL_AREA ( #210305 ) ;
#175703 = CARTESIAN_POINT ( 'NONE',  ( -2.550000000000001155, 2.499999999999998668, -1.849324200890690717 ) ) ;
#175704 =( NAMED_UNIT ( * ) SI_UNIT ( $, .STERADIAN. ) SOLID_ANGLE_UNIT ( ) );
#175705 = CARTESIAN_POINT ( 'NONE',  ( -0.6801582343750125492, 2.182291667008062763, 1.178068619123824323 ) ) ;
#175706 = CARTESIAN_POINT ( 'NONE',  ( -11.88237951145550042, 12.34319347378714937, -0.9087114598430712231 ) ) ;
#175707 = CARTESIAN_POINT ( 'NONE',  ( -9.528683032306089373, 10.01121838064558744, 0.7998128361456462443 ) ) ;
#175708 = CARTESIAN_POINT ( 'NONE',  ( 6.714312387265682247, 8.856450423275211037, 1.599625672291281386 ) ) ;
#175709 = CARTESIAN_POINT ( 'NONE',  ( -2.788906526875773208E-15, 8.937500000000001776, -1.499999999999998446 ) ) ;
#175710 = CARTESIAN_POINT ( 'NONE',  ( 2.982817717652554101, -0.1347461720548545627, -1.820777111243766733 ) ) ;
#175711 = CARTESIAN_POINT ( 'NONE',  ( 1.817678338065799704, -0.2697497798337232244, 2.190168480848574628 ) ) ;
#175712 = EDGE_LOOP ( 'NONE', ( #136152, #177147, #173419, #56764 ) ) ;
#175713 = CARTESIAN_POINT ( 'NONE',  ( -7.282664789195997912, 8.525472337930658284, 1.199719254218452047 ) ) ;
#175714 = CARTESIAN_POINT ( 'NONE',  ( -3.285556943749998737, -1.917708332855377673, 1.896917185911908499 ) ) ;
#175715 = CARTESIAN_POINT ( 'NONE',  ( -6.886651960737580680, 10.12184548991413457, -1.199719254218440723 ) ) ;
#175716 = CARTESIAN_POINT ( 'NONE',  ( 1.564719475598770337, 0.6377593443319184985, 1.916497437154760508 ) ) ;
#175717 = CARTESIAN_POINT ( 'NONE',  ( 1.119968162728638417, -0.5116716972351254000, 2.057716464106795318 ) ) ;
#175718 = EDGE_CURVE ( 'NONE', #57699, #200355, #23464, .T. ) ;
#175719 = EDGE_LOOP ( 'NONE', ( #117527, #91670, #145129, #13730 ) ) ;
#175720 = CARTESIAN_POINT ( 'NONE',  ( -5.743814354044916470, 6.730146830254374990, -1.199719254218453823 ) ) ;
#175721 = CARTESIAN_POINT ( 'NONE',  ( 3.133497910287503796, 1.768579976953125632, -0.5793101531420452588 ) ) ;
#175722 = CARTESIAN_POINT ( 'NONE',  ( 9.083072846151447166, 12.68433652289702884, 1.199719254218450271 ) ) ;
#175723 = CARTESIAN_POINT ( 'NONE',  ( 5.994767569012836361, -2.000857541758268354, 0.2496038112331094849 ) ) ;
#175724 = EDGE_LOOP ( 'NONE', ( #51593, #103523, #129192, #86289 ) ) ;
#175725 = ORIENTED_EDGE ( 'NONE', *, *, #180960, .F. ) ;
#175726 = CARTESIAN_POINT ( 'NONE',  ( -10.13202086811422475, 10.71511252242175161, -0.7998128361456291469 ) ) ;
#175727 = CARTESIAN_POINT ( 'NONE',  ( 3.756323439517950558, 0.6585720284536450420, 1.702948436616057881 ) ) ;
#175728 = CIRCLE ( 'NONE', #110071, 0.05000000000000012768 ) ;
#175731 = VERTEX_POINT ( 'NONE', #159155 ) ;
#175730 = CARTESIAN_POINT ( 'NONE',  ( -5.435328143874127882, 6.463069452080541843, -1.319038057358821403 ) ) ;
#175729 = CARTESIAN_POINT ( 'NONE',  ( -6.154475385960665790, 6.144919136567696505, 0.000000000000000000 ) ) ;
#175732 = CARTESIAN_POINT ( 'NONE',  ( 6.212391540903618115, 7.031971956796816414, -1.022972206104319826 ) ) ;
#175733 = CARTESIAN_POINT ( 'NONE',  ( 6.661482485103542572, -0.5350097378542042481, -1.943772860543022230 ) ) ;
#175734 = CARTESIAN_POINT ( 'NONE',  ( 6.017501326166345699, -1.026660802952833240, -1.528114487065170390 ) ) ;
#175735 = CARTESIAN_POINT ( 'NONE',  ( -0.02319159430949970999, 0.003959926571647092407, -1.810968101872318714 ) ) ;
#175736 = CARTESIAN_POINT ( 'NONE',  ( 4.407023800010228420, 1.785630936674869274, -1.461832730142158088 ) ) ;
#175737 = CARTESIAN_POINT ( 'NONE',  ( 7.042534447655770080, 7.180988041878682004, -0.7998128361456341429 ) ) ;
#175738 = CARTESIAN_POINT ( 'NONE',  ( 6.872347393157318685, -1.336039616365672700, 1.699942530728588919 ) ) ;
#175739 = CARTESIAN_POINT ( 'NONE',  ( 6.714312387265682247, 8.856450423275211037, 1.599625672291281386 ) ) ;
#175740 = CARTESIAN_POINT ( 'NONE',  ( 2.366656106817651040, 0.09313060749883492195, -1.939932752287050199 ) ) ;
#175741 = EDGE_CURVE ( 'NONE', #105328, #104090, #51943, .T. ) ;
#175742 = CARTESIAN_POINT ( 'NONE',  ( 5.870575887392723402, -0.5666052741825926553, 2.227357739769205924 ) ) ;
#175743 = CARTESIAN_POINT ( 'NONE',  ( -2.535011536075375105, 5.133042487381368701, 1.000000000000011324 ) ) ;
#175744 = CARTESIAN_POINT ( 'NONE',  ( -6.064239847062411926, 10.29697326487330500, 0.000000000000000000 ) ) ;
#175745 = CARTESIAN_POINT ( 'NONE',  ( 4.065207594588423845, 0.2294239933214488880, -1.856472568989680161 ) ) ;
#175746 = ORIENTED_EDGE ( 'NONE', *, *, #161141, .T. ) ;
#175748 = CIRCLE ( 'NONE', #110088, 0.1399999999999995970 ) ;
#175747 = AXIS2_PLACEMENT_3D ( 'NONE', #1116, #67178, #199317 ) ;
#175751 = CARTESIAN_POINT ( 'NONE',  ( -4.111865726694519552, 8.019203457777400956, 0.000000000000000000 ) ) ;
#175750 = CARTESIAN_POINT ( 'NONE',  ( -0.7500000000000006661, 1.889583334016155192, -1.299038105676652011 ) ) ;
#175749 = CARTESIAN_POINT ( 'NONE',  ( 2.918110517850933672, -1.910018876965378309, 0.09814724848770939314 ) ) ;
#175752 = CARTESIAN_POINT ( 'NONE',  ( 3.651171877326536030, -1.804458330144659950, 1.270265763067345066 ) ) ;
#175753 = CARTESIAN_POINT ( 'NONE',  ( 1.224999999999998757, 0.9375000006827949317, -8.673617379884035472E-15 ) ) ;
#175754 = CARTESIAN_POINT ( 'NONE',  ( 6.983263157960370116, 6.036630394911544073, 2.541087343977180613 ) ) ;
#175755 = CARTESIAN_POINT ( 'NONE',  ( 5.600926855776875435, 7.627776979863398310, -1.443375672974078761 ) ) ;
#175756 = CARTESIAN_POINT ( 'NONE',  ( -5.926322542504872892, 8.007405281046052536, -1.443375672974066548 ) ) ;
#175757 = CARTESIAN_POINT ( 'NONE',  ( 1.827351761895773530, -1.857630472158870116, 0.6603073207397982536 ) ) ;
#175758 = CARTESIAN_POINT ( 'NONE',  ( 2.151827808644761308, -1.853761708218491178, -1.374033529217959515 ) ) ;
#175759 = CARTESIAN_POINT ( 'NONE',  ( 2.295295855072278624, -1.753792786583353580, 0.8793850528211948347 ) ) ;
#175760 = CARTESIAN_POINT ( 'NONE',  ( -4.261005416444848315, 8.193199762486115034, 0.7998128361456350310 ) ) ;
#175761 = CARTESIAN_POINT ( 'NONE',  ( 6.034046607691841757, 1.223980295139483809, 1.660032098485002994 ) ) ;
#175762 = CARTESIAN_POINT ( 'NONE',  ( 3.551873057100283226, 6.127307085716883428, 1.082531754730558626 ) ) ;
#175763 = CARTESIAN_POINT ( 'NONE',  ( 3.872279980006509970, -1.995268062538615883, -0.2910826752766728642 ) ) ;
#175764 = CARTESIAN_POINT ( 'NONE',  ( 4.041212305325117882, 6.872442235258051646, -1.199719254218448494 ) ) ;
#175765 = ORIENTED_EDGE ( 'NONE', *, *, #68124, .T. ) ;
#175766 = CARTESIAN_POINT ( 'NONE',  ( -9.459838494033043332, 12.05956421450382088, 1.599625672291281386 ) ) ;
#175767 = CARTESIAN_POINT ( 'NONE',  ( 0.000000000000000000, -0.2000000000000057288, 0.000000000000000000 ) ) ;
#175768 = CARTESIAN_POINT ( 'NONE',  ( 8.238550898598388628, 12.76339314834017102, 0.7998128361456462443 ) ) ;
#175769 = CARTESIAN_POINT ( 'NONE',  ( 2.219799714087321796, 0.3745715905324221162, -2.138378345340052444 ) ) ;
#175770 = DIRECTION ( 'NONE',  ( -0.6483454320283799088, 0.000000000000000000, 0.7613463080411786432 ) ) ;
#175771 = CARTESIAN_POINT ( 'NONE',  ( -4.797597452551693564, 14.53090166595112365, -11.00826955084990111 ) ) ;
#175772 = DIRECTION ( 'NONE',  ( 0.000000000000000000, 0.000000000000000000, -1.000000000000000000 ) ) ;
#175773 = CARTESIAN_POINT ( 'NONE',  ( 2.002991962376502233, 1.552455721610061179, 1.043161660468715279 ) ) ;
#175774 = CARTESIAN_POINT ( 'NONE',  ( 6.116527240895272222, 1.456737685447502262, -1.597155580871166602 ) ) ;
#175776 = CARTESIAN_POINT ( 'NONE',  ( 6.727182134110202050, 0.5964276595885747989, 1.864301751488647962 ) ) ;
#175775 = CARTESIAN_POINT ( 'NONE',  ( -0.02224634325196597762, 0.2233488839939681836, -2.322587069611138144 ) ) ;
#175777 = CARTESIAN_POINT ( 'NONE',  ( 1.364683531249986537, 1.113541667008082658, 0.7879004041258500513 ) ) ;
#175778 = CARTESIAN_POINT ( 'NONE',  ( -1.355148357678327198, 3.930362057294688682, 0.6430964159811503045 ) ) ;
#175779 = CARTESIAN_POINT ( 'NONE',  ( 1.787617358713189386, 1.829539840090635749, -0.5563488465884156575 ) ) ;
#175780 = AXIS2_PLACEMENT_3D ( 'NONE', #150543, #211396, #66042 ) ;
#175781 =( BOUNDED_CURVE ( )  B_SPLINE_CURVE ( 2, ( #3588, #132597, #83798, #33986, #16653, #118507, #84870, #149891, #36108 ),
 .UNSPECIFIED., .F., .F. ) 
 B_SPLINE_CURVE_WITH_KNOTS ( ( 3, 2, 2, 2, 3 ),
 ( 0.3541666666666666852, 0.3611111111111111049, 0.3750000000000000000, 0.3888888888888888951, 0.3958333333333333703 ),
 .UNSPECIFIED. ) 
 CURVE ( )  GEOMETRIC_REPRESENTATION_ITEM ( )  RATIONAL_B_SPLINE_CURVE ( ( 0.9330127018922194093, 0.9330127018922196314, 1.000000000000000000, 0.8660254037844387076, 1.000000000000000000, 0.8660254037844387076, 1.000000000000000000, 0.9330127018922190762, 0.9330127018922194093 ) ) 
 REPRESENTATION_ITEM ( '' )  );
#175782 = CARTESIAN_POINT ( 'NONE',  ( 3.942089010115860326, 1.761346036062165332, 0.1732582469678861092 ) ) ;
#175783 = CARTESIAN_POINT ( 'NONE',  ( 1.717294761138322912, 1.590556852780611097, 1.061263400373997134 ) ) ;
#175784 = CARTESIAN_POINT ( 'NONE',  ( -5.579343907223557331, 6.467988298970945849, 1.199719254218450271 ) ) ;
#175785 = CARTESIAN_POINT ( 'NONE',  ( 6.591422782704708716, -0.4110296003016626898, 1.877638232857116174 ) ) ;
#175786 = CARTESIAN_POINT ( 'NONE',  ( 0.7499999999999885647, 0.4833333333333564297, 1.299038105676657340 ) ) ;
#175787 = CARTESIAN_POINT ( 'NONE',  ( 0.8189040078958352842, -1.500748464528355974, 1.426492703164506937 ) ) ;
#175788 = CARTESIAN_POINT ( 'NONE',  ( -1.364683531250014514, -0.6572916663252459379, 0.7879004041258379498 ) ) ;
#175789 = AXIS2_PLACEMENT_3D ( 'NONE', #126382, #175068, #158802 ) ;
#175790 = CARTESIAN_POINT ( 'NONE',  ( 5.506679003988666388, 1.415762158562785533, -1.222804595763474333 ) ) ;
#175791 = CARTESIAN_POINT ( 'NONE',  ( 2.139018802738294589, -1.631172329757241801, 0.8201644002571031322 ) ) ;
#175793 = CARTESIAN_POINT ( 'NONE',  ( 4.702859892337409420, 8.240897811179339172, 0.6291740908887258898 ) ) ;
#175792 = CARTESIAN_POINT ( 'NONE',  ( 5.461621781982892720, 0.4335984126433762853, -2.163701019753036192 ) ) ;
#175794 = CARTESIAN_POINT ( 'NONE',  ( -1.201851678989727383E-14, 5.509375000341415252, -1.575800808251660134 ) ) ;
#175795 = CARTESIAN_POINT ( 'NONE',  ( 2.646997546006967905, -0.3502154465670388461, -2.032575613165943818 ) ) ;
#175796 = CARTESIAN_POINT ( 'NONE',  ( -7.714753101375940503, 8.959299025482085455, 1.199719254218462483 ) ) ;
#175797 = DIRECTION ( 'NONE',  ( -1.000000000000000000, 5.578564026256490882E-16, -1.264049978315544409E-61 ) ) ;
#175798 = CARTESIAN_POINT ( 'NONE',  ( 9.399880572976245574, 9.860948844760784482, 0.7998128361456462443 ) ) ;
#175799 = CARTESIAN_POINT ( 'NONE',  ( 1.363015705810368239, 3.696841092726506517, -0.6271916676896889253 ) ) ;
#175800 = CARTESIAN_POINT ( 'NONE',  ( 0.7378453340087381962, -1.528073262844112268, -1.529135702860604074 ) ) ;
#175801 = CARTESIAN_POINT ( 'NONE',  ( 5.722423353419669567, 8.833855124701747386, 1.199719254218451159 ) ) ;
#175802 = ORIENTED_EDGE ( 'NONE', *, *, #180630, .T. ) ;
#175803 = CARTESIAN_POINT ( 'NONE',  ( 5.072747062355987602, 1.430223858385268665, -1.497173470029027120 ) ) ;
#175804 = CARTESIAN_POINT ( 'NONE',  ( 1.364683531249988757, 0.4468750003414206917, 0.000000000000000000 ) ) ;
#175805 = CARTESIAN_POINT ( 'NONE',  ( 2.548304106926166490, 2.161049004374314464, 0.05582717182670697553 ) ) ;
#175806 = CARTESIAN_POINT ( 'NONE',  ( -4.607477032339801326, 8.379641378740778634, 0.1280868206084313787 ) ) ;
#175807 = CARTESIAN_POINT ( 'NONE',  ( 3.334632977657724151, 1.279679970181834436, -1.562544408365494686 ) ) ;
#175808 = CARTESIAN_POINT ( 'NONE',  ( 6.720655732516647163, 1.258879151752972048, 2.189434846530075252 ) ) ;
#175809 = EDGE_CURVE ( 'NONE', #159827, #185972, #4277, .T. ) ;
#175812 = CARTESIAN_POINT ( 'NONE',  ( 5.965224400332808763, 9.903252867122883885, -0.7216878364870267237 ) ) ;
#175811 = CARTESIAN_POINT ( 'NONE',  ( 3.475000000000000533, -2.274999999999999467, 0.000000000000000000 ) ) ;
#175810 = DIRECTION ( 'NONE',  ( 0.9486832980505138790, -0.3162277660168376636, -3.312310031615527152E-15 ) ) ;
#175813 = CARTESIAN_POINT ( 'NONE',  ( -6.688968683495758683, 8.897159112202094988, -1.599625672291271394 ) ) ;
#175814 = CARTESIAN_POINT ( 'NONE',  ( 0.9367328597341374463, -1.586666764284098807, 1.244388658875786424 ) ) ;
#175816 = CARTESIAN_POINT ( 'NONE',  ( 6.427279137517246888, -1.429865906218323435, -1.660902671979214595 ) ) ;
#175815 = CARTESIAN_POINT ( 'NONE',  ( -3.893162665418476109, 7.693773542963529444, 1.040834085586084257E-14 ) ) ;
#175817 = CARTESIAN_POINT ( 'NONE',  ( -0.7500000000000215383, 4.972916667349482012, 1.299038105676671107 ) ) ;
#175818 = CARTESIAN_POINT ( 'NONE',  ( 4.341997288149157086, -1.180789491531178292, -1.504210074635865757 ) ) ;
#175819 = CARTESIAN_POINT ( 'NONE',  ( -11.96533679318059917, 12.34753988812995296, 0.9151144679398905968 ) ) ;
#175820 = CARTESIAN_POINT ( 'NONE',  ( 4.161989969270883272, 7.799479364217271282, 0.7216878364870317197 ) ) ;
#175822 = CARTESIAN_POINT ( 'NONE',  ( 2.952750085323506024, -1.864176452196796507, -0.7691048347045483791 ) ) ;
#175821 = CARTESIAN_POINT ( 'NONE',  ( -8.148087131688683371, 11.48955683940339867, -1.082531754730543083 ) ) ;
#175823 = CARTESIAN_POINT ( 'NONE',  ( 1.364683531250000303, 13.06770833367473728, -0.7879004041258355073 ) ) ;
#175824 = CIRCLE ( 'NONE', #144773, 2.500000000000007994 ) ;
#175825 = CARTESIAN_POINT ( 'NONE',  ( 5.297747862459361912, -0.6177129893134482019, 1.610538751920454592 ) ) ;
#175826 = CARTESIAN_POINT ( 'NONE',  ( 6.013923656113508542, 9.173938811177871244, -1.199719254218452047 ) ) ;
#175827 = CARTESIAN_POINT ( 'NONE',  ( 2.347533153460546806, 5.890539112345938300, 0.000000000000000000 ) ) ;
#175828 = DIRECTION ( 'NONE',  ( 0.000000000000000000, 1.000000000000000000, 0.000000000000000000 ) ) ;
#175829 = CARTESIAN_POINT ( 'NONE',  ( 3.919104170388473030, -0.1403237101727794756, 1.865361397874479632 ) ) ;
#175830 = EDGE_CURVE ( 'NONE', #105777, #118869, #110201, .T. ) ;
#175831 = DIRECTION ( 'NONE',  ( 0.000000000000000000, 0.000000000000000000, -1.000000000000000000 ) ) ;
#175832 = ORIENTED_EDGE ( 'NONE', *, *, #90678, .F. ) ;
#175833 = CARTESIAN_POINT ( 'NONE',  ( 0.9013344411078340057, -1.777497804657724334, 1.061070337243313455 ) ) ;
#175834 = DIRECTION ( 'NONE',  ( -1.000000000000000000, 0.000000000000000000, -8.638326563840826660E-31 ) ) ;
#175835 = ORIENTED_EDGE ( 'NONE', *, *, #104398, .T. ) ;
#175836 = CARTESIAN_POINT ( 'NONE',  ( 6.270143006926431006, 1.806086713848788161, -0.1406222877055433862 ) ) ;
#175837 = CARTESIAN_POINT ( 'NONE',  ( 3.203469434578891661, 6.959407783642502565, -0.7998128361456362523 ) ) ;
#175838 = CARTESIAN_POINT ( 'NONE',  ( 0.4217375466794699435, -1.802849824360297060, 0.1778772001973498718 ) ) ;
#175839 = CARTESIAN_POINT ( 'NONE',  ( 4.706088717274885092, 8.504537580213796133, 0.7216878364870317197 ) ) ;
#175840 = AXIS2_PLACEMENT_3D ( 'NONE', #148594, #32700, #98782 ) ;
#175841 = CARTESIAN_POINT ( 'NONE',  ( 1.849999999999999867, 0.1967728318288075040, 0.5999999999999968692 ) ) ;
#175842 = EDGE_LOOP ( 'NONE', ( #112319, #53980, #97681, #54768 ) ) ;
#175844 = CARTESIAN_POINT ( 'NONE',  ( 7.239163954692881653, 10.53310948286200599, -1.199719254218441611 ) ) ;
#175843 = CARTESIAN_POINT ( 'NONE',  ( 0.8890225878602634468, 0.1407106197201784259, 1.956863499422318631 ) ) ;
#175845 = CARTESIAN_POINT ( 'NONE',  ( 4.815990648786471873, 0.9809511849332609446, -1.645218558792021613 ) ) ;
#175846 = CARTESIAN_POINT ( 'NONE',  ( 0.000000000000000000, 2.999999999999999112, -2.500000000000000444 ) ) ;
#175847 = CARTESIAN_POINT ( 'NONE',  ( -6.435690514315323796, 6.800136771869164320, 0.4354173353855045336 ) ) ;
#175848 =( NAMED_UNIT ( * ) PLANE_ANGLE_UNIT ( ) SI_UNIT ( $, .RADIAN. ) );
#175850 = ORIENTED_EDGE ( 'NONE', *, *, #100401, .T. ) ;
#175849 = CARTESIAN_POINT ( 'NONE',  ( 6.182154858151487353, 6.314861544039274577, -0.7216878364870257245 ) ) ;
#175851 = ADVANCED_FACE ( 'NONE', ( #160224 ), #193778, .F. ) ;
#175852 = B_SPLINE_CURVE_WITH_KNOTS ( 'NONE', 3,
 ( #80284, #161554, #45677, #79218 ),
 .UNSPECIFIED., .F., .F.,
 ( 4, 4 ),
 ( 0.000000000000000000, 2.032232339056924315E-05 ),
 .UNSPECIFIED. ) ;
#175853 = CARTESIAN_POINT ( 'NONE',  ( -9.056483424248693126, 10.62861408545402675, 1.082531754730558626 ) ) ;
#175854 = CARTESIAN_POINT ( 'NONE',  ( 1.973706723050288936, 2.068691090354588091, -0.6273066937243013674 ) ) ;
#175855 = CARTESIAN_POINT ( 'NONE',  ( -5.496904935697871863, 5.377753611261092637, 0.7998128361456281477 ) ) ;
#175856 = CARTESIAN_POINT ( 'NONE',  ( 6.034787771858531435, 10.05468647722803865, 0.000000000000000000 ) ) ;
#175857 = CARTESIAN_POINT ( 'NONE',  ( -3.952365473583647315, 4.569846793057691592, 1.199719254218462483 ) ) ;
#175858 = EDGE_CURVE ( 'NONE', #140091, #8935, #211084, .T. ) ;
#175859 = CARTESIAN_POINT ( 'NONE',  ( 4.981388616008130654, 1.702979688329594676, -0.6582044668519275721 ) ) ;
#175860 = CARTESIAN_POINT ( 'NONE',  ( 11.62299063338605087, 6.986215174415851159, 1.907829974770760328 ) ) ;
#175861 = CARTESIAN_POINT ( 'NONE',  ( 0.7550724807275938089, -1.663022853828221681, -1.058333363951379003 ) ) ;
#175862 = CARTESIAN_POINT ( 'NONE',  ( 3.216961742616857745, 1.504763323797538410, -1.180078671740567131 ) ) ;
#175863 = VERTEX_POINT ( 'NONE', #59515 ) ;
#175864 = CARTESIAN_POINT ( 'NONE',  ( 10.38819714233671121, 3.487142912321096855, 5.997628416522882588 ) ) ;
#175865 = CARTESIAN_POINT ( 'NONE',  ( 4.316829372628319561, -1.460888098903726728, 1.321172513512254065 ) ) ;
#175866 = ORIENTED_EDGE ( 'NONE', *, *, #152411, .T. ) ;
#175867 = CARTESIAN_POINT ( 'NONE',  ( 6.392136499528294102, -0.5222240449473265489, -1.870457282704639290 ) ) ;
#175868 = ORIENTED_EDGE ( 'NONE', *, *, #12933, .F. ) ;
#175869 = CARTESIAN_POINT ( 'NONE',  ( -5.936491157937300756, 8.019268665717216749, 1.599625672291263179 ) ) ;
#175871 = CARTESIAN_POINT ( 'NONE',  ( 6.451439665316073935, -1.893653415279672902, 0.9546920624979161607 ) ) ;
#175870 = CARTESIAN_POINT ( 'NONE',  ( -4.447956913735107598, 7.346977611736363656, 1.199719254218452935 ) ) ;
#175872 = CARTESIAN_POINT ( 'NONE',  ( 6.902509602688803980, 9.146290184594002781, -1.443375672974064550 ) ) ;
#175873 = CARTESIAN_POINT ( 'NONE',  ( 3.932203299393256302, -0.9856607118853939475, -1.638553295466014248 ) ) ;
#175874 = CARTESIAN_POINT ( 'NONE',  ( 0.000000000000000000, -2.079999999999998295, 0.000000000000000000 ) ) ;
#175875 = LINE ( 'NONE', #208337, #136825 ) ;
#175876 = FILL_AREA_STYLE ('',( #109862 ) ) ;
#175877 = CARTESIAN_POINT ( 'NONE',  ( 4.617841973404108735, -0.5345865524139911118, 1.940763608534997520 ) ) ;
#175878 = CARTESIAN_POINT ( 'NONE',  ( 1.459778984583645340E-15, 0.08000000000000020983, -11.92000000000000171 ) ) ;
#175879 = CARTESIAN_POINT ( 'NONE',  ( 5.883392091387671385, 1.685093539698417242, -0.7030590484573000509 ) ) ;
#175880 = CARTESIAN_POINT ( 'NONE',  ( 1.381394743813993964, -0.05274132383669553892, 2.069866178704110382 ) ) ;
#175881 = CARTESIAN_POINT ( 'NONE',  ( -7.036318535812428721, 11.15286269184909784, 0.000000000000000000 ) ) ;
#175882 = AXIS2_PLACEMENT_3D ( 'NONE', #137280, #9392, #154588 ) ;
#175883 = CARTESIAN_POINT ( 'NONE',  ( -5.670379370357061077, 7.341873695786736320, -1.227147999111227294 ) ) ;
#175884 = CARTESIAN_POINT ( 'NONE',  ( -5.810221930991193690E-16, 2.125000000682803147, 1.224999999999976774 ) ) ;
#175885 = CARTESIAN_POINT ( 'NONE',  ( -2.900957617708239678, -3.232243495192087757, 1.542507481629952881 ) ) ;
#175886 = CARTESIAN_POINT ( 'NONE',  ( 7.149227073107712549, 7.235186428247455837, -0.7998128361456281477 ) ) ;
#175887 = CARTESIAN_POINT ( 'NONE',  ( 6.211043768836185031, 6.418841616496599123, 0.7216878364870328300 ) ) ;
#175888 = CARTESIAN_POINT ( 'NONE',  ( 2.758194185376297902, 5.305311418659259814, 1.199719254218452047 ) ) ;
#175889 = CARTESIAN_POINT ( 'NONE',  ( 0.6823417656249934904, 12.00520833367473017, 1.181850606188764807 ) ) ;
#175890 = CARTESIAN_POINT ( 'NONE',  ( -4.111146893441842920, 5.819424013814012753, 1.599625672291267398 ) ) ;
#175892 = CARTESIAN_POINT ( 'NONE',  ( -7.144220599758281054, 7.299621885998258897, 0.7998128361456341429 ) ) ;
#175891 = SURFACE_SIDE_STYLE ('',( #109879 ) ) ;
#175893 = CARTESIAN_POINT ( 'NONE',  ( 3.498401880895495086, -1.707742140280370746, 0.3003691301488361498 ) ) ;
#175894 = CARTESIAN_POINT ( 'NONE',  ( -5.362413449404877852, 6.214902764849178141, -1.199719254218446718 ) ) ;
#175895 = AXIS2_PLACEMENT_3D ( 'NONE', #49978, #181042, #149614 ) ;
#175896 = CARTESIAN_POINT ( 'NONE',  ( 2.659107809384615884, 1.665393510391148801, -1.229642267604726058 ) ) ;
#175897 = CARTESIAN_POINT ( 'NONE',  ( 3.779011003814860548, 1.787463462570267447, -1.134484337778138174 ) ) ;
#175898 = CARTESIAN_POINT ( 'NONE',  ( 7.914208982075123799, 10.25632978388623684, -1.599625672291262513 ) ) ;
#175899 = CARTESIAN_POINT ( 'NONE',  ( 1.364683531249988535, 3.863541667008087543, 0.7879004041258499402 ) ) ;
#175900 = CARTESIAN_POINT ( 'NONE',  ( 0.9011414689646871645, -1.692011168669171672, 1.007586202480597048 ) ) ;
#175901 = CARTESIAN_POINT ( 'NONE',  ( 6.101957686160805139, 6.023808750328159434, -0.2146407016825630509 ) ) ;
#175902 = CARTESIAN_POINT ( 'NONE',  ( 4.039966587192267866, 4.776011108888172707, 1.082531754730560403 ) ) ;
#175904 = DIRECTION ( 'NONE',  ( 5.551115123125764829E-17, 0.000000000000000000, -1.000000000000000000 ) ) ;
#175903 = CARTESIAN_POINT ( 'NONE',  ( 0.000000000000000000, -1.487500000000001599, -4.012584370867899430 ) ) ;
#175905 = CARTESIAN_POINT ( 'NONE',  ( 3.609589514692018053, -2.258491968568816066, 0.3911977494595666460 ) ) ;
#175906 = CARTESIAN_POINT ( 'NONE',  ( 0.9260630535584664091, 1.089557764695957554, -1.464779044915397455 ) ) ;
#175907 = CARTESIAN_POINT ( 'NONE',  ( 3.691585721427274258, 1.799035686688513325, -0.6489376663148455071 ) ) ;
#175908 = CARTESIAN_POINT ( 'NONE',  ( 6.703580607314123085, 6.785541894813420072, 0.000000000000000000 ) ) ;
#175909 = CARTESIAN_POINT ( 'NONE',  ( 7.144783764277405247, 8.398297815487545392, -1.082531754730543971 ) ) ;
#175910 = CARTESIAN_POINT ( 'NONE',  ( -9.104463846776669200, 10.58062822844965645, -1.199719254218441611 ) ) ;
#175911 = CARTESIAN_POINT ( 'NONE',  ( 1.775641216270260170, 0.3400756789797795832, -1.984116031292797677 ) ) ;
#175912 = CARTESIAN_POINT ( 'NONE',  ( 1.920681792755131845, -1.391007931628859939, 1.383589105726056756 ) ) ;
#175913 = CARTESIAN_POINT ( 'NONE',  ( -7.486073373039941359, 11.88550270185529278, -0.7998128361456291469 ) ) ;
#175914 = CARTESIAN_POINT ( 'NONE',  ( -5.442708600882160574, 8.437244903416123876, -1.199719254218446718 ) ) ;
#175915 = LINE ( 'NONE', #124035, #2216 ) ;
#175917 = CARTESIAN_POINT ( 'NONE',  ( 3.045496301383675330, 0.6385914081092295413, -1.650799995714345325 ) ) ;
#175916 = CARTESIAN_POINT ( 'NONE',  ( 5.472635741755179417, -0.05041999219103148605, -2.090201512065153366 ) ) ;
#175918 = CARTESIAN_POINT ( 'NONE',  ( 2.007420792093927986E-08, -6.938893903907228378E-15, -1.225000000000033396 ) ) ;
#175919 = CARTESIAN_POINT ( 'NONE',  ( 6.562434020506859866, -2.092894318229638895, -0.9354203566987564500 ) ) ;
#175920 = CARTESIAN_POINT ( 'NONE',  ( 5.120954501598782294, -1.650910780824323298, 0.5508982476954398244 ) ) ;
#175921 = CARTESIAN_POINT ( 'NONE',  ( 6.916630921265960019, 11.22115317478565188, 0.7998128361456462443 ) ) ;
#175922 = DIRECTION ( 'NONE',  ( 0.000000000000000000, 1.000000000000000000, 0.000000000000000000 ) ) ;
#175923 = CARTESIAN_POINT ( 'NONE',  ( 5.307816166741994302, -1.486200299559970128, 0.8926388968444918248 ) ) ;
#175924 = CARTESIAN_POINT ( 'NONE',  ( 6.303213947599001443, -1.837614076384209261, 1.156103312670229810 ) ) ;
#175925 = CARTESIAN_POINT ( 'NONE',  ( -11.48243876534946217, 11.37999999999998302, 3.199999999999997957 ) ) ;
#175926 = CARTESIAN_POINT ( 'NONE',  ( 6.350795928397162449, -1.845624747684541989, -0.8128223418941012968 ) ) ;
#175927 = CARTESIAN_POINT ( 'NONE',  ( 5.406250000000002665, 1.895863743163962223, -0.7852924748302683167 ) ) ;
#175928 = CARTESIAN_POINT ( 'NONE',  ( 0.7499999999999902300, 5.347916667349482012, -1.299038105676658228 ) ) ;
#175929 = CARTESIAN_POINT ( 'NONE',  ( 3.522408793619712153, 1.222923848883204156, -1.488421986030899591 ) ) ;
#175930 = CARTESIAN_POINT ( 'NONE',  ( 0.7500000000000006661, 10.86458333401613174, 1.299038105676657340 ) ) ;
#175931 = CARTESIAN_POINT ( 'NONE',  ( 0.1357878378635381522, -0.1024811726445598314, 2.219055157331132566 ) ) ;
#175932 = VERTEX_POINT ( 'NONE', #125673 ) ;
#175933 = CARTESIAN_POINT ( 'NONE',  ( -0.7499999999999972244, 3.858333333333359594, -1.299038105676652011 ) ) ;
#175934 = CARTESIAN_POINT ( 'NONE',  ( 6.094553744542824170, 7.069066442510145265, 1.199719254218462483 ) ) ;
#175935 = STYLED_ITEM ( 'NONE', ( #98085 ), #154563 ) ;
#175936 = CARTESIAN_POINT ( 'NONE',  ( 2.807538669062619174, 1.903917518177394630, -1.144040067606937550 ) ) ;
#175937 = CARTESIAN_POINT ( 'NONE',  ( -0.02900071798685524560, 0.6937575422599016051, -2.255700163050919471 ) ) ;
#175938 = CARTESIAN_POINT ( 'NONE',  ( 6.778713617152772208, 10.85232362007950258, -0.7216878364870267237 ) ) ;
#175939 = CARTESIAN_POINT ( 'NONE',  ( -7.809133291347029271, 12.05447990663947877, 0.000000000000000000 ) ) ;
#175940 = CARTESIAN_POINT ( 'NONE',  ( 7.241463443474815520, 8.581367117876336437, -1.082531754730548412 ) ) ;
#175941 = CARTESIAN_POINT ( 'NONE',  ( 0.5807041986926939625, -0.7231374404764076003, 1.882475062126743204 ) ) ;
#175943 = CARTESIAN_POINT ( 'NONE',  ( 5.986801016505616246, 1.986937900772387078, 0.5535461689152029185 ) ) ;
#175942 = CARTESIAN_POINT ( 'NONE',  ( 7.716561984472250835, 12.15440608185967086, 1.040834085586084257E-14 ) ) ;
#175944 = CARTESIAN_POINT ( 'NONE',  ( 1.499999999999990896, 5.275000000000022560, 1.214306433183764966E-14 ) ) ;
#175945 = CARTESIAN_POINT ( 'NONE',  ( -4.115063316947640715, 4.759660943649018705, 1.199719254218462483 ) ) ;
#175946 = SURFACE_STYLE_FILL_AREA ( #209470 ) ;
#175947 = CARTESIAN_POINT ( 'NONE',  ( -1.402160292154681736E-14, 1.196875000341419026, -1.575800808251659024 ) ) ;
#175948 = CARTESIAN_POINT ( 'NONE',  ( 0.3503969169679886919, -1.426633182142377443, 1.047046497418676392 ) ) ;
#175949 = CARTESIAN_POINT ( 'NONE',  ( 5.959525138608227302, -1.649545596257080637, -0.5353374286216765476 ) ) ;
#175950 = CARTESIAN_POINT ( 'NONE',  ( 6.040530583712122592, -1.465329908677007742, 0.9388326107527265041 ) ) ;
#175951 = CARTESIAN_POINT ( 'NONE',  ( 2.595625714788946770, -0.7159257691751429453, 2.177794363412302481 ) ) ;
#175952 = CARTESIAN_POINT ( 'NONE',  ( -1.364683531250000748, 0.009375000341420303140, 0.000000000000000000 ) ) ;
#175953 = CARTESIAN_POINT ( 'NONE',  ( 2.114959233223293822, -1.785989328681826027, 0.4467204754193611627 ) ) ;
#175954 = CARTESIAN_POINT ( 'NONE',  ( 8.910733272679570049, 11.41894145625809820, -1.599625672291255185 ) ) ;
#175955 = CARTESIAN_POINT ( 'NONE',  ( 0.000000000000000000, 3.999999999999994671, 12.00000000000000355 ) ) ;
#175956 = CARTESIAN_POINT ( 'NONE',  ( 2.520284954824199453, 1.194270260598716771, -1.380820861806408617 ) ) ;
#175957 = EDGE_CURVE ( 'NONE', #177712, #20719, #67472, .T. ) ;
#175958 = CARTESIAN_POINT ( 'NONE',  ( 4.289685514112329123, 1.556909497225898109, -1.281360267751927129 ) ) ;
#175959 = CARTESIAN_POINT ( 'NONE',  ( -3.755245360860939297, 4.443836344834937613, -1.082531754730548412 ) ) ;
#175960 = CARTESIAN_POINT ( 'NONE',  ( 4.702146809683701356, 5.356480858934594025, -2.500000000000000444 ) ) ;
#175961 = CARTESIAN_POINT ( 'NONE',  ( 5.385806172021708527, 1.412131043145675280, 1.562536384088798691 ) ) ;
#175962 = CARTESIAN_POINT ( 'NONE',  ( -6.898401231254901234, 6.942556279419168419, -0.7998128361456291469 ) ) ;
#175963 = CARTESIAN_POINT ( 'NONE',  ( 9.224544533040779370, 13.18315223404453107, 9.019998505197957428 ) ) ;
#175964 =( BOUNDED_SURFACE ( )  B_SPLINE_SURFACE ( 1, 2, ( 
 ( #102881, #167877, #98625, #85552, #148444, #14, #66078, #132219, #34669, #151642, #185172, #198229, #3211, #20541, #86625, #69279, #152692, #131187, #100739, #49865, #115991, #99682, #165751, #83419, #103954, #40018, #206761, #89849, #58393, #25875, #23744, #108279, #189455, #88775, #8564, #154833, #124549, #123491, #190507, #155899, #55196, #172152, #7486, #6417, #73568, #171067, #120268, #169997, #56264, #139670, #136461, #140750, #72489, #173229, #187318, #138590, #202480, #105029, #90910, #186243, #204613, #91985, #70344, #205692, #174300, #122423, #37878, #54133, #188380, #21584, #121343, #87689, #106129, #42164, #57327, #158044, #153764, #41096, #5332, #107206, #24809, #74645, #156975, #71415, #137527, #203542, #38946, #22664, #111473, #29093, #28019, #161226, #110410, #59453, #43233, #209946, #177478, #75707, #79959, #11756, #112532, #126672, #160158, #141822, #44288, #30154, #125610, #94117, #179608, #9630, #192635, #46415, #113604, #77830, #176413, #109350, #97303, #31229, #191569, #146062, #143951, #162293, #128796, #78886, #61585, #195855, #175360, #212075, #211015, #127754, #193711, #63714, #129872, #207824, #12813, #95177, #26941, #93048, #47495, #159089, #10687, #194778, #76757, #142879, #208881, #13880, #60511, #45354, #145009, #62638, #178544, #96242, #35472, #32287, #213146, #131956, #133018, #130917, #118934, #100477, #83151, #34405, #149230, #66873, #199017, #214181, #19218, #197966, #49597, #150317, #36538, #64776, #165477, #50664, #196910, #135140, #200096, #147120, #117868, #14938, #48550, #81033, #114668, #805, #183859, #85296, #180662, #182787, #167619, #151382, #116790, #98353, #164418, #99423, #101550, #51745, #115721, #16002, #82087, #52795, #2952, #69023, #181712, #17073, #33341, #166553, #201156, #18141, #148180, #65809, #84229, #1883, #67943, #134088, #184914, #163362, #5080, #4018, #103697, #104769, #190255, #153511, #170818, #56007, #22409, #88518, #189202, #90657, #168681, #138333, #171888, #20285, #154580, #7225, #23485, #106948, #122159, #102625, #6157, #72226, #187058 ),
 ( #139403, #86370, #57073, #152439, #70087, #136202, #53874, #204349, #123237, #172971, #202220, #188126, #24550, #156719, #39757, #89592, #140496, #105862, #120007, #185983, #155641, #37617, #71155, #169748, #73301, #8310, #205437, #74395, #58137, #40839, #206506, #124296, #121091, #21336, #38691, #87442, #137272, #203292, #54939, #26696, #143705, #61341, #60264, #193471, #142622, #91735, #75455, #27770, #209697, #108024, #112289, #44039, #144767, #158842, #192385, #174050, #76511, #62400, #157788, #126421, #211833, #41913, #10439, #78641, #145828, #110158, #208631, #141568, #129625, #63470, #25623, #176170, #160978, #29914, #128563, #159904, #92797, #28841, #93866, #125352, #207576, #11511, #194528, #210777, #77582, #9384, #59196, #191315, #46175, #95996, #127500, #45115, #111225, #177228, #178305, #94929, #42983, #109093, #175109, #12569, #162050, #13640, #79712, #81845, #98124, #97063, #196668, #197715, #71707, #32037, #49357, #151927, #115476, #184402, #70636, #186543, #47247, #19769, #53349, #113361, #36022, #103170, #119483, #202774, #3501, #195610, #102100, #168170, #65565, #136747, #179366, #85851, #131712, #48308, #64535, #54425, #21879, #147928, #164175, #69571, #4561, #152987, #213944, #104245, #135681, #130679, #86919, #30988, #114419, #120566, #163116, #146882, #212902, #14698, #87985, #185470, #170291, #80792, #37092, #15760, #169232, #201705, #180419, #154060, #20822, #38173, #5626, #138888, #124834, #92289, #139965, #157269, #73871, #41393, #109648, #105326, #108569, #171363, #43525, #8859, #22957, #40317, #39234, #6711, #42460, #107504, #173532, #91207, #74938, #89072, #93345, #158333, #188682, #190800, #187607, #9927, #57624, #141049, #205988, #76001, #26173, #90136, #155129, #72787, #27238, #142106, #125907, #106423, #123782, #156203, #25105, #174596, #207055, #204907, #55485, #56560, #203839, #122719, #24033, #172446, #7779, #189741, #58686, #208119, #59747, #10980, #191864, #175651, #159381, #137820, #121639, #163661, #65058, #143184, #112835, #146362, #209175, #145314, #196156, #212376, #81330 ) ),
 .UNSPECIFIED., .F., .F., .T. ) 
 B_SPLINE_SURFACE_WITH_KNOTS ( ( 2, 2 ),
 ( 3, 2, 2, 2, 2, 2, 2, 2, 2, 2, 2, 2, 2, 2, 2, 2, 2, 2, 2, 2, 2, 2, 2, 2, 2, 2, 2, 2, 2, 2, 2, 2, 2, 2, 2, 2, 2, 2, 2, 2, 2, 2, 2, 2, 2, 2, 2, 2, 2, 2, 2, 2, 2, 2, 2, 2, 2, 2, 2, 2, 2, 2, 2, 2, 2, 2, 2, 2, 2, 2, 2, 2, 2, 2, 2, 2, 2, 2, 2, 2, 2, 2, 2, 2, 2, 2, 2, 2, 2, 2, 2, 2, 2, 2, 2, 2, 2, 2, 2, 2, 2, 2, 2, 2, 2, 2, 2, 2, 2, 2, 2, 2, 2, 2, 2, 2, 2, 2, 2, 2, 3 ),
 ( 0.000000000000000000, 1.000000000000000000 ),
 ( 0.000000000000000000, 0.008333333333333333218, 0.01666666666666666644, 0.02500000000000000139, 0.03333333333333333287, 0.04166666666666666435, 0.05000000000000000278, 0.05833333333333333426, 0.06666666666666666574, 0.07499999999999999722, 0.08333333333333332871, 0.09166666666666666019, 0.1000000000000000056, 0.1083333333333333370, 0.1166666666666666685, 0.1250000000000000000, 0.1333333333333333315, 0.1416666666666666630, 0.1499999999999999944, 0.1583333333333333259, 0.1666666666666666574, 0.1749999999999999889, 0.1833333333333333204, 0.1916666666666666796, 0.2000000000000000111, 0.2083333333333333426, 0.2166666666666666741, 0.2250000000000000056, 0.2333333333333333370, 0.2416666666666666685, 0.2500000000000000000, 0.2583333333333333592, 0.2666666666666666630, 0.2750000000000000222, 0.2833333333333333259, 0.2916666666666666852, 0.2999999999999999889, 0.3083333333333333481, 0.3166666666666666519, 0.3250000000000000111, 0.3333333333333333148, 0.3416666666666666741, 0.3499999999999999778, 0.3583333333333333370, 0.3666666666666666408, 0.3750000000000000000, 0.3833333333333333592, 0.3916666666666666630, 0.4000000000000000222, 0.4083333333333333259, 0.4166666666666666852, 0.4249999999999999889, 0.4333333333333333481, 0.4416666666666666519, 0.4500000000000000111, 0.4583333333333333148, 0.4666666666666666741, 0.4749999999999999778, 0.4833333333333333370, 0.4916666666666666408, 0.5000000000000000000, 0.5083333333333333037, 0.5166666666666667185, 0.5250000000000000222, 0.5333333333333333259, 0.5416666666666666297, 0.5500000000000000444, 0.5583333333333333481, 0.5666666666666666519, 0.5749999999999999556, 0.5833333333333333703, 0.5916666666666666741, 0.5999999999999999778, 0.6083333333333332815, 0.6166666666666666963, 0.6250000000000000000, 0.6333333333333333037, 0.6416666666666667185, 0.6500000000000000222, 0.6583333333333333259, 0.6666666666666666297, 0.6750000000000000444, 0.6833333333333333481, 0.6916666666666666519, 0.6999999999999999556, 0.7083333333333333703, 0.7166666666666666741, 0.7249999999999999778, 0.7333333333333332815, 0.7416666666666666963, 0.7500000000000000000, 0.7583333333333333037, 0.7666666666666667185, 0.7750000000000000222, 0.7833333333333333259, 0.7916666666666666297, 0.8000000000000000444, 0.8083333333333333481, 0.8166666666666666519, 0.8249999999999999556, 0.8333333333333333703, 0.8416666666666666741, 0.8499999999999999778, 0.8583333333333332815, 0.8666666666666666963, 0.8750000000000000000, 0.8833333333333333037, 0.8916666666666667185, 0.9000000000000000222, 0.9083333333333333259, 0.9166666666666666297, 0.9250000000000000444, 0.9333333333333333481, 0.9416666666666666519, 0.9499999999999999556, 0.9583333333333333703, 0.9666666666666666741, 0.9749999999999999778, 0.9833333333333332815, 0.9916666666666666963, 1.000000000000000000 ),
 .UNSPECIFIED. ) 
 GEOMETRIC_REPRESENTATION_ITEM ( )  RATIONAL_B_SPLINE_SURFACE ( (
 ( 1.000000000000000000, 0.8660254037844387076, 1.000000000000000000, 0.8660254037844387076, 1.000000000000000000, 0.8660254037844387076, 1.000000000000000000, 0.8660254037844387076, 1.000000000000000000, 0.8660254037844387076, 1.000000000000000000, 0.8660254037844387076, 1.000000000000000000, 0.8660254037844387076, 1.000000000000000000, 0.8660254037844387076, 1.000000000000000000, 0.8660254037844387076, 1.000000000000000000, 0.8660254037844387076, 1.000000000000000000, 0.8660254037844387076, 1.000000000000000000, 0.8660254037844387076, 1.000000000000000000, 0.8660254037844387076, 1.000000000000000000, 0.8660254037844387076, 1.000000000000000000, 0.8660254037844387076, 1.000000000000000000, 0.8660254037844387076, 1.000000000000000000, 0.8660254037844387076, 1.000000000000000000, 0.8660254037844387076, 1.000000000000000000, 0.8660254037844387076, 1.000000000000000000, 0.8660254037844387076, 1.000000000000000000, 0.8660254037844387076, 1.000000000000000000, 0.8660254037844387076, 1.000000000000000000, 0.8660254037844387076, 1.000000000000000000, 0.8660254037844387076, 1.000000000000000000, 0.8660254037844387076, 1.000000000000000000, 0.8660254037844387076, 1.000000000000000000, 0.8660254037844387076, 1.000000000000000000, 0.8660254037844387076, 1.000000000000000000, 0.8660254037844387076, 1.000000000000000000, 0.8660254037844387076, 1.000000000000000000, 0.8660254037844387076, 1.000000000000000000, 0.8660254037844387076, 1.000000000000000000, 0.8660254037844387076, 1.000000000000000000, 0.8660254037844387076, 1.000000000000000000, 0.8660254037844387076, 1.000000000000000000, 0.8660254037844387076, 1.000000000000000000, 0.8660254037844387076, 1.000000000000000000, 0.8660254037844387076, 1.000000000000000000, 0.8660254037844387076, 1.000000000000000000, 0.8660254037844387076, 1.000000000000000000, 0.8660254037844387076, 1.000000000000000000, 0.8660254037844387076, 1.000000000000000000, 0.8660254037844387076, 1.000000000000000000, 0.8660254037844387076, 1.000000000000000000, 0.8660254037844387076, 1.000000000000000000, 0.8660254037844387076, 1.000000000000000000, 0.8660254037844387076, 1.000000000000000000, 0.8660254037844387076, 1.000000000000000000, 0.8660254037844387076, 1.000000000000000000, 0.8660254037844387076, 1.000000000000000000, 0.8660254037844387076, 1.000000000000000000, 0.8660254037844387076, 1.000000000000000000, 0.8660254037844387076, 1.000000000000000000, 0.8660254037844387076, 1.000000000000000000, 0.8660254037844387076, 1.000000000000000000, 0.8660254037844387076, 1.000000000000000000, 0.8660254037844387076, 1.000000000000000000, 0.8660254037844387076, 1.000000000000000000, 0.8660254037844387076, 1.000000000000000000, 0.8660254037844387076, 1.000000000000000000, 0.8660254037844387076, 1.000000000000000000, 0.8660254037844387076, 1.000000000000000000, 0.8660254037844387076, 1.000000000000000000, 0.8660254037844387076, 1.000000000000000000, 0.8660254037844387076, 1.000000000000000000, 0.8660254037844387076, 1.000000000000000000, 0.8660254037844387076, 1.000000000000000000, 0.8660254037844387076, 1.000000000000000000, 0.8660254037844387076, 1.000000000000000000, 0.8660254037844387076, 1.000000000000000000, 0.8660254037844387076, 1.000000000000000000, 0.8660254037844387076, 1.000000000000000000, 0.8660254037844387076, 1.000000000000000000, 0.8660254037844387076, 1.000000000000000000, 0.8660254037844387076, 1.000000000000000000, 0.8660254037844387076, 1.000000000000000000, 0.8660254037844387076, 1.000000000000000000, 0.8660254037844387076, 1.000000000000000000, 0.8660254037844387076, 1.000000000000000000, 0.8660254037844387076, 1.000000000000000000, 0.8660254037844387076, 1.000000000000000000, 0.8660254037844387076, 1.000000000000000000, 0.8660254037844387076, 1.000000000000000000, 0.8660254037844387076, 1.000000000000000000, 0.8660254037844387076, 1.000000000000000000, 0.8660254037844387076, 1.000000000000000000, 0.8660254037844387076, 1.000000000000000000, 0.8660254037844387076, 1.000000000000000000, 0.8660254037844387076, 1.000000000000000000, 0.8660254037844387076, 1.000000000000000000, 0.8660254037844387076, 1.000000000000000000, 0.8660254037844387076, 1.000000000000000000, 0.8660254037844387076, 1.000000000000000000, 0.8660254037844387076, 1.000000000000000000, 0.8660254037844387076, 1.000000000000000000, 0.8660254037844387076, 1.000000000000000000, 0.8660254037844387076, 1.000000000000000000, 0.8660254037844387076, 1.000000000000000000, 0.8660254037844387076, 1.000000000000000000, 0.8660254037844387076, 1.000000000000000000, 0.8660254037844387076, 1.000000000000000000, 0.8660254037844387076, 1.000000000000000000, 0.8660254037844387076, 1.000000000000000000, 0.8660254037844387076, 1.000000000000000000, 0.8660254037844387076, 1.000000000000000000, 0.8660254037844387076, 1.000000000000000000, 0.8660254037844387076, 1.000000000000000000, 0.8660254037844387076, 1.000000000000000000, 0.8660254037844387076, 1.000000000000000000, 0.8660254037844387076, 1.000000000000000000, 0.8660254037844387076, 1.000000000000000000, 0.8660254037844387076, 1.000000000000000000, 0.8660254037844387076, 1.000000000000000000, 0.8660254037844387076, 1.000000000000000000, 0.8660254037844387076, 1.000000000000000000, 0.8660254037844387076, 1.000000000000000000, 0.8660254037844387076, 1.000000000000000000, 0.8660254037844387076, 1.000000000000000000, 0.8660254037844387076, 1.000000000000000000, 0.8660254037844387076, 1.000000000000000000),
 ( 1.000000000000000000, 0.8660254037844387076, 1.000000000000000000, 0.8660254037844387076, 1.000000000000000000, 0.8660254037844387076, 1.000000000000000000, 0.8660254037844387076, 1.000000000000000000, 0.8660254037844387076, 1.000000000000000000, 0.8660254037844387076, 1.000000000000000000, 0.8660254037844387076, 1.000000000000000000, 0.8660254037844387076, 1.000000000000000000, 0.8660254037844387076, 1.000000000000000000, 0.8660254037844387076, 1.000000000000000000, 0.8660254037844387076, 1.000000000000000000, 0.8660254037844387076, 1.000000000000000000, 0.8660254037844387076, 1.000000000000000000, 0.8660254037844387076, 1.000000000000000000, 0.8660254037844387076, 1.000000000000000000, 0.8660254037844387076, 1.000000000000000000, 0.8660254037844387076, 1.000000000000000000, 0.8660254037844387076, 1.000000000000000000, 0.8660254037844387076, 1.000000000000000000, 0.8660254037844387076, 1.000000000000000000, 0.8660254037844387076, 1.000000000000000000, 0.8660254037844387076, 1.000000000000000000, 0.8660254037844387076, 1.000000000000000000, 0.8660254037844387076, 1.000000000000000000, 0.8660254037844387076, 1.000000000000000000, 0.8660254037844387076, 1.000000000000000000, 0.8660254037844387076, 1.000000000000000000, 0.8660254037844387076, 1.000000000000000000, 0.8660254037844387076, 1.000000000000000000, 0.8660254037844387076, 1.000000000000000000, 0.8660254037844387076, 1.000000000000000000, 0.8660254037844387076, 1.000000000000000000, 0.8660254037844387076, 1.000000000000000000, 0.8660254037844387076, 1.000000000000000000, 0.8660254037844387076, 1.000000000000000000, 0.8660254037844387076, 1.000000000000000000, 0.8660254037844387076, 1.000000000000000000, 0.8660254037844387076, 1.000000000000000000, 0.8660254037844387076, 1.000000000000000000, 0.8660254037844387076, 1.000000000000000000, 0.8660254037844387076, 1.000000000000000000, 0.8660254037844387076, 1.000000000000000000, 0.8660254037844387076, 1.000000000000000000, 0.8660254037844387076, 1.000000000000000000, 0.8660254037844387076, 1.000000000000000000, 0.8660254037844387076, 1.000000000000000000, 0.8660254037844387076, 1.000000000000000000, 0.8660254037844387076, 1.000000000000000000, 0.8660254037844387076, 1.000000000000000000, 0.8660254037844387076, 1.000000000000000000, 0.8660254037844387076, 1.000000000000000000, 0.8660254037844387076, 1.000000000000000000, 0.8660254037844387076, 1.000000000000000000, 0.8660254037844387076, 1.000000000000000000, 0.8660254037844387076, 1.000000000000000000, 0.8660254037844387076, 1.000000000000000000, 0.8660254037844387076, 1.000000000000000000, 0.8660254037844387076, 1.000000000000000000, 0.8660254037844387076, 1.000000000000000000, 0.8660254037844387076, 1.000000000000000000, 0.8660254037844387076, 1.000000000000000000, 0.8660254037844387076, 1.000000000000000000, 0.8660254037844387076, 1.000000000000000000, 0.8660254037844387076, 1.000000000000000000, 0.8660254037844387076, 1.000000000000000000, 0.8660254037844387076, 1.000000000000000000, 0.8660254037844387076, 1.000000000000000000, 0.8660254037844387076, 1.000000000000000000, 0.8660254037844387076, 1.000000000000000000, 0.8660254037844387076, 1.000000000000000000, 0.8660254037844387076, 1.000000000000000000, 0.8660254037844387076, 1.000000000000000000, 0.8660254037844387076, 1.000000000000000000, 0.8660254037844387076, 1.000000000000000000, 0.8660254037844387076, 1.000000000000000000, 0.8660254037844387076, 1.000000000000000000, 0.8660254037844387076, 1.000000000000000000, 0.8660254037844387076, 1.000000000000000000, 0.8660254037844387076, 1.000000000000000000, 0.8660254037844387076, 1.000000000000000000, 0.8660254037844387076, 1.000000000000000000, 0.8660254037844387076, 1.000000000000000000, 0.8660254037844387076, 1.000000000000000000, 0.8660254037844387076, 1.000000000000000000, 0.8660254037844387076, 1.000000000000000000, 0.8660254037844387076, 1.000000000000000000, 0.8660254037844387076, 1.000000000000000000, 0.8660254037844387076, 1.000000000000000000, 0.8660254037844387076, 1.000000000000000000, 0.8660254037844387076, 1.000000000000000000, 0.8660254037844387076, 1.000000000000000000, 0.8660254037844387076, 1.000000000000000000, 0.8660254037844387076, 1.000000000000000000, 0.8660254037844387076, 1.000000000000000000, 0.8660254037844387076, 1.000000000000000000, 0.8660254037844387076, 1.000000000000000000, 0.8660254037844387076, 1.000000000000000000, 0.8660254037844387076, 1.000000000000000000, 0.8660254037844387076, 1.000000000000000000, 0.8660254037844387076, 1.000000000000000000, 0.8660254037844387076, 1.000000000000000000, 0.8660254037844387076, 1.000000000000000000, 0.8660254037844387076, 1.000000000000000000, 0.8660254037844387076, 1.000000000000000000, 0.8660254037844387076, 1.000000000000000000, 0.8660254037844387076, 1.000000000000000000, 0.8660254037844387076, 1.000000000000000000, 0.8660254037844387076, 1.000000000000000000, 0.8660254037844387076, 1.000000000000000000, 0.8660254037844387076, 1.000000000000000000, 0.8660254037844387076, 1.000000000000000000, 0.8660254037844387076, 1.000000000000000000, 0.8660254037844387076, 1.000000000000000000, 0.8660254037844387076, 1.000000000000000000, 0.8660254037844387076, 1.000000000000000000, 0.8660254037844387076, 1.000000000000000000, 0.8660254037844387076, 1.000000000000000000, 0.8660254037844387076, 1.000000000000000000, 0.8660254037844387076, 1.000000000000000000, 0.8660254037844387076, 1.000000000000000000) ) ) 
 REPRESENTATION_ITEM ( '' )  SURFACE ( )  );
#175965 = CARTESIAN_POINT ( 'NONE',  ( 2.541538742049511246, 1.893869637037654208, -0.8368498079355383146 ) ) ;
#175966 = CARTESIAN_POINT ( 'NONE',  ( 4.029797971759831121, 5.724516938518342535, -1.599625672291255185 ) ) ;
#175967 = CARTESIAN_POINT ( 'NONE',  ( -3.355169270512988773E-14, 1.234375000341463968, 1.570758158831764062 ) ) ;
#175968 = CARTESIAN_POINT ( 'NONE',  ( 5.127636373287420390, -0.3106611864900838960, 2.097473367668806876 ) ) ;
#175969 = CARTESIAN_POINT ( 'NONE',  ( 0.9614038661405551744, 0.3767496340168969837, -1.889141571593662805 ) ) ;
#175970 = EDGE_LOOP ( 'NONE', ( #48232, #75401, #82850, #201444, #175206 ) ) ;
#175971 = CARTESIAN_POINT ( 'NONE',  ( -3.630551273409382329, 7.457669928944732796, 0.7998128361456352531 ) ) ;
#175972 = CARTESIAN_POINT ( 'NONE',  ( 9.772729797352075920, 10.29593960653257234, -0.7998128361456281477 ) ) ;
#175973 = CARTESIAN_POINT ( 'NONE',  ( 6.509323147892504657, 6.766834225395614411, 0.000000000000000000 ) ) ;
#175974 = CARTESIAN_POINT ( 'NONE',  ( 0.000000000000000000, -1.443749999044082966, -4.012584370867899430 ) ) ;
#175975 = AXIS2_PLACEMENT_3D ( 'NONE', #148812, #169325, #101111 ) ;
#175976 = CARTESIAN_POINT ( 'NONE',  ( -6.078132937628113908, 5.985576603521232109, 1.040834085586084257E-14 ) ) ;
#175977 = CARTESIAN_POINT ( 'NONE',  ( -0.2044637419536878831, -0.1604900674421188000, -2.186121014245277383 ) ) ;
#175978 = CARTESIAN_POINT ( 'NONE',  ( 1.958176110230916755, 2.100372442369624171, -0.1540336313638566157 ) ) ;
#175979 = CARTESIAN_POINT ( 'NONE',  ( -3.793249116773374396, 7.647484079536056356, 0.7998128361456352531 ) ) ;
#175980 = CARTESIAN_POINT ( 'NONE',  ( 7.618792255875527886, 10.97600916757510170, 1.199719254218460707 ) ) ;
#175981 = CARTESIAN_POINT ( 'NONE',  ( 6.877813048773076865, -1.805165420234026818, 0.4518952398848713470 ) ) ;
#175982 = CARTESIAN_POINT ( 'NONE',  ( 8.599949509769960088, 8.927695937686774386, 1.040834085586084257E-14 ) ) ;
#175983 = CARTESIAN_POINT ( 'NONE',  ( -0.4153311931459208184, 3.850000000000006306, -0.4999999999999961142 ) ) ;
#175984 = CARTESIAN_POINT ( 'NONE',  ( -3.634467696915153034, 6.397906858779740524, 1.199719254218452935 ) ) ;
#175985 = CARTESIAN_POINT ( 'NONE',  ( -9.327646496521984076, 11.90534021740758064, -1.443375672974059665 ) ) ;
#175986 = CARTESIAN_POINT ( 'NONE',  ( 0.1234922912959918878, 1.848187084301698757, 1.039613981531524400 ) ) ;
#175987 = CYLINDRICAL_SURFACE ( 'NONE', #22697, 0.7500000000000011102 ) ;
#175989 = CARTESIAN_POINT ( 'NONE',  ( 1.820681965693775162, -1.389665069980907441, 1.385087887197037571 ) ) ;
#175988 = CARTESIAN_POINT ( 'NONE',  ( 0.6124999999999793943, -0.4166666666666346552, 1.060881119635891157 ) ) ;
#175990 = CARTESIAN_POINT ( 'NONE',  ( 0.9366540776252421097, 2.129889809250965271, 0.3686189752144660714 ) ) ;
#175992 = CARTESIAN_POINT ( 'NONE',  ( -5.747036748294815922, 6.247280920146251582, 1.064921034751656226 ) ) ;
#175991 = CARTESIAN_POINT ( 'NONE',  ( -4.925354943514475003, 8.968274210734028529, 0.000000000000000000 ) ) ;
#175993 = CARTESIAN_POINT ( 'NONE',  ( 0.6823417656249882723, 1.676041667008083769, -1.181850606188749264 ) ) ;
#175994 = CARTESIAN_POINT ( 'NONE',  ( 3.075252150474018009, 1.257817891742564642, -1.193625562640305615 ) ) ;
#175995 = CARTESIAN_POINT ( 'NONE',  ( 1.991783209624857331, -0.4627563367010344986, -1.677588981799936541 ) ) ;
#175996 = AXIS2_PLACEMENT_3D ( 'NONE', #101972, #90007, #75868 ) ;
#175997 = CARTESIAN_POINT ( 'NONE',  ( 6.073689629242148058, 8.109057205581079231, -1.443375672974057666 ) ) ;
#175998 = CARTESIAN_POINT ( 'NONE',  ( -11.50715376448619764, 7.744667295756731740, 4.958460396591308772 ) ) ;
#175999 = EDGE_CURVE ( 'NONE', #24518, #8935, #64844, .T. ) ;
#176000 = CARTESIAN_POINT ( 'NONE',  ( 1.827499746633702182, -1.427720486614523221, 1.423741782973136694 ) ) ;
#176001 = CARTESIAN_POINT ( 'NONE',  ( 6.925078400183550364, 3.684205305355064297, 2.658256427561227486 ) ) ;
#176002 = CARTESIAN_POINT ( 'NONE',  ( -4.797606254389363833, 6.690569611577942943, 1.599625672291263179 ) ) ;
#176003 = CARTESIAN_POINT ( 'NONE',  ( 0.7781230576423033840, -1.097119503657293382, 1.637799472441689996 ) ) ;
#176005 = CARTESIAN_POINT ( 'NONE',  ( -5.397554552016258889, 7.390509292142662723, 1.443375672974058777 ) ) ;
#176004 = CARTESIAN_POINT ( 'NONE',  ( 6.082274476537278041, 0.9889857280602430967, 1.636697341158253272 ) ) ;
#176006 = CARTESIAN_POINT ( 'NONE',  ( -5.221298554594238084, 8.145246509451649075, 1.082531754730549967 ) ) ;
#176007 = CARTESIAN_POINT ( 'NONE',  ( 6.387826650694035990, 7.481494509678370264, -1.199719254218452047 ) ) ;
#176008 = CARTESIAN_POINT ( 'NONE',  ( -5.921879234118920365, 10.13088588310589699, 0.000000000000000000 ) ) ;
#176009 = CARTESIAN_POINT ( 'NONE',  ( 1.277996545170931197, 1.989402420072207800, -0.3474319251903742467 ) ) ;
#176010 =( LENGTH_UNIT ( ) NAMED_UNIT ( * ) SI_UNIT ( .MILLI., .METRE. ) );
#176011 = CARTESIAN_POINT ( 'NONE',  ( 5.878008146920711496, 1.368277704907730374, 1.858044196986943675 ) ) ;
#176012 = CARTESIAN_POINT ( 'NONE',  ( 5.687936657224680559, -1.243353266631580523, -1.517579924814119074 ) ) ;
#176013 = EDGE_CURVE ( 'NONE', #87871, #117162, #170798, .T. ) ;
#176014 = CARTESIAN_POINT ( 'NONE',  ( 2.817183829107517745, -1.704460984269993817, -0.9711623693852902139 ) ) ;
#176015 = CARTESIAN_POINT ( 'NONE',  ( 7.639129486296027061, 10.99973593639901814, 1.199719254218460707 ) ) ;
#176016 = CARTESIAN_POINT ( 'NONE',  ( 0.5103889644224939293, -1.913802852362624929, 0.6352017490645139874 ) ) ;
#176017 = ORIENTED_EDGE ( 'NONE', *, *, #17814, .F. ) ;
#176018 = CARTESIAN_POINT ( 'NONE',  ( 1.745463160119866686, 0.3564436455325488695, -2.086969855494016368 ) ) ;
#176020 = CARTESIAN_POINT ( 'NONE',  ( -8.694856585065634746, 9.038420858865048757, 0.7998128361456462443 ) ) ;
#176019 = CARTESIAN_POINT ( 'NONE',  ( -4.569261463005423352, 5.289558780716470565, -1.199719254218446718 ) ) ;
#176021 = CARTESIAN_POINT ( 'NONE',  ( 2.466542765887615563, 0.09048117372523720170, -1.839033023284454060 ) ) ;
#176022 = VERTEX_POINT ( 'NONE', #150281 ) ;
#176023 = CARTESIAN_POINT ( 'NONE',  ( 11.62784165634802136, 8.211123330874524839, -2.995123467788005200 ) ) ;
#176024 = CARTESIAN_POINT ( 'NONE',  ( 3.111701630267147412, 1.674174984267240429, 1.301503359413098249 ) ) ;
#176025 = CARTESIAN_POINT ( 'NONE',  ( 1.499999999999987121, 3.827083334016153415, -0.8660254037844323793 ) ) ;
#176026 = CARTESIAN_POINT ( 'NONE',  ( 7.721532178182734185, 8.967207948423393304, 1.199719254218462483 ) ) ;
#176027 = CARTESIAN_POINT ( 'NONE',  ( 5.826972158823246595, 10.02016096192762085, -0.7998128361456481317 ) ) ;
#176028 = CARTESIAN_POINT ( 'NONE',  ( 2.776696059289599283, -1.970994871289712069, -0.6015693623636628740 ) ) ;
#176030 = CARTESIAN_POINT ( 'NONE',  ( 0.01093749962182561514, -1.805946196879631094, 0.3578947576599255664 ) ) ;
#176029 = CARTESIAN_POINT ( 'NONE',  ( -6.367525699912501835, 10.58053041653993098, -0.7998128361456291469 ) ) ;
#176031 = CARTESIAN_POINT ( 'NONE',  ( -1.001543065824772872E-14, 4.321875000341417916, 1.575800808251672791 ) ) ;
#176032 = CARTESIAN_POINT ( 'NONE',  ( -0.02244404828160087226, 0.2256878572204877031, -2.222431841814066278 ) ) ;
#176033 = CARTESIAN_POINT ( 'NONE',  ( 1.354875605471919542, 3.923167251739089423, 0.6436714776511552882 ) ) ;
#176034 = VECTOR ( 'NONE', #185724, 1000.000000000000000 ) ;
#176035 = CARTESIAN_POINT ( 'NONE',  ( 0.06543086261080394150, -1.973449318085427340, -0.9880335165917543128 ) ) ;
#176036 = CARTESIAN_POINT ( 'NONE',  ( 2.442968603456824095, 0.4936193734879111283, 2.207763252559187261 ) ) ;
#176037 = CARTESIAN_POINT ( 'NONE',  ( -9.002250809794006159, 10.56534270192358704, -1.082531754730543971 ) ) ;
#176038 = CARTESIAN_POINT ( 'NONE',  ( 2.970771795020191064, -1.368765343908146415, 1.186782720094860855 ) ) ;
#176039 = CARTESIAN_POINT ( 'NONE',  ( 3.573361294032686430, 1.391295603808204051, 1.317194196901736669 ) ) ;
#176040 = CARTESIAN_POINT ( 'NONE',  ( 3.807136610393092813, -1.694265131726957252, 1.189645435975445809 ) ) ;
#176041 = CARTESIAN_POINT ( 'NONE',  ( 1.364683531249986537, 2.217708333674751398, -0.7879004041258239610 ) ) ;
#176042 = CARTESIAN_POINT ( 'NONE',  ( 2.325019196037684477, -0.001775356835979901692, 1.971640592446997298 ) ) ;
#176043 = CARTESIAN_POINT ( 'NONE',  ( 6.621714856310891406, -1.867994803139013005, 0.4708039761674199797 ) ) ;
#176044 = CARTESIAN_POINT ( 'NONE',  ( 2.500682550815761740, 1.503739811390795378, -1.112508705057350999 ) ) ;
#176046 = CARTESIAN_POINT ( 'NONE',  ( 4.595841027163160675, 8.489102040997540399, 0.04885061651019838302 ) ) ;
#176045 = CARTESIAN_POINT ( 'NONE',  ( 2.790017796326722532, 1.632578265707486098, 1.631241332076227346 ) ) ;
#176047 = CARTESIAN_POINT ( 'NONE',  ( 2.629178708315405455, 0.09452080204645990635, -1.858793618116144186 ) ) ;
#176048 = CARTESIAN_POINT ( 'NONE',  ( -1.201851678989727383E-14, 2.821875000341418804, 1.575800808251672791 ) ) ;
#176049 = CARTESIAN_POINT ( 'NONE',  ( 6.391093295415360309, 0.1985076180841711668, 2.053089703019762791 ) ) ;
#176050 = CARTESIAN_POINT ( 'NONE',  ( -5.786632634934295361, 5.645492917045106473, 0.7998128361456341429 ) ) ;
#176051 = CARTESIAN_POINT ( 'NONE',  ( 6.612626235163189925, 8.737816579155630592, -1.599625672291262513 ) ) ;
#176052 = CARTESIAN_POINT ( 'NONE',  ( -1.446922511646519416, 3.374038201079560650, 0.4002501213623008702 ) ) ;
#176053 = CARTESIAN_POINT ( 'NONE',  ( 0.9968619785027620361, -0.5136065205212798634, -2.042351051948914531 ) ) ;
#176054 = CARTESIAN_POINT ( 'NONE',  ( 1.364683531249988535, 3.717708333674750953, -0.7879004041258239610 ) ) ;
#176055 = CARTESIAN_POINT ( 'NONE',  ( 5.747404748698970778, -1.700087083557629386, -1.334863535946126500 ) ) ;
#176056 = CARTESIAN_POINT ( 'NONE',  ( 0.1584709747761771925, 2.014675524564497167, 0.1441611394625528231 ) ) ;
#176057 = CARTESIAN_POINT ( 'NONE',  ( 1.364683531249984538, -1.094791666325247936, -0.7879004041258309554 ) ) ;
#176058 = CARTESIAN_POINT ( 'NONE',  ( -5.097502569058225852, 5.049433873430440478, -0.7216878364870207285 ) ) ;
#176059 = EDGE_CURVE ( 'NONE', #26620, #7055, #11411, .T. ) ;
#176062 = CARTESIAN_POINT ( 'NONE',  ( 4.704316114261903436, 4.590716342834741504, 1.214306433183764966E-14 ) ) ;
#176061 = CARTESIAN_POINT ( 'NONE',  ( -3.285556943749998737, -0.7802083328553744979, 1.896917185911908499 ) ) ;
#176060 = CARTESIAN_POINT ( 'NONE',  ( 5.365994935958575240, 9.482354201918870018, 0.7998128361456341429 ) ) ;
#176063 = CARTESIAN_POINT ( 'NONE',  ( -3.383641855062333281, 6.105276709951447778, -1.199719254218452047 ) ) ;
#176064 = CARTESIAN_POINT ( 'NONE',  ( 4.329314735043091389, -1.561880650076686861, -1.275557594027726394 ) ) ;
#176066 = CARTESIAN_POINT ( 'NONE',  ( -5.573810548549546162, 9.516879716700865188, 0.7216878364870267237 ) ) ;
#176065 = CARTESIAN_POINT ( 'NONE',  ( -8.134528978519403708, 11.47373899403920205, 1.082531754730549967 ) ) ;
#176068 = CARTESIAN_POINT ( 'NONE',  ( -8.012344526598182026E-15, 10.04687500034140335, -1.575800808251669460 ) ) ;
#176067 = CARTESIAN_POINT ( 'NONE',  ( 5.875883356151954118, 1.283970044810868849, 1.738936680771227206 ) ) ;
#176069 = DIRECTION ( 'NONE',  ( -1.276756478318932585E-15, 1.000000000000000000, -1.665334536937738262E-16 ) ) ;
#176070 = CARTESIAN_POINT ( 'NONE',  ( -11.31484017231561445, 6.389126039234806598, 4.001117297664503525 ) ) ;
#176072 = CARTESIAN_POINT ( 'NONE',  ( -0.07089544441234334193, -1.481030113823898375, -1.214736957437832832 ) ) ;
#176071 = CARTESIAN_POINT ( 'NONE',  ( -5.978782553502159480, 8.958701498185728695, 1.082531754730548412 ) ) ;
#176073 = CARTESIAN_POINT ( 'NONE',  ( 0.6823417656249899377, 1.155208333674752286, 1.181850606188755259 ) ) ;
#176074 = CARTESIAN_POINT ( 'NONE',  ( 0.008622031262369225790, 14.55347103577515000, 11.95585889282743253 ) ) ;
#176075 = DIRECTION ( 'NONE',  ( 0.000000000000000000, 1.000000000000000000, 0.000000000000000000 ) ) ;
#176076 = CARTESIAN_POINT ( 'NONE',  ( 2.297083607218278978, 1.332544580598886252, 1.095227982430951208 ) ) ;
#176077 = CARTESIAN_POINT ( 'NONE',  ( 8.154303043976348420, 8.478051404252736845, 0.7998128361456281477 ) ) ;
#176078 = CARTESIAN_POINT ( 'NONE',  ( 4.667750024854814050, 8.667735138964429709, -0.7998128361456381397 ) ) ;
#176079 = CARTESIAN_POINT ( 'NONE',  ( -1.364683531250014514, -0.9489583329919112353, -0.7879004041258359514 ) ) ;
#176080 = CARTESIAN_POINT ( 'NONE',  ( 0.5086179708909451813, 1.535567861042252957, 0.8796773807029609760 ) ) ;
#176081 = CARTESIAN_POINT ( 'NONE',  ( 2.174478567003877316, 0.8628565524405201748, 1.818940509527650295 ) ) ;
#176082 = CARTESIAN_POINT ( 'NONE',  ( 4.189106276498237413, 3.989638198777126110, -0.7216878364870188411 ) ) ;
#176083 = CARTESIAN_POINT ( 'NONE',  ( 3.803933094734159415, -0.6430795383850876901, 2.110982628114480786 ) ) ;
#176084 = CARTESIAN_POINT ( 'NONE',  ( 5.436453865645980876, -1.212139536413152197, 1.801006579369943239 ) ) ;
#176085 = ORIENTED_EDGE ( 'NONE', *, *, #177186, .F. ) ;
#176086 = CARTESIAN_POINT ( 'NONE',  ( 1.499999999999985123, -0.4541666666666469010, -0.8660254037844323793 ) ) ;
#176087 = CARTESIAN_POINT ( 'NONE',  ( 8.731087737076324018, 9.288616569451617622, 1.040834085586084257E-14 ) ) ;
#176089 = CARTESIAN_POINT ( 'NONE',  ( 2.689077551358230789, 1.704951624378052033, 1.076298511635757738 ) ) ;
#176088 = CARTESIAN_POINT ( 'NONE',  ( 3.492942606646631809, -2.044086983709763050, -0.5638711869686771072 ) ) ;
#176091 = ORIENTED_EDGE ( 'NONE', *, *, #184288, .F. ) ;
#176090 = CARTESIAN_POINT ( 'NONE',  ( 3.586021145937230870, 1.010873021915110748, 1.503094931805592394 ) ) ;
#176092 = CARTESIAN_POINT ( 'NONE',  ( 4.864343252252968597, 8.897093904262280972, 0.000000000000000000 ) ) ;
#176093 = ORIENTED_EDGE ( 'NONE', *, *, #12933, .T. ) ;
#176094 = CARTESIAN_POINT ( 'NONE',  ( 0.2681426532152464959, -1.225442487749365483, 1.413462724991432218 ) ) ;
#176095 = CARTESIAN_POINT ( 'NONE',  ( 4.690231075323689325, 7.559354456931247412, 1.199719254218462483 ) ) ;
#176096 = CARTESIAN_POINT ( 'NONE',  ( 6.147073579019600054, -1.539581890156189292, 0.9809480439507823890 ) ) ;
#176098 = CARTESIAN_POINT ( 'NONE',  ( 1.956118367686721538, -1.175378340988470827, 1.512710158094223933 ) ) ;
#176097 = CARTESIAN_POINT ( 'NONE',  ( -3.846762897975357198, 5.510976019103107859, -1.599625672291256295 ) ) ;
#176099 =( LENGTH_UNIT ( ) NAMED_UNIT ( * ) SI_UNIT ( .MILLI., .METRE. ) );
#176100 = CARTESIAN_POINT ( 'NONE',  ( 4.255647627037052709E-16, 0.5000000000000004441, 3.475000000000000089 ) ) ;
#176101 = CARTESIAN_POINT ( 'NONE',  ( -1.364683531250012516, 1.592708333674756727, 0.7879004041258379498 ) ) ;
#176102 = CARTESIAN_POINT ( 'NONE',  ( 0.000000000000000000, 8.999999999999998224, 0.000000000000000000 ) ) ;
#176103 = CARTESIAN_POINT ( 'NONE',  ( -7.472515219426274946, 11.86968485597268064, 0.000000000000000000 ) ) ;
#176104 = EDGE_CURVE ( 'NONE', #85209, #69840, #198181, .T. ) ;
#176105 = CARTESIAN_POINT ( 'NONE',  ( 5.647404790089923132, -1.701416311724871067, -1.333359258283283166 ) ) ;
#176106 = CARTESIAN_POINT ( 'NONE',  ( -5.817857314039913241, 5.960124085900898372, 0.000000000000000000 ) ) ;
#176107 = CARTESIAN_POINT ( 'NONE',  ( -5.725286006720766707, 9.901527117808042178, 0.7998128361456291469 ) ) ;
#176108 = CARTESIAN_POINT ( 'NONE',  ( 2.883181758455736432, -1.960942133159260692, -0.8077274430827171559 ) ) ;
#176110 = CARTESIAN_POINT ( 'NONE',  ( -10.61989522411177944, 7.619981102720494448, -4.513857952992439415 ) ) ;
#176109 = CARTESIAN_POINT ( 'NONE',  ( -4.858589159720606787, 4.879621185664173133, 0.4920435892086290064 ) ) ;
#176111 = CARTESIAN_POINT ( 'NONE',  ( 4.130118527232538028, 1.057347662480428108, -1.663647784685320818 ) ) ;
#176112 = CARTESIAN_POINT ( 'NONE',  ( -0.2047996464942871964, -0.1441562275304847374, -1.980932652848297115 ) ) ;
#176113 = EDGE_LOOP ( 'NONE', ( #161460, #38991, #150283, #75158 ) ) ;
#176114 = CARTESIAN_POINT ( 'NONE',  ( 5.665271214873143890, 1.955333520279872506, -0.8127364881663766694 ) ) ;
#176115 = ADVANCED_FACE ( 'NONE', ( #188090 ), #50649, .T. ) ;
#176116 = CARTESIAN_POINT ( 'NONE',  ( 0.5024991115675537801, 2.064720838319131779, 0.1538615064654233477 ) ) ;
#176117 = CARTESIAN_POINT ( 'NONE',  ( 2.958853767740171392, 0.2844919188511252917, -1.920881014358867489 ) ) ;
#176118 = ORIENTED_EDGE ( 'NONE', *, *, #213502, .F. ) ;
#176119 = CARTESIAN_POINT ( 'NONE',  ( -4.247512733928926920, 7.321623457166534621, -0.8935899926269799121 ) ) ;
#176120 = CARTESIAN_POINT ( 'NONE',  ( 6.200875153403774043, 8.327716660428123419, -1.599625672291283607 ) ) ;
#176122 = CARTESIAN_POINT ( 'NONE',  ( 6.169123589417988995, 7.156064594864501416, -1.199719254218445830 ) ) ;
#176121 = CARTESIAN_POINT ( 'NONE',  ( 4.083990600187762610, -2.067889708199427190, -0.3066597852425279047 ) ) ;
#176123 = CARTESIAN_POINT ( 'NONE',  ( 5.519577934094864524, 5.612131475965050242, 0.7216878364870328300 ) ) ;
#176125 = VERTEX_POINT ( 'NONE', #121057 ) ;
#176124 = CARTESIAN_POINT ( 'NONE',  ( 0.2756360753965527155, 1.792041154956749871, -0.2637626551888968551 ) ) ;
#176126 = CARTESIAN_POINT ( 'NONE',  ( 5.795608111622330583, 1.668732747960173235, 1.444295198399044855 ) ) ;
#176127 = AXIS2_PLACEMENT_3D ( 'NONE', #191951, #162697, #59841 ) ;
#176128 = CARTESIAN_POINT ( 'NONE',  ( -0.01400375819625959001, -6.304807775344903220, -11.00039779441144461 ) ) ;
#176129 = CARTESIAN_POINT ( 'NONE',  ( 2.925073249431627165, 2.077443920948469192, 0.7446974470129497092 ) ) ;
#176130 = CARTESIAN_POINT ( 'NONE',  ( 8.796542737168120851, 9.157054702984622097, -0.7998128361456211532 ) ) ;
#176131 = CYLINDRICAL_SURFACE ( 'NONE', #78810, 0.08000000000000041800 ) ;
#176132 = CARTESIAN_POINT ( 'NONE',  ( 2.174333686202088334, 0.8191313854410250395, 1.728107290330855639 ) ) ;
#176133 = CARTESIAN_POINT ( 'NONE',  ( 9.694243528971124846, 11.26870452434320491, 1.199719254218450271 ) ) ;
#176134 = CARTESIAN_POINT ( 'NONE',  ( 5.863751307568212390, -0.5067217619753560109, 2.007263066363853987 ) ) ;
#176136 = CARTESIAN_POINT ( 'NONE',  ( 3.274459119871219848, -1.289031633699176949, 1.735169069618908821 ) ) ;
#176135 = CARTESIAN_POINT ( 'NONE',  ( -1.123270288249902160, 2.800000000000024691, 0.7750000000000117906 ) ) ;
#176137 = CARTESIAN_POINT ( 'NONE',  ( 4.528971853086540378, -2.003544689622422936, 0.8885388601788182239 ) ) ;
#176138 = ORIENTED_EDGE ( 'NONE', *, *, #44421, .F. ) ;
#176139 = CARTESIAN_POINT ( 'NONE',  ( 9.561524646135536543, 12.17819805862340310, -1.599625672291262513 ) ) ;
#176140 = CARTESIAN_POINT ( 'NONE',  ( 0.7500000000000006661, 12.91666666666666607, -1.299038105676657340 ) ) ;
#176141 = AXIS2_PLACEMENT_3D ( 'NONE', #100492, #82101, #183873 ) ;
#176142 = CARTESIAN_POINT ( 'NONE',  ( 3.562760505341037831, 7.378580699531681830, -1.734723475976807094E-15 ) ) ;
#176143 = CARTESIAN_POINT ( 'NONE',  ( 1.642778471875001811, -2.180208332855374742, 2.845375778867859751 ) ) ;
#176144 = CARTESIAN_POINT ( 'NONE',  ( -2.993318053567081360, 6.714231172462041819, 0.000000000000000000 ) ) ;
#176145 = ADVANCED_FACE ( 'NONE', ( #187024 ), #14591, .T. ) ;
#176146 = CARTESIAN_POINT ( 'NONE',  ( -8.839552966430007430, 11.33589776563360019, -1.443375672974059665 ) ) ;
#176147 = CARTESIAN_POINT ( 'NONE',  ( 5.682802662783380754, 6.658966523782627434, 1.199719254218452935 ) ) ;
#176148 = CARTESIAN_POINT ( 'NONE',  ( 5.436411051413860385, -1.154718516627372127, 1.718110687276501958 ) ) ;
#176149 = CARTESIAN_POINT ( 'NONE',  ( 4.336495953379083446, 1.889596944713485049, 0.3744603196194126182 ) ) ;
#176150 = CARTESIAN_POINT ( 'NONE',  ( 6.345324880664913181, 0.3618513607092630480, -2.085922816363374288 ) ) ;
#176151 = CARTESIAN_POINT ( 'NONE',  ( -4.904003162269379601, 4.835767286957110223, -0.1818790228878807702 ) ) ;
#176152 = CARTESIAN_POINT ( 'NONE',  ( 5.066996723205273057, 6.934582148538044777, 1.599625672291267398 ) ) ;
#176153 = CARTESIAN_POINT ( 'NONE',  ( -4.213209511989692402, 3.978029986984279898, -0.5398075284353744951 ) ) ;
#176154 = CARTESIAN_POINT ( 'NONE',  ( 4.645333151331359822, 1.761124666023382579, -0.8816396696852289994 ) ) ;
#176155 = CARTESIAN_POINT ( 'NONE',  ( 0.7443833103580773658, 0.6396484562771963533, 2.096019810003430184 ) ) ;
#176156 = CARTESIAN_POINT ( 'NONE',  ( 4.547361323050268744, -1.413013347330991598, -1.156083184146582177 ) ) ;
#176157 = CARTESIAN_POINT ( 'NONE',  ( 5.234856708652215751, 9.121433570154021453, 0.7216878364870317197 ) ) ;
#176158 = CARTESIAN_POINT ( 'NONE',  ( 4.500943809612556024, 4.353448654077163305, 1.214306433183764966E-14 ) ) ;
#176159 = CARTESIAN_POINT ( 'NONE',  ( -5.769876891067536206, 8.889217585290882795, 1.199719254218454489 ) ) ;
#176160 = CARTESIAN_POINT ( 'NONE',  ( 4.420840606507738357, 7.315341919971147355, 1.199719254218451159 ) ) ;
#176161 = ORIENTED_EDGE ( 'NONE', *, *, #124205, .T. ) ;
#176163 = CARTESIAN_POINT ( 'NONE',  ( 5.291276029577359985, -0.05376236717486576611, -2.012660120947160181 ) ) ;
#176162 = CARTESIAN_POINT ( 'NONE',  ( 2.682954136603598272, 1.303717545168959990, 1.300458928786947688 ) ) ;
#176164 = CARTESIAN_POINT ( 'NONE',  ( 1.388484499181727561, -0.05552238045265603383, 2.297868740670248044 ) ) ;
#176165 = CARTESIAN_POINT ( 'NONE',  ( 5.752778578519474273, -0.4731148833870613690, -1.903749215227706015 ) ) ;
#176166 = CARTESIAN_POINT ( 'NONE',  ( -7.040761844198392794, 7.108643661186573759, -0.7998128361456291469 ) ) ;
#176167 = LINE ( 'NONE', #99971, #57218 ) ;
#176168 = CARTESIAN_POINT ( 'NONE',  ( -4.959585264500673496, 4.680604318205876524, 1.214306433183764966E-14 ) ) ;
#176169 = CARTESIAN_POINT ( 'NONE',  ( 0.9595327444568906294, 1.691550050060253829, 1.193477315110213599 ) ) ;
#176170 = CARTESIAN_POINT ( 'NONE',  ( -3.772911886352873445, 7.623757310712140800, 0.7998128361456352531 ) ) ;
#176172 = CARTESIAN_POINT ( 'NONE',  ( 0.1978467685152424937, -1.870139902624564865, -0.05068021481659244765 ) ) ;
#176171 = CARTESIAN_POINT ( 'NONE',  ( 1.048509228467583876, -1.645825662996244443, 1.289236127856315139 ) ) ;
#176173 = CARTESIAN_POINT ( 'NONE',  ( 0.5631007116328431428, 7.823254984196703177, -1.919102855466201518 ) ) ;
#176174 = CARTESIAN_POINT ( 'NONE',  ( -1.201851678989727383E-14, 3.384375000341421025, 1.575800808251672791 ) ) ;
#176175 = CARTESIAN_POINT ( 'NONE',  ( 1.628031597684251208, 0.1703553616784689029, 1.732092769550299227 ) ) ;
#176176 = CARTESIAN_POINT ( 'NONE',  ( 3.974511587100456822, 7.788680618259193444, 1.040834085586084257E-14 ) ) ;
#176178 = CARTESIAN_POINT ( 'NONE',  ( 1.528885273045258231, 8.694317336386671258, 2.518424357262873059 ) ) ;
#176177 = DIRECTION ( 'NONE',  ( 3.330669073875479482E-16, -3.330669073875479482E-16, -1.000000000000000000 ) ) ;
#176179 = CARTESIAN_POINT ( 'NONE',  ( 2.701417116451056533, -0.5414251306648624196, 1.637772108618321454 ) ) ;
#176180 = CARTESIAN_POINT ( 'NONE',  ( 2.208753784402537335, 1.959192758111829136, 0.9821998110004714899 ) ) ;
#176181 = CARTESIAN_POINT ( 'NONE',  ( 0.1055823559395060729, -0.08803060671099156853, 1.732021048141555220 ) ) ;
#176182 = CARTESIAN_POINT ( 'NONE',  ( 4.653060005753134831, -1.773635849817876586, 1.313014255023836618 ) ) ;
#176183 = CARTESIAN_POINT ( 'NONE',  ( -10.41986968326957808, 5.020773655391575829, -5.279272669861445166 ) ) ;
#176184 = CARTESIAN_POINT ( 'NONE',  ( 2.676840970354518845, 1.421027823260514911, -1.641450307487320792 ) ) ;
#176185 = CARTESIAN_POINT ( 'NONE',  ( 0.8908993799596062191, 1.611356928563783208, -0.8583080905386344384 ) ) ;
#176186 = CARTESIAN_POINT ( 'NONE',  ( 2.993478482863177081, -0.4084587893785693868, 2.077413892881809776 ) ) ;
#176187 = CARTESIAN_POINT ( 'NONE',  ( 6.639320575229259447, 2.978120323461688201, 2.350396677589302374 ) ) ;
#176188 = EDGE_LOOP ( 'NONE', ( #58649, #12983, #39778, #118078, #124552, #115402 ) ) ;
#176190 = CARTESIAN_POINT ( 'NONE',  ( -1.402160292154681736E-14, 1.009375000341417916, -1.575800808251659024 ) ) ;
#176189 = CARTESIAN_POINT ( 'NONE',  ( 3.228363206396630769, 2.236961789864226002, 0.5003539455325100027 ) ) ;
#176191 = CARTESIAN_POINT ( 'NONE',  ( -7.834948825496938163, -5.907420853759296264, -7.720982897393569466 ) ) ;
#176192 = CARTESIAN_POINT ( 'NONE',  ( 5.054492339796319733, 4.791329239384148231, -0.7998128361456211532 ) ) ;
#176193 = CARTESIAN_POINT ( 'NONE',  ( 5.549557930969759134, -2.008940618436024117, 0.9481178722350207533 ) ) ;
#176194 = CARTESIAN_POINT ( 'NONE',  ( -5.558479791922849245, 9.428717490644563881, 0.7216878364870458196 ) ) ;
#176195 = CARTESIAN_POINT ( 'NONE',  ( 3.714570900464274850, 6.317121236308204324, 1.082531754730558626 ) ) ;
#176196 = CARTESIAN_POINT ( 'NONE',  ( -5.707619481228814351, 9.602713794834864203, -0.7216878364870207285 ) ) ;
#176197 = CARTESIAN_POINT ( 'NONE',  ( 4.773879485787624333, 4.742149952939897162, -0.7216878364870357165 ) ) ;
#176198 = VERTEX_POINT ( 'NONE', #94633 ) ;
#176199 = CARTESIAN_POINT ( 'NONE',  ( 3.902970337090125863, -1.038992709432768891, -1.728002613881730598 ) ) ;
#176201 = CARTESIAN_POINT ( 'NONE',  ( 1.639586372526161684, 1.907294469559306815, -0.7855861486642725655 ) ) ;
#176200 = CARTESIAN_POINT ( 'NONE',  ( 4.801558957534076022, 8.753569217098425170, 0.7998128361456462443 ) ) ;
#176202 = FACE_BOUND ( 'NONE', #88343, .T. ) ;
#176203 = CARTESIAN_POINT ( 'NONE',  ( 4.543390873910913896, 5.433615786718446472, 1.082531754730549078 ) ) ;
#176204 = CARTESIAN_POINT ( 'NONE',  ( 3.285556943750000514, -3.463541666188707957, 1.896917185911906500 ) ) ;
#176205 = CARTESIAN_POINT ( 'NONE',  ( 0.6823417656249917140, 5.342708333674749177, 1.181850606188765695 ) ) ;
#176206 = CARTESIAN_POINT ( 'NONE',  ( 4.910206770677443266, 1.512653250323254817, -1.585896273577400706 ) ) ;
#176207 = CARTESIAN_POINT ( 'NONE',  ( 2.725232599228684993, 2.001511357256777313, 0.2440295182731533341 ) ) ;
#176208 = CARTESIAN_POINT ( 'NONE',  ( 1.786409390178132162, 1.601450680722369846, -0.9084932335857234253 ) ) ;
#176209 = CARTESIAN_POINT ( 'NONE',  ( 7.470706336329915764, 8.674577799595093452, -1.199719254218441611 ) ) ;
#176210 = CARTESIAN_POINT ( 'NONE',  ( 6.299803673773761936, -0.6120917497752301761, 1.720027978493202436 ) ) ;
#176211 = CARTESIAN_POINT ( 'NONE',  ( 0.001177798100650446610, -2.252613640939280515, 0.4573402144308849615 ) ) ;
#176212 = CARTESIAN_POINT ( 'NONE',  ( -7.395082721250053837, 10.71501471051202614, -1.199719254218446718 ) ) ;
#176214 = CARTESIAN_POINT ( 'NONE',  ( -4.468294144155606773, 7.370704380560280100, 1.199719254218452935 ) ) ;
#176213 = CARTESIAN_POINT ( 'NONE',  ( 6.086863830973287648, -0.3249354738291005407, -2.238958312302678610 ) ) ;
#176215 = CARTESIAN_POINT ( 'NONE',  ( 1.436301726765435438, 1.036571610867568216, -1.833232669937171266 ) ) ;
#176216 = CARTESIAN_POINT ( 'NONE',  ( -4.762657100150483380, 8.778460060142702304, 0.000000000000000000 ) ) ;
#176217 = CARTESIAN_POINT ( 'NONE',  ( 7.670162217029129259, 9.971608557999250166, 1.599625672291281386 ) ) ;
#176218 = CARTESIAN_POINT ( 'NONE',  ( 6.821160681006781523, 9.051383109298340557, 1.443375672974063439 ) ) ;
#176219 = CARTESIAN_POINT ( 'NONE',  ( -7.446452682403657874, 9.710614100936176385, -1.599625672291263179 ) ) ;
#176220 = DIRECTION ( 'NONE',  ( -0.000000000000000000, -1.000000000000000000, -0.000000000000000000 ) ) ;
#176221 = CARTESIAN_POINT ( 'NONE',  ( 6.710922848640084482, 9.812865175846695820, -1.082531754730537976 ) ) ;
#176222 = CARTESIAN_POINT ( 'NONE',  ( 4.026354976812863917, 7.791716866330316904, -0.3671166487079768892 ) ) ;
#176223 = CARTESIAN_POINT ( 'NONE',  ( -8.297226821883391779, 11.66355314463053006, 1.082531754730549967 ) ) ;
#176225 = CARTESIAN_POINT ( 'NONE',  ( 3.375417215397161552, -1.960608319544883793, -1.044296844735680185 ) ) ;
#176224 = CARTESIAN_POINT ( 'NONE',  ( 1.617596980227502756, 1.765956010477184535, 1.173731981927571555 ) ) ;
#176226 = DIRECTION ( 'NONE',  ( -0.000000000000000000, -1.000000000000000000, -0.000000000000000000 ) ) ;
#176228 = CIRCLE ( 'NONE', #203858, 5.799999999999999822 ) ;
#176227 = CARTESIAN_POINT ( 'NONE',  ( -4.925354943514475003, 8.968274210734028529, 0.000000000000000000 ) ) ;
#176229 = CARTESIAN_POINT ( 'NONE',  ( 6.322179702674084467, 6.270297829408224111, 1.040834085586084257E-14 ) ) ;
#176230 = CARTESIAN_POINT ( 'NONE',  ( 4.105873170248697690, 0.6631157982108953908, -1.846516426336957784 ) ) ;
#176231 = CARTESIAN_POINT ( 'NONE',  ( 10.05067194643221207, 10.62020544712608938, 0.7998128361456462443 ) ) ;
#176232 = CARTESIAN_POINT ( 'NONE',  ( -5.512743837300482674, 6.249232958799082027, 0.9732600881407500459 ) ) ;
#176233 = CARTESIAN_POINT ( 'NONE',  ( 3.816783937446950770, 4.411668334231586996, 1.199719254218464037 ) ) ;
#176234 = CARTESIAN_POINT ( 'NONE',  ( -1.402160292154681736E-14, 0.3218750003414227456, 1.575800808251672791 ) ) ;
#176235 = CARTESIAN_POINT ( 'NONE',  ( -5.668717624289589807, 5.786127781192186958, 0.7216878364870257245 ) ) ;
#176237 = ORIENTED_EDGE ( 'NONE', *, *, #184968, .F. ) ;
#176236 = CARTESIAN_POINT ( 'NONE',  ( -7.551528373131759508, 7.912463978182924684, 1.040834085586084257E-14 ) ) ;
#176238 = CARTESIAN_POINT ( 'NONE',  ( 3.691739789689612472, 1.995538565534977549, -0.7177698711837015022 ) ) ;
#176239 = CARTESIAN_POINT ( 'NONE',  ( -5.984998465789844069, 5.947196063035064206, 0.7998128361456281477 ) ) ;
#176240 = CARTESIAN_POINT ( 'NONE',  ( 3.872077330825273389, 1.198917189070296541, 1.798566189592496034 ) ) ;
#176241 = CARTESIAN_POINT ( 'NONE',  ( 3.966218424140379728, -1.719484690100345325, -0.6589542199007536460 ) ) ;
#176242 = CARTESIAN_POINT ( 'NONE',  ( -4.511607644515479798, 7.038970647229928268, 1.150300019105324978 ) ) ;
#176243 = CARTESIAN_POINT ( 'NONE',  ( -0.6823417656250003738, -0.2197916663252488800, -1.181850606188749264 ) ) ;
#176244 = CARTESIAN_POINT ( 'NONE',  ( 5.876847675788273939, 1.605460876287589045, -0.6722632963065499068 ) ) ;
#176245 = CARTESIAN_POINT ( 'NONE',  ( 6.727182134110202050, 0.5964276595885747989, 1.864301751488647962 ) ) ;
#176246 = CARTESIAN_POINT ( 'NONE',  ( 2.873965376416980355, 6.296784005887697155, -0.7216878364870267237 ) ) ;
#176247 = CARTESIAN_POINT ( 'NONE',  ( 12.00011339110129605, 6.571252426151665382, -0.4971413739769103834 ) ) ;
#176248 = EDGE_CURVE ( 'NONE', #147848, #4590, #154417, .T. ) ;
#176249 = CARTESIAN_POINT ( 'NONE',  ( 2.870174731959000525, 1.155358403710282866, 1.826860881501219280 ) ) ;
#176250 = AXIS2_PLACEMENT_3D ( 'NONE', #205343, #56980, #141477 ) ;
#176251 = CARTESIAN_POINT ( 'NONE',  ( 6.098982473628085543, 0.9961464269193781584, -1.752763620266280187 ) ) ;
#176252 = CARTESIAN_POINT ( 'NONE',  ( -7.307481607641392429, 11.46921960898288972, 0.7216878364870458196 ) ) ;
#176253 = CARTESIAN_POINT ( 'NONE',  ( 2.342841879718413622, 0.4729757327756216601, 2.109170662781891359 ) ) ;
#176254 = CARTESIAN_POINT ( 'NONE',  ( 3.884019131438942285, -0.9746410142534560617, 1.713524893406521699 ) ) ;
#176255 = CARTESIAN_POINT ( 'NONE',  ( -0.05867695357848409787, -1.698172713885632401, -1.384993232510664640 ) ) ;
#176256 = CARTESIAN_POINT ( 'NONE',  ( 4.317874670498635048, 1.191976824791032064, -1.533171632797071693 ) ) ;
#176259 = VERTEX_POINT ( 'NONE', #144471 ) ;
#176258 = DIRECTION ( 'NONE',  ( 0.000000000000000000, 0.000000000000000000, 1.000000000000000000 ) ) ;
#176257 = CARTESIAN_POINT ( 'NONE',  ( -9.300530188850304469, 9.952966096521256745, 1.040834085586084257E-14 ) ) ;
#176260 = CARTESIAN_POINT ( 'NONE',  ( -5.661411662158206681, 8.762674818229999829, -1.199719254218452047 ) ) ;
#176261 = DIRECTION ( 'NONE',  ( 0.000000000000000000, 0.000000000000000000, 1.000000000000000000 ) ) ;
#176263 = ORIENTED_EDGE ( 'NONE', *, *, #109624, .T. ) ;
#176262 = CARTESIAN_POINT ( 'NONE',  ( -3.318713740295064163, 7.093859473644694269, 0.000000000000000000 ) ) ;
#176264 = CARTESIAN_POINT ( 'NONE',  ( -8.961576348508655698, 9.557519949455999253, -0.7216878364870267237 ) ) ;
#176265 = CARTESIAN_POINT ( 'NONE',  ( 2.081372155488591780, -0.1082299263688718260, -2.204229314041641352 ) ) ;
#176266 = CARTESIAN_POINT ( 'NONE',  ( -3.285556943750000514, -0.8385416661887076240, -1.896917185911906500 ) ) ;
#176267 = CARTESIAN_POINT ( 'NONE',  ( 6.930524233185829885, -1.209519613549964845, 1.545115813350018241 ) ) ;
#176268 = CARTESIAN_POINT ( 'NONE',  ( 0.6823417656249899377, 5.488541667008087543, -1.181850606188754593 ) ) ;
#176269 = CARTESIAN_POINT ( 'NONE',  ( 0.7499999999999902300, 3.847916667349481123, -1.299038105676658228 ) ) ;
#176270 = CARTESIAN_POINT ( 'NONE',  ( 5.877843389052785028, 6.166481636157870483, -0.8510708418205383818 ) ) ;
#176272 = CARTESIAN_POINT ( 'NONE',  ( 0.4019237886466850984, 12.70758545099816850, -1.499999999999996669 ) ) ;
#176271 = CARTESIAN_POINT ( 'NONE',  ( 4.041739190205284160, 7.729463131965888856, 0.000000000000000000 ) ) ;
#176273 = CARTESIAN_POINT ( 'NONE',  ( 5.050657991863417351, -1.557144343216086968, -0.9820927893566462341 ) ) ;
#176274 = EDGE_LOOP ( 'NONE', ( #26247, #138709, #28934, #29290 ) ) ;
#176275 = CARTESIAN_POINT ( 'NONE',  ( -0.6124999999999984901, 2.770833334016134408, -1.060881119635941339 ) ) ;
#176276 = CARTESIAN_POINT ( 'NONE',  ( -8.830438121202295321, 9.196599317691152464, -0.7998128361456291469 ) ) ;
#176277 = CARTESIAN_POINT ( 'NONE',  ( -4.161989969715295778, 4.726297878971393196, 2.420000000000010587 ) ) ;
#176278 = CARTESIAN_POINT ( 'NONE',  ( 5.888958097455845753, -2.014202512972632420, -0.6635655960139997811 ) ) ;
#176279 = FACE_OUTER_BOUND ( 'NONE', #112059, .T. ) ;
#176280 = CARTESIAN_POINT ( 'NONE',  ( 6.308621549060418054, 6.254479983525607523, 0.7998128361456341429 ) ) ;
#176281 = CARTESIAN_POINT ( 'NONE',  ( 6.134070664438048048, 1.019536383099900245, -1.790854842558225801 ) ) ;
#176284 = CARTESIAN_POINT ( 'NONE',  ( 4.897927690869709139, -0.6253142351902387652, -1.731941863025769246 ) ) ;
#176283 = CARTESIAN_POINT ( 'NONE',  ( 2.330303589177587398, -1.147911989558418222, 1.464751052146954224 ) ) ;
#176282 = CARTESIAN_POINT ( 'NONE',  ( 3.790776250277827941, 4.071658342522865404, -0.8783347955927873763 ) ) ;
#176285 = CARTESIAN_POINT ( 'NONE',  ( 5.947222937888848371, 10.09017719417900416, 1.040834085586084257E-14 ) ) ;
#176286 = CARTESIAN_POINT ( 'NONE',  ( -9.453965130556928997, 14.52925576243678130, -7.390745083414802075 ) ) ;
#176287 = CARTESIAN_POINT ( 'NONE',  ( -5.271087860662956537, 9.371629280740593870, 0.000000000000000000 ) ) ;
#176289 = ORIENTED_EDGE ( 'NONE', *, *, #123836, .T. ) ;
#176288 = DIRECTION ( 'NONE',  ( 0.000000000000000000, -0.000000000000000000, 1.000000000000000000 ) ) ;
#176290 = CARTESIAN_POINT ( 'NONE',  ( 4.987059637548557411, -0.2676712469649074055, -2.190530366034774801 ) ) ;
#176291 = CARTESIAN_POINT ( 'NONE',  ( 5.589262808440923713, 1.998987879104210608, -1.059483486058722779 ) ) ;
#176292 = CARTESIAN_POINT ( 'NONE',  ( -4.609409038966229666, 8.321468278861834378, -0.7216878364870267237 ) ) ;
#176293 = CARTESIAN_POINT ( 'NONE',  ( 5.677939507029830857, 1.783257022268599723, -0.3182440143107477248 ) ) ;
#176294 = CARTESIAN_POINT ( 'NONE',  ( 0.1281391398850126040, 2.011452084832816123, 0.1435147193784985509 ) ) ;
#176295 = DIRECTION ( 'NONE',  ( 0.7592566023653005702, -0.6507913734559639396, 0.000000000000000000 ) ) ;
#176296 = VECTOR ( 'NONE', #137509, 1000.000000000000000 ) ;
#176297 = CARTESIAN_POINT ( 'NONE',  ( 6.649288223980674317, -1.503899034092892162, -1.112267350887645945 ) ) ;
#176298 = CARTESIAN_POINT ( 'NONE',  ( 5.320932177894995618, 1.445329238430465013, -1.252218921613167169 ) ) ;
#176299 = DIRECTION ( 'NONE',  ( 0.000000000000000000, 1.000000000000000000, 0.000000000000000000 ) ) ;
#176300 = CARTESIAN_POINT ( 'NONE',  ( 0.9713206009373563932, 1.803875226702996049, -0.4951341686536685494 ) ) ;
#176301 = CARTESIAN_POINT ( 'NONE',  ( 0.7961116948485976730, -0.9110139862544311962, -1.799120828532501326 ) ) ;
#176303 = CARTESIAN_POINT ( 'NONE',  ( 4.266313661023513504, 0.9922932564179194337, 1.857654695958657953 ) ) ;
#176302 = CARTESIAN_POINT ( 'NONE',  ( -8.805130697071332335, 12.36007068230351358, 1.199719254218462483 ) ) ;
#176304 = CARTESIAN_POINT ( 'NONE',  ( 9.423080456697809026, 10.95234760669099749, -1.199719254218446718 ) ) ;
#176306 = CARTESIAN_POINT ( 'NONE',  ( -6.516665389662827934, 10.75452672124865217, 0.000000000000000000 ) ) ;
#176305 = CARTESIAN_POINT ( 'NONE',  ( -1.500000000000001332, 0.1500000000000251132, 0.000000000000000000 ) ) ;
#176307 = CARTESIAN_POINT ( 'NONE',  ( -11.78331023100045627, 11.29999999999998117, 1.799999999999999600 ) ) ;
#176308 = CARTESIAN_POINT ( 'NONE',  ( 2.970967976831692781, -1.526577591334898454, 1.322595846222093030 ) ) ;
#176309 = CARTESIAN_POINT ( 'NONE',  ( 0.6823417656249882723, 2.926041667008084879, -1.181850606188754593 ) ) ;
#176310 = CARTESIAN_POINT ( 'NONE',  ( 2.184835310096557404, 5.700724961754617404, 1.040834085586084257E-14 ) ) ;
#176311 = CARTESIAN_POINT ( 'NONE',  ( 4.886082254767631916, -1.023713625618065004, 1.903838226609423590 ) ) ;
#176312 = CARTESIAN_POINT ( 'NONE',  ( 8.011942431032855083, 8.311964022485323511, 0.7998128361456291469 ) ) ;
#176313 = CARTESIAN_POINT ( 'NONE',  ( -1.499999999999997780, 4.900000000000022560, 1.214306433183764966E-14 ) ) ;
#176315 = CARTESIAN_POINT ( 'NONE',  ( -9.499606441938682977, -9.580980486002397711, 0.08647223992180037844 ) ) ;
#176314 = CARTESIAN_POINT ( 'NONE',  ( 5.806634928402749196, 9.996434193103704402, -0.7998128361456481317 ) ) ;
#176316 = CARTESIAN_POINT ( 'NONE',  ( 8.554831740098654436, 11.00372300158037042, 1.443375672974076540 ) ) ;
#176318 = CARTESIAN_POINT ( 'NONE',  ( 8.266499440872674853, 15.18128111188595675, -8.700183093162271675 ) ) ;
#176317 = CARTESIAN_POINT ( 'NONE',  ( 0.9245737983274513461, 1.070221580302813891, 1.888989948743382552 ) ) ;
#176319 = CARTESIAN_POINT ( 'NONE',  ( -6.561783159334141580, 7.718130443053708767, -1.082531754730544860 ) ) ;
#176320 = CARTESIAN_POINT ( 'NONE',  ( -0.6823417656250003738, 1.717708333674752730, -1.181850606188749264 ) ) ;
#176321 = CARTESIAN_POINT ( 'NONE',  ( 1.980270094416748394, -2.150034404144373301, -0.4237573071887782983 ) ) ;
#176322 = CARTESIAN_POINT ( 'NONE',  ( 6.206481105300311718, 7.020237702803970414, -1.025761867992080356 ) ) ;
#176323 = CARTESIAN_POINT ( 'NONE',  ( 2.114515676104791186, -1.066955051536956356, -1.995125387583786214 ) ) ;
#176324 = CARTESIAN_POINT ( 'NONE',  ( -7.691553217654356622, 7.867900263551875994, -0.7998128361456291469 ) ) ;
#176325 = CARTESIAN_POINT ( 'NONE',  ( -0.6823417656250212460, 5.113541667008086655, 1.181850606188767472 ) ) ;
#176326 = CARTESIAN_POINT ( 'NONE',  ( 5.590372323399994237, 7.390087136190794936, 1.241407824010079652 ) ) ;
#176327 = CARTESIAN_POINT ( 'NONE',  ( -0.7500000000000179856, 12.79166666666666607, 1.299038105676658228 ) ) ;
#176328 = CARTESIAN_POINT ( 'NONE',  ( 6.861835142292143530, 8.138467433163244280, 1.082531754730549967 ) ) ;
#176329 = CARTESIAN_POINT ( 'NONE',  ( 3.989309445023786704, 1.280397443517577782, 1.221928027103141634 ) ) ;
#176330 = CARTESIAN_POINT ( 'NONE',  ( 8.503988664269582998, 10.94440607977979063, 1.599625672291281386 ) ) ;
#176331 = CARTESIAN_POINT ( 'NONE',  ( 0.4640741377587159211, 2.083006155408675397, -0.3091503547662070583 ) ) ;
#176333 = CARTESIAN_POINT ( 'NONE',  ( 0.7499999999999885647, 1.816666666666688634, -1.299038105676652899 ) ) ;
#176332 = CARTESIAN_POINT ( 'NONE',  ( 0.6823417656249934904, 8.692708333674733723, 1.181850606188764807 ) ) ;
#176334 = CARTESIAN_POINT ( 'NONE',  ( -5.984998465789844069, 5.947196063035064206, 0.7998128361456281477 ) ) ;
#176335 = CARTESIAN_POINT ( 'NONE',  ( 5.976185453469534892, -2.006962702346287930, -0.1948244327795861652 ) ) ;
#176337 = ORIENTED_EDGE ( 'NONE', *, *, #94595, .T. ) ;
#176336 = CARTESIAN_POINT ( 'NONE',  ( 5.009926431283926895, -0.6449355957302944642, 1.693101296380158383 ) ) ;
#176338 = CARTESIAN_POINT ( 'NONE',  ( 8.211434591371064684, 12.73175745657494851, -0.7998128361456352531 ) ) ;
#176339 = CARTESIAN_POINT ( 'NONE',  ( 3.168673215318769110, -1.727878594304607995, -0.7172629358194044791 ) ) ;
#176340 = CARTESIAN_POINT ( 'NONE',  ( 4.891501605334720004, -1.894957309059261297, 0.8341102180390786991 ) ) ;
#176341 = CARTESIAN_POINT ( 'NONE',  ( -5.438229012412888252, 9.358701257874761481, -0.7216878364870338292 ) ) ;
#176342 = CARTESIAN_POINT ( 'NONE',  ( 3.364870901607376563, -0.9372182959936623536, -0.3762680151246870497 ) ) ;
#176343 = CARTESIAN_POINT ( 'NONE',  ( 7.052212457402625922, 11.37933163361175382, -0.7998128361456291469 ) ) ;
#176344 = CARTESIAN_POINT ( 'NONE',  ( -1.527007413433568939, 8.693555224946434734, 2.520068491016817624 ) ) ;
#176345 = CARTESIAN_POINT ( 'NONE',  ( 7.075376061485196821, 9.347967719856493218, 1.599625672291268286 ) ) ;
#176346 = EDGE_CURVE ( 'NONE', #127758, #187716, #126121, .T. ) ;
#176347 = CARTESIAN_POINT ( 'NONE',  ( 0.000000000000000000, -4.500000000000003553, 0.000000000000000000 ) ) ;
#176348 = CARTESIAN_POINT ( 'NONE',  ( -0.6823417656250003738, -1.032291666325242607, -1.181850606188749264 ) ) ;
#176349 = CARTESIAN_POINT ( 'NONE',  ( 3.613678190204441254, 0.4790664972640528152, -1.902336835828049244 ) ) ;
#176350 = CARTESIAN_POINT ( 'NONE',  ( 0.8958609827393304581, 0.1455075039201655374, 2.010896580075637541 ) ) ;
#176351 = CARTESIAN_POINT ( 'NONE',  ( -5.144392941742557568, 4.966489618313220333, -0.7998128361456362523 ) ) ;
#176352 = CARTESIAN_POINT ( 'NONE',  ( 7.397945374551106568, 11.78268670361832093, -0.7998128361456291469 ) ) ;
#176353 = CARTESIAN_POINT ( 'NONE',  ( 0.9658262494645246665, 0.9167188063998463754, 1.630421345857439475 ) ) ;
#176354 = CARTESIAN_POINT ( 'NONE',  ( 1.364683531249990311, 3.884375000341417028, 1.214306433183764966E-14 ) ) ;
#176355 = CARTESIAN_POINT ( 'NONE',  ( 2.953388010686915255, -1.773442693046624496, 0.9528950618205129786 ) ) ;
#176357 = CARTESIAN_POINT ( 'NONE',  ( 2.390374844762462203, -0.8132668539616545456, -1.954994498336021458 ) ) ;
#176356 = CARTESIAN_POINT ( 'NONE',  ( -7.063434843039784639, 7.343021526408956667, 1.040834085586084257E-14 ) ) ;
#176359 = EDGE_CURVE ( 'NONE', #43490, #114100, #156627, .T. ) ;
#176358 = FACE_OUTER_BOUND ( 'NONE', #32797, .T. ) ;
#176360 = CARTESIAN_POINT ( 'NONE',  ( 4.686024408448190570, -1.271122505372159539, -1.634150330299996012 ) ) ;
#176361 = CARTESIAN_POINT ( 'NONE',  ( 3.074666975249065626, 6.809138247757705820, 0.000000000000000000 ) ) ;
#176363 = CARTESIAN_POINT ( 'NONE',  ( 11.91826848676304706, 13.50833707238735570, 1.400000051402189971 ) ) ;
#176362 = CARTESIAN_POINT ( 'NONE',  ( 6.509723796436136745, -0.9841294377065135102, -1.844520550012812565 ) ) ;
#176365 = EDGE_LOOP ( 'NONE', ( #58128, #153265, #161627 ) ) ;
#176364 = CARTESIAN_POINT ( 'NONE',  ( 4.805575371506604299, -0.4859443722219913830, 1.759630929660048526 ) ) ;
#176366 = CARTESIAN_POINT ( 'NONE',  ( 8.565000355531088516, 11.01558638625153286, -1.599625672291257406 ) ) ;
#176367 = CARTESIAN_POINT ( 'NONE',  ( -0.3000000000000172529, 3.975028841772365595, -0.9637995837462973725 ) ) ;
#176368 = CARTESIAN_POINT ( 'NONE',  ( 9.781847885788174324, 12.99548848723393490, -8.037988007782987054 ) ) ;
#176369 = CIRCLE ( 'NONE', #20645, 0.08000000000000009881 ) ;
#176370 = CARTESIAN_POINT ( 'NONE',  ( 6.036183878773405453, 1.092744051193066834, -1.917163762461614240 ) ) ;
#176372 =( BOUNDED_SURFACE ( )  B_SPLINE_SURFACE ( 3, 3, ( 
 ( #115551, #3832, #100305, #99256, #199921, #52620, #168502, #153321 ),
 ( #132843, #119821, #101366, #118748, #165304, #16899, #82980, #17963 ),
 ( #184731, #84050, #36357, #150138, #19038, #149053, #198847, #50494 ),
 ( #182609, #67764, #1710, #51568, #20101, #117693, #183685, #86189 ),
 ( #69906, #202029, #85116, #152258, #2773, #200972, #136016, #53689 ),
 ( #137084, #91282, #157341, #173608, #26241, #8929, #75010, #141119 ),
 ( #207130, #28387, #58756, #12126, #11051, #94483, #176772, #124908 ) ),
 .UNSPECIFIED., .T., .F., .T. ) 
 B_SPLINE_SURFACE_WITH_KNOTS ( ( 4, 3, 4 ),
 ( 4, 2, 2, 4 ),
 ( 0.000000000000000000, 0.5000000000000000000, 1.000000000000000000 ),
 ( 0.000000000000000000, 0.08643212109064271620, 0.5432160605453213442, 1.000000000000000000 ),
 .UNSPECIFIED. ) 
 GEOMETRIC_REPRESENTATION_ITEM ( )  RATIONAL_B_SPLINE_SURFACE ( (
 ( 1.000000000000000000, 1.000000000000000000, 1.000000000000000000, 1.000000000000000000, 1.000000000000000000, 1.000000000000000000, 1.000000000000000000, 1.000000000000000000),
 ( 0.3333333333333333703, 0.3333333333333333703, 0.3333333333333333703, 0.3333333333333333703, 0.3333333333333333703, 0.3333333333333333703, 0.3333333333333333703, 0.3333333333333333703),
 ( 0.3333333333333333703, 0.3333333333333333703, 0.3333333333333333703, 0.3333333333333333703, 0.3333333333333333703, 0.3333333333333333703, 0.3333333333333333703, 0.3333333333333333703),
 ( 1.000000000000000000, 1.000000000000000000, 1.000000000000000000, 1.000000000000000000, 1.000000000000000000, 1.000000000000000000, 1.000000000000000000, 1.000000000000000000),
 ( 0.3333333333333333703, 0.3333333333333333703, 0.3333333333333333703, 0.3333333333333333703, 0.3333333333333333703, 0.3333333333333333703, 0.3333333333333333703, 0.3333333333333333703),
 ( 0.3333333333333333703, 0.3333333333333333703, 0.3333333333333333703, 0.3333333333333333703, 0.3333333333333333703, 0.3333333333333333703, 0.3333333333333333703, 0.3333333333333333703),
 ( 1.000000000000000000, 1.000000000000000000, 1.000000000000000000, 1.000000000000000000, 1.000000000000000000, 1.000000000000000000, 1.000000000000000000, 1.000000000000000000) ) ) 
 REPRESENTATION_ITEM ( '' )  SURFACE ( )  );
#176371 = CARTESIAN_POINT ( 'NONE',  ( -0.6823417656250003738, 11.96354166700806765, 1.181850606188754593 ) ) ;
#176373 = CARTESIAN_POINT ( 'NONE',  ( 4.758414378865199801, 1.907420806491459064, 0.1369992607160031295 ) ) ;
#176374 = CARTESIAN_POINT ( 'NONE',  ( -9.969323024750229578, 10.52529837183042716, -0.7998128361456291469 ) ) ;
#176375 = CARTESIAN_POINT ( 'NONE',  ( 7.467843683028853263, 7.606905806488803101, 0.7998128361456341429 ) ) ;
#176376 = CARTESIAN_POINT ( 'NONE',  ( -11.80235830595198010, 11.29999999999999893, -1.696088231482795416 ) ) ;
#176377 = CARTESIAN_POINT ( 'NONE',  ( 3.185802909086945967, 5.700225246367978116, 1.082531754730546636 ) ) ;
#176378 = CARTESIAN_POINT ( 'NONE',  ( 1.500000000000001332, 9.875000000000001776, 0.000000000000000000 ) ) ;
#176379 = CARTESIAN_POINT ( 'NONE',  ( 4.202137545231717120, 6.989912005157271402, 1.199719254218462483 ) ) ;
#176380 = ORIENTED_EDGE ( 'NONE', *, *, #199200, .F. ) ;
#176381 = DIRECTION ( 'NONE',  ( -0.000000000000000000, -1.000000000000000000, -0.000000000000000000 ) ) ;
#176382 = DIRECTION ( 'NONE',  ( 1.000000000000000000, -0.000000000000000000, 1.224646799147353207E-16 ) ) ;
#176383 = CARTESIAN_POINT ( 'NONE',  ( 6.424584688029230328, 8.588711117491191871, 1.599625672291268286 ) ) ;
#176384 = CARTESIAN_POINT ( 'NONE',  ( 3.055305189271266375, 6.508347120884369730, 0.2706067644346449308 ) ) ;
#176385 = CARTESIAN_POINT ( 'NONE',  ( -5.984664909832329904, 7.106694798503815136, 1.079546468792412783 ) ) ;
#176386 = EDGE_CURVE ( 'NONE', #181928, #140668, #163891, .T. ) ;
#176387 = CARTESIAN_POINT ( 'NONE',  ( -4.595850885352567694, 8.305650432979225783, 1.040834085586084257E-14 ) ) ;
#176388 = CARTESIAN_POINT ( 'NONE',  ( 4.359110081993588182, 5.044382169536003602, -1.199719254218452047 ) ) ;
#176389 = CARTESIAN_POINT ( 'NONE',  ( 1.990998161727207449, 0.1877779126488627881, 1.960439330322023999 ) ) ;
#176390 = CARTESIAN_POINT ( 'NONE',  ( 3.146111402376899235, 0.9091623069825971459, 1.799915193831227889 ) ) ;
#176391 = CARTESIAN_POINT ( 'NONE',  ( -7.212047647465563038, 10.50147379109678880, -1.199719254218446718 ) ) ;
#176392 = CARTESIAN_POINT ( 'NONE',  ( 6.364626766972446781, 6.390095747748157251, 0.7998128361456352531 ) ) ;
#176393 = CARTESIAN_POINT ( 'NONE',  ( 6.827182134110224787, 2.426453598513299337, 2.470348285387702347 ) ) ;
#176394 = CARTESIAN_POINT ( 'NONE',  ( 3.187623232016934871, -0.8878212517344568067, 2.003729935572157839 ) ) ;
#176395 = CARTESIAN_POINT ( 'NONE',  ( 9.601931918643629160, 4.115787718308530962, -7.121346131705980298 ) ) ;
#176396 = CARTESIAN_POINT ( 'NONE',  ( 2.520427876150105995, 1.259661825572227167, -1.457548065151576200 ) ) ;
#176397 = CARTESIAN_POINT ( 'NONE',  ( -9.643927338022246332, 10.14567007064778004, -0.7998128361456291469 ) ) ;
#176398 = FACE_OUTER_BOUND ( 'NONE', #130425, .T. ) ;
#176399 = CARTESIAN_POINT ( 'NONE',  ( 0.2331563151865729544, 6.948071805571808035, -2.540803835148666145 ) ) ;
#176400 = CARTESIAN_POINT ( 'NONE',  ( 4.312902262922978736, 5.164712407232485702, -1.082531754730548412 ) ) ;
#176401 = CARTESIAN_POINT ( 'NONE',  ( 8.932124273304774320, 9.315233161810734686, 0.7998128361456462443 ) ) ;
#176402 = CARTESIAN_POINT ( 'NONE',  ( 5.072158865288233009, 7.010880990960010273, 1.443375672974065660 ) ) ;
#176403 = ORIENTED_EDGE ( 'NONE', *, *, #150546, .F. ) ;
#176405 = CARTESIAN_POINT ( 'NONE',  ( 2.561191855132368467, -1.672464352163150147, 1.120165047906955147 ) ) ;
#176404 = CARTESIAN_POINT ( 'NONE',  ( 6.198766299729112639, 1.534709720371667308, 1.016988835930050739 ) ) ;
#176406 = CARTESIAN_POINT ( 'NONE',  ( 3.972236164830291738, 1.968842830503451991, 1.185689330230592642 ) ) ;
#176408 = CARTESIAN_POINT ( 'NONE',  ( 2.553354172538614630, 1.434905519572576171, 1.184926768776579431 ) ) ;
#176407 = CARTESIAN_POINT ( 'NONE',  ( -0.02880301295727759683, -0.006976478922920535501, -2.273770288744044521 ) ) ;
#176409 = CARTESIAN_POINT ( 'NONE',  ( 1.642778471875001811, -2.442708332855377140, 2.845375778867859751 ) ) ;
#176410 = DIRECTION ( 'NONE',  ( 0.6507913734559651608, -0.7592566023652994600, 0.000000000000000000 ) ) ;
#176411 = CARTESIAN_POINT ( 'NONE',  ( 5.695548698317931091, 1.764485844685494742, -0.7379451211212140205 ) ) ;
#176412 = CARTESIAN_POINT ( 'NONE',  ( -8.532158741701643123, 8.848606708273724308, 0.7998128361456462443 ) ) ;
#176413 = CARTESIAN_POINT ( 'NONE',  ( -6.305950844131887223, 6.529566537674873494, 0.000000000000000000 ) ) ;
#176415 = CARTESIAN_POINT ( 'NONE',  ( 3.696050037196423332, -1.868490534004090931, -0.09263902202472777681 ) ) ;
#176414 = CARTESIAN_POINT ( 'NONE',  ( 4.827721544939969966, 1.073412050285113661, -1.793994897088858176 ) ) ;
#176416 = CARTESIAN_POINT ( 'NONE',  ( 5.992340707560151358, 8.014150130285418783, 1.443375672974062551 ) ) ;
#176417 = ORIENTED_EDGE ( 'NONE', *, *, #180914, .F. ) ;
#176418 = DIRECTION ( 'NONE',  ( -5.551115123125782702E-17, 0.000000000000000000, 1.000000000000000000 ) ) ;
#176419 = CARTESIAN_POINT ( 'NONE',  ( -0.01154776750710303362, -8.267087321559111857, -11.00021059652968347 ) ) ;
#176420 = CARTESIAN_POINT ( 'NONE',  ( 6.006443931695136129, -0.6276177885309804916, -1.606848298988555301 ) ) ;
#176421 = CARTESIAN_POINT ( 'NONE',  ( -5.117312914154178216, 8.057616602233474978, -1.199719254218452047 ) ) ;
#176422 = CARTESIAN_POINT ( 'NONE',  ( 1.582203977811939000, -0.5845794355729941882, 1.632800797419992955 ) ) ;
#176423 = CARTESIAN_POINT ( 'NONE',  ( -11.81900460097218186, 11.25757134874137755, -1.592493057836596337 ) ) ;
#176424 = CARTESIAN_POINT ( 'NONE',  ( -1.499999999999997780, 8.627523663848661428, -2.579999999999990301 ) ) ;
#176425 = CARTESIAN_POINT ( 'NONE',  ( -5.249999999999987566, 0.000000000000000000, 1.599999999999997202 ) ) ;
#176426 = CARTESIAN_POINT ( 'NONE',  ( 5.682552277248558603, 1.299237613850280360, -1.739252610423980938 ) ) ;
#176427 = CARTESIAN_POINT ( 'NONE',  ( 4.125493313500066428, -1.746467973620144942, 0.5319596651164605339 ) ) ;
#176428 = CARTESIAN_POINT ( 'NONE',  ( 1.955835763735654487, -0.6658547638305843952, 1.845409454533278648 ) ) ;
#176429 = CARTESIAN_POINT ( 'NONE',  ( 6.280470216940358341, -0.5666190470481970998, -2.040018813895160044 ) ) ;
#176430 = CARTESIAN_POINT ( 'NONE',  ( 9.475938008234967569, 4.398642192756169855, 7.290290965542337354 ) ) ;
#176431 = CARTESIAN_POINT ( 'NONE',  ( -8.631737353394710155, 13.22211067893587533, 1.040834085586084257E-14 ) ) ;
#176432 = CARTESIAN_POINT ( 'NONE',  ( 6.401421083946654100, 10.62007503124645957, -0.7998128361456291469 ) ) ;
#176433 = CARTESIAN_POINT ( 'NONE',  ( 2.367978261241600713, 0.5630001329197281690, -2.044326955284565539 ) ) ;
#176434 = CARTESIAN_POINT ( 'NONE',  ( -3.633221978782290140, 6.222214161012547429, -1.082531754730549967 ) ) ;
#176435 = CARTESIAN_POINT ( 'NONE',  ( -5.219871119622601086, 6.450327202623305389, -1.173442693870077935 ) ) ;
#176436 = CARTESIAN_POINT ( 'NONE',  ( 6.965710887581792576, -0.4882203796070741508, 2.123536573467856403 ) ) ;
#176438 = CARTESIAN_POINT ( 'NONE',  ( -0.7500000000000179856, 13.57291666734946389, 1.299038105676658228 ) ) ;
#176437 = CARTESIAN_POINT ( 'NONE',  ( -11.20845505065987346, 1.972237431424385790, 3.641847810297710097 ) ) ;
#176440 = ORIENTED_EDGE ( 'NONE', *, *, #102432, .F. ) ;
#176439 = CARTESIAN_POINT ( 'NONE',  ( 3.106314965395097438, -0.8985160938580877277, 2.031629072759451926 ) ) ;
#176441 = CARTESIAN_POINT ( 'NONE',  ( 0.8448572530952251913, 0.4413087945813984336, -2.255810399402935484 ) ) ;
#176443 = CARTESIAN_POINT ( 'NONE',  ( 5.032111728107424575, 1.183179145130999643, 1.689302184701612086 ) ) ;
#176442 = CARTESIAN_POINT ( 'NONE',  ( 3.871016551901614200, 4.474939717762034697, -1.199719254218446718 ) ) ;
#176445 = CARTESIAN_POINT ( 'NONE',  ( 0.000000000000000000, -2.887499999999999289, -4.012584370867899430 ) ) ;
#176444 = CARTESIAN_POINT ( 'NONE',  ( 3.217027588192558074, 6.975225629525113824, -1.734723475976807094E-15 ) ) ;
#176446 = CARTESIAN_POINT ( 'NONE',  ( 0.2329586101569553480, 1.399178205689523224, -2.105666472772389941 ) ) ;
#176447 = CARTESIAN_POINT ( 'NONE',  ( 5.390138975101268493, -0.4531076923771395482, -1.784498753146485539 ) ) ;
#176448 = DIRECTION ( 'NONE',  ( 0.000000000000000000, 0.000000000000000000, -1.000000000000000000 ) ) ;
#176449 = CARTESIAN_POINT ( 'NONE',  ( 3.357615597678655917, 7.068968630600412695, 0.7998128361456321445 ) ) ;
#176450 = CARTESIAN_POINT ( 'NONE',  ( 3.469487465715580310, 1.682841854137674398, -0.3771888234031828824 ) ) ;
#176451 = CARTESIAN_POINT ( 'NONE',  ( 1.200408080392855181, 1.350732740426639822, -1.497504596960941958 ) ) ;
#176452 = CARTESIAN_POINT ( 'NONE',  ( 3.024404714233555946, -2.025920917938589749, 1.086156575756046294 ) ) ;
#176453 = CARTESIAN_POINT ( 'NONE',  ( 2.759333473672697767, -1.967098484071924558, -1.117512413888957612 ) ) ;
#176454 = CARTESIAN_POINT ( 'NONE',  ( 5.022148466640797615, -1.125808720090130111, -1.779717422886097244 ) ) ;
#176455 = CARTESIAN_POINT ( 'NONE',  ( -5.750066545971566079, 8.762142499391876171, 1.082531754730550855 ) ) ;
#176456 = CARTESIAN_POINT ( 'NONE',  ( 3.215802288110910290, -0.8691132097216300867, -1.541513200001721540 ) ) ;
#176458 = CARTESIAN_POINT ( 'NONE',  ( 0.1294186239076781653, -2.093018298938463140, 0.9351526010841960668 ) ) ;
#176457 = CARTESIAN_POINT ( 'NONE',  ( 5.370438244344566847, 5.438135171256338829, 0.000000000000000000 ) ) ;
#176459 = CARTESIAN_POINT ( 'NONE',  ( 4.628748294741646951, -1.682209325509572473, 0.7487199040775437409 ) ) ;
#176460 = CARTESIAN_POINT ( 'NONE',  ( -5.949330478298285207, 5.835307067636438028, 0.7998128361456341429 ) ) ;
#176461 = CARTESIAN_POINT ( 'NONE',  ( 5.951666246274803562, 7.006327377817825663, 1.082531754730558626 ) ) ;
#176462 = CARTESIAN_POINT ( 'NONE',  ( -1.500000000000011324, 3.170833333333354265, 0.8660254037844403729 ) ) ;
#176463 = CARTESIAN_POINT ( 'NONE',  ( 4.505938053128990539, -0.9357023767473917619, -1.981784127816770935 ) ) ;
#176464 = CARTESIAN_POINT ( 'NONE',  ( -3.490334480514268645, 6.159475096320226939, -1.199719254218452935 ) ) ;
#176465 = CARTESIAN_POINT ( 'NONE',  ( 0.1368715580175494662, 8.236096389522833405, -2.000481929432700756 ) ) ;
#176466 = CARTESIAN_POINT ( 'NONE',  ( 4.738769824615551407, -2.007376682328159134, -0.5062664373569197851 ) ) ;
#176467 = DIRECTION ( 'NONE',  ( -5.578564026256490882E-16, -1.000000000000000000, -9.066213480720158442E-32 ) ) ;
#176468 = CIRCLE ( 'NONE', #138453, 12.00000000000000355 ) ;
#176469 = CARTESIAN_POINT ( 'NONE',  ( 1.364683531249988535, 4.655208333674755394, -0.7879004041258300672 ) ) ;
#176470 = CARTESIAN_POINT ( 'NONE',  ( 3.035679594228014810, -1.294101122711612151, -1.427291446562365618 ) ) ;
#176471 = CARTESIAN_POINT ( 'NONE',  ( -0.6823417656250039265, 8.817708333674733723, -1.181850606188755259 ) ) ;
#176472 = CARTESIAN_POINT ( 'NONE',  ( 0.1764466950717893667, 2.196028898142581731, -0.3343166089466164115 ) ) ;
#176473 = ORIENTED_EDGE ( 'NONE', *, *, #130972, .F. ) ;
#176475 = SURFACE_SIDE_STYLE ('',( #128866 ) ) ;
#176474 = CARTESIAN_POINT ( 'NONE',  ( -3.797692425603673705, 6.484372692295976570, 1.082531754730549967 ) ) ;
#176476 = CARTESIAN_POINT ( 'NONE',  ( 3.897079088924235712, 6.634010472798538949, 1.199719254218462483 ) ) ;
#176477 = DIRECTION ( 'NONE',  ( -0.000000000000000000, -8.546850786086437571E-32, -1.000000000000000000 ) ) ;
#176478 = CARTESIAN_POINT ( 'NONE',  ( 0.4019237886466778820, 11.10491455036742536, 1.500000000000001554 ) ) ;
#176479 = CARTESIAN_POINT ( 'NONE',  ( 0.04420220085362167040, 7.036439304898326697, -4.015252406538079022 ) ) ;
#176480 = CARTESIAN_POINT ( 'NONE',  ( 3.362058906508964107, 6.866226457661666061, -0.7216878364870351614 ) ) ;
#176481 = CARTESIAN_POINT ( 'NONE',  ( 0.9944974185457016169, 1.932217576897478528, 0.3389098420027157332 ) ) ;
#176482 = CARTESIAN_POINT ( 'NONE',  ( -0.6823417656250003738, 1.030208333674752286, -1.181850606188749264 ) ) ;
#176483 = EDGE_CURVE ( 'NONE', #179460, #63230, #63217, .T. ) ;
#176484 = CARTESIAN_POINT ( 'NONE',  ( 6.649309733611729278, -1.732918351142084035, -1.292073167451508686 ) ) ;
#176485 = CARTESIAN_POINT ( 'NONE',  ( 5.986763597034562068, 1.890319730748804439, 0.5246630281777532323 ) ) ;
#176486 = CARTESIAN_POINT ( 'NONE',  ( -8.676328237741483207, 12.20980114641871062, -1.199719254218446718 ) ) ;
#176487 = CARTESIAN_POINT ( 'NONE',  ( -6.710922848640111127, 6.931757532942661726, 0.7216878364870317197 ) ) ;
#176488 = CARTESIAN_POINT ( 'NONE',  ( 5.717692609583751029, -2.109997883074541392, 0.4692839721026839661 ) ) ;
#176490 = ORIENTED_EDGE ( 'NONE', *, *, #97999, .F. ) ;
#176489 = CARTESIAN_POINT ( 'NONE',  ( -0.03132844593999471045, -5.600264386820912321, -10.94526678918446727 ) ) ;
#176491 = CARTESIAN_POINT ( 'NONE',  ( 1.364683531249990311, 3.884375000341417028, 1.214306433183764966E-14 ) ) ;
#176492 = CARTESIAN_POINT ( 'NONE',  ( 0.4911964603225346115, 1.381658100223854380, 1.261112594198803061 ) ) ;
#176493 = CARTESIAN_POINT ( 'NONE',  ( 6.116466030266402676, 0.5002120791919911769, -1.660072079997718442 ) ) ;
#176495 = CARTESIAN_POINT ( 'NONE',  ( 3.474349307649237328, -2.112600797985896950, -0.5827812199917583591 ) ) ;
#176494 = CARTESIAN_POINT ( 'NONE',  ( 0.6801582343749744686, 0.4739583336747441034, 1.178068619123803451 ) ) ;
#176496 = CARTESIAN_POINT ( 'NONE',  ( 4.137936126805092485, -1.588447180316322260, -1.674080592224574504 ) ) ;
#176497 = CARTESIAN_POINT ( 'NONE',  ( 6.221960870361377793, -1.141027836104959281, -1.715851070140647527 ) ) ;
#176498 = CARTESIAN_POINT ( 'NONE',  ( 1.306472565299764410, 1.712382563992039586, 0.9159111323687963990 ) ) ;
#176499 = CARTESIAN_POINT ( 'NONE',  ( -5.788968402910818156, 7.776882441527838807, 1.443375672974064550 ) ) ;
#176500 = ADVANCED_FACE ( 'NONE', ( #61038 ), #28543, .T. ) ;
#176501 = PRESENTATION_STYLE_ASSIGNMENT (( #78987 ) ) ;
#176502 = CARTESIAN_POINT ( 'NONE',  ( 5.361630242575341931, -1.673063676233761621, -1.302930760576012092 ) ) ;
#176503 = CARTESIAN_POINT ( 'NONE',  ( 1.986954140179174155, -2.015912935764123670, 0.05229865529512293942 ) ) ;
#176504 = CARTESIAN_POINT ( 'NONE',  ( -6.534666851662457532, 6.726125536468730459, 1.040834085586084257E-14 ) ) ;
#176505 = CARTESIAN_POINT ( 'NONE',  ( 5.174942826180319422, -2.076333920960464763, -0.7478091396579674699 ) ) ;
#176506 = DIRECTION ( 'NONE',  ( 0.000000000000000000, 0.000000000000000000, -1.000000000000000000 ) ) ;
#176507 = CARTESIAN_POINT ( 'NONE',  ( -0.9596184899144685199, -3.128028181787985584, -3.256865572402548814 ) ) ;
#176508 = CARTESIAN_POINT ( 'NONE',  ( 0.04711308451243316486, -1.408776630263553375, -1.161003007932148501 ) ) ;
#176509 = CARTESIAN_POINT ( 'NONE',  ( -7.584860592202423035, 7.813701877183096833, -0.7998128361456362523 ) ) ;
#176511 = CARTESIAN_POINT ( 'NONE',  ( -5.387385936583831914, 7.378645907471495846, -1.599625672291271394 ) ) ;
#176510 = CARTESIAN_POINT ( 'NONE',  ( -5.370252646843524325, 7.685795487962019834, 1.333085116894404232 ) ) ;
#176512 = CARTESIAN_POINT ( 'NONE',  ( -10.44369227015510404, 5.112964020592959180, 5.232143560358712087 ) ) ;
#176513 = ORIENTED_EDGE ( 'NONE', *, *, #174092, .F. ) ;
#176514 = CARTESIAN_POINT ( 'NONE',  ( 4.452062314400541787, 2.060485596604546110, -0.04854883430290175134 ) ) ;
#176515 = CARTESIAN_POINT ( 'NONE',  ( 4.097261965275050599, 7.670716846599076710, -0.6648547660955180794 ) ) ;
#176516 = CARTESIAN_POINT ( 'NONE',  ( 0.1288460037565949678, -8.008893676011954454, 9.499262961676864236 ) ) ;
#176517 = CARTESIAN_POINT ( 'NONE',  ( -5.199715606040888005, 6.025088614257851027, -1.199719254218446718 ) ) ;
#176518 = CARTESIAN_POINT ( 'NONE',  ( -3.383641855062333281, 6.105276709951447778, -1.199719254218452047 ) ) ;
#176519 = CARTESIAN_POINT ( 'NONE',  ( 5.004559639922408820, -2.004681531738555123, -0.2449335584770311880 ) ) ;
#176521 = ORIENTED_EDGE ( 'NONE', *, *, #162536, .F. ) ;
#176520 = CARTESIAN_POINT ( 'NONE',  ( 1.499999999999987121, 1.004166666666687968, 0.8660254037844524744 ) ) ;
#176523 = CARTESIAN_POINT ( 'NONE',  ( 7.754900677336718395, 11.99120852362745460, -0.7216878364870267237 ) ) ;
#176522 = CARTESIAN_POINT ( 'NONE',  ( -4.197131071882288289, 7.054347462908075350, -1.199719254218455378 ) ) ;
#176524 = CARTESIAN_POINT ( 'NONE',  ( 7.416473721875251890, 8.611306416064660851, 1.199719254218462483 ) ) ;
#176525 = CARTESIAN_POINT ( 'NONE',  ( 4.135659164760732587, -1.419885373862592726, -1.493960738838293389 ) ) ;
#176526 = CARTESIAN_POINT ( 'NONE',  ( 2.918592439375994552, -1.356299846568160827, -1.492255409411529898 ) ) ;
#176527 = ORIENTED_EDGE ( 'NONE', *, *, #157520, .T. ) ;
#176528 = CARTESIAN_POINT ( 'NONE',  ( 6.727182134110201162, 1.237345558575109861, 2.302850971298702643 ) ) ;
#176529 = CARTESIAN_POINT ( 'NONE',  ( 5.138703914779377158, 5.953908307786102583, 1.199719254218462483 ) ) ;
#176531 = ORIENTED_EDGE ( 'NONE', *, *, #180626, .T. ) ;
#176530 = CARTESIAN_POINT ( 'NONE',  ( -0.2828007905114904852, 7.102855049428780099, -1.981079112686744192 ) ) ;
#176532 = CARTESIAN_POINT ( 'NONE',  ( 2.811874868751465417, -1.677748492350576770, 1.117661080827489606 ) ) ;
#176533 = CARTESIAN_POINT ( 'NONE',  ( 2.765369989423609454, 0.9851603262180377296, 1.555203531693909680 ) ) ;
#176534 = EDGE_CURVE ( 'NONE', #102958, #212297, #77130, .T. ) ;
#176535 = CARTESIAN_POINT ( 'NONE',  ( 1.173011757359025520, -1.460375281577396489, 1.786833355454720884 ) ) ;
#176536 = CARTESIAN_POINT ( 'NONE',  ( 4.817943484809818600, 6.714296380401858499, 1.599625672291269396 ) ) ;
#176537 = CARTESIAN_POINT ( 'NONE',  ( 2.038557401052975671, 2.137775048120754029, 0.3193135401893046899 ) ) ;
#176538 = CARTESIAN_POINT ( 'NONE',  ( -5.713871673155502151, 8.753601821068331290, 1.199719254218452047 ) ) ;
#176539 = ORIENTED_EDGE ( 'NONE', *, *, #147605, .T. ) ;
#176540 = CARTESIAN_POINT ( 'NONE',  ( 8.283668668269706714, 8.766627655843896250, 1.040834085586084257E-14 ) ) ;
#176541 = CARTESIAN_POINT ( 'NONE',  ( 1.375632740723360836, 1.111493989511678881, 1.504490780774490499 ) ) ;
#176542 = ORIENTED_EDGE ( 'NONE', *, *, #95866, .T. ) ;
#176543 = CARTESIAN_POINT ( 'NONE',  ( 5.998895389381466714, 1.612053949438954303, -1.134635204971563782 ) ) ;
#176546 = ADVANCED_FACE ( 'NONE', ( #194235 ), #80490, .F. ) ;
#176545 = CARTESIAN_POINT ( 'NONE',  ( 8.310784975052673218, 10.71900177569337487, -1.443375672974063439 ) ) ;
#176544 = CARTESIAN_POINT ( 'NONE',  ( 0.6823417656249917140, 3.342708333674754506, 1.181850606188765695 ) ) ;
#176548 = CARTESIAN_POINT ( 'NONE',  ( 0.3994152196779980346, 1.832435997337564348, -1.229551327501000380 ) ) ;
#176547 = CARTESIAN_POINT ( 'NONE',  ( -7.413611068574208041, 7.543634422958360730, 0.7998128361456341429 ) ) ;
#176549 = CARTESIAN_POINT ( 'NONE',  ( 6.707487347292075519, -1.660346423639452951, -1.236579608897829363 ) ) ;
#176550 = CARTESIAN_POINT ( 'NONE',  ( 4.482942347612929979, 8.381849838857084123, 1.040834085586084257E-14 ) ) ;
#176551 = CARTESIAN_POINT ( 'NONE',  ( -4.550733115681270036, 8.460939068270139529, 0.7998128361456481317 ) ) ;
#176552 = CARTESIAN_POINT ( 'NONE',  ( 6.539320575229278454, 2.035006821797652687, 2.408631514295301645 ) ) ;
#176553 = CARTESIAN_POINT ( 'NONE',  ( 5.102397915883716273, -0.6633297369818305089, -1.856656708325474581 ) ) ;
#176554 = CARTESIAN_POINT ( 'NONE',  ( -0.01710467543277957581, -1.380256469788909035, 1.610041658517608054 ) ) ;
#176555 = CARTESIAN_POINT ( 'NONE',  ( 0.7499999999999885647, 0.01458333401615358182, 1.299038105676657340 ) ) ;
#176556 = CARTESIAN_POINT ( 'NONE',  ( 5.057380973065424001, -1.947307563149714316, -1.238062830034118988 ) ) ;
#176557 = CARTESIAN_POINT ( 'NONE',  ( 1.428664617098963863, -1.311459235982143534, 1.591897985181329966 ) ) ;
#176558 = CARTESIAN_POINT ( 'NONE',  ( 8.297226821883377568, 8.782445501726501291, -0.7216878364870267237 ) ) ;
#176559 = CARTESIAN_POINT ( 'NONE',  ( 4.016958651398847557, 7.908478536599129249, -0.7998128361456362523 ) ) ;
#176560 = CARTESIAN_POINT ( 'NONE',  ( 5.259637247458703868, 5.100941308315409373, 0.000000000000000000 ) ) ;
#176561 =( BOUNDED_SURFACE ( )  B_SPLINE_SURFACE ( 3, 3, ( 
 ( #40860, #26713, #106966, #24571, #154598, #124315, #122180, #191333, #105883, #10456, #76529 ),
 ( #8329, #58156, #207593, #142642, #208650, #190274, #187076, #157805, #38709, #59212, #170835 ),
 ( #41931, #204369, #89610, #22426, #171908, #6176, #138352, #56027, #23504, #155661, #7243 ),
 ( #112308, #110176, #180434, #209713, #163132, #176187, #78657, #15775, #60281, #28858, #97079 ),
 ( #144785, #210793, #113378, #29931, #14716, #27787, #126438, #12585, #98140, #178323, #93885 ),
 ( #62416, #159925, #45131, #179384, #192401, #11528, #13657, #80807, #128580, #193489, #44057 ),
 ( #147945, #77598, #143721, #96015, #111241, #160993, #177246, #61358, #127517, #194546, #94945 ) ),
 .UNSPECIFIED., .T., .F., .T. ) 
 B_SPLINE_SURFACE_WITH_KNOTS ( ( 4, 3, 4 ),
 ( 4, 1, 1, 1, 1, 1, 1, 1, 4 ),
 ( 0.000000000000000000, 0.5000000000000000000, 1.000000000000000000 ),
 ( 0.000000000000000000, 0.2255234228546724728, 0.3973271701647976828, 0.5245128843546777997, 0.6161923999872991331, 0.6815320185768301009, 0.7298552812456317040, 0.7704940248801678271, 1.000000000000000000 ),
 .UNSPECIFIED. ) 
 GEOMETRIC_REPRESENTATION_ITEM ( )  RATIONAL_B_SPLINE_SURFACE ( (
 ( 1.000000000000000222, 1.000000000000000222, 1.000000000000000666, 0.9999999999999996669, 1.000000000000000222, 0.9999999999999997780, 1.000000000000000000, 1.000000000000000222, 1.000000000000000000, 1.000000000000000000, 1.000000000000000000),
 ( 0.3333333333333334259, 0.3333333333333334259, 0.3333333333333335369, 0.3333333333333333148, 0.3333333333333333148, 0.3333333333333333703, 0.3333333333333333703, 0.3333333333333334814, 0.3333333333333333148, 0.3333333333333334259, 0.3333333333333333703),
 ( 0.3333333333333334259, 0.3333333333333334259, 0.3333333333333335369, 0.3333333333333333148, 0.3333333333333333148, 0.3333333333333333703, 0.3333333333333333703, 0.3333333333333334814, 0.3333333333333333148, 0.3333333333333334259, 0.3333333333333333703),
 ( 1.000000000000000222, 1.000000000000000222, 1.000000000000000666, 0.9999999999999996669, 1.000000000000000222, 0.9999999999999997780, 1.000000000000000000, 1.000000000000000222, 1.000000000000000000, 1.000000000000000000, 1.000000000000000000),
 ( 0.3333333333333334259, 0.3333333333333334259, 0.3333333333333335369, 0.3333333333333333148, 0.3333333333333333148, 0.3333333333333333703, 0.3333333333333333703, 0.3333333333333334814, 0.3333333333333333148, 0.3333333333333334259, 0.3333333333333333703),
 ( 0.3333333333333334259, 0.3333333333333334259, 0.3333333333333335369, 0.3333333333333333148, 0.3333333333333333148, 0.3333333333333333703, 0.3333333333333333703, 0.3333333333333334814, 0.3333333333333333148, 0.3333333333333334259, 0.3333333333333333703),
 ( 1.000000000000000222, 1.000000000000000222, 1.000000000000000666, 0.9999999999999996669, 1.000000000000000222, 0.9999999999999997780, 1.000000000000000000, 1.000000000000000222, 1.000000000000000000, 1.000000000000000000, 1.000000000000000000) ) ) 
 REPRESENTATION_ITEM ( '' )  SURFACE ( )  );
#176562 = CARTESIAN_POINT ( 'NONE',  ( 1.364683531249988757, 2.446875000341415696, 1.214306433183764966E-14 ) ) ;
#176563 = CARTESIAN_POINT ( 'NONE',  ( 4.146814880933355596, 5.931313009212638931, 1.599625672291261402 ) ) ;
#176564 = CARTESIAN_POINT ( 'NONE',  ( 5.111060722227499298, 8.906728576000002562, -0.7216878364870267237 ) ) ;
#176565 = CARTESIAN_POINT ( 'NONE',  ( 4.809118753965334392, -1.746635306876740401, 1.289517135737711540 ) ) ;
#176567 = CARTESIAN_POINT ( 'NONE',  ( 4.317794123949899365, 1.129187743159822288, -1.454283868005897151 ) ) ;
#176566 = CARTESIAN_POINT ( 'NONE',  ( -4.311129659465605002, 4.131998812239033647, 0.7216878364870317197 ) ) ;
#176569 = CARTESIAN_POINT ( 'NONE',  ( 8.917737905728806425, 3.499999999999989342, 8.029567276306217138 ) ) ;
#176568 = CARTESIAN_POINT ( 'NONE',  ( -1.201851678989727383E-14, 5.696875000341416140, -1.575800808251660134 ) ) ;
#176570 = CARTESIAN_POINT ( 'NONE',  ( 5.442994344319362021, -1.727133847215430729, -1.348975639928217118 ) ) ;
#176571 = CARTESIAN_POINT ( 'NONE',  ( 0.6124999999999741762, 0.1458333340161460656, 1.060881119635889380 ) ) ;
#176572 = CARTESIAN_POINT ( 'NONE',  ( 5.998944898715565799, 1.853732409352136568, -1.296943227565182877 ) ) ;
#176573 = CARTESIAN_POINT ( 'NONE',  ( -3.978601536817720330, 7.845232424458246534, -0.1334687937623244003 ) ) ;
#176574 = DIRECTION ( 'NONE',  ( 1.000000000000000000, 0.000000000000000000, 0.000000000000000000 ) ) ;
#176575 = CARTESIAN_POINT ( 'NONE',  ( 4.725438941449205288, 8.332574750205820280, 0.7120043264817934592 ) ) ;
#176576 = CIRCLE ( 'NONE', #138545, 0.08000000000000014044 ) ;
#176577 = CARTESIAN_POINT ( 'NONE',  ( -4.136646265500964148, 6.879818838842817641, -1.082531754730551743 ) ) ;
#176578 = CARTESIAN_POINT ( 'NONE',  ( 0.000000000000000000, 13.49999999999999822, 0.000000000000000000 ) ) ;
#176579 = CARTESIAN_POINT ( 'NONE',  ( 1.059032582198644601, 0.3505281480379630610, -1.734596922625891713 ) ) ;
#176580 = CARTESIAN_POINT ( 'NONE',  ( 5.092444288794719220, -1.116435683446183713, 1.674956235503543889 ) ) ;
#176581 = CARTESIAN_POINT ( 'NONE',  ( 4.821896187954575197, 8.777295985922343391, 0.7998128361456462443 ) ) ;
#176582 = CARTESIAN_POINT ( 'NONE',  ( 3.962026973360888604, 2.090321222856437178, -0.2555144258320155015 ) ) ;
#176583 = CARTESIAN_POINT ( 'NONE',  ( 2.056118223505171372, -1.176884799952466087, 1.511379468370318113 ) ) ;
#176584 = CARTESIAN_POINT ( 'NONE',  ( -0.02244404828157658613, 5.719765766439059540, -2.783169749654360814 ) ) ;
#176585 = CARTESIAN_POINT ( 'NONE',  ( 3.490635713810024132, 1.920951117756137583, 0.4340392168088512692 ) ) ;
#176586 = CARTESIAN_POINT ( 'NONE',  ( 5.238538122511118722, 1.199862898965612823, -1.624631798562142793 ) ) ;
#176587 = CARTESIAN_POINT ( 'NONE',  ( 2.078771448894382701, -0.08914341469279044028, -1.868647664167771616 ) ) ;
#176590 = ORIENTED_EDGE ( 'NONE', *, *, #83296, .T. ) ;
#176589 = CARTESIAN_POINT ( 'NONE',  ( 1.248149539447914735, 0.9399939672071171426, -1.665319807275446706 ) ) ;
#176588 = CARTESIAN_POINT ( 'NONE',  ( 5.355954780876127863, 1.722648150766812103, -0.09025627888907016005 ) ) ;
#176592 = CARTESIAN_POINT ( 'NONE',  ( 5.531363484695522637, 5.555604941673978558, -0.7216878364870207285 ) ) ;
#176591 = CARTESIAN_POINT ( 'NONE',  ( 1.647397727484143592, -1.863059487452220386, 1.182652941231487453 ) ) ;
#176593 = VECTOR ( 'NONE', #69038, 1000.000000000000000 ) ;
#176594 = CARTESIAN_POINT ( 'NONE',  ( -1.201851678989727383E-14, 1.634375000341421025, 1.575800808251672791 ) ) ;
#176595 = CARTESIAN_POINT ( 'NONE',  ( 6.805303039055573322, 10.02693841461847057, 1.199719254218460707 ) ) ;
#176596 = CARTESIAN_POINT ( 'NONE',  ( 6.526239545637954720, 1.075124705556152138, -1.530631868311462362 ) ) ;
#176597 = CARTESIAN_POINT ( 'NONE',  ( 0.04851965725442013155, 7.069405242467053263, -4.059206989956010148 ) ) ;
#176598 = CARTESIAN_POINT ( 'NONE',  ( -5.362413449404877852, 6.214902764849178141, -1.199719254218446718 ) ) ;
#176599 = B_SPLINE_CURVE_WITH_KNOTS ( 'NONE', 3,
 ( #208535, #58041, #127400, #143606 ),
 .UNSPECIFIED., .F., .F.,
 ( 4, 4 ),
 ( 0.000000000000000000, 0.002006560693247956984 ),
 .UNSPECIFIED. ) ;
#176600 = DIRECTION ( 'NONE',  ( -0.000000000000000000, -1.000000000000000000, -0.000000000000000000 ) ) ;
#176601 = CARTESIAN_POINT ( 'NONE',  ( 2.119664376568120012, 0.3561266789769075292, -2.039353370234835872 ) ) ;
#176602 = CARTESIAN_POINT ( 'NONE',  ( 1.499999999999989120, 3.254166666666690855, 0.8660254037844524744 ) ) ;
#176603 = CARTESIAN_POINT ( 'NONE',  ( 5.555090253297246150, 7.504024600312024340, 1.599625672291267398 ) ) ;
#176604 = CARTESIAN_POINT ( 'NONE',  ( -7.226659571283968297, 8.389856573708110332, 1.199719254218450271 ) ) ;
#176605 = CARTESIAN_POINT ( 'NONE',  ( 5.564695703766185275, 5.456842840674144490, 0.000000000000000000 ) ) ;
#176606 = CARTESIAN_POINT ( 'NONE',  ( 6.147156607449644206, 0.2074554230099104890, 2.110329589018632657 ) ) ;
#176607 = CARTESIAN_POINT ( 'NONE',  ( 11.86145016429273191, 19.00000000000000000, 1.179999999999997051 ) ) ;
#176608 = CARTESIAN_POINT ( 'NONE',  ( 1.364683531249988535, 2.613541667008089764, 0.7879004041258500513 ) ) ;
#176610 = CARTESIAN_POINT ( 'NONE',  ( 4.546061579283848353, 4.198160018786257552, -0.7998128361456211532 ) ) ;
#176609 = DIRECTION ( 'NONE',  ( -0.000000000000000000, 1.000000000000000000, 0.000000000000000000 ) ) ;
#176611 = CARTESIAN_POINT ( 'NONE',  ( 4.130232389481975908, 0.2495678132241747615, -2.000550906993769473 ) ) ;
#176612 = CARTESIAN_POINT ( 'NONE',  ( 4.997249278368244951, -0.2745004324337502744, 1.895803710022869959 ) ) ;
#176613 = CARTESIAN_POINT ( 'NONE',  ( 7.334597915313080918, 9.580116872663850813, 1.040834085586084257E-14 ) ) ;
#176614 = CARTESIAN_POINT ( 'NONE',  ( 3.157961424266928052, 0.9873743524775533409, 1.956624655947765357 ) ) ;
#176615 = FACE_OUTER_BOUND ( 'NONE', #152642, .T. ) ;
#176616 = CARTESIAN_POINT ( 'NONE',  ( 0.7499999999999902300, 1.014583334016154526, 1.299038105676657340 ) ) ;
#176617 = CARTESIAN_POINT ( 'NONE',  ( 5.519794446587845016, -0.4848760706452569513, 1.953846845731139759 ) ) ;
#176618 = CARTESIAN_POINT ( 'NONE',  ( -6.663996196316808174, 7.733415969579778171, -1.199719254218446718 ) ) ;
#176620 = CARTESIAN_POINT ( 'NONE',  ( -0.01795374796791787686, -2.016030408028956167, -0.04665595434990427171 ) ) ;
#176619 = CARTESIAN_POINT ( 'NONE',  ( -2.819732761962332024, 6.233512622357263666, -0.7216878364870267237 ) ) ;
#176622 = EDGE_CURVE ( 'NONE', #133392, #45686, #52856, .T. ) ;
#176621 = CARTESIAN_POINT ( 'NONE',  ( 1.364683531249996529, 9.276041667008062319, 0.7879004041258405033 ) ) ;
#176624 = CARTESIAN_POINT ( 'NONE',  ( -6.933015448541747006, 9.181880338089085214, 1.599625672291269396 ) ) ;
#176623 = CARTESIAN_POINT ( 'NONE',  ( 3.069954157378000925, -1.243473088950231675, 1.680628819622100423 ) ) ;
#176626 = ORIENTED_EDGE ( 'NONE', *, *, #153081, .T. ) ;
#176625 = CARTESIAN_POINT ( 'NONE',  ( 1.518105509412637444, 1.162241833864360974, -1.274548180342775838 ) ) ;
#176627 = CARTESIAN_POINT ( 'NONE',  ( 6.099870585610251972, 1.463495690422533579, 1.534846084132005961 ) ) ;
#176628 = CARTESIAN_POINT ( 'NONE',  ( 6.148786358997489820, 7.132337826040578754, -1.199719254218446718 ) ) ;
#176629 = DIRECTION ( 'NONE',  ( 0.000000000000000000, -1.000000000000000000, 0.000000000000000000 ) ) ;
#176630 = CARTESIAN_POINT ( 'NONE',  ( 7.721398836998395687, -6.134628647623487474, 7.721398836998373483 ) ) ;
#176631 = CYLINDRICAL_SURFACE ( 'NONE', #202490, 3.475000000000000089 ) ;
#176632 = CARTESIAN_POINT ( 'NONE',  ( 5.296431564432884542, 9.330920591813708143, 1.040834085586084257E-14 ) ) ;
#176633 = EDGE_LOOP ( 'NONE', ( #41395, #81396, #43622, #203809 ) ) ;
#176634 = CARTESIAN_POINT ( 'NONE',  ( -1.499999999999997780, 6.280000000000035776, -3.469446951953614189E-15 ) ) ;
#176635 = CARTESIAN_POINT ( 'NONE',  ( 1.471055694106305101, -1.553634009935511484, -0.9311844293155254748 ) ) ;
#176636 = CARTESIAN_POINT ( 'NONE',  ( -4.557512192488103686, 8.468847991211438497, -0.7998128361456281477 ) ) ;
#176637 = ORIENTED_EDGE ( 'NONE', *, *, #38876, .T. ) ;
#176638 = CARTESIAN_POINT ( 'NONE',  ( 2.205172540517054802, 5.724451730578533848, 1.040834085586084257E-14 ) ) ;
#176639 = ORIENTED_EDGE ( 'NONE', *, *, #89445, .T. ) ;
#176640 = CARTESIAN_POINT ( 'NONE',  ( 5.422335090822693715, 5.290755458906732933, 0.000000000000000000 ) ) ;
#176641 = CARTESIAN_POINT ( 'NONE',  ( 2.842218536208180435, 1.004546245467073717, -1.507189720918320486 ) ) ;
#176642 = CARTESIAN_POINT ( 'NONE',  ( 6.639320575229255006, 7.629137130509086262, 2.596737603865982624 ) ) ;
#176643 = SURFACE_SIDE_STYLE ('',( #60747 ) ) ;
#176644 = CARTESIAN_POINT ( 'NONE',  ( 4.014365637759117256, 7.575528411784208771, 0.2883143100938356240 ) ) ;
#176645 = CARTESIAN_POINT ( 'NONE',  ( 3.560865204049929122, 1.468383728701172064, -1.143307097947023010 ) ) ;
#176646 = CARTESIAN_POINT ( 'NONE',  ( 1.563933522115690922, -1.023182376180698849, 1.619245466209729756 ) ) ;
#176647 = CARTESIAN_POINT ( 'NONE',  ( 0.9030137451815029026, 1.489685209907613439, 1.054989265776705709 ) ) ;
#176648 = CARTESIAN_POINT ( 'NONE',  ( -7.777967379493323286, -5.907420853759296264, -7.664830294503433450 ) ) ;
#176649 = CARTESIAN_POINT ( 'NONE',  ( -9.569358774130435563, 3.553060279300347180, -7.167287524826059020 ) ) ;
#176650 = CARTESIAN_POINT ( 'NONE',  ( 4.855733865602142707, 8.067643820953190215, 0.9155131637919884380 ) ) ;
#176651 = SURFACE_STYLE_FILL_AREA ( #129054 ) ;
#176652 = CARTESIAN_POINT ( 'NONE',  ( -2.155383234892699562, 5.458438174109348395, 1.040834085586084257E-14 ) ) ;
#176653 = CARTESIAN_POINT ( 'NONE',  ( 7.782016984564054773, 10.10210578678999482, 1.443375672974076540 ) ) ;
#176654 = CARTESIAN_POINT ( 'NONE',  ( 5.313322838536244319, -1.661678602684885986, -1.056841482759300233 ) ) ;
#176655 = CARTESIAN_POINT ( 'NONE',  ( -6.064574784014443942, 5.969758757638621738, -0.7998128361456291469 ) ) ;
#176656 = DIRECTION ( 'NONE',  ( 0.000000000000000000, 0.000000000000000000, -1.000000000000000000 ) ) ;
#176657 = CARTESIAN_POINT ( 'NONE',  ( 0.02354010051478470922, -1.288079656314411459, -1.647238045112088267 ) ) ;
#176658 = CARTESIAN_POINT ( 'NONE',  ( 8.633844893804129228, 8.967240552393299424, -0.7998128361456211532 ) ) ;
#176659 = CARTESIAN_POINT ( 'NONE',  ( 4.911117597291495329, 1.675855952751242883, 0.9498910403669177382 ) ) ;
#176660 = CARTESIAN_POINT ( 'NONE',  ( -6.175902666224832416, 7.163973517805802160, -1.199719254218446718 ) ) ;
#176661 = CARTESIAN_POINT ( 'NONE',  ( 1.166719304534512558, -1.648536928579244165, -0.7845717211837842653 ) ) ;
#176662 = CARTESIAN_POINT ( 'NONE',  ( 2.051678093609669240, -1.773579625386853875, -1.313098587465796774 ) ) ;
#176663 = CARTESIAN_POINT ( 'NONE',  ( -5.983791420057156252, 7.107340751733106643, 1.079986564815892613 ) ) ;
#176664 = CARTESIAN_POINT ( 'NONE',  ( -0.09280742163705632541, -9.178267117872113801, 9.499822780340156925 ) ) ;
#176665 = CARTESIAN_POINT ( 'NONE',  ( 0.6253724811571198527, 0.1964764651697422093, -1.959740272926189464 ) ) ;
#176666 = CARTESIAN_POINT ( 'NONE',  ( 2.735803960117746403, 1.927664933923057600, 0.2353960755621438972 ) ) ;
#176667 = CARTESIAN_POINT ( 'NONE',  ( 1.212267286723569981, -1.587592435625035270, -1.242539042498117086 ) ) ;
#176669 = CARTESIAN_POINT ( 'NONE',  ( 5.260548175522302472, -0.6249328720258572334, -1.753037815340392935 ) ) ;
#176668 = CARTESIAN_POINT ( 'NONE',  ( -5.818384198920079520, 6.817144982608731141, 1.199719254218452935 ) ) ;
#176670 = CARTESIAN_POINT ( 'NONE',  ( 4.899292406491845497, 6.809203455697518947, -1.599625672291273171 ) ) ;
#176671 = CARTESIAN_POINT ( 'NONE',  ( -11.41381675112453209, 13.40000000000000036, -3.704697986577182078 ) ) ;
#176672 = CARTESIAN_POINT ( 'NONE',  ( 10.42352117080803708, 11.05519620889787724, -0.7998128361456281477 ) ) ;
#176673 = CARTESIAN_POINT ( 'NONE',  ( -5.416646063859567484, 6.278174148379618735, 1.199719254218450271 ) ) ;
#176674 = CARTESIAN_POINT ( 'NONE',  ( -7.075376061485238566, 9.347967719856493218, 1.599625672291269396 ) ) ;
#176675 = CARTESIAN_POINT ( 'NONE',  ( 1.488088480104592826, -2.181432686776756391, -0.2102995727721947705 ) ) ;
#176676 = CARTESIAN_POINT ( 'NONE',  ( 4.094199201646931741, 4.839282492418613302, -1.082531754730543083 ) ) ;
#176677 = CARTESIAN_POINT ( 'NONE',  ( 6.556249800660121529, 9.806652646482286073, 1.199719254218452047 ) ) ;
#176678 = CARTESIAN_POINT ( 'NONE',  ( -3.719872605471121751, 6.605953636083950364, -2.419999999999998597 ) ) ;
#176679 = CARTESIAN_POINT ( 'NONE',  ( 3.299243935302543118, 1.439784963707075649, 1.122460502641378755 ) ) ;
#176680 = CARTESIAN_POINT ( 'NONE',  ( -4.783329267523015460, 4.474972321731942593, -0.7998128361456221525 ) ) ;
#176681 = CARTESIAN_POINT ( 'NONE',  ( -2.903417451620861289, 6.539070793532962611, 0.7998128361456341429 ) ) ;
#176682 = CARTESIAN_POINT ( 'NONE',  ( -5.203215198707511036, 7.836405505866204102, -1.276579466623083858 ) ) ;
#176683 = DIRECTION ( 'NONE',  ( 2.949029909160572061E-17, 1.000000000000000000, -8.673600428462353400E-15 ) ) ;
#176684 = CARTESIAN_POINT ( 'NONE',  ( 8.204655514564224816, 12.72384853363364066, 1.040834085586084257E-14 ) ) ;
#176685 = CARTESIAN_POINT ( 'NONE',  ( 1.242661541247750856, 0.3750627104036097781, 1.889477121596821352 ) ) ;
#176686 = CARTESIAN_POINT ( 'NONE',  ( 5.102378460580520247, 1.956245014681293970, 0.1482201060269832671 ) ) ;
#176687 = CARTESIAN_POINT ( 'NONE',  ( -6.744291347794091784, 9.955758108146730123, -1.199719254218440723 ) ) ;
#176688 = CARTESIAN_POINT ( 'NONE',  ( 4.310602774141044868, 7.116454772218158809, -1.199719254218452047 ) ) ;
#176689 = EDGE_CURVE ( 'NONE', #185175, #105328, #176926, .T. ) ;
#176690 = CARTESIAN_POINT ( 'NONE',  ( 5.495707582769355781, -2.191739722525353429, -0.0009102486706394352645 ) ) ;
#176691 = PLANE ( 'NONE',  #160021 ) ;
#176692 = CARTESIAN_POINT ( 'NONE',  ( 3.502843950909264592, 0.4983820457637299639, 2.009271733256080772 ) ) ;
#176694 = CARTESIAN_POINT ( 'NONE',  ( -1.364683531250000748, 1.571875000341421691, 0.000000000000000000 ) ) ;
#176693 = CARTESIAN_POINT ( 'NONE',  ( 0.1331565106231328843, 0.003911343561965873426, -1.946049565259087455 ) ) ;
#176695 = EDGE_LOOP ( 'NONE', ( #179990, #37574, #23084, #117762, #31181, #212857, #87815, #127985, #94526, #174561, #211825, #49831, #114635, #204195, #19974, #89183, #141879 ) ) ;
#176696 = CARTESIAN_POINT ( 'NONE',  ( 3.780169564947546856, 1.941421826978003251, -1.230584599089700637 ) ) ;
#176698 = ORIENTED_EDGE ( 'NONE', *, *, #150667, .F. ) ;
#176697 = CARTESIAN_POINT ( 'NONE',  ( 7.049876689426101350, 9.247942109129029475, -1.443375672974057666 ) ) ;
#176700 = CARTESIAN_POINT ( 'NONE',  ( 0.000000000000000000, -0.8968749995220406390, -3.793834371823813001 ) ) ;
#176699 = CARTESIAN_POINT ( 'NONE',  ( 4.421367491832268293, 7.211993602896056288, 1.082531754730549078 ) ) ;
#176701 = DIRECTION ( 'NONE',  ( 0.000000000000000000, -1.000000000000000000, 0.000000000000000000 ) ) ;
#176702 = CARTESIAN_POINT ( 'NONE',  ( -10.96785329849812562, -5.223431457505089526, 0.4373225248172959434 ) ) ;
#176703 = CARTESIAN_POINT ( 'NONE',  ( 3.785046133934614865, 1.407330997726879973, 1.338362524258763786 ) ) ;
#176704 = VERTEX_POINT ( 'NONE', #31754 ) ;
#176705 = CARTESIAN_POINT ( 'NONE',  ( 9.368320956918608999, 11.95279375453699622, 1.443375672974076540 ) ) ;
#176706 = ORIENTED_EDGE ( 'NONE', *, *, #141556, .T. ) ;
#176707 = CARTESIAN_POINT ( 'NONE',  ( 5.414289803398987466, -1.912571729023364364, 0.006307610287324683096 ) ) ;
#176708 = CARTESIAN_POINT ( 'NONE',  ( 5.948237010872538200, 1.723075781188963207, 0.07969437682242562493 ) ) ;
#176709 = CARTESIAN_POINT ( 'NONE',  ( 4.768767694835816862, -0.2516295123269947642, -2.000731945836851544 ) ) ;
#176710 = CARTESIAN_POINT ( 'NONE',  ( -0.7500000000000006661, 9.708333333333332149, -1.299038105676657340 ) ) ;
#176711 = CARTESIAN_POINT ( 'NONE',  ( 2.209865124170300898, -0.4819264253047173541, 2.153463223375853719 ) ) ;
#176713 = CARTESIAN_POINT ( 'NONE',  ( -11.97929049433705373, 12.22000000000000064, 0.7046979865771783036 ) ) ;
#176712 = CARTESIAN_POINT ( 'NONE',  ( -8.859363311525973117, 12.42334206583395328, -1.199719254218446718 ) ) ;
#176715 = CARTESIAN_POINT ( 'NONE',  ( 6.485617131683707903, 1.222450955268041373, 1.279935727357548458 ) ) ;
#176714 = CARTESIAN_POINT ( 'NONE',  ( 2.132869701138325969, -1.867042483574256728, 0.9408474824332532238 ) ) ;
#176716 = CARTESIAN_POINT ( 'NONE',  ( 5.854138739207011888, 0.1455364397412381439, -2.011204036175239018 ) ) ;
#176718 = CARTESIAN_POINT ( 'NONE',  ( 3.486539624822242889, -0.4467316994782115636, -2.248153690150441975 ) ) ;
#176717 = CARTESIAN_POINT ( 'NONE',  ( 4.050854035433010480, 7.948023151305657841, 0.000000000000000000 ) ) ;
#176719 = CARTESIAN_POINT ( 'NONE',  ( 0.8490573499697011695, 1.738566659290440963, -0.08130723561216267326 ) ) ;
#176720 = VECTOR ( 'NONE', #50347, 1000.000000000000114 ) ;
#176721 = CARTESIAN_POINT ( 'NONE',  ( 2.988655875014298857, -1.259908772670719657, 1.705623289672608678 ) ) ;
#176722 = CARTESIAN_POINT ( 'NONE',  ( 3.009610312849396951, 6.452363523749469643, -0.06592220986071165023 ) ) ;
#176723 = CARTESIAN_POINT ( 'NONE',  ( 1.493026163575939425, 1.669116110853157808, 0.4689669769783275100 ) ) ;
#176724 = CARTESIAN_POINT ( 'NONE',  ( 1.360316468749957597, 1.276041667008120051, 0.7853790794158580502 ) ) ;
#176725 = FACE_OUTER_BOUND ( 'NONE', #194350, .T. ) ;
#176726 = CARTESIAN_POINT ( 'NONE',  ( 0.8894206616707257540, 0.1598827910747530057, 2.165323314709698632 ) ) ;
#176727 = CARTESIAN_POINT ( 'NONE',  ( 3.380092458137720968, -2.014432998692190058, -0.09411721906785883163 ) ) ;
#176728 = CARTESIAN_POINT ( 'NONE',  ( 5.093750000000003553, -1.895863743164187376, -0.7852924748297283042 ) ) ;
#176729 = CARTESIAN_POINT ( 'NONE',  ( -1.500000000000001332, 1.181250000682816603, 0.000000000000000000 ) ) ;
#176730 = CARTESIAN_POINT ( 'NONE',  ( 0.1297406284284522426, -1.182532350666727128, -1.521449160436913584 ) ) ;
#176731 = CARTESIAN_POINT ( 'NONE',  ( -1.364683531250010295, 13.38020833367473017, 0.7879004041258445001 ) ) ;
#176732 = CARTESIAN_POINT ( 'NONE',  ( 3.006315081767933606, -0.8967225907310495403, 2.032537921011686954 ) ) ;
#176733 = ORIENTED_EDGE ( 'NONE', *, *, #138676, .F. ) ;
#176734 = FACE_BOUND ( 'NONE', #107324, .T. ) ;
#176735 = CARTESIAN_POINT ( 'NONE',  ( -0.7500000000000249800, -0.8083333333333136972, 1.299038105676659116 ) ) ;
#176736 = CARTESIAN_POINT ( 'NONE',  ( 7.618792255875527886, 10.97600916757510170, 1.199719254218460707 ) ) ;
#176737 = EDGE_CURVE ( 'NONE', #88820, #8341, #165408, .T. ) ;
#176738 = CARTESIAN_POINT ( 'NONE',  ( 4.915436192723389830, -0.9368120511010556983, -1.466610992562596527 ) ) ;
#176739 = CARTESIAN_POINT ( 'NONE',  ( 4.123457186961496213, 0.2424046295769199388, -1.946780420294342617 ) ) ;
#176741 = CARTESIAN_POINT ( 'NONE',  ( -7.063434843039784639, 7.343021526408956667, 1.040834085586084257E-14 ) ) ;
#176740 = CARTESIAN_POINT ( 'NONE',  ( 3.871016551901614200, 4.474939717762034697, -1.199719254218446718 ) ) ;
#176742 = CARTESIAN_POINT ( 'NONE',  ( -1.409302795777316097, 4.214550261772070705, -0.5172811130322977347 ) ) ;
#176743 = CARTESIAN_POINT ( 'NONE',  ( 4.411571241670419141, -0.3925092328114428986, 2.227967001921112633 ) ) ;
#176744 = CARTESIAN_POINT ( 'NONE',  ( 1.979039114045421988, 1.923815945824264073, 0.7444423131674202665 ) ) ;
#176745 = CARTESIAN_POINT ( 'NONE',  ( -6.449928391799210736, 8.548002428564306143, -1.599625672291263179 ) ) ;
#176746 = VERTEX_POINT ( 'NONE', #192081 ) ;
#176747 = CARTESIAN_POINT ( 'NONE',  ( 1.499999999999987121, 1.035416667349484232, 0.8660254037844524744 ) ) ;
#176748 = CARTESIAN_POINT ( 'NONE',  ( 3.356579238971897805, -1.418645411611328067, 1.219307012350186126 ) ) ;
#176749 = CARTESIAN_POINT ( 'NONE',  ( 2.092031233620697872, -0.3790036544207425195, 1.692025817237676311 ) ) ;
#176750 = CARTESIAN_POINT ( 'NONE',  ( 6.585463931165095985, -0.9389328202267492873, 1.978239266594773671 ) ) ;
#176751 = CARTESIAN_POINT ( 'NONE',  ( 0.7455094363101981703, -1.891729906373079029, 1.136061337225414913 ) ) ;
#176752 = CARTESIAN_POINT ( 'NONE',  ( 4.135729569369491543, -1.488772398488470872, -1.567562023322838671 ) ) ;
#176753 = CARTESIAN_POINT ( 'NONE',  ( 4.347558855881414885, 1.941490382076584975, -0.04909019101095174475 ) ) ;
#176754 = EDGE_CURVE ( 'NONE', #112905, #21324, #121792, .T. ) ;
#176755 = FACE_OUTER_BOUND ( 'NONE', #18439, .T. ) ;
#176756 = CARTESIAN_POINT ( 'NONE',  ( -0.3713344243775837383, 2.999999999999995115, 0.3713344243775316689 ) ) ;
#176757 = CARTESIAN_POINT ( 'NONE',  ( 0.1762450972803019933, 2.096614079038420897, -0.3174041833761130360 ) ) ;
#176758 = CARTESIAN_POINT ( 'NONE',  ( 1.360316468749947605, 2.536458333674726173, -0.7853790794159141164 ) ) ;
#176759 = CARTESIAN_POINT ( 'NONE',  ( 5.625625018759272677, 0.3960990390993284205, 1.976956468877195894 ) ) ;
#176760 = CARTESIAN_POINT ( 'NONE',  ( -9.016335848287868160, 10.47781223021269170, 1.199719254218462483 ) ) ;
#176761 = CARTESIAN_POINT ( 'NONE',  ( 6.774270308322468459, 11.05506579301824743, 0.7998128361456462443 ) ) ;
#176762 = CARTESIAN_POINT ( 'NONE',  ( 1.284279953904126748, 10.64264068711930733, 0.7750000000000013545 ) ) ;
#176763 = CARTESIAN_POINT ( 'NONE',  ( 2.947667120405720986, 0.6567698719579934119, -1.703645827024417914 ) ) ;
#176764 = CARTESIAN_POINT ( 'NONE',  ( 2.714145368365259436, -2.182908968410116834, 0.3227909207665635716 ) ) ;
#176765 = ORIENTED_EDGE ( 'NONE', *, *, #75861, .F. ) ;
#176766 = CARTESIAN_POINT ( 'NONE',  ( -4.570507181138272479, 7.385989907086349504, 1.082531754730549967 ) ) ;
#176767 = UNCERTAINTY_MEASURE_WITH_UNIT (LENGTH_MEASURE( 1.000000000000000082E-05 ), #107834, 'distance_accuracy_value', 'NONE');
#176768 = CARTESIAN_POINT ( 'NONE',  ( 1.642778471875000035, -2.413541666188709911, -2.845375778867859751 ) ) ;
#176769 = CARTESIAN_POINT ( 'NONE',  ( -8.993135964566285168, 9.386413468282476913, -0.7998128361456291469 ) ) ;
#176770 = CARTESIAN_POINT ( 'NONE',  ( 0.9670638486888746277, -1.589497524861957611, 1.246053474203263178 ) ) ;
#176771 = CARTESIAN_POINT ( 'NONE',  ( 0.8211285067932658777, 1.603129840700336706, -1.388046135824993366 ) ) ;
#176772 = CARTESIAN_POINT ( 'NONE',  ( -8.752560982292409975, 14.99999996918461775, -9.356054898121708874 ) ) ;
#176773 = VERTEX_POINT ( 'NONE', #119451 ) ;
#176774 = CARTESIAN_POINT ( 'NONE',  ( -6.231907884136888676, 7.299589282028351001, -1.199719254218453823 ) ) ;
#176775 = CARTESIAN_POINT ( 'NONE',  ( 2.061162768541408230, 1.543764177570670970, 1.038864413082870142 ) ) ;
#176776 = CARTESIAN_POINT ( 'NONE',  ( 4.379447312414087357, 5.068108938359919158, -1.199719254218452047 ) ) ;
#176777 = CARTESIAN_POINT ( 'NONE',  ( 1.129994055010040022, -1.371941552271437770, -1.670562328977095445 ) ) ;
#176778 = CARTESIAN_POINT ( 'NONE',  ( 5.942029771888944545, -1.730864577151491890, -1.034168155301495862 ) ) ;
#176779 = ORIENTED_EDGE ( 'NONE', *, *, #66529, .T. ) ;
#176780 = VERTEX_POINT ( 'NONE', #199549 ) ;
#176781 = CARTESIAN_POINT ( 'NONE',  ( -9.134442807305063639, 11.67993591332117376, 1.599625672291281386 ) ) ;
#176782 = CARTESIAN_POINT ( 'NONE',  ( 3.668406916800326822, -1.225078373119499187, 1.353803248016255178 ) ) ;
#176783 = AXIS2_PLACEMENT_3D ( 'NONE', #175473, #109466, #59565 ) ;
#176786 = ORIENTED_EDGE ( 'NONE', *, *, #188776, .F. ) ;
#176785 = CARTESIAN_POINT ( 'NONE',  ( -5.409091473909686698, 6.481950958801420803, -1.333638828535830045 ) ) ;
#176784 = CARTESIAN_POINT ( 'NONE',  ( -4.847922445338252118, 7.813604065273374921, -1.199719254218453823 ) ) ;
#176787 = CARTESIAN_POINT ( 'NONE',  ( 5.323208952783781811, 7.729862296028469970, 1.309151360253474339 ) ) ;
#176788 = CARTESIAN_POINT ( 'NONE',  ( 5.975935433960425591, 1.776740614516297390, 0.9528632009266968517 ) ) ;
#176789 = CARTESIAN_POINT ( 'NONE',  ( 6.316338248019477852, 1.719745045379994286, 0.6579504788090041467 ) ) ;
#176790 = CARTESIAN_POINT ( 'NONE',  ( -10.99126615174920651, -5.166862915010145052, 0.4382560683119391398 ) ) ;
#176791 = CARTESIAN_POINT ( 'NONE',  ( 4.635575047956096206, -2.111140572116900316, 0.9323621513206108435 ) ) ;
#176792 = CARTESIAN_POINT ( 'NONE',  ( 4.342354338126830804, 8.288106837781779035, -0.7998128361456381397 ) ) ;
#176793 = CARTESIAN_POINT ( 'NONE',  ( 5.501312752317830679, 1.763641270444433307, 1.249554385337700024 ) ) ;
#176794 = CARTESIAN_POINT ( 'NONE',  ( 6.982612806237943559, 8.105135347821125436, -1.199719254218446718 ) ) ;
#176795 = CARTESIAN_POINT ( 'NONE',  ( 1.768985407559420020, 1.857901784229658793, -0.5654475766003872472 ) ) ;
#176796 = CARTESIAN_POINT ( 'NONE',  ( 4.692867332335362462, -1.408920786844407802, -1.815866644984363232 ) ) ;
#176797 = CARTESIAN_POINT ( 'NONE',  ( 5.583321308294927121, 6.218571175896433267, -0.9806921612870276306 ) ) ;
#176798 = CARTESIAN_POINT ( 'NONE',  ( -6.831329296439251131, 9.063246493969506545, -1.599625672291271394 ) ) ;
#176799 = CARTESIAN_POINT ( 'NONE',  ( 5.119927267529915227, -1.001353885182048931, -1.579878405157906673 ) ) ;
#176800 = VERTEX_POINT ( 'NONE', #169199 ) ;
#176804 = ADVANCED_FACE ( 'NONE', ( #134605 ), #51190, .F. ) ;
#176803 = CARTESIAN_POINT ( 'NONE',  ( -4.827585214917754719, 7.789877296449459365, -1.199719254218453823 ) ) ;
#176802 = CARTESIAN_POINT ( 'NONE',  ( 1.499999999999989120, -0.1937499993171845625, 0.000000000000000000 ) ) ;
#176801 = CARTESIAN_POINT ( 'NONE',  ( 2.812653035604309348, -0.5591599321941118639, -1.828790038765286452 ) ) ;
#176805 = CARTESIAN_POINT ( 'NONE',  ( 3.862124860921032354, 2.190326239153097543, -0.2693113811002012525 ) ) ;
#176806 = CARTESIAN_POINT ( 'NONE',  ( 6.983263157960402090, -0.0002233252893329463486, 1.845923184817334084 ) ) ;
#176807 = CARTESIAN_POINT ( 'NONE',  ( -0.2108831679770959699, 2.036692374882024037, -2.313561348563981657 ) ) ;
#176808 = CARTESIAN_POINT ( 'NONE',  ( 4.353576723319599218, 8.093273587265928271, -0.7216878364870357165 ) ) ;
#176809 = CARTESIAN_POINT ( 'NONE',  ( -5.763624699140882157, 7.817591130454727200, -1.443375672974066548 ) ) ;
#176810 = CARTESIAN_POINT ( 'NONE',  ( 1.317580156568556538, -1.924246910545416522, 0.4277698889081028577 ) ) ;
#176811 = EDGE_CURVE ( 'NONE', #185214, #20648, #25180, .T. ) ;
#176812 = CARTESIAN_POINT ( 'NONE',  ( 1.431196836673795936, 2.224535207900823153, 0.6132342015414853353 ) ) ;
#176813 = CARTESIAN_POINT ( 'NONE',  ( 3.033595934319989418, 1.863777508880835487, -0.6128360024686765328 ) ) ;
#176814 = CARTESIAN_POINT ( 'NONE',  ( -5.960744811863571968, 6.983232364376142698, 1.199719254218452935 ) ) ;
#176815 = CARTESIAN_POINT ( 'NONE',  ( 5.910998778867512016, -1.629530645011644463, 1.264396865911474821 ) ) ;
#176816 = CARTESIAN_POINT ( 'NONE',  ( 4.473827502829567315, 7.202920605734387749, -1.082531754730548412 ) ) ;
#176817 = CARTESIAN_POINT ( 'NONE',  ( 4.206772801990143584, 8.129928378955675328, 0.7998128361456271485 ) ) ;
#176818 = EDGE_LOOP ( 'NONE', ( #27718, #206630, #131924, #174516, #155537, #127518, #185682 ) ) ;
#176819 = CARTESIAN_POINT ( 'NONE',  ( -4.893288865221945727, 4.903436309528101056, 0.4027703449977599881 ) ) ;
#176820 = CARTESIAN_POINT ( 'NONE',  ( 6.776370306708061619, -7.161464053357560644, 6.781144757626056396 ) ) ;
#176821 = CARTESIAN_POINT ( 'NONE',  ( 8.563946585326370098, 13.14302144952281814, 0.7998128361456462443 ) ) ;
#176822 = CARTESIAN_POINT ( 'NONE',  ( 1.903425830921786188, -1.835712436893768063, 1.158886079418340875 ) ) ;
#176823 = ADVANCED_BREP_SHAPE_REPRESENTATION ( '', ( #12474, #200407 ), #197031 ) ;
#176824 = CARTESIAN_POINT ( 'NONE',  ( -0.7500000000000006661, 12.20833333333333570, -1.299038105676657340 ) ) ;
#176825 = B_SPLINE_CURVE_WITH_KNOTS ( 'NONE', 3,
 ( #35745, #53063, #36806, #167887, #19488, #151652 ),
 .UNSPECIFIED., .F., .F.,
 ( 4, 2, 4 ),
 ( 0.000000000000000000, 0.0003132070624402877746, 0.0006264141248805755492 ),
 .UNSPECIFIED. ) ;
#176826 = CARTESIAN_POINT ( 'NONE',  ( 11.41381676900473430, 11.03041960022390988, -3.704697931490291918 ) ) ;
#176827 = CARTESIAN_POINT ( 'NONE',  ( -7.548736457559128255, -7.034525084977406806, 7.548736457552015722 ) ) ;
#176828 = CARTESIAN_POINT ( 'NONE',  ( 2.460033746253722065, 0.7958763861501785275, 1.692906160045657860 ) ) ;
#176829 = CARTESIAN_POINT ( 'NONE',  ( 6.538358481810655043, 2.137031053877674225, 0.3242996077847115632 ) ) ;
#176831 = CARTESIAN_POINT ( 'NONE',  ( 6.827182134110225675, 7.053278108740402175, 2.409100297097351184 ) ) ;
#176830 = CARTESIAN_POINT ( 'NONE',  ( -0.02244404828160087226, 1.323617703852699057, -2.440988974267483957 ) ) ;
#176832 = CARTESIAN_POINT ( 'NONE',  ( 1.364683531249988757, -0.1156249996585798079, 0.000000000000000000 ) ) ;
#176833 =( NAMED_UNIT ( * ) SI_UNIT ( $, .STERADIAN. ) SOLID_ANGLE_UNIT ( ) );
#176834 = CARTESIAN_POINT ( 'NONE',  ( 2.455592584850064153, -1.418247937500687561, -1.282927761235647335 ) ) ;
#176835 = CARTESIAN_POINT ( 'NONE',  ( 4.170580646280578563, -1.651567487535645640, -0.6365977468129493388 ) ) ;
#176836 = CARTESIAN_POINT ( 'NONE',  ( 2.033716200607054159, -1.854476301366870805, 0.4660679227486630438 ) ) ;
#176837 = CARTESIAN_POINT ( 'NONE',  ( -3.893162665418476109, 7.693773542963529444, 1.040834085586084257E-14 ) ) ;
#176839 = CARTESIAN_POINT ( 'NONE',  ( 0.07520289192196588646, 1.421326540713454323, 1.284674935297628773 ) ) ;
#176838 = CARTESIAN_POINT ( 'NONE',  ( 8.280982047128212287, -6.442483420143131134, -7.626074736120320274 ) ) ;
#176840 = CARTESIAN_POINT ( 'NONE',  ( 0.7499999999999885647, -0.7666666666666446250, 1.299038105676657340 ) ) ;
#176841 = CARTESIAN_POINT ( 'NONE',  ( 0.7134375191242479097, -1.748147108003229810, -1.108949491591210146 ) ) ;
#176842 = CARTESIAN_POINT ( 'NONE',  ( 0.6823417656249864960, -1.011458332991911568, -1.181850606188749264 ) ) ;
#176843 = CARTESIAN_POINT ( 'NONE',  ( 10.50000000000000178, 13.40000000000000036, -3.600000000000002309 ) ) ;
#176844 = CARTESIAN_POINT ( 'NONE',  ( 5.594569530875262764, -0.4557361262383100020, -1.814172972432124720 ) ) ;
#176845 = CARTESIAN_POINT ( 'NONE',  ( 1.805030607383810715, 1.517133602069477893, 1.015288170653723343 ) ) ;
#176847 = CARTESIAN_POINT ( 'NONE',  ( 4.615647837050825153, 8.347533190886938570, 0.2882115401751338402 ) ) ;
#176846 = CARTESIAN_POINT ( 'NONE',  ( 4.846401659255799466, 2.200796399388889935, 0.1645688927329121420 ) ) ;
#176848 = CARTESIAN_POINT ( 'NONE',  ( 1.364683531249990311, 5.426041667008086655, 0.7879004041258500513 ) ) ;
#176849 = CARTESIAN_POINT ( 'NONE',  ( 3.561030563730323006, 1.627881067681248073, -1.266672197246907494 ) ) ;
#176850 = CARTESIAN_POINT ( 'NONE',  ( -9.352427035328430449, 9.805586384171650849, 1.040834085586084257E-14 ) ) ;
#176851 = FILL_AREA_STYLE_COLOUR ( '', #189023 ) ;
#176852 = CARTESIAN_POINT ( 'NONE',  ( 1.493145604987275998, 3.264456235588189426, 0.1636410324438895558 ) ) ;
#176853 = CIRCLE ( 'NONE', #138830, 0.07999999999999951594 ) ;
#176854 = CARTESIAN_POINT ( 'NONE',  ( -1.734723475976807094E-15, -9.900000000000005684, -10.91970695577494332 ) ) ;
#176855 = CARTESIAN_POINT ( 'NONE',  ( 5.318541398310776103, 9.426991741329731056, -0.7998128361456481317 ) ) ;
#176856 = ORIENTED_EDGE ( 'NONE', *, *, #206271, .F. ) ;
#176857 = CARTESIAN_POINT ( 'NONE',  ( 5.687960312649480876, -1.310561514506687564, -1.602779375087557412 ) ) ;
#176858 = CARTESIAN_POINT ( 'NONE',  ( 1.364683531249986537, 0.1760416670080860446, 0.7879004041258500513 ) ) ;
#176859 = CARTESIAN_POINT ( 'NONE',  ( 2.196749789412206333, -0.5742421066207163971, -2.083876772215712325 ) ) ;
#176860 = B_SPLINE_CURVE_WITH_KNOTS ( 'NONE', 3,
 ( #48530, #129852, #193690, #32268 ),
 .UNSPECIFIED., .F., .F.,
 ( 4, 4 ),
 ( 0.0005910214237608091628, 0.001001414237305831186 ),
 .UNSPECIFIED. ) ;
#176861 = CARTESIAN_POINT ( 'NONE',  ( -4.636404737997885661, 8.342837909782009120, -0.3584692566244596645 ) ) ;
#176862 = CARTESIAN_POINT ( 'NONE',  ( 2.965494806321045562, -1.652366046825021417, -1.161084516292823832 ) ) ;
#176863 = CARTESIAN_POINT ( 'NONE',  ( 7.657759090810039915, -5.412329794880678335, 7.842350841322885735 ) ) ;
#176864 = PRODUCT ( 'base', 'base', '', ( #8103 ) ) ;
#176867 = CARTESIAN_POINT ( 'NONE',  ( 6.290620087060792009, 10.28288116830553101, -0.7216878364870267237 ) ) ;
#176866 = CARTESIAN_POINT ( 'NONE',  ( 1.737499999999999378, -0.8166666666666668739, -3.009438278150925683 ) ) ;
#176865 = SURFACE_STYLE_USAGE ( .BOTH. , #193102 ) ;
#176868 = CARTESIAN_POINT ( 'NONE',  ( -5.465345319640241506, 5.548860092434608760, 0.7216878364870257245 ) ) ;
#176869 = CARTESIAN_POINT ( 'NONE',  ( 1.393767942625488532, -2.000731169080074423, 0.2516357431460446992 ) ) ;
#176871 = CARTESIAN_POINT ( 'NONE',  ( 5.864808805604325492, 0.1626094438406736342, -2.185560445749204828 ) ) ;
#176870 = CARTESIAN_POINT ( 'NONE',  ( -4.904298879841297421, 6.744767997946721216, 1.599625672291267398 ) ) ;
#176872 = CARTESIAN_POINT ( 'NONE',  ( -1.201851678989727383E-14, 5.118750000682815937, -1.732050807568863648 ) ) ;
#176873 = CARTESIAN_POINT ( 'NONE',  ( 4.799029005866479736, -0.2398712174674077491, -1.897248949554980024 ) ) ;
#176874 = CARTESIAN_POINT ( 'NONE',  ( -4.952806187693842510, 4.672695395264567786, 0.7998128361456341429 ) ) ;
#176875 = CARTESIAN_POINT ( 'NONE',  ( 6.114364089638786304, 8.156510742710487705, 1.443375672974076540 ) ) ;
#176877 = CARTESIAN_POINT ( 'NONE',  ( 3.831657784458125438, 0.6766976527424087839, -1.899625577706779422 ) ) ;
#176876 = CARTESIAN_POINT ( 'NONE',  ( -10.11401940567025548, 10.90203684947788076, 1.040834085586084257E-14 ) ) ;
#176878 = CARTESIAN_POINT ( 'NONE',  ( 0.6823417656249969321, 13.33854166700806942, -1.181850606188757036 ) ) ;
#176879 = CARTESIAN_POINT ( 'NONE',  ( -3.923105346307911745, 5.670318552149568703, -1.599625672291283607 ) ) ;
#176880 = CARTESIAN_POINT ( 'NONE',  ( 5.245002492778637837, -1.477622881800463306, 0.8893561077145789584 ) ) ;
#176881 = CARTESIAN_POINT ( 'NONE',  ( 5.905458427204159477, 9.047396044116986502, 1.199719254218452047 ) ) ;
#176882 = CARTESIAN_POINT ( 'NONE',  ( 2.333974999846879061, 5.874721266463329705, -0.7998128361456291469 ) ) ;
#176883 = VECTOR ( 'NONE', #108765, 1000.000000000000114 ) ;
#176884 = CARTESIAN_POINT ( 'NONE',  ( -1.201851678989727383E-14, 3.868750000682817713, -1.732050807568863648 ) ) ;
#176885 = CARTESIAN_POINT ( 'NONE',  ( 11.94105721237523277, 10.07259609010266388, -1.187919463087249827 ) ) ;
#176886 = CARTESIAN_POINT ( 'NONE',  ( 1.164989683304976875, 1.570165760251106990, -1.349419213858449318 ) ) ;
#176887 = CARTESIAN_POINT ( 'NONE',  ( 0.4382560683119269829, -5.166862915010145052, 10.99126615174920474 ) ) ;
#176888 = ORIENTED_EDGE ( 'NONE', *, *, #2389, .F. ) ;
#176889 = CARTESIAN_POINT ( 'NONE',  ( 5.760388245948376174, 1.809740711040405348, 0.08207984589548086851 ) ) ;
#176890 = CARTESIAN_POINT ( 'NONE',  ( 4.355912491740495440, 8.303924683664389406, 0.000000000000000000 ) ) ;
#176891 = CARTESIAN_POINT ( 'NONE',  ( 0.05236148938883232462, -1.314980595004966002, 1.528755779884483523 ) ) ;
#176892 = CARTESIAN_POINT ( 'NONE',  ( 0.3514446173804542939, -1.281351489097491303, -1.280874292944272685 ) ) ;
#176893 = CARTESIAN_POINT ( 'NONE',  ( 5.194182247366868843, 8.113610817686430110, 1.082531754730548412 ) ) ;
#176894 = CARTESIAN_POINT ( 'NONE',  ( 1.394453263437886604E-15, -1.268749999044084253, 3.474999999999999645 ) ) ;
#176895 = CARTESIAN_POINT ( 'NONE',  ( 3.416156609664961152, 1.390242785425911620, -1.694013327489252152 ) ) ;
#176896 = ORIENTED_EDGE ( 'NONE', *, *, #173196, .F. ) ;
#176897 = STYLED_ITEM ( 'NONE', ( #112775 ), #165716 ) ;
#176899 = CARTESIAN_POINT ( 'NONE',  ( 7.214910300766615769, 11.56914578420308715, -0.7998128361456291469 ) ) ;
#176898 = CARTESIAN_POINT ( 'NONE',  ( 1.117545225965112188, 0.3861695934333775337, -1.923310697798483293 ) ) ;
#176900 = CARTESIAN_POINT ( 'NONE',  ( 5.273012193977356432, 1.687281682853270848, -0.9070163062135666587 ) ) ;
#176901 = CARTESIAN_POINT ( 'NONE',  ( -6.353279334749129426, 6.853861929151015886, 0.6383911273219675664 ) ) ;
#176902 = CARTESIAN_POINT ( 'NONE',  ( 0.6124999999999776179, 0.6666666666666626329, -1.060881119635955327 ) ) ;
#176903 = CARTESIAN_POINT ( 'NONE',  ( -0.6823417656250246877, -0.4489583329919111243, 1.181850606188755259 ) ) ;
#176905 = ORIENTED_EDGE ( 'NONE', *, *, #97268, .T. ) ;
#176904 = CARTESIAN_POINT ( 'NONE',  ( 5.504247177468186258, 6.484338464210099851, 1.082531754730558626 ) ) ;
#176906 = CARTESIAN_POINT ( 'NONE',  ( -9.327646496521989405, 10.94497100310623594, -1.082531754730539753 ) ) ;
#176907 = CARTESIAN_POINT ( 'NONE',  ( 2.307699607974790901, -0.4742087202370263155, 2.108885336910087283 ) ) ;
#176908 = CARTESIAN_POINT ( 'NONE',  ( -5.808742468812186033, 5.741564066561132940, 0.000000000000000000 ) ) ;
#176909 = CARTESIAN_POINT ( 'NONE',  ( 6.048345925472178308, 9.110135108809304327, 1.082531754730549967 ) ) ;
#176910 = CARTESIAN_POINT ( 'NONE',  ( 1.641335390984842491, -1.319735721761399638, -1.261605215524951085 ) ) ;
#176911 = FACE_OUTER_BOUND ( 'NONE', #46633, .T. ) ;
#176912 = CARTESIAN_POINT ( 'NONE',  ( 4.506759567000420574, 1.410888988908312047, -1.158519065656477220 ) ) ;
#176913 = CARTESIAN_POINT ( 'NONE',  ( 11.31666751210511102, 7.462798040830318946, -3.198044674750592620 ) ) ;
#176914 = CARTESIAN_POINT ( 'NONE',  ( 3.076317393561965208, 0.8638369986560844316, 1.706277067364105893 ) ) ;
#176915 = ORIENTED_EDGE ( 'NONE', *, *, #88237, .F. ) ;
#176916 = CARTESIAN_POINT ( 'NONE',  ( 3.578522297727056767, 1.251517597477384447, -1.520772613757546354 ) ) ;
#176917 = VERTEX_POINT ( 'NONE', #149762 ) ;
#176918 = CARTESIAN_POINT ( 'NONE',  ( 6.427294056597427918, -1.271908742016104821, -1.467670737461545860 ) ) ;
#176919 = EDGE_LOOP ( 'NONE', ( #105392, #209821, #148147, #48542, #113022 ) ) ;
#176920 = CARTESIAN_POINT ( 'NONE',  ( -7.435720902452096936, 7.639705572474380091, 0.000000000000000000 ) ) ;
#176922 = CARTESIAN_POINT ( 'NONE',  ( 6.999862025036637014, -6.532648833121176501, -6.392587740394701790 ) ) ;
#176921 = CARTESIAN_POINT ( 'NONE',  ( -5.798046968499580345, 6.793418213784815585, 1.199719254218452935 ) ) ;
#176923 = CARTESIAN_POINT ( 'NONE',  ( 5.655159470231527763, 9.611786791996525636, -0.7216878364870458196 ) ) ;
#176924 = CARTESIAN_POINT ( 'NONE',  ( 3.650944405621194377, 0.2833616294029631111, 1.891055170903446658 ) ) ;
#176925 = CARTESIAN_POINT ( 'NONE',  ( 5.777328231396808178, 6.232550548966264259, -0.9930585829777474061 ) ) ;
#176926 = LINE ( 'NONE', #15466, #115236 ) ;
#176927 = CARTESIAN_POINT ( 'NONE',  ( 5.090160327287878594, 4.903218234782778850, -0.7998128361456481317 ) ) ;
#176928 = CARTESIAN_POINT ( 'NONE',  ( 5.127594652646677353, -0.2932247039480195827, 1.991498814599843792 ) ) ;
#176929 = DIRECTION ( 'NONE',  ( 0.000000000000000000, -1.000000000000000000, 0.000000000000000000 ) ) ;
#176930 = CARTESIAN_POINT ( 'NONE',  ( 5.971303284387838417, 0.1295235881030691594, -1.821162830480331563 ) ) ;
#176931 = CARTESIAN_POINT ( 'NONE',  ( 0.6255436495894195481, 0.2045281481408110225, -2.060252820462626477 ) ) ;
#176932 = CARTESIAN_POINT ( 'NONE',  ( -6.385527162356466668, 10.39360608948380182, 0.000000000000000000 ) ) ;
#176933 = AXIS2_PLACEMENT_3D ( 'NONE', #55701, #6925, #8006 ) ;
#176934 = CARTESIAN_POINT ( 'NONE',  ( -6.382290003970109815, 6.834844811514095397, -0.5765442458998057962 ) ) ;
#176935 = DIRECTION ( 'NONE',  ( 0.000000000000000000, 0.000000000000000000, -1.000000000000000000 ) ) ;
#176936 = FACE_OUTER_BOUND ( 'NONE', #47871, .T. ) ;
#176937 = CARTESIAN_POINT ( 'NONE',  ( 5.937581207780954884, 9.014596278131406848, -1.199719254218440723 ) ) ;
#176938 = AXIS2_PLACEMENT_3D ( 'NONE', #128244, #11176, #144445 ) ;
#176939 = CARTESIAN_POINT ( 'NONE',  ( -10.50060100873255031, 5.377693802073529206, 5.808388628131297970 ) ) ;
#176940 = EDGE_CURVE ( 'NONE', #177712, #32739, #2730, .T. ) ;
#176941 = CARTESIAN_POINT ( 'NONE',  ( 0.1333692844072559280, 0.001398348041498076455, -2.053671342968105051 ) ) ;
#176942 = CARTESIAN_POINT ( 'NONE',  ( -8.012344526598182026E-15, 12.35937500034139624, -1.575800808251669460 ) ) ;
#176943 = CARTESIAN_POINT ( 'NONE',  ( -3.761497552787613330, 6.475832013972435242, 1.199719254218464037 ) ) ;
#176944 = CARTESIAN_POINT ( 'NONE',  ( -7.391130018105325661, 8.652015104991543026, -1.199719254218452047 ) ) ;
#176945 = EDGE_CURVE ( 'NONE', #163746, #72143, #53318, .T. ) ;
#176946 = CARTESIAN_POINT ( 'NONE',  ( 4.254371668973718990, 1.680547194560323643, -0.4271837243535313022 ) ) ;
#176947 = CARTESIAN_POINT ( 'NONE',  ( -4.066556009095094737, 6.831733546331167695, 1.199719254218464037 ) ) ;
#176948 = CARTESIAN_POINT ( 'NONE',  ( 0.9189038144036645317, -1.502058968113138437, 1.424965263859011122 ) ) ;
#176949 =( BOUNDED_SURFACE ( )  B_SPLINE_SURFACE ( 3, 3, ( 
 ( #118946, #85308, #67953, #170829, #2964, #133028, #53884, #202232, #34417, #199027, #150327, #168692, #185994, #83162, #1894, #5092, #149242, #52808, #50674, #18153, #134098, #69035, #201168, #817, #200106, #66886, #71167, #166564, #84240, #183870, #135152, #184925, #137284, #120018, #151394, #101561, #51758, #35484, #117879, #20296, #167629, #152450, #36549, #37628, #102635, #203303, #86382, #4028, #103708, #169759, #54950, #70098, #21347, #121103, #187070, #26707, #139417, #124310, #141580, #91747, #60276, #126433, #138346, #175121, #123250, #74408, #207588, #154591, #208644, #189214, #72238, #24564, #89604, #157800, #25635, #8324, #90670, #40854, #192396, #6170, #206519, #188139, #158853, #122173, #88530, #204363, #190269, #191327, #106960, #155655, #56019, #59207, #9396, #44051, #10451, #92810, #39771, #41926, #75468, #105876, #58151, #205452, #125364, #171900, #23498, #172985, #76524, #156733, #142635, #7237, #73314, #109106, #110171, #140508, #57085, #108037, #22420, #174063, #42993, #176182, #62411, #162062, #13651, #15771, #212913, #178317, #194539, #93880, #128575, #27781, #47259, #46186, #30999, #193482, #64547, #209708, #164185, #45126, #127512, #196681, #146893, #180430, #79724, #210788, #177239, #28853, #32047, #78652, #63483, #80803, #97074, #213954, #65575, #77593, #114431, #112302, #145840, #130690, #159918, #147939, #29926, #11523, #96009, #94940, #163127, #179379, #211845, #129637, #195624, #131722, #143716, #113372, #111236, #98135, #61352, #160988, #12580, #14710, #48319, #81856, #144780, #197727, #49366, #184665, #153246, #37361, #119749, #132771, #68775, #168433, #99185, #85047, #17890, #36284, #181478, #66625, #199851, #103436, #117617, #21079, #50424, #116543, #201960, #137012, #169497, #87181, #182534, #1635, #166300, #20030, #560, #4821, #198775, #185728, #70901, #86118, #3758, #34162, #152189, #151135, #51493, #100233, #203039, #35217, #165235, #69834, #135943, #83976, #16829, #150064, #200900, #53616, #115485, #67694, #33108, #82912, #2701, #148985, #133841, #183610, #101293, #167374, #18962, #134894, #52549, #118679, #102362, #194014, #29403, #121902, #155384, #105596, #110711, #154324, #111781, #71970, #128058, #13129, #176711, #160459, #138080, #28324, #90398, #205176, #39498, #79207, #188946, #104514, #94420, #12067, #5898, #170557, #187869, #143193, #78136, #145324, #171629, #61897, #54679, #24292, #22141, #204093, #23224, #40586, #172716, #186805, #89336, #120829, #45664, #55746, #38434, #6968, #106691, #156468, #177787, #144266, #56818, #73049, #88255, #139148, #122988, #209184, #8055, #126985, #77063, #210259, #60824, #95495, #192944, #44596, #161542, #182015, #1125, #197212, #31538, #212386, #64028, #67187, #113920, #98665, #116029, #66115, #34707, #100776, #112845, #149539, #97614, #48852, #33646, #129119, #183095, #163671, #46733, #213445, #130174, #132258, #52, #114966, #65068, #15254, #166858, #195096, #180966, #162604, #133324, #96557, #62950, #178861, #164720, #165792, #81341, #196166, #30472, #99720, #198265, #18454, #199327, #50973, #14180, #16309, #49908, #80273, #32588, #179916, #17375, #146371, #47807, #147420, #117095, #131224, #82394, #148483, #83459, #84531, #211325, #36836, #5378, #167920, #38989, #184153, #138633, #19517, #101851, #171113, #121386, #154875, #136500 ),
 ( #88818, #102919, #202521, #55239, #68257, #122467, #168980, #200393, #152731, #3252, #71457, #153807, #54170, #4313, #20580, #188426, #134390, #120309, #85594, #72535, #35776, #2181, #118167, #103995, #105074, #86664, #69320, #52041, #187359, #137570, #40061, #204656, #6458, #151682, #170039, #203587, #135430, #186284, #53095, #22705, #201452, #119229, #70384, #56305, #37921, #106171, #185212, #21625, #172197, #23786, #150620, #87733, #157019, #190549, #140789, #142923, #189497, #143998, #107251, #160198, #45400, #208923, #192677, #173272, #60558, #125649, #25920, #74688, #111516, #9673, #139711, #126717, #44331, #41141, #205735, #8605, #175398, #110453, #177522, #206803, #94159, #89892, #59492, #57369, #24852, #58436, #75750, #207868, #7529, #124589, #155943, #77876, #90954, #73612, #42205, #141860, #191611, #209990, #176454, #127798, #28066, #26983, #43273, #108322, #109393, #11801, #61632, #93090, #159131, #174342, #123532, #92028, #158085, #10732, #76802, #193753, #180710, #12858, #113654, #198018, #48597, #33392, #179658, #178593, #81080, #96290, #14986, #13925, #99470, #80005, #46459, #162342, #165529, #161272, #146110, #50713, #212121, #49646, #115769, #63759, #78933, #129919, #30202, #164466, #17121, #31278, #195905, #47541, #97353, #181758, #163410, #147167, #83198, #64821, #145055, #213194, #148228, #130967, #194823, #196959, #114715, #82136, #32333, #98401, #16052, #214230, #149280, #65858, #132008, #861, #66927, #133069, #199067, #116839, #29134, #95222, #211058, #62683, #128842, #112581, #18193, #138385, #35520, #51798, #187105, #118981, #67995, #38739, #186033, #87494, #152486, #120058, #85348, #137321, #203337, #151429, #19266, #54990, #204403, #121142, #37669, #104821, #88569, #200144, #135191, #1935, #167665, #201207, #4068, #103745, #3002, #100529, #182840, #134137, #202270, #153559, #36586, #183909, #168731, #117916, #101597, #102673, #71205, #154627, #70138, #184960, #53921, #69071, #170867, #20333, #52846, #22457, #169796, #5130, #136250, #21385, #86419, #6207, #72276, #56056, #34457, #166604, #84278, #150365, #191364, #208680, #27817, #139454, #74441, #155691, #106994, #140543, #157835, #43031, #90709, #39809, #122213, #7274, #141613, #92845, #190301, #123287, #108070, #205486, #189250, #41958, #10485, #93914, #9432, #58185, #207623, #159955, #158889, #59240, #91778, #73351, #125399, #126468, #192431, #174098, #109143, #57120, #188175, #77629, #40889, #156771, #173019, #105915, #175156, #171940, #206557, #76559, #26742, #44086, #124343, #24600, #25671, #8357, #75502, #142669, #110205, #60309, #176215, #11559, #143751, #23531, #209746, #89639, #46223, #81892, #15806, #112340, #45159, #178352, #62447, #196715, #49401, #63523, #13688, #29960, #96046, #147978, #129675, #179415, #197763, #97110, #111273, #162099, #180467, #195660, #12617, #163162, #146929, #114467, #79758, #47294, #212946, #211882, #213988, #32083, #98171, #145874, #130724, #115520, #65608, #113409, #164219, #31036, #131758, #181515, #33144, #128610, #177276, #16869, #194577, #99224, #78690, #14747, #165274, #28892, #80839, #64583, #48356, #127547, #144815, #82949, #149023, #61388, #193518, #210822, #94976, #161022, #22183, #137051, #186844, #67730, #101331, #51533, #53654, #100272, #54721, #17929, #70941, #170597, #119786, #103474, #84013 ),
 ( #133881, #86156, #169536, #88299, #199888, #4862, #598, #184702, #116580, #150104, #117658, #200938, #118714, #132811, #183651, #66664, #203077, #166337, #198815, #167412, #52586, #36323, #120870, #37399, #2740, #19004, #50461, #85085, #182575, #152227, #151169, #69872, #1676, #21116, #34197, #38476, #35255, #68811, #87222, #185767, #104553, #102401, #134933, #168469, #20067, #3798, #135981, #201996, #153286, #9172, #192174, #43835, #55785, #92594, #40627, #206298, #58993, #72010, #126212, #106730, #204132, #156508, #7008, #75247, #157579, #140279, #8097, #172757, #109951, #138123, #124088, #105639, #76308, #39538, #5939, #121942, #107813, #108882, #24332, #73085, #187908, #125149, #141359, #175961, #142415, #171667, #90440, #23263, #25415, #74186, #207373, #89375, #42775, #155424, #208423, #139186, #205216, #174905, #191107, #158636, #57923, #188983, #56858, #123032, #10233, #190051, #41703, #26484, #60057, #27556, #154360, #173838, #91520, #144558, #29708, #179156, #11294, #114220, #210568, #143488, #45968, #28634, #129422, #63260, #95789, #112089, #128358, #180219, #77373, #161846, #127286, #130475, #193257, #159695, #209485, #79510, #162907, #62202, #94721, #61126, #30780, #195405, #31841, #64334, #212692, #44904, #145628, #113150, #111012, #13434, #12359, #47035, #177017, #160764, #194326, #196466, #178090, #48108, #78438, #211625, #80579, #97917, #163976, #93652, #96859, #14489, #146677, #22201, #119803, #66679, #149035, #182590, #168485, #185782, #2756, #150119, #134947, #17943, #1692, #68825, #37416, #54737, #36339, #85099, #20084, #186861, #103492, #86172, #118731, #34213, #152242, #153303, #4878, #200953, #3814, #166352, #611, #104569, #100286, #117673, #84030, #132826, #69886, #198830, #19019, #169553, #135999, #70957, #151184, #67746, #52602, #133896, #21134, #87238, #137067, #184715, #183666, #199903, #51549, #203092, #35270, #102417, #53671, #202012, #38491, #170614, #50475, #120887, #101348, #116596, #167427, #5955, #60072, #189000, #138138, #90457, #155440, #157595, #91536, #74202, #156523, #106746, #126228, #72026, #57939, #39554, #10248, #187924, #154378, #55802, #41719, #42788, #40643, #7025, #204147, #59007, #9190, #192189, #76324, #92607, #105655, #107829, #141375, #121957, #124104, #205232, #75261, #171683, #23280, #172773, #142429, #8114, #208438, #89392, #73101, #174920, #109967, #43853, #175978, #139202, #190067, #56873, #26500, #24347, #88314, #123049, #158650, #140296, #207386, #191122, #206315, #125163, #173854, #25430, #108897, #197528, #161861, #77388, #212708, #146692, #193274, #143504, #94736, #113167, #130495, #115290, #160782, #31857, #27571, #211640, #209501, #177032, #12375, #13451, #145645, #159711, #144573, #49172, #15566, #44919, #93669, #128374, #79527, #63276, #81653, #64349, #29723, #45983, #11310, #194341, #61141, #179171, #112104, #96874, #111027, #196482, #127303, #147740, #28649, #78455, #48124, #95805, #210587, #129438, #30795, #80596, #62217, #195421, #162924, #178107, #180234, #114236, #97933, #47051, #14504, #163991, #213756, #65379, #131525, #1438, #201775, #135751, #119552, #33965, #16631, #136816, #100042, #50227, #185538, #117420, #66434, #37166, #184471, #85924, #150941, #118487, #83777, #53415, #103244, #149870, #17691, #169304, #202843, #20888, #36088, #86985, #153055 ),
 ( #151997, #69643, #198580, #3569, #2504, #183417, #166105, #54492, #101091, #82715, #4631, #70703, #132577, #148792, #67503, #52359, #181281, #32907, #133649, #98985, #165038, #68576, #362, #116346, #199648, #167178, #84851, #182337, #51295, #35020, #18767, #134703, #200708, #102172, #168239, #19838, #177577, #160251, #122791, #138960, #38240, #6778, #186614, #208976, #72853, #192729, #137892, #11852, #154129, #111569, #203911, #71776, #144050, #94211, #127854, #106493, #155197, #121713, #187675, #193804, #23028, #10781, #28117, #44383, #161328, #12912, #55558, #76856, #89143, #104313, #60612, #170362, #204981, #77930, #142975, #45453, #56626, #39305, #172519, #105400, #24104, #171438, #29190, #188750, #40389, #93143, #95280, #21947, #159180, #145108, #126771, #210046, #61685, #110505, #88057, #176505, #78992, #211114, #120636, #5699, #15042, #47595, #31330, #149335, #131021, #80062, #146163, #212178, #16105, #179713, #181814, #64875, #13975, #164520, #148282, #115827, #113709, #197013, #214281, #213245, #915, #33446, #99523, #147220, #132061, #199119, #83251, #48649, #165582, #97407, #66982, #17176, #133120, #129973, #112638, #18245, #195960, #63813, #50762, #114766, #162399, #116892, #65914, #182891, #32390, #198071, #163462, #34508, #100581, #81134, #180763, #166655, #84329, #150415, #49699, #62738, #128898, #98455, #82189, #96344, #194879, #46515, #178647, #30258, #187157, #134183, #1982, #35569, #21432, #38786, #70186, #3051, #202321, #85395, #69120, #136298, #104867, #122263, #103795, #152532, #87540, #39861, #170912, #153609, #186086, #101649, #5180, #6257, #72328, #53970, #71256, #19319, #68046, #171992, #167716, #185011, #151481, #4117, #22507, #36638, #88617, #154672, #138434, #135241, #51845, #23584, #201255, #52895, #204452, #120107, #119029, #56106, #137369, #121188, #37717, #203386, #102722, #188221, #105970, #168779, #20384, #89691, #200192, #117964, #55039, #183958, #86468, #169845, #108122, #189297, #140596, #25722, #57171, #28940, #126522, #73404, #155742, #40937, #175208, #192483, #9482, #156818, #141665, #24650, #8405, #75554, #44135, #61432, #43083, #91831, #26790, #193565, #110256, #92895, #125454, #107042, #158940, #160004, #11605, #207676, #10536, #173069, #7327, #111322, #90757, #124393, #74490, #139507, #76609, #205534, #157890, #176265, #142723, #77679, #59295, #206607, #191416, #58236, #109196, #190351, #143800, #42013, #174149, #208732, #209797, #123333, #60359, #177326, #27866, #93963, #127599, #45208, #78739, #211933, #96094, #15857, #82998, #97159, #47343, #79809, #63567, #181565, #163214, #112386, #178398, #30010, #48409, #129724, #214037, #14796, #46269, #196766, #180516, #148027, #145921, #80887, #32136, #31086, #33193, #65662, #131810, #179462, #164268, #16918, #115569, #99276, #195708, #113457, #165325, #50512, #49450, #81944, #149074, #651, #162149, #146977, #128660, #212995, #64632, #210870, #182629, #197819, #12665, #95024, #194626, #114521, #66717, #130771, #13736, #98217, #132861, #198865, #116634, #161074, #144863, #62495, #184752, #119843, #72064, #4915, #185821, #3852, #133935, #53710, #38528, #104605, #168524, #37452, #51588, #34252, #204184, #199940, #2793, #117713, #100324, #103531, #17982, #118768, #203134, #169590, #170652, #36380, #183703, #86208, #101388, #20122, #19059 ),
 ( #85137, #84071, #151224, #35311, #21172, #22240, #102458, #200994, #68864, #134983, #120923, #152279, #167463, #52639, #69926, #202050, #136037, #153344, #87275, #70992, #137105, #54776, #186896, #88350, #154414, #5993, #138174, #55840, #121996, #166391, #150160, #1728, #67785, #208470, #124137, #76355, #8151, #60106, #142462, #126265, #40677, #23319, #143540, #106780, #56909, #192222, #190099, #73134, #43885, #191157, #92640, #157625, #125194, #90493, #109999, #176011, #172808, #89427, #209534, #24380, #123082, #27603, #41752, #139238, #93704, #42824, #158682, #9222, #108930, #156556, #159744, #11342, #74235, #140328, #77423, #61176, #187961, #174951, #39589, #105693, #205269, #206346, #7061, #57974, #107864, #155478, #171720, #10281, #189040, #173890, #25465, #207417, #91573, #75294, #141410, #59036, #26533, #194373, #47082, #15600, #32944, #14536, #63309, #212744, #165075, #97967, #64378, #96906, #12408, #146725, #131560, #197561, #113200, #130523, #144605, #127336, #82750, #78488, #95839, #210620, #193306, #196514, #111059, #211673, #81688, #48157, #49205, #129471, #62246, #179206, #46017, #30830, #112136, #115325, #178140, #128406, #29754, #181315, #44951, #161895, #148823, #13482, #147772, #213788, #79557, #177066, #145676, #195453, #114269, #99017, #162958, #80633, #180266, #31890, #65411, #164025, #16666, #396, #28682, #94768, #160816, #185571, #68610, #17721, #168271, #152031, #119588, #51326, #134734, #3601, #2535, #4665, #37201, #103275, #150970, #135783, #202875, #87017, #200742, #169337, #101123, #153090, #20922, #52391, #118519, #120668, #70738, #184503, #84883, #198615, #167211, #132608, #69679, #18799, #201807, #83809, #136851, #100072, #54523, #149902, #1469, #186646, #38272, #104349, #36122, #102206, #67536, #133678, #170393, #183448, #19872, #21982, #53449, #85956, #88091, #154165, #66467, #50261, #116380, #182368, #33998, #166134, #199683, #117454, #35052, #72888, #75041, #8968, #206092, #7887, #24136, #43633, #137920, #189850, #171471, #142208, #105436, #71809, #187710, #173639, #174701, #172551, #138995, #203940, #190906, #141158, #109748, #208222, #10030, #23061, #25212, #58789, #55588, #41495, #122825, #207165, #121743, #89177, #90238, #59854, #73974, #126006, #155229, #6810, #92392, #27350, #191967, #175758, #205016, #107608, #56662, #158428, #156304, #93453, #188787, #76104, #5730, #124944, #108673, #40422, #42570, #91316, #140069, #106525, #39338, #57727, #123884, #26276, #157373, #110806, #209278, #12166, #30576, #47912, #32688, #78238, #163774, #159490, #129226, #60925, #94520, #144360, #145427, #63058, #77166, #62001, #115074, #147523, #176812, #11089, #45768, #197315, #143287, #195199, #28427, #81446, #44699, #127082, #193045, #112950, #114022, #111885, #210361, #160558, #130277, #14282, #48956, #213544, #15352, #128157, #178961, #212492, #194117, #46836, #177889, #80377, #29502, #95595, #161643, #65167, #13238, #131322, #79311, #211428, #31639, #181070, #96657, #162710, #146472, #64133, #196265, #97716, #180018, #152841, #116131, #169080, #54276, #3357, #201557, #182119, #69428, #134493, #34804, #83561, #120413, #18556, #148582, #135533, #53203, #50007, #151, #165892, #184252, #119334, #186388, #17477, #103025, #98768, #68360, #66217, #33749, #149643, #84633, #2284, #16415, #1225, #164825 ),
 ( #199433, #82495, #35879, #51075, #168021, #99826, #185321, #132365, #86769, #67287, #133426, #36944, #20679, #4415, #150724, #117201, #183198, #100879, #70486, #166966, #200497, #136602, #19625, #52140, #202626, #198367, #118268, #101954, #85696, #151784, #170145, #9777, #138737, #87841, #40160, #105177, #107349, #41242, #23883, #106274, #56406, #38025, #71563, #57474, #8707, #172295, #39090, #89989, #121490, #171213, #156040, #140893, #158184, #139812, #188530, #123633, #75849, #74791, #189596, #7629, #137670, #173371, #42307, #108422, #73714, #24955, #55338, #104096, #207968, #203691, #6560, #187462, #21732, #91057, #153912, #122567, #206903, #157118, #174444, #205840, #22807, #58534, #88922, #124689, #154975, #26020, #72640, #204755, #190647, #92130, #5482, #141956, #59594, #125751, #212229, #146211, #176556, #175500, #94262, #192779, #112685, #179759, #193854, #144101, #28166, #160301, #63862, #45504, #209022, #60658, #126822, #145157, #11904, #96394, #111620, #143027, #79042, #62787, #30309, #77978, #177632, #128950, #127903, #130018, #162445, #14020, #61735, #46565, #113755, #196009, #29240, #80107, #210096, #47644, #31376, #97452, #44437, #27089, #147260, #110554, #95332, #163507, #161381, #76903, #15091, #194928, #81181, #12965, #178695, #211163, #213292, #64918, #191713, #43371, #109493, #93197, #159228, #10829, #6032, #39624, #148324, #83293, #164563, #115870, #3889, #32433, #7099, #104641, #48693, #69959, #88384, #153379, #138212, #136071, #65955, #185856, #198113, #119878, #181855, #204224, #33492, #214323, #49743, #55876, #114808, #99565, #155518, #165629, #154454, #72101, #17217, #180807, #149378, #132104, #54814, #122033, #202086, #53744, #37488, #103566, #187999, #169625, #21208, #87310, #4950, #71028, #137142, #38566, #203169, #82233, #120963, #186934, #170688, #22275, #105729, #171759, #23355, #89464, #131067, #197055, #98499, #16148, #209566, #93738, #9259, #176045, #107903, #159777, #27638, #11377, #140363, #123118, #28715, #206382, #156592, #77456, #75329, #172846, #143574, #76389, #192255, #42857, #10315, #190136, #61212, #127369, #41790, #124172, #193340, #94802, #44985, #142498, #111094, #177100, #90530, #25502, #106816, #58008, #157661, #189078, #160850, #43918, #205309, #73171, #24417, #92673, #110033, #141446, #74271, #59072, #8186, #173929, #207453, #139277, #56946, #174984, #125232, #158717, #40711, #91610, #208504, #108964, #191190, #60139, #26568, #126296, #146759, #15638, #29789, #12442, #182406, #112170, #195485, #95874, #78521, #164059, #210653, #14573, #132642, #161929, #13519, #99053, #34035, #148858, #198648, #79592, #48191, #145711, #165108, #179240, #66503, #211709, #82786, #100108, #131595, #115359, #63345, #197597, #114303, #162992, #129504, #144638, #212777, #62281, #49240, #181351, #178174, #128441, #47119, #98002, #32977, #194407, #113236, #16700, #46049, #196548, #30864, #96942, #80668, #64412, #130558, #180301, #31923, #81725, #432, #147808, #213827, #65444, #50297, #116415, #5766, #202913, #168308, #184535, #83846, #52428, #17757, #37239, #118554, #20956, #183480, #54558, #199720, #154199, #35089, #117489, #186679, #136886, #170431, #152065, #200776, #167245, #18833, #22018, #68645, #53485, #70773, #87054, #119623, #120704, #71847, #201841, #36158, #3635, #38307, #149935, #137955 ),
 ( #88128, #104384, #102237, #203975, #19906, #55622, #121779, #187746, #84917, #1504, #39374, #151005, #101159, #166169, #85991, #51366, #67570, #169372, #133714, #135817, #103310, #134768, #2575, #69714, #185607, #153126, #4697, #122863, #172589, #27383, #23097, #7925, #127116, #90271, #126038, #59889, #156340, #89212, #74011, #106562, #26311, #93484, #107642, #57760, #140103, #206130, #192001, #173674, #188824, #40458, #24168, #58825, #123921, #10064, #25249, #56696, #207200, #190939, #158464, #189889, #91349, #42603, #41530, #43666, #76140, #142243, #157411, #174738, #159523, #109783, #9002, #208255, #75077, #175792, #11122, #77199, #141190, #155265, #60959, #124978, #108710, #143318, #92424, #205054, #209312, #193083, #105471, #171504, #6846, #72924, #139030, #65199, #13271, #95627, #131351, #183, #213577, #114057, #197347, #164856, #62037, #211457, #78268, #29535, #129261, #160591, #132399, #15384, #176846, #44733, #144394, #64166, #81478, #112982, #45800, #30608, #128191, #111921, #178993, #147555, #16447, #146508, #195231, #130309, #82528, #48989, #196296, #14317, #210395, #47943, #115107, #181105, #96696, #180050, #194152, #110840, #66251, #177921, #79344, #161677, #28459, #31672, #94553, #46869, #32720, #97749, #98802, #162744, #145462, #80410, #63092, #212525, #163808, #148614, #12198, #70518, #52174, #1259, #67317, #133461, #151818, #100910, #103060, #200528, #149678, #85733, #69461, #36977, #183230, #118300, #135566, #134524, #136633, #169114, #20710, #68395, #53237, #120447, #4448, #184286, #86804, #18590, #202660, #152870, #54309, #51107, #33782, #153944, #117232, #199465, #186421, #35912, #83596, #38059, #201590, #104130, #168056, #119367, #166999, #170176, #21764, #84668, #34836, #87872, #5512, #71593, #185355, #198401, #50043, #150757, #2319, #17508, #101987, #19658, #99861, #116166, #182152, #165923, #3391, #171244, #157154, #108459, #205874, #138770, #123667, #6593, #204788, #57508, #26055, #43405, #24991, #73750, #8746, #175534, #174479, #74827, #107387, #22840, #140927, #141991, #208005, #189630, #206941, #155008, #137702, #93230, #88954, #106306, #72673, #203722, #58570, #121524, #7665, #92168, #124724, #59630, #139845, #56441, #41278, #122600, #173410, #188563, #125788, #40194, #172328, #23917, #191750, #55370, #90022, #159262, #156079, #158220, #9809, #91094, #187494, #190685, #42344, #75884, #109528, #27124, #10863, #39124, #105207, #144137, #212262, #81215, #63896, #112719, #130051, #31411, #176591, #193892, #192815, #210130, #111654, #126857, #147295, #14054, #209057, #76936, #110589, #194965, #80143, #161416, #11941, #13000, #94297, #78013, #79076, #146246, #97485, #62826, #29274, #46601, #163542, #196044, #178731, #211200, #28203, #30346, #47678, #113789, #145194, #96431, #160337, #143062, #60693, #61772, #95366, #127940, #45540, #179791, #177666, #128986, #15127, #162482, #44473, #206570, #205498, #108082, #123298, #41971, #40900, #60320, #107005, #73364, #189261, #192444, #188186, #173030, #77641, #24612, #76571, #10498, #90721, #39821, #156783, #57131, #191376, #44099, #58197, #8369, #74452, #140556, #142683, #124355, #139469, #190313, #174111, #9442, #25683, #175167, #91792, #7286, #157848, #141624, #109155, #75513, #207634, #59252, #125410, #208693, #26754, #92855, #43042, #158901, #110219 ) ),
 .UNSPECIFIED., .T., .F., .T. ) 
 B_SPLINE_SURFACE_WITH_KNOTS ( ( 4, 3, 4 ),
 ( 4, 1, 1, 1, 1, 1, 1, 1, 1, 1, 1, 1, 1, 1, 1, 1, 1, 1, 1, 1, 1, 1, 1, 1, 1, 1, 1, 1, 1, 1, 1, 1, 1, 1, 1, 1, 1, 1, 1, 1, 1, 1, 1, 1, 1, 1, 1, 1, 1, 1, 1, 1, 1, 1, 1, 1, 1, 1, 1, 1, 1, 1, 1, 1, 1, 1, 1, 1, 1, 1, 1, 1, 1, 1, 1, 1, 1, 1, 1, 1, 1, 1, 1, 1, 1, 1, 1, 1, 1, 1, 1, 1, 1, 1, 1, 1, 1, 1, 1, 1, 1, 1, 1, 1, 1, 1, 1, 1, 1, 1, 1, 1, 1, 1, 1, 1, 1, 1, 1, 1, 1, 1, 1, 1, 1, 1, 1, 1, 1, 1, 1, 1, 1, 1, 1, 1, 1, 1, 1, 1, 1, 1, 1, 1, 1, 1, 1, 1, 1, 1, 1, 1, 1, 1, 1, 1, 1, 1, 1, 1, 1, 1, 1, 1, 1, 1, 1, 1, 1, 1, 1, 1, 1, 1, 1, 1, 1, 1, 1, 1, 1, 1, 1, 1, 1, 1, 1, 1, 1, 1, 1, 1, 1, 1, 1, 1, 1, 1, 1, 1, 1, 1, 1, 1, 1, 1, 1, 1, 1, 1, 1, 1, 1, 1, 1, 1, 1, 1, 1, 1, 1, 1, 1, 1, 1, 1, 1, 1, 1, 1, 1, 1, 1, 1, 1, 1, 1, 1, 1, 1, 1, 1, 1, 1, 1, 1, 1, 1, 1, 1, 1, 1, 1, 1, 1, 1, 1, 1, 1, 1, 1, 1, 1, 1, 1, 1, 1, 1, 1, 1, 1, 1, 1, 1, 1, 1, 1, 1, 1, 1, 1, 1, 1, 1, 1, 1, 1, 1, 1, 1, 1, 1, 1, 1, 1, 1, 1, 1, 1, 1, 1, 1, 1, 1, 1, 1, 1, 1, 1, 1, 1, 1, 1, 1, 1, 1, 1, 1, 1, 1, 1, 1, 1, 1, 1, 1, 1, 1, 1, 1, 1, 1, 1, 1, 1, 1, 1, 1, 1, 1, 1, 1, 1, 1, 1, 1, 1, 1, 1, 1, 1, 1, 1, 1, 1, 1, 1, 1, 1, 1, 1, 1, 1, 1, 1, 1, 1, 1, 1, 1, 1, 1, 1, 1, 1, 1, 1, 1, 1, 1, 1, 1, 1, 1, 4 ),
 ( 0.000000000000000000, 0.5000000000000000000, 1.000000000000000000 ),
 ( 0.000000000000000000, 0.002599878613971510263, 0.005208762566300055921, 0.007813076245110234588, 0.01041697056762492211, 0.01302017924898362516, 0.01562522799165661294, 0.01822895742955179393, 0.02083332403451576206, 0.02343772221867868391, 0.02604143078293654281, 0.02864626161639613477, 0.03124961764961396021, 0.03385452714844047750, 0.03645799780571232912, 0.03906266225314121432, 0.04166671052383312535, 0.04427076094224517699, 0.04687542278318937439, 0.04947889361195772356, 0.05208380280015859759, 0.05468715921365963767, 0.05729198803509916865, 0.05989568673917144287, 0.06250009379223495087, 0.06510449848632135494, 0.06770819839843210397, 0.07031302545632363288, 0.07291638160390327694, 0.07552129054917994244, 0.07812475961953217751, 0.08072942239586503033, 0.08333346963797970408, 0.08593751866472883194, 0.08854217935802578821, 0.09114564884740632145, 0.09375055680876714925, 0.09635391199924973893, 0.09895873945611717570, 0.1015624370353711836, 0.1041668426700886191, 0.1067712463110160465, 0.1093749448896196713, 0.1119797708301935452, 0.1145831257515418783, 0.1171880334468678037, 0.1197915013940491491, 0.1223961628153678316, 0.1250002090321265524, 0.1276042567216372492, 0.1302089163955687523, 0.1328123846563000476, 0.1354172914881497103, 0.1380206455552074885, 0.1406254717515977581, 0.1432291683081768907, 0.1458335726268597532, 0.1484379753169847160, 0.1510416726638619811, 0.1536464975900906083, 0.1562498513865758776, 0.1588547579349887939, 0.1614582248604825021, 0.1640628850295551278, 0.1666669303230295940, 0.1692709767774011609, 0.1718756355346959253, 0.1744791026682601387, 0.1770840084736199360, 0.1796873615186004858, 0.1822921865574477218, 0.1848958821930496710, 0.1875002852981585977, 0.1901046871399069693, 0.1927083833567690418, 0.1953132073715553307, 0.1979165601445126987, 0.2005214656490191816, 0.2031249316542690642, 0.2057295906738217384, 0.2083336351460475244, 0.2109376804673406547, 0.2135423384106908962, 0.2161458045185324639, 0.2187507094003866837, 0.2213540615246011867, 0.2239588855088016361, 0.2265625803250888304, 0.2291669823190463362, 0.2317713834148095453, 0.2343750786033309830, 0.2369799018095430365, 0.2395832536602726381, 0.2421881582238437913, 0.2447916234102597566, 0.2473962813829825302, 0.2500003251359625422, 0.2526043694262022354, 0.2552090266582678346, 0.2578124918417971090, 0.2604173959030967600, 0.2630207472078238129, 0.2656255702402394725, 0.2682292643388430320, 0.2708336653240377978, 0.2734380657761767419, 0.2760417600379992398, 0.2786465825384744077, 0.2812499335682448476, 0.2838548372938197173, 0.2864583017627815864, 0.2890629587913320364, 0.2916670019270400371, 0.2942710452882197347, 0.2968757019116316509, 0.2994791662722288139, 0.3020840696158954564, 0.3046874202023847622, 0.3072922423858477359, 0.3098959358683710530, 0.3125003359471613118, 0.3151047358580104651, 0.3177084292947467969, 0.3203132511922952008, 0.3229166015023476888, 0.3255215044928377321, 0.3281249683456989308, 0.3307296245327063788, 0.3333336671530912065, 0.3359377096871765112, 0.3385423658045411677, 0.3411458294435600336, 0.3437507321724898035, 0.3463540821419661686, 0.3489589035792820537, 0.3515625965473047621, 0.3541669958220223235, 0.3567713952938928457, 0.3593750880071304721, 0.3619799094045394461, 0.3645832590960911834, 0.3671881614543835437, 0.3697916247924753486, 0.3723962802405443862, 0.3750003224475334518, 0.3776043642564660408, 0.3802090199703688222, 0.3828124829891406122, 0.3854173852062082184, 0.3880207346598750218, 0.3906255554538268782, 0.3932292480089087938, 0.3958336465818629857, 0.3984380457170473289, 0.4010417378083525053, 0.4036465588083897882, 0.4062499079826380477, 0.4088548098116001062, 0.4114582727362346981, 0.4140629275479489335, 0.4166669694434522730, 0.4192710106291533956, 0.4218756660421624782, 0.4244791285419997062, 0.4270840303500617607, 0.4296873793891050619, 0.4322921996424575197, 0.4348958918861421385, 0.4375002898596233591, 0.4401046887603987101, 0.4427083803313200949, 0.4453132010367379379, 0.4479165497948640051, 0.4505214511973463787, 0.4531249138098211726, 0.4557295680877478938, 0.4583336097736617210, 0.4609376504380365280, 0.4635423056527069874, 0.4661457677349071238, 0.4687506692368063055, 0.4713540179623986193, 0.4739588377779012651, 0.4765625298117197040, 0.4791669272880037522, 0.4817713260566358624, 0.4843750172087082362, 0.4869798377222476216, 0.4895831861654201811, 0.4921880872442612742, 0.4947915496458628049, 0.4973962034925555886, 0.5000002450707665691, 0.5026042853157074441, 0.5052089404345847523, 0.5078124022004342208, 0.5104173034990032720, 0.5130206520123070657, 0.5156254714926987726, 0.5182291634181735995, 0.5208335604995248946, 0.5234379592382720769, 0.5260416500730202838, 0.5286464704974140894, 0.5312498187267931105, 0.5338547195848227789, 0.5364581818768299204, 0.5390628353948335727, 0.5416668769672219330, 0.5442709168946127107, 0.5468755720202369552, 0.5494790335710144635, 0.5520839347690799093, 0.5546872831712518215, 0.5572921024192640793, 0.5598957943379132551, 0.5625001911265891108, 0.5651045899377058479, 0.5677082805566486812, 0.5703131009946261765, 0.5729164491113668545, 0.5755213498514099024, 0.5781248121350983649, 0.5807294654269519185, 0.5833335070953961088, 0.5859375468071157389, 0.5885422020420250089, 0.5911456634790059894, 0.5937505646793920233, 0.5963539130715860281, 0.5989587321899475514, 0.6015624242032879820, 0.6041668208015419372, 0.6067712197872831004, 0.6093749102919370220, 0.6119797308462270324, 0.6145830789514836745, 0.6171879796763642956, 0.6197914420530098445, 0.6223960952212510556, 0.6250001370876311357, 0.6276041766855571247, 0.6302088321322918407, 0.6328122935567517260, 0.6354171948622837629, 0.6380205433456558328, 0.6406253624370956690, 0.6432290546466469250, 0.6458334511567334069, 0.6484378504193577530, 0.6510415409112403351, 0.6536463616845760161, 0.6562497098795055939, 0.6588546106920506462, 0.6614580732629331550, 0.6640627264101022220, 0.6666667685763031370, 0.6692708081623160998, 0.6718754639234225667, 0.6744789254366408970, 0.6770838269501499029, 0.6796871756258610064, 0.6822919947931124218, 0.6848956873004010681, 0.6875000838245786117, 0.6901044834663523364, 0.6927081740469867022, 0.6953129951421085364, 0.6979163435278744609, 0.7005212445309179081, 0.7031247073973251327, 0.7057293606259679164, 0.7083334031938842701, 0.7109374428698714832, 0.7135420990479055536, 0.7161455607511696408, 0.7187504625754957965, 0.7213538115447158949, 0.7239586308905210377, 0.7265623237970838533, 0.7291667204376187650, 0.7317711205608201652, 0.7343748113317387638, 0.7369796328513985584, 0.7395829815291747877, 0.7421878828255610294, 0.7447913460887924941, 0.7473959995014650692, 0.7500000425730045661, 0.7526040824408628538, 0.7552087391383944803, 0.7578122011330034047, 0.7604171033709996586, 0.7630204527349119248, 0.7656252723620247114, 0.7682289657694127971, 0.7708333626285834850, 0.7734377633355060677, 0.7760414543982535607, 0.7786462764452187768, 0.7812496255161931469, 0.7838545272087811266, 0.7864579909701516769, 0.7890626446694239959, 0.7916666883465109938, 0.7942707285081521684, 0.7968753858277685120, 0.7994788482150362308, 0.8020837509695725176, 0.8046871008293766669, 0.8072919208405671121, 0.8098956148503495545, 0.8125000120304503026, 0.8151044134234068927, 0.8177081048795449281, 0.8203129275566022338, 0.8229162771219805661, 0.8255211793136476572, 0.8281246436744912343, 0.8307292977629509023, 0.8333333421475307423, 0.8359373827048843797, 0.8385420407491936956, 0.8411455036304537058, 0.8437504070044209437, 0.8463537574613370085, 0.8489585779593948889, 0.8515622726731627568, 0.8541666702765071673, 0.8567710724578335713, 0.8593747644089445581, 0.8619795878189033811, 0.8645829379799131464, 0.8671878407735589267, 0.8697913058352330085, 0.8723959604154888359, 0.8750000056095312839, 0.8776040466645483873, 0.8802087055361843548, 0.8828121690127931354, 0.8854170731091063340, 0.8880204242643787715, 0.8906252453521178447, 0.8932289408714879642, 0.8958333390004131758, 0.8984377420724726226, 0.9010414346201626179, 0.9036462588658594752, 0.9062496097237539017, 0.9088545132223035949, 0.9114579790861923048, 0.9140626342608790811, 0.9166666803663815477, 0.9192707220210388774, 0.9218753818226663732, 0.9244788459960084914, 0.9270837509176034219, 0.9296871028724987829, 0.9322919246527909820, 0.9348956210794385768, 0.9375000198362011261, 0.9401044239011964176, 0.9427081171475072408, 0.9453129423329229564, 0.9479162939871883520, 0.9505211982878988275, 0.9531246650646376661, 0.9557293209618126228, 0.9583333680330715643, 0.9609374102905526849, 0.9635420713365114853, 0.9661455366701111602, 0.9687504417289087844, 0.9713537931426093897, 0.9739586182492501187, 0.9765623229037746489, 0.9791667147516245340, 0.9817710778420317697, 0.9843748014325267581, 0.9869798465897002826, 0.9895830499482988207, 0.9921869381715581193, 0.9947912477285243416, 0.9974001254724073062, 1.000000000000000000 ),
 .UNSPECIFIED. ) 
 GEOMETRIC_REPRESENTATION_ITEM ( )  RATIONAL_B_SPLINE_SURFACE ( (
 ( 1.000000000000000222, 1.000000000000000222, 1.000000000000000222, 1.000000000000000222, 1.000000000000000444, 1.000000000000000000, 1.000000000000000666, 0.9999999999999997780, 1.000000000000000444, 1.000000000000000000, 1.000000000000000444, 1.000000000000000444, 1.000000000000000000, 1.000000000000000444, 1.000000000000000000, 1.000000000000000444, 1.000000000000000222, 1.000000000000000222, 1.000000000000000222, 1.000000000000000444, 1.000000000000000444, 1.000000000000000000, 1.000000000000000444, 1.000000000000000000, 1.000000000000000222, 1.000000000000000222, 1.000000000000000444, 1.000000000000000222, 1.000000000000000222, 1.000000000000000444, 1.000000000000000444, 1.000000000000000444, 1.000000000000000000, 1.000000000000000444, 1.000000000000000444, 1.000000000000000000, 1.000000000000000444, 1.000000000000000444, 1.000000000000000000, 1.000000000000000444, 1.000000000000000444, 1.000000000000000000, 1.000000000000000222, 1.000000000000000444, 1.000000000000000222, 1.000000000000000222, 1.000000000000000000, 1.000000000000000444, 1.000000000000000222, 1.000000000000000222, 1.000000000000000222, 1.000000000000000222, 1.000000000000000222, 1.000000000000000222, 1.000000000000000444, 1.000000000000000000, 1.000000000000000444, 0.9999999999999997780, 1.000000000000000666, 1.000000000000000444, 1.000000000000000444, 1.000000000000000000, 1.000000000000000444, 1.000000000000000222, 1.000000000000000222, 1.000000000000000444, 1.000000000000000222, 1.000000000000000444, 1.000000000000000000, 1.000000000000000444, 1.000000000000000222, 1.000000000000000444, 1.000000000000000444, 1.000000000000000222, 1.000000000000000222, 1.000000000000000222, 1.000000000000000444, 0.9999999999999997780, 1.000000000000000444, 1.000000000000000000, 1.000000000000000444, 1.000000000000000000, 1.000000000000000444, 0.9999999999999997780, 1.000000000000000444, 0.9999999999999997780, 1.000000000000000444, 1.000000000000000222, 1.000000000000000444, 1.000000000000000000, 1.000000000000000222, 1.000000000000000444, 1.000000000000000444, 1.000000000000000222, 1.000000000000000444, 1.000000000000000444, 1.000000000000000222, 1.000000000000000222, 1.000000000000000222, 1.000000000000000222, 1.000000000000000000, 1.000000000000000222, 1.000000000000000222, 1.000000000000000222, 1.000000000000000444, 1.000000000000000000, 1.000000000000000444, 0.9999999999999997780, 1.000000000000000666, 1.000000000000000222, 1.000000000000000444, 1.000000000000000000, 1.000000000000000444, 1.000000000000000222, 1.000000000000000222, 1.000000000000000444, 1.000000000000000000, 1.000000000000000000, 1.000000000000000444, 1.000000000000000000, 1.000000000000000444, 1.000000000000000000, 1.000000000000000444, 1.000000000000000222, 1.000000000000000444, 1.000000000000000222, 1.000000000000000444, 1.000000000000000222, 1.000000000000000444, 1.000000000000000000, 1.000000000000000444, 1.000000000000000222, 1.000000000000000444, 1.000000000000000000, 1.000000000000000444, 1.000000000000000000, 1.000000000000000444, 1.000000000000000000, 1.000000000000000444, 1.000000000000000222, 1.000000000000000444, 1.000000000000000222, 1.000000000000000444, 0.9999999999999997780, 1.000000000000000444, 1.000000000000000000, 1.000000000000000444, 1.000000000000000222, 1.000000000000000222, 1.000000000000000222, 1.000000000000000222, 1.000000000000000444, 0.9999999999999997780, 1.000000000000000444, 1.000000000000000000, 1.000000000000000000, 1.000000000000000222, 1.000000000000000222, 1.000000000000000666, 0.9999999999999997780, 1.000000000000000000, 1.000000000000000444, 1.000000000000000222, 1.000000000000000444, 1.000000000000000000, 1.000000000000000222, 1.000000000000000444, 1.000000000000000222, 1.000000000000000000, 1.000000000000000444, 1.000000000000000222, 1.000000000000000222, 1.000000000000000444, 1.000000000000000222, 1.000000000000000000, 1.000000000000000444, 1.000000000000000000, 1.000000000000000444, 1.000000000000000222, 1.000000000000000222, 1.000000000000000444, 0.9999999999999997780, 1.000000000000000444, 0.9999999999999997780, 1.000000000000000444, 1.000000000000000222, 1.000000000000000444, 1.000000000000000222, 1.000000000000000222, 1.000000000000000444, 1.000000000000000000, 1.000000000000000222, 1.000000000000000444, 1.000000000000000000, 1.000000000000000444, 1.000000000000000000, 1.000000000000000222, 1.000000000000000444, 1.000000000000000000, 1.000000000000000444, 0.9999999999999997780, 1.000000000000000444, 1.000000000000000222, 1.000000000000000444, 1.000000000000000000, 1.000000000000000000, 1.000000000000000444, 1.000000000000000000, 1.000000000000000222, 1.000000000000000444, 1.000000000000000222, 1.000000000000000444, 1.000000000000000222, 1.000000000000000444, 1.000000000000000444, 1.000000000000000444, 1.000000000000000000, 1.000000000000000444, 1.000000000000000222, 1.000000000000000444, 1.000000000000000222, 1.000000000000000000, 1.000000000000000222, 1.000000000000000444, 1.000000000000000222, 1.000000000000000444, 1.000000000000000000, 1.000000000000000222, 1.000000000000000000, 1.000000000000000444, 1.000000000000000000, 1.000000000000000444, 1.000000000000000444, 1.000000000000000444, 1.000000000000000444, 1.000000000000000000, 1.000000000000000222, 1.000000000000000444, 1.000000000000000000, 1.000000000000000444, 1.000000000000000444, 1.000000000000000444, 1.000000000000000222, 1.000000000000000222, 1.000000000000000222, 0.9999999999999997780, 1.000000000000000444, 1.000000000000000222, 1.000000000000000222, 1.000000000000000000, 1.000000000000000444, 1.000000000000000000, 1.000000000000000444, 1.000000000000000000, 1.000000000000000000, 1.000000000000000666, 1.000000000000000000, 1.000000000000000444, 1.000000000000000000, 1.000000000000000444, 1.000000000000000222, 0.9999999999999997780, 1.000000000000000444, 1.000000000000000000, 1.000000000000000444, 1.000000000000000222, 1.000000000000000444, 1.000000000000000222, 1.000000000000000222, 1.000000000000000444, 1.000000000000000000, 1.000000000000000222, 1.000000000000000444, 1.000000000000000222, 1.000000000000000000, 1.000000000000000444, 0.9999999999999997780, 1.000000000000000444, 1.000000000000000222, 1.000000000000000222, 1.000000000000000222, 1.000000000000000000, 1.000000000000000444, 1.000000000000000222, 1.000000000000000666, 0.9999999999999997780, 1.000000000000000444, 1.000000000000000222, 1.000000000000000000, 1.000000000000000222, 1.000000000000000444, 1.000000000000000222, 1.000000000000000000, 1.000000000000000444, 1.000000000000000222, 1.000000000000000444, 1.000000000000000000, 1.000000000000000444, 1.000000000000000222, 1.000000000000000444, 1.000000000000000222, 1.000000000000000222, 1.000000000000000444, 1.000000000000000222, 1.000000000000000444, 1.000000000000000000, 1.000000000000000444, 1.000000000000000222, 1.000000000000000222, 1.000000000000000000, 1.000000000000000666, 0.9999999999999997780, 1.000000000000000444, 1.000000000000000222, 1.000000000000000444, 1.000000000000000222, 1.000000000000000444, 1.000000000000000000, 1.000000000000000444, 1.000000000000000222, 1.000000000000000222, 1.000000000000000444, 1.000000000000000222, 1.000000000000000444, 1.000000000000000000, 1.000000000000000444, 1.000000000000000444, 0.9999999999999997780, 1.000000000000000444, 1.000000000000000000, 1.000000000000000444, 1.000000000000000444, 1.000000000000000222, 1.000000000000000000, 1.000000000000000444, 1.000000000000000222, 1.000000000000000444, 1.000000000000000000, 1.000000000000000444, 1.000000000000000222, 1.000000000000000444, 1.000000000000000222, 1.000000000000000444, 1.000000000000000222, 1.000000000000000222, 1.000000000000000444, 1.000000000000000444, 1.000000000000000000, 1.000000000000000444, 0.9999999999999997780, 1.000000000000000444, 1.000000000000000222, 1.000000000000000222, 1.000000000000000222, 1.000000000000000444, 1.000000000000000222, 1.000000000000000222, 1.000000000000000444, 1.000000000000000000, 1.000000000000000444, 1.000000000000000000, 1.000000000000000444, 1.000000000000000222, 1.000000000000000000, 1.000000000000000222, 1.000000000000000444, 1.000000000000000000, 1.000000000000000444, 1.000000000000000000, 1.000000000000000444, 1.000000000000000444, 1.000000000000000000, 1.000000000000000444, 1.000000000000000000, 1.000000000000000444, 1.000000000000000000, 1.000000000000000444, 1.000000000000000000, 1.000000000000000444, 1.000000000000000000, 1.000000000000000444, 1.000000000000000000, 1.000000000000000444, 1.000000000000000222, 1.000000000000000222, 1.000000000000000222, 1.000000000000000222),
 ( 0.3333333333333334259, 0.3333333333333334259, 0.3333333333333333703, 0.3333333333333334259, 0.3333333333333334814, 0.3333333333333333148, 0.3333333333333335924, 0.3333333333333333148, 0.3333333333333334259, 0.3333333333333333703, 0.3333333333333334814, 0.3333333333333334814, 0.3333333333333333148, 0.3333333333333334814, 0.3333333333333333703, 0.3333333333333334259, 0.3333333333333334259, 0.3333333333333333703, 0.3333333333333334814, 0.3333333333333334259, 0.3333333333333335369, 0.3333333333333333148, 0.3333333333333335369, 0.3333333333333333703, 0.3333333333333333703, 0.3333333333333334259, 0.3333333333333334814, 0.3333333333333334814, 0.3333333333333333148, 0.3333333333333335369, 0.3333333333333335924, 0.3333333333333334259, 0.3333333333333333703, 0.3333333333333335369, 0.3333333333333334259, 0.3333333333333334259, 0.3333333333333334814, 0.3333333333333335369, 0.3333333333333333703, 0.3333333333333334259, 0.3333333333333335369, 0.3333333333333333148, 0.3333333333333334259, 0.3333333333333335369, 0.3333333333333333703, 0.3333333333333334259, 0.3333333333333333703, 0.3333333333333335369, 0.3333333333333333703, 0.3333333333333334814, 0.3333333333333333703, 0.3333333333333334259, 0.3333333333333333703, 0.3333333333333333703, 0.3333333333333334259, 0.3333333333333333703, 0.3333333333333334259, 0.3333333333333333148, 0.3333333333333336479, 0.3333333333333334259, 0.3333333333333334814, 0.3333333333333333703, 0.3333333333333335369, 0.3333333333333334259, 0.3333333333333334259, 0.3333333333333334259, 0.3333333333333334259, 0.3333333333333333703, 0.3333333333333333703, 0.3333333333333335369, 0.3333333333333333703, 0.3333333333333335369, 0.3333333333333334259, 0.3333333333333333703, 0.3333333333333334814, 0.3333333333333334259, 0.3333333333333333703, 0.3333333333333333148, 0.3333333333333335369, 0.3333333333333333703, 0.3333333333333335369, 0.3333333333333333703, 0.3333333333333334814, 0.3333333333333333703, 0.3333333333333334259, 0.3333333333333333148, 0.3333333333333335369, 0.3333333333333333703, 0.3333333333333334814, 0.3333333333333333148, 0.3333333333333334814, 0.3333333333333334259, 0.3333333333333335369, 0.3333333333333334259, 0.3333333333333334814, 0.3333333333333334259, 0.3333333333333334259, 0.3333333333333334259, 0.3333333333333334259, 0.3333333333333333703, 0.3333333333333333703, 0.3333333333333334814, 0.3333333333333333703, 0.3333333333333333703, 0.3333333333333335369, 0.3333333333333332593, 0.3333333333333335369, 0.3333333333333332593, 0.3333333333333335924, 0.3333333333333334259, 0.3333333333333334814, 0.3333333333333333703, 0.3333333333333334814, 0.3333333333333334259, 0.3333333333333334259, 0.3333333333333334814, 0.3333333333333333703, 0.3333333333333333703, 0.3333333333333334814, 0.3333333333333333703, 0.3333333333333334814, 0.3333333333333333703, 0.3333333333333334259, 0.3333333333333334259, 0.3333333333333335369, 0.3333333333333333703, 0.3333333333333335369, 0.3333333333333334259, 0.3333333333333335369, 0.3333333333333334259, 0.3333333333333334259, 0.3333333333333334814, 0.3333333333333334814, 0.3333333333333333703, 0.3333333333333334814, 0.3333333333333333148, 0.3333333333333335369, 0.3333333333333333148, 0.3333333333333335369, 0.3333333333333334259, 0.3333333333333334259, 0.3333333333333334814, 0.3333333333333334814, 0.3333333333333333703, 0.3333333333333335369, 0.3333333333333333703, 0.3333333333333334259, 0.3333333333333334814, 0.3333333333333334814, 0.3333333333333334259, 0.3333333333333334259, 0.3333333333333335369, 0.3333333333333333148, 0.3333333333333335924, 0.3333333333333333703, 0.3333333333333333703, 0.3333333333333335369, 0.3333333333333333703, 0.3333333333333335924, 0.3333333333333333148, 0.3333333333333333703, 0.3333333333333334814, 0.3333333333333333703, 0.3333333333333335369, 0.3333333333333333703, 0.3333333333333334259, 0.3333333333333334814, 0.3333333333333333703, 0.3333333333333334259, 0.3333333333333334259, 0.3333333333333334259, 0.3333333333333334814, 0.3333333333333333703, 0.3333333333333334259, 0.3333333333333333703, 0.3333333333333335369, 0.3333333333333333703, 0.3333333333333334259, 0.3333333333333334259, 0.3333333333333333703, 0.3333333333333334814, 0.3333333333333333703, 0.3333333333333334259, 0.3333333333333333703, 0.3333333333333334814, 0.3333333333333335369, 0.3333333333333334259, 0.3333333333333334259, 0.3333333333333333703, 0.3333333333333335369, 0.3333333333333333703, 0.3333333333333333703, 0.3333333333333335369, 0.3333333333333333703, 0.3333333333333335924, 0.3333333333333332593, 0.3333333333333335369, 0.3333333333333334259, 0.3333333333333333703, 0.3333333333333335369, 0.3333333333333333703, 0.3333333333333333703, 0.3333333333333334259, 0.3333333333333335369, 0.3333333333333333148, 0.3333333333333333703, 0.3333333333333335369, 0.3333333333333334259, 0.3333333333333333703, 0.3333333333333335369, 0.3333333333333333703, 0.3333333333333335924, 0.3333333333333333703, 0.3333333333333335369, 0.3333333333333334259, 0.3333333333333334814, 0.3333333333333334259, 0.3333333333333334259, 0.3333333333333334814, 0.3333333333333334259, 0.3333333333333334259, 0.3333333333333333148, 0.3333333333333333703, 0.3333333333333334814, 0.3333333333333334814, 0.3333333333333334259, 0.3333333333333333703, 0.3333333333333334259, 0.3333333333333333148, 0.3333333333333335369, 0.3333333333333333703, 0.3333333333333334814, 0.3333333333333335369, 0.3333333333333335369, 0.3333333333333335369, 0.3333333333333333703, 0.3333333333333334259, 0.3333333333333334259, 0.3333333333333333148, 0.3333333333333335369, 0.3333333333333334259, 0.3333333333333334259, 0.3333333333333334259, 0.3333333333333334814, 0.3333333333333334259, 0.3333333333333333148, 0.3333333333333334814, 0.3333333333333334259, 0.3333333333333333703, 0.3333333333333333703, 0.3333333333333334814, 0.3333333333333333703, 0.3333333333333334814, 0.3333333333333334814, 0.3333333333333333148, 0.3333333333333335924, 0.3333333333333333148, 0.3333333333333335369, 0.3333333333333333148, 0.3333333333333335924, 0.3333333333333333703, 0.3333333333333333148, 0.3333333333333334259, 0.3333333333333334259, 0.3333333333333334259, 0.3333333333333333703, 0.3333333333333334814, 0.3333333333333333703, 0.3333333333333334814, 0.3333333333333334814, 0.3333333333333333703, 0.3333333333333334259, 0.3333333333333334259, 0.3333333333333334814, 0.3333333333333333703, 0.3333333333333333703, 0.3333333333333334259, 0.3333333333333334259, 0.3333333333333333703, 0.3333333333333334259, 0.3333333333333333703, 0.3333333333333334259, 0.3333333333333334259, 0.3333333333333333703, 0.3333333333333335924, 0.3333333333333332593, 0.3333333333333335369, 0.3333333333333334259, 0.3333333333333333703, 0.3333333333333333148, 0.3333333333333335924, 0.3333333333333333148, 0.3333333333333333703, 0.3333333333333334259, 0.3333333333333334814, 0.3333333333333335369, 0.3333333333333333703, 0.3333333333333334259, 0.3333333333333333703, 0.3333333333333335369, 0.3333333333333333703, 0.3333333333333334259, 0.3333333333333334814, 0.3333333333333333703, 0.3333333333333335369, 0.3333333333333333148, 0.3333333333333335369, 0.3333333333333334259, 0.3333333333333334259, 0.3333333333333333703, 0.3333333333333335369, 0.3333333333333333703, 0.3333333333333335369, 0.3333333333333334814, 0.3333333333333333703, 0.3333333333333334814, 0.3333333333333333703, 0.3333333333333333703, 0.3333333333333335369, 0.3333333333333333703, 0.3333333333333334259, 0.3333333333333334814, 0.3333333333333333703, 0.3333333333333334259, 0.3333333333333333148, 0.3333333333333335369, 0.3333333333333334259, 0.3333333333333333703, 0.3333333333333334814, 0.3333333333333334259, 0.3333333333333334814, 0.3333333333333334259, 0.3333333333333333703, 0.3333333333333333703, 0.3333333333333334259, 0.3333333333333334259, 0.3333333333333334259, 0.3333333333333334259, 0.3333333333333333703, 0.3333333333333334814, 0.3333333333333334814, 0.3333333333333333703, 0.3333333333333335369, 0.3333333333333333703, 0.3333333333333334814, 0.3333333333333334814, 0.3333333333333335369, 0.3333333333333333148, 0.3333333333333335369, 0.3333333333333333703, 0.3333333333333333148, 0.3333333333333334814, 0.3333333333333333703, 0.3333333333333334814, 0.3333333333333333703, 0.3333333333333334814, 0.3333333333333333703, 0.3333333333333335369, 0.3333333333333333703, 0.3333333333333334814, 0.3333333333333334259, 0.3333333333333334814, 0.3333333333333334259, 0.3333333333333333703, 0.3333333333333333703, 0.3333333333333334814, 0.3333333333333334259, 0.3333333333333334814, 0.3333333333333334259, 0.3333333333333334259, 0.3333333333333334259, 0.3333333333333333703, 0.3333333333333334259, 0.3333333333333333703, 0.3333333333333334814, 0.3333333333333333148, 0.3333333333333335369, 0.3333333333333333703, 0.3333333333333334814, 0.3333333333333333703, 0.3333333333333335369, 0.3333333333333334259, 0.3333333333333334259, 0.3333333333333334259, 0.3333333333333334259, 0.3333333333333334259, 0.3333333333333334259),
 ( 0.3333333333333334259, 0.3333333333333334259, 0.3333333333333333703, 0.3333333333333334259, 0.3333333333333334814, 0.3333333333333333148, 0.3333333333333335924, 0.3333333333333333148, 0.3333333333333334259, 0.3333333333333333703, 0.3333333333333334814, 0.3333333333333334814, 0.3333333333333333148, 0.3333333333333334814, 0.3333333333333333703, 0.3333333333333334259, 0.3333333333333334259, 0.3333333333333333703, 0.3333333333333334814, 0.3333333333333334259, 0.3333333333333335369, 0.3333333333333333148, 0.3333333333333335369, 0.3333333333333333703, 0.3333333333333333703, 0.3333333333333334259, 0.3333333333333334814, 0.3333333333333334814, 0.3333333333333333148, 0.3333333333333335369, 0.3333333333333335924, 0.3333333333333334259, 0.3333333333333333703, 0.3333333333333335369, 0.3333333333333334259, 0.3333333333333334259, 0.3333333333333334814, 0.3333333333333335369, 0.3333333333333333703, 0.3333333333333334259, 0.3333333333333335369, 0.3333333333333333148, 0.3333333333333334259, 0.3333333333333335369, 0.3333333333333333703, 0.3333333333333334259, 0.3333333333333333703, 0.3333333333333335369, 0.3333333333333333703, 0.3333333333333334814, 0.3333333333333333703, 0.3333333333333334259, 0.3333333333333333703, 0.3333333333333333703, 0.3333333333333334259, 0.3333333333333333703, 0.3333333333333334259, 0.3333333333333333148, 0.3333333333333336479, 0.3333333333333334259, 0.3333333333333334814, 0.3333333333333333703, 0.3333333333333335369, 0.3333333333333334259, 0.3333333333333334259, 0.3333333333333334259, 0.3333333333333334259, 0.3333333333333333703, 0.3333333333333333703, 0.3333333333333335369, 0.3333333333333333703, 0.3333333333333335369, 0.3333333333333334259, 0.3333333333333333703, 0.3333333333333334814, 0.3333333333333334259, 0.3333333333333333703, 0.3333333333333333148, 0.3333333333333335369, 0.3333333333333333703, 0.3333333333333335369, 0.3333333333333333703, 0.3333333333333334814, 0.3333333333333333703, 0.3333333333333334259, 0.3333333333333333148, 0.3333333333333335369, 0.3333333333333333703, 0.3333333333333334814, 0.3333333333333333148, 0.3333333333333334814, 0.3333333333333334259, 0.3333333333333335369, 0.3333333333333334259, 0.3333333333333334814, 0.3333333333333334259, 0.3333333333333334259, 0.3333333333333334259, 0.3333333333333334259, 0.3333333333333333703, 0.3333333333333333703, 0.3333333333333334814, 0.3333333333333333703, 0.3333333333333333703, 0.3333333333333335369, 0.3333333333333332593, 0.3333333333333335369, 0.3333333333333332593, 0.3333333333333335924, 0.3333333333333334259, 0.3333333333333334814, 0.3333333333333333703, 0.3333333333333334814, 0.3333333333333334259, 0.3333333333333334259, 0.3333333333333334814, 0.3333333333333333703, 0.3333333333333333703, 0.3333333333333334814, 0.3333333333333333703, 0.3333333333333334814, 0.3333333333333333703, 0.3333333333333334259, 0.3333333333333334259, 0.3333333333333335369, 0.3333333333333333703, 0.3333333333333335369, 0.3333333333333334259, 0.3333333333333335369, 0.3333333333333334259, 0.3333333333333334259, 0.3333333333333334814, 0.3333333333333334814, 0.3333333333333333703, 0.3333333333333334814, 0.3333333333333333148, 0.3333333333333335369, 0.3333333333333333148, 0.3333333333333335369, 0.3333333333333334259, 0.3333333333333334259, 0.3333333333333334814, 0.3333333333333334814, 0.3333333333333333703, 0.3333333333333335369, 0.3333333333333333703, 0.3333333333333334259, 0.3333333333333334814, 0.3333333333333334814, 0.3333333333333334259, 0.3333333333333334259, 0.3333333333333335369, 0.3333333333333333148, 0.3333333333333335924, 0.3333333333333333703, 0.3333333333333333703, 0.3333333333333335369, 0.3333333333333333703, 0.3333333333333335924, 0.3333333333333333148, 0.3333333333333333703, 0.3333333333333334814, 0.3333333333333333703, 0.3333333333333335369, 0.3333333333333333703, 0.3333333333333334259, 0.3333333333333334814, 0.3333333333333333703, 0.3333333333333334259, 0.3333333333333334259, 0.3333333333333334259, 0.3333333333333334814, 0.3333333333333333703, 0.3333333333333334259, 0.3333333333333333703, 0.3333333333333335369, 0.3333333333333333703, 0.3333333333333334259, 0.3333333333333334259, 0.3333333333333333703, 0.3333333333333334814, 0.3333333333333333703, 0.3333333333333334259, 0.3333333333333333703, 0.3333333333333334814, 0.3333333333333335369, 0.3333333333333334259, 0.3333333333333334259, 0.3333333333333333703, 0.3333333333333335369, 0.3333333333333333703, 0.3333333333333333703, 0.3333333333333335369, 0.3333333333333333703, 0.3333333333333335924, 0.3333333333333332593, 0.3333333333333335369, 0.3333333333333334259, 0.3333333333333333703, 0.3333333333333335369, 0.3333333333333333703, 0.3333333333333333703, 0.3333333333333334259, 0.3333333333333335369, 0.3333333333333333148, 0.3333333333333333703, 0.3333333333333335369, 0.3333333333333334259, 0.3333333333333333703, 0.3333333333333335369, 0.3333333333333333703, 0.3333333333333335924, 0.3333333333333333703, 0.3333333333333335369, 0.3333333333333334259, 0.3333333333333334814, 0.3333333333333334259, 0.3333333333333334259, 0.3333333333333334814, 0.3333333333333334259, 0.3333333333333334259, 0.3333333333333333148, 0.3333333333333333703, 0.3333333333333334814, 0.3333333333333334814, 0.3333333333333334259, 0.3333333333333333703, 0.3333333333333334259, 0.3333333333333333148, 0.3333333333333335369, 0.3333333333333333703, 0.3333333333333334814, 0.3333333333333335369, 0.3333333333333335369, 0.3333333333333335369, 0.3333333333333333703, 0.3333333333333334259, 0.3333333333333334259, 0.3333333333333333148, 0.3333333333333335369, 0.3333333333333334259, 0.3333333333333334259, 0.3333333333333334259, 0.3333333333333334814, 0.3333333333333334259, 0.3333333333333333148, 0.3333333333333334814, 0.3333333333333334259, 0.3333333333333333703, 0.3333333333333333703, 0.3333333333333334814, 0.3333333333333333703, 0.3333333333333334814, 0.3333333333333334814, 0.3333333333333333148, 0.3333333333333335924, 0.3333333333333333148, 0.3333333333333335369, 0.3333333333333333148, 0.3333333333333335924, 0.3333333333333333703, 0.3333333333333333148, 0.3333333333333334259, 0.3333333333333334259, 0.3333333333333334259, 0.3333333333333333703, 0.3333333333333334814, 0.3333333333333333703, 0.3333333333333334814, 0.3333333333333334814, 0.3333333333333333703, 0.3333333333333334259, 0.3333333333333334259, 0.3333333333333334814, 0.3333333333333333703, 0.3333333333333333703, 0.3333333333333334259, 0.3333333333333334259, 0.3333333333333333703, 0.3333333333333334259, 0.3333333333333333703, 0.3333333333333334259, 0.3333333333333334259, 0.3333333333333333703, 0.3333333333333335924, 0.3333333333333332593, 0.3333333333333335369, 0.3333333333333334259, 0.3333333333333333703, 0.3333333333333333148, 0.3333333333333335924, 0.3333333333333333148, 0.3333333333333333703, 0.3333333333333334259, 0.3333333333333334814, 0.3333333333333335369, 0.3333333333333333703, 0.3333333333333334259, 0.3333333333333333703, 0.3333333333333335369, 0.3333333333333333703, 0.3333333333333334259, 0.3333333333333334814, 0.3333333333333333703, 0.3333333333333335369, 0.3333333333333333148, 0.3333333333333335369, 0.3333333333333334259, 0.3333333333333334259, 0.3333333333333333703, 0.3333333333333335369, 0.3333333333333333703, 0.3333333333333335369, 0.3333333333333334814, 0.3333333333333333703, 0.3333333333333334814, 0.3333333333333333703, 0.3333333333333333703, 0.3333333333333335369, 0.3333333333333333703, 0.3333333333333334259, 0.3333333333333334814, 0.3333333333333333703, 0.3333333333333334259, 0.3333333333333333148, 0.3333333333333335369, 0.3333333333333334259, 0.3333333333333333703, 0.3333333333333334814, 0.3333333333333334259, 0.3333333333333334814, 0.3333333333333334259, 0.3333333333333333703, 0.3333333333333333703, 0.3333333333333334259, 0.3333333333333334259, 0.3333333333333334259, 0.3333333333333334259, 0.3333333333333333703, 0.3333333333333334814, 0.3333333333333334814, 0.3333333333333333703, 0.3333333333333335369, 0.3333333333333333703, 0.3333333333333334814, 0.3333333333333334814, 0.3333333333333335369, 0.3333333333333333148, 0.3333333333333335369, 0.3333333333333333703, 0.3333333333333333148, 0.3333333333333334814, 0.3333333333333333703, 0.3333333333333334814, 0.3333333333333333703, 0.3333333333333334814, 0.3333333333333333703, 0.3333333333333335369, 0.3333333333333333703, 0.3333333333333334814, 0.3333333333333334259, 0.3333333333333334814, 0.3333333333333334259, 0.3333333333333333703, 0.3333333333333333703, 0.3333333333333334814, 0.3333333333333334259, 0.3333333333333334814, 0.3333333333333334259, 0.3333333333333334259, 0.3333333333333334259, 0.3333333333333333703, 0.3333333333333334259, 0.3333333333333333703, 0.3333333333333334814, 0.3333333333333333148, 0.3333333333333335369, 0.3333333333333333703, 0.3333333333333334814, 0.3333333333333333703, 0.3333333333333335369, 0.3333333333333334259, 0.3333333333333334259, 0.3333333333333334259, 0.3333333333333334259, 0.3333333333333334259, 0.3333333333333334259),
 ( 1.000000000000000222, 1.000000000000000222, 1.000000000000000222, 1.000000000000000222, 1.000000000000000444, 1.000000000000000000, 1.000000000000000666, 0.9999999999999997780, 1.000000000000000444, 1.000000000000000000, 1.000000000000000444, 1.000000000000000444, 1.000000000000000000, 1.000000000000000444, 1.000000000000000000, 1.000000000000000444, 1.000000000000000222, 1.000000000000000222, 1.000000000000000222, 1.000000000000000444, 1.000000000000000444, 1.000000000000000000, 1.000000000000000444, 1.000000000000000000, 1.000000000000000222, 1.000000000000000222, 1.000000000000000444, 1.000000000000000222, 1.000000000000000222, 1.000000000000000444, 1.000000000000000444, 1.000000000000000444, 1.000000000000000000, 1.000000000000000444, 1.000000000000000444, 1.000000000000000000, 1.000000000000000444, 1.000000000000000444, 1.000000000000000000, 1.000000000000000444, 1.000000000000000444, 1.000000000000000000, 1.000000000000000222, 1.000000000000000444, 1.000000000000000222, 1.000000000000000222, 1.000000000000000000, 1.000000000000000444, 1.000000000000000222, 1.000000000000000222, 1.000000000000000222, 1.000000000000000222, 1.000000000000000222, 1.000000000000000222, 1.000000000000000444, 1.000000000000000000, 1.000000000000000444, 0.9999999999999997780, 1.000000000000000666, 1.000000000000000444, 1.000000000000000444, 1.000000000000000000, 1.000000000000000444, 1.000000000000000222, 1.000000000000000222, 1.000000000000000444, 1.000000000000000222, 1.000000000000000444, 1.000000000000000000, 1.000000000000000444, 1.000000000000000222, 1.000000000000000444, 1.000000000000000444, 1.000000000000000222, 1.000000000000000222, 1.000000000000000222, 1.000000000000000444, 0.9999999999999997780, 1.000000000000000444, 1.000000000000000000, 1.000000000000000444, 1.000000000000000000, 1.000000000000000444, 0.9999999999999997780, 1.000000000000000444, 0.9999999999999997780, 1.000000000000000444, 1.000000000000000222, 1.000000000000000444, 1.000000000000000000, 1.000000000000000222, 1.000000000000000444, 1.000000000000000444, 1.000000000000000222, 1.000000000000000444, 1.000000000000000444, 1.000000000000000222, 1.000000000000000222, 1.000000000000000222, 1.000000000000000222, 1.000000000000000000, 1.000000000000000222, 1.000000000000000222, 1.000000000000000222, 1.000000000000000444, 1.000000000000000000, 1.000000000000000444, 0.9999999999999997780, 1.000000000000000666, 1.000000000000000222, 1.000000000000000444, 1.000000000000000000, 1.000000000000000444, 1.000000000000000222, 1.000000000000000222, 1.000000000000000444, 1.000000000000000000, 1.000000000000000000, 1.000000000000000444, 1.000000000000000000, 1.000000000000000444, 1.000000000000000000, 1.000000000000000444, 1.000000000000000222, 1.000000000000000444, 1.000000000000000222, 1.000000000000000444, 1.000000000000000222, 1.000000000000000444, 1.000000000000000000, 1.000000000000000444, 1.000000000000000222, 1.000000000000000444, 1.000000000000000000, 1.000000000000000444, 1.000000000000000000, 1.000000000000000444, 1.000000000000000000, 1.000000000000000444, 1.000000000000000222, 1.000000000000000444, 1.000000000000000222, 1.000000000000000444, 0.9999999999999997780, 1.000000000000000444, 1.000000000000000000, 1.000000000000000444, 1.000000000000000222, 1.000000000000000222, 1.000000000000000222, 1.000000000000000222, 1.000000000000000444, 0.9999999999999997780, 1.000000000000000444, 1.000000000000000000, 1.000000000000000000, 1.000000000000000222, 1.000000000000000222, 1.000000000000000666, 0.9999999999999997780, 1.000000000000000000, 1.000000000000000444, 1.000000000000000222, 1.000000000000000444, 1.000000000000000000, 1.000000000000000222, 1.000000000000000444, 1.000000000000000222, 1.000000000000000000, 1.000000000000000444, 1.000000000000000222, 1.000000000000000222, 1.000000000000000444, 1.000000000000000222, 1.000000000000000000, 1.000000000000000444, 1.000000000000000000, 1.000000000000000444, 1.000000000000000222, 1.000000000000000222, 1.000000000000000444, 0.9999999999999997780, 1.000000000000000444, 0.9999999999999997780, 1.000000000000000444, 1.000000000000000222, 1.000000000000000444, 1.000000000000000222, 1.000000000000000222, 1.000000000000000444, 1.000000000000000000, 1.000000000000000222, 1.000000000000000444, 1.000000000000000000, 1.000000000000000444, 1.000000000000000000, 1.000000000000000222, 1.000000000000000444, 1.000000000000000000, 1.000000000000000444, 0.9999999999999997780, 1.000000000000000444, 1.000000000000000222, 1.000000000000000444, 1.000000000000000000, 1.000000000000000000, 1.000000000000000444, 1.000000000000000000, 1.000000000000000222, 1.000000000000000444, 1.000000000000000222, 1.000000000000000444, 1.000000000000000222, 1.000000000000000444, 1.000000000000000444, 1.000000000000000444, 1.000000000000000000, 1.000000000000000444, 1.000000000000000222, 1.000000000000000444, 1.000000000000000222, 1.000000000000000000, 1.000000000000000222, 1.000000000000000444, 1.000000000000000222, 1.000000000000000444, 1.000000000000000000, 1.000000000000000222, 1.000000000000000000, 1.000000000000000444, 1.000000000000000000, 1.000000000000000444, 1.000000000000000444, 1.000000000000000444, 1.000000000000000444, 1.000000000000000000, 1.000000000000000222, 1.000000000000000444, 1.000000000000000000, 1.000000000000000444, 1.000000000000000444, 1.000000000000000444, 1.000000000000000222, 1.000000000000000222, 1.000000000000000222, 0.9999999999999997780, 1.000000000000000444, 1.000000000000000222, 1.000000000000000222, 1.000000000000000000, 1.000000000000000444, 1.000000000000000000, 1.000000000000000444, 1.000000000000000000, 1.000000000000000000, 1.000000000000000666, 1.000000000000000000, 1.000000000000000444, 1.000000000000000000, 1.000000000000000444, 1.000000000000000222, 0.9999999999999997780, 1.000000000000000444, 1.000000000000000000, 1.000000000000000444, 1.000000000000000222, 1.000000000000000444, 1.000000000000000222, 1.000000000000000222, 1.000000000000000444, 1.000000000000000000, 1.000000000000000222, 1.000000000000000444, 1.000000000000000222, 1.000000000000000000, 1.000000000000000444, 0.9999999999999997780, 1.000000000000000444, 1.000000000000000222, 1.000000000000000222, 1.000000000000000222, 1.000000000000000000, 1.000000000000000444, 1.000000000000000222, 1.000000000000000666, 0.9999999999999997780, 1.000000000000000444, 1.000000000000000222, 1.000000000000000000, 1.000000000000000222, 1.000000000000000444, 1.000000000000000222, 1.000000000000000000, 1.000000000000000444, 1.000000000000000222, 1.000000000000000444, 1.000000000000000000, 1.000000000000000444, 1.000000000000000222, 1.000000000000000444, 1.000000000000000222, 1.000000000000000222, 1.000000000000000444, 1.000000000000000222, 1.000000000000000444, 1.000000000000000000, 1.000000000000000444, 1.000000000000000222, 1.000000000000000222, 1.000000000000000000, 1.000000000000000666, 0.9999999999999997780, 1.000000000000000444, 1.000000000000000222, 1.000000000000000444, 1.000000000000000222, 1.000000000000000444, 1.000000000000000000, 1.000000000000000444, 1.000000000000000222, 1.000000000000000222, 1.000000000000000444, 1.000000000000000222, 1.000000000000000444, 1.000000000000000000, 1.000000000000000444, 1.000000000000000444, 0.9999999999999997780, 1.000000000000000444, 1.000000000000000000, 1.000000000000000444, 1.000000000000000444, 1.000000000000000222, 1.000000000000000000, 1.000000000000000444, 1.000000000000000222, 1.000000000000000444, 1.000000000000000000, 1.000000000000000444, 1.000000000000000222, 1.000000000000000444, 1.000000000000000222, 1.000000000000000444, 1.000000000000000222, 1.000000000000000222, 1.000000000000000444, 1.000000000000000444, 1.000000000000000000, 1.000000000000000444, 0.9999999999999997780, 1.000000000000000444, 1.000000000000000222, 1.000000000000000222, 1.000000000000000222, 1.000000000000000444, 1.000000000000000222, 1.000000000000000222, 1.000000000000000444, 1.000000000000000000, 1.000000000000000444, 1.000000000000000000, 1.000000000000000444, 1.000000000000000222, 1.000000000000000000, 1.000000000000000222, 1.000000000000000444, 1.000000000000000000, 1.000000000000000444, 1.000000000000000000, 1.000000000000000444, 1.000000000000000444, 1.000000000000000000, 1.000000000000000444, 1.000000000000000000, 1.000000000000000444, 1.000000000000000000, 1.000000000000000444, 1.000000000000000000, 1.000000000000000444, 1.000000000000000000, 1.000000000000000444, 1.000000000000000000, 1.000000000000000444, 1.000000000000000222, 1.000000000000000222, 1.000000000000000222, 1.000000000000000222),
 ( 0.3333333333333334259, 0.3333333333333334259, 0.3333333333333333703, 0.3333333333333334259, 0.3333333333333334814, 0.3333333333333333148, 0.3333333333333335924, 0.3333333333333333148, 0.3333333333333334259, 0.3333333333333333703, 0.3333333333333334814, 0.3333333333333334814, 0.3333333333333333148, 0.3333333333333334814, 0.3333333333333333703, 0.3333333333333334259, 0.3333333333333334259, 0.3333333333333333703, 0.3333333333333334814, 0.3333333333333334259, 0.3333333333333335369, 0.3333333333333333148, 0.3333333333333335369, 0.3333333333333333703, 0.3333333333333333703, 0.3333333333333334259, 0.3333333333333334814, 0.3333333333333334814, 0.3333333333333333148, 0.3333333333333335369, 0.3333333333333335924, 0.3333333333333334259, 0.3333333333333333703, 0.3333333333333335369, 0.3333333333333334259, 0.3333333333333334259, 0.3333333333333334814, 0.3333333333333335369, 0.3333333333333333703, 0.3333333333333334259, 0.3333333333333335369, 0.3333333333333333148, 0.3333333333333334259, 0.3333333333333335369, 0.3333333333333333703, 0.3333333333333334259, 0.3333333333333333703, 0.3333333333333335369, 0.3333333333333333703, 0.3333333333333334814, 0.3333333333333333703, 0.3333333333333334259, 0.3333333333333333703, 0.3333333333333333703, 0.3333333333333334259, 0.3333333333333333703, 0.3333333333333334259, 0.3333333333333333148, 0.3333333333333336479, 0.3333333333333334259, 0.3333333333333334814, 0.3333333333333333703, 0.3333333333333335369, 0.3333333333333334259, 0.3333333333333334259, 0.3333333333333334259, 0.3333333333333334259, 0.3333333333333333703, 0.3333333333333333703, 0.3333333333333335369, 0.3333333333333333703, 0.3333333333333335369, 0.3333333333333334259, 0.3333333333333333703, 0.3333333333333334814, 0.3333333333333334259, 0.3333333333333333703, 0.3333333333333333148, 0.3333333333333335369, 0.3333333333333333703, 0.3333333333333335369, 0.3333333333333333703, 0.3333333333333334814, 0.3333333333333333703, 0.3333333333333334259, 0.3333333333333333148, 0.3333333333333335369, 0.3333333333333333703, 0.3333333333333334814, 0.3333333333333333148, 0.3333333333333334814, 0.3333333333333334259, 0.3333333333333335369, 0.3333333333333334259, 0.3333333333333334814, 0.3333333333333334259, 0.3333333333333334259, 0.3333333333333334259, 0.3333333333333334259, 0.3333333333333333703, 0.3333333333333333703, 0.3333333333333334814, 0.3333333333333333703, 0.3333333333333333703, 0.3333333333333335369, 0.3333333333333332593, 0.3333333333333335369, 0.3333333333333332593, 0.3333333333333335924, 0.3333333333333334259, 0.3333333333333334814, 0.3333333333333333703, 0.3333333333333334814, 0.3333333333333334259, 0.3333333333333334259, 0.3333333333333334814, 0.3333333333333333703, 0.3333333333333333703, 0.3333333333333334814, 0.3333333333333333703, 0.3333333333333334814, 0.3333333333333333703, 0.3333333333333334259, 0.3333333333333334259, 0.3333333333333335369, 0.3333333333333333703, 0.3333333333333335369, 0.3333333333333334259, 0.3333333333333335369, 0.3333333333333334259, 0.3333333333333334259, 0.3333333333333334814, 0.3333333333333334814, 0.3333333333333333703, 0.3333333333333334814, 0.3333333333333333148, 0.3333333333333335369, 0.3333333333333333148, 0.3333333333333335369, 0.3333333333333334259, 0.3333333333333334259, 0.3333333333333334814, 0.3333333333333334814, 0.3333333333333333703, 0.3333333333333335369, 0.3333333333333333703, 0.3333333333333334259, 0.3333333333333334814, 0.3333333333333334814, 0.3333333333333334259, 0.3333333333333334259, 0.3333333333333335369, 0.3333333333333333148, 0.3333333333333335924, 0.3333333333333333703, 0.3333333333333333703, 0.3333333333333335369, 0.3333333333333333703, 0.3333333333333335924, 0.3333333333333333148, 0.3333333333333333703, 0.3333333333333334814, 0.3333333333333333703, 0.3333333333333335369, 0.3333333333333333703, 0.3333333333333334259, 0.3333333333333334814, 0.3333333333333333703, 0.3333333333333334259, 0.3333333333333334259, 0.3333333333333334259, 0.3333333333333334814, 0.3333333333333333703, 0.3333333333333334259, 0.3333333333333333703, 0.3333333333333335369, 0.3333333333333333703, 0.3333333333333334259, 0.3333333333333334259, 0.3333333333333333703, 0.3333333333333334814, 0.3333333333333333703, 0.3333333333333334259, 0.3333333333333333703, 0.3333333333333334814, 0.3333333333333335369, 0.3333333333333334259, 0.3333333333333334259, 0.3333333333333333703, 0.3333333333333335369, 0.3333333333333333703, 0.3333333333333333703, 0.3333333333333335369, 0.3333333333333333703, 0.3333333333333335924, 0.3333333333333332593, 0.3333333333333335369, 0.3333333333333334259, 0.3333333333333333703, 0.3333333333333335369, 0.3333333333333333703, 0.3333333333333333703, 0.3333333333333334259, 0.3333333333333335369, 0.3333333333333333148, 0.3333333333333333703, 0.3333333333333335369, 0.3333333333333334259, 0.3333333333333333703, 0.3333333333333335369, 0.3333333333333333703, 0.3333333333333335924, 0.3333333333333333703, 0.3333333333333335369, 0.3333333333333334259, 0.3333333333333334814, 0.3333333333333334259, 0.3333333333333334259, 0.3333333333333334814, 0.3333333333333334259, 0.3333333333333334259, 0.3333333333333333148, 0.3333333333333333703, 0.3333333333333334814, 0.3333333333333334814, 0.3333333333333334259, 0.3333333333333333703, 0.3333333333333334259, 0.3333333333333333148, 0.3333333333333335369, 0.3333333333333333703, 0.3333333333333334814, 0.3333333333333335369, 0.3333333333333335369, 0.3333333333333335369, 0.3333333333333333703, 0.3333333333333334259, 0.3333333333333334259, 0.3333333333333333148, 0.3333333333333335369, 0.3333333333333334259, 0.3333333333333334259, 0.3333333333333334259, 0.3333333333333334814, 0.3333333333333334259, 0.3333333333333333148, 0.3333333333333334814, 0.3333333333333334259, 0.3333333333333333703, 0.3333333333333333703, 0.3333333333333334814, 0.3333333333333333703, 0.3333333333333334814, 0.3333333333333334814, 0.3333333333333333148, 0.3333333333333335924, 0.3333333333333333148, 0.3333333333333335369, 0.3333333333333333148, 0.3333333333333335924, 0.3333333333333333703, 0.3333333333333333148, 0.3333333333333334259, 0.3333333333333334259, 0.3333333333333334259, 0.3333333333333333703, 0.3333333333333334814, 0.3333333333333333703, 0.3333333333333334814, 0.3333333333333334814, 0.3333333333333333703, 0.3333333333333334259, 0.3333333333333334259, 0.3333333333333334814, 0.3333333333333333703, 0.3333333333333333703, 0.3333333333333334259, 0.3333333333333334259, 0.3333333333333333703, 0.3333333333333334259, 0.3333333333333333703, 0.3333333333333334259, 0.3333333333333334259, 0.3333333333333333703, 0.3333333333333335924, 0.3333333333333332593, 0.3333333333333335369, 0.3333333333333334259, 0.3333333333333333703, 0.3333333333333333148, 0.3333333333333335924, 0.3333333333333333148, 0.3333333333333333703, 0.3333333333333334259, 0.3333333333333334814, 0.3333333333333335369, 0.3333333333333333703, 0.3333333333333334259, 0.3333333333333333703, 0.3333333333333335369, 0.3333333333333333703, 0.3333333333333334259, 0.3333333333333334814, 0.3333333333333333703, 0.3333333333333335369, 0.3333333333333333148, 0.3333333333333335369, 0.3333333333333334259, 0.3333333333333334259, 0.3333333333333333703, 0.3333333333333335369, 0.3333333333333333703, 0.3333333333333335369, 0.3333333333333334814, 0.3333333333333333703, 0.3333333333333334814, 0.3333333333333333703, 0.3333333333333333703, 0.3333333333333335369, 0.3333333333333333703, 0.3333333333333334259, 0.3333333333333334814, 0.3333333333333333703, 0.3333333333333334259, 0.3333333333333333148, 0.3333333333333335369, 0.3333333333333334259, 0.3333333333333333703, 0.3333333333333334814, 0.3333333333333334259, 0.3333333333333334814, 0.3333333333333334259, 0.3333333333333333703, 0.3333333333333333703, 0.3333333333333334259, 0.3333333333333334259, 0.3333333333333334259, 0.3333333333333334259, 0.3333333333333333703, 0.3333333333333334814, 0.3333333333333334814, 0.3333333333333333703, 0.3333333333333335369, 0.3333333333333333703, 0.3333333333333334814, 0.3333333333333334814, 0.3333333333333335369, 0.3333333333333333148, 0.3333333333333335369, 0.3333333333333333703, 0.3333333333333333148, 0.3333333333333334814, 0.3333333333333333703, 0.3333333333333334814, 0.3333333333333333703, 0.3333333333333334814, 0.3333333333333333703, 0.3333333333333335369, 0.3333333333333333703, 0.3333333333333334814, 0.3333333333333334259, 0.3333333333333334814, 0.3333333333333334259, 0.3333333333333333703, 0.3333333333333333703, 0.3333333333333334814, 0.3333333333333334259, 0.3333333333333334814, 0.3333333333333334259, 0.3333333333333334259, 0.3333333333333334259, 0.3333333333333333703, 0.3333333333333334259, 0.3333333333333333703, 0.3333333333333334814, 0.3333333333333333148, 0.3333333333333335369, 0.3333333333333333703, 0.3333333333333334814, 0.3333333333333333703, 0.3333333333333335369, 0.3333333333333334259, 0.3333333333333334259, 0.3333333333333334259, 0.3333333333333334259, 0.3333333333333334259, 0.3333333333333334259),
 ( 0.3333333333333334259, 0.3333333333333334259, 0.3333333333333333703, 0.3333333333333334259, 0.3333333333333334814, 0.3333333333333333148, 0.3333333333333335924, 0.3333333333333333148, 0.3333333333333334259, 0.3333333333333333703, 0.3333333333333334814, 0.3333333333333334814, 0.3333333333333333148, 0.3333333333333334814, 0.3333333333333333703, 0.3333333333333334259, 0.3333333333333334259, 0.3333333333333333703, 0.3333333333333334814, 0.3333333333333334259, 0.3333333333333335369, 0.3333333333333333148, 0.3333333333333335369, 0.3333333333333333703, 0.3333333333333333703, 0.3333333333333334259, 0.3333333333333334814, 0.3333333333333334814, 0.3333333333333333148, 0.3333333333333335369, 0.3333333333333335924, 0.3333333333333334259, 0.3333333333333333703, 0.3333333333333335369, 0.3333333333333334259, 0.3333333333333334259, 0.3333333333333334814, 0.3333333333333335369, 0.3333333333333333703, 0.3333333333333334259, 0.3333333333333335369, 0.3333333333333333148, 0.3333333333333334259, 0.3333333333333335369, 0.3333333333333333703, 0.3333333333333334259, 0.3333333333333333703, 0.3333333333333335369, 0.3333333333333333703, 0.3333333333333334814, 0.3333333333333333703, 0.3333333333333334259, 0.3333333333333333703, 0.3333333333333333703, 0.3333333333333334259, 0.3333333333333333703, 0.3333333333333334259, 0.3333333333333333148, 0.3333333333333336479, 0.3333333333333334259, 0.3333333333333334814, 0.3333333333333333703, 0.3333333333333335369, 0.3333333333333334259, 0.3333333333333334259, 0.3333333333333334259, 0.3333333333333334259, 0.3333333333333333703, 0.3333333333333333703, 0.3333333333333335369, 0.3333333333333333703, 0.3333333333333335369, 0.3333333333333334259, 0.3333333333333333703, 0.3333333333333334814, 0.3333333333333334259, 0.3333333333333333703, 0.3333333333333333148, 0.3333333333333335369, 0.3333333333333333703, 0.3333333333333335369, 0.3333333333333333703, 0.3333333333333334814, 0.3333333333333333703, 0.3333333333333334259, 0.3333333333333333148, 0.3333333333333335369, 0.3333333333333333703, 0.3333333333333334814, 0.3333333333333333148, 0.3333333333333334814, 0.3333333333333334259, 0.3333333333333335369, 0.3333333333333334259, 0.3333333333333334814, 0.3333333333333334259, 0.3333333333333334259, 0.3333333333333334259, 0.3333333333333334259, 0.3333333333333333703, 0.3333333333333333703, 0.3333333333333334814, 0.3333333333333333703, 0.3333333333333333703, 0.3333333333333335369, 0.3333333333333332593, 0.3333333333333335369, 0.3333333333333332593, 0.3333333333333335924, 0.3333333333333334259, 0.3333333333333334814, 0.3333333333333333703, 0.3333333333333334814, 0.3333333333333334259, 0.3333333333333334259, 0.3333333333333334814, 0.3333333333333333703, 0.3333333333333333703, 0.3333333333333334814, 0.3333333333333333703, 0.3333333333333334814, 0.3333333333333333703, 0.3333333333333334259, 0.3333333333333334259, 0.3333333333333335369, 0.3333333333333333703, 0.3333333333333335369, 0.3333333333333334259, 0.3333333333333335369, 0.3333333333333334259, 0.3333333333333334259, 0.3333333333333334814, 0.3333333333333334814, 0.3333333333333333703, 0.3333333333333334814, 0.3333333333333333148, 0.3333333333333335369, 0.3333333333333333148, 0.3333333333333335369, 0.3333333333333334259, 0.3333333333333334259, 0.3333333333333334814, 0.3333333333333334814, 0.3333333333333333703, 0.3333333333333335369, 0.3333333333333333703, 0.3333333333333334259, 0.3333333333333334814, 0.3333333333333334814, 0.3333333333333334259, 0.3333333333333334259, 0.3333333333333335369, 0.3333333333333333148, 0.3333333333333335924, 0.3333333333333333703, 0.3333333333333333703, 0.3333333333333335369, 0.3333333333333333703, 0.3333333333333335924, 0.3333333333333333148, 0.3333333333333333703, 0.3333333333333334814, 0.3333333333333333703, 0.3333333333333335369, 0.3333333333333333703, 0.3333333333333334259, 0.3333333333333334814, 0.3333333333333333703, 0.3333333333333334259, 0.3333333333333334259, 0.3333333333333334259, 0.3333333333333334814, 0.3333333333333333703, 0.3333333333333334259, 0.3333333333333333703, 0.3333333333333335369, 0.3333333333333333703, 0.3333333333333334259, 0.3333333333333334259, 0.3333333333333333703, 0.3333333333333334814, 0.3333333333333333703, 0.3333333333333334259, 0.3333333333333333703, 0.3333333333333334814, 0.3333333333333335369, 0.3333333333333334259, 0.3333333333333334259, 0.3333333333333333703, 0.3333333333333335369, 0.3333333333333333703, 0.3333333333333333703, 0.3333333333333335369, 0.3333333333333333703, 0.3333333333333335924, 0.3333333333333332593, 0.3333333333333335369, 0.3333333333333334259, 0.3333333333333333703, 0.3333333333333335369, 0.3333333333333333703, 0.3333333333333333703, 0.3333333333333334259, 0.3333333333333335369, 0.3333333333333333148, 0.3333333333333333703, 0.3333333333333335369, 0.3333333333333334259, 0.3333333333333333703, 0.3333333333333335369, 0.3333333333333333703, 0.3333333333333335924, 0.3333333333333333703, 0.3333333333333335369, 0.3333333333333334259, 0.3333333333333334814, 0.3333333333333334259, 0.3333333333333334259, 0.3333333333333334814, 0.3333333333333334259, 0.3333333333333334259, 0.3333333333333333148, 0.3333333333333333703, 0.3333333333333334814, 0.3333333333333334814, 0.3333333333333334259, 0.3333333333333333703, 0.3333333333333334259, 0.3333333333333333148, 0.3333333333333335369, 0.3333333333333333703, 0.3333333333333334814, 0.3333333333333335369, 0.3333333333333335369, 0.3333333333333335369, 0.3333333333333333703, 0.3333333333333334259, 0.3333333333333334259, 0.3333333333333333148, 0.3333333333333335369, 0.3333333333333334259, 0.3333333333333334259, 0.3333333333333334259, 0.3333333333333334814, 0.3333333333333334259, 0.3333333333333333148, 0.3333333333333334814, 0.3333333333333334259, 0.3333333333333333703, 0.3333333333333333703, 0.3333333333333334814, 0.3333333333333333703, 0.3333333333333334814, 0.3333333333333334814, 0.3333333333333333148, 0.3333333333333335924, 0.3333333333333333148, 0.3333333333333335369, 0.3333333333333333148, 0.3333333333333335924, 0.3333333333333333703, 0.3333333333333333148, 0.3333333333333334259, 0.3333333333333334259, 0.3333333333333334259, 0.3333333333333333703, 0.3333333333333334814, 0.3333333333333333703, 0.3333333333333334814, 0.3333333333333334814, 0.3333333333333333703, 0.3333333333333334259, 0.3333333333333334259, 0.3333333333333334814, 0.3333333333333333703, 0.3333333333333333703, 0.3333333333333334259, 0.3333333333333334259, 0.3333333333333333703, 0.3333333333333334259, 0.3333333333333333703, 0.3333333333333334259, 0.3333333333333334259, 0.3333333333333333703, 0.3333333333333335924, 0.3333333333333332593, 0.3333333333333335369, 0.3333333333333334259, 0.3333333333333333703, 0.3333333333333333148, 0.3333333333333335924, 0.3333333333333333148, 0.3333333333333333703, 0.3333333333333334259, 0.3333333333333334814, 0.3333333333333335369, 0.3333333333333333703, 0.3333333333333334259, 0.3333333333333333703, 0.3333333333333335369, 0.3333333333333333703, 0.3333333333333334259, 0.3333333333333334814, 0.3333333333333333703, 0.3333333333333335369, 0.3333333333333333148, 0.3333333333333335369, 0.3333333333333334259, 0.3333333333333334259, 0.3333333333333333703, 0.3333333333333335369, 0.3333333333333333703, 0.3333333333333335369, 0.3333333333333334814, 0.3333333333333333703, 0.3333333333333334814, 0.3333333333333333703, 0.3333333333333333703, 0.3333333333333335369, 0.3333333333333333703, 0.3333333333333334259, 0.3333333333333334814, 0.3333333333333333703, 0.3333333333333334259, 0.3333333333333333148, 0.3333333333333335369, 0.3333333333333334259, 0.3333333333333333703, 0.3333333333333334814, 0.3333333333333334259, 0.3333333333333334814, 0.3333333333333334259, 0.3333333333333333703, 0.3333333333333333703, 0.3333333333333334259, 0.3333333333333334259, 0.3333333333333334259, 0.3333333333333334259, 0.3333333333333333703, 0.3333333333333334814, 0.3333333333333334814, 0.3333333333333333703, 0.3333333333333335369, 0.3333333333333333703, 0.3333333333333334814, 0.3333333333333334814, 0.3333333333333335369, 0.3333333333333333148, 0.3333333333333335369, 0.3333333333333333703, 0.3333333333333333148, 0.3333333333333334814, 0.3333333333333333703, 0.3333333333333334814, 0.3333333333333333703, 0.3333333333333334814, 0.3333333333333333703, 0.3333333333333335369, 0.3333333333333333703, 0.3333333333333334814, 0.3333333333333334259, 0.3333333333333334814, 0.3333333333333334259, 0.3333333333333333703, 0.3333333333333333703, 0.3333333333333334814, 0.3333333333333334259, 0.3333333333333334814, 0.3333333333333334259, 0.3333333333333334259, 0.3333333333333334259, 0.3333333333333333703, 0.3333333333333334259, 0.3333333333333333703, 0.3333333333333334814, 0.3333333333333333148, 0.3333333333333335369, 0.3333333333333333703, 0.3333333333333334814, 0.3333333333333333703, 0.3333333333333335369, 0.3333333333333334259, 0.3333333333333334259, 0.3333333333333334259, 0.3333333333333334259, 0.3333333333333334259, 0.3333333333333334259),
 ( 1.000000000000000222, 1.000000000000000222, 1.000000000000000222, 1.000000000000000222, 1.000000000000000444, 1.000000000000000000, 1.000000000000000666, 0.9999999999999997780, 1.000000000000000444, 1.000000000000000000, 1.000000000000000444, 1.000000000000000444, 1.000000000000000000, 1.000000000000000444, 1.000000000000000000, 1.000000000000000444, 1.000000000000000222, 1.000000000000000222, 1.000000000000000222, 1.000000000000000444, 1.000000000000000444, 1.000000000000000000, 1.000000000000000444, 1.000000000000000000, 1.000000000000000222, 1.000000000000000222, 1.000000000000000444, 1.000000000000000222, 1.000000000000000222, 1.000000000000000444, 1.000000000000000444, 1.000000000000000444, 1.000000000000000000, 1.000000000000000444, 1.000000000000000444, 1.000000000000000000, 1.000000000000000444, 1.000000000000000444, 1.000000000000000000, 1.000000000000000444, 1.000000000000000444, 1.000000000000000000, 1.000000000000000222, 1.000000000000000444, 1.000000000000000222, 1.000000000000000222, 1.000000000000000000, 1.000000000000000444, 1.000000000000000222, 1.000000000000000222, 1.000000000000000222, 1.000000000000000222, 1.000000000000000222, 1.000000000000000222, 1.000000000000000444, 1.000000000000000000, 1.000000000000000444, 0.9999999999999997780, 1.000000000000000666, 1.000000000000000444, 1.000000000000000444, 1.000000000000000000, 1.000000000000000444, 1.000000000000000222, 1.000000000000000222, 1.000000000000000444, 1.000000000000000222, 1.000000000000000444, 1.000000000000000000, 1.000000000000000444, 1.000000000000000222, 1.000000000000000444, 1.000000000000000444, 1.000000000000000222, 1.000000000000000222, 1.000000000000000222, 1.000000000000000444, 0.9999999999999997780, 1.000000000000000444, 1.000000000000000000, 1.000000000000000444, 1.000000000000000000, 1.000000000000000444, 0.9999999999999997780, 1.000000000000000444, 0.9999999999999997780, 1.000000000000000444, 1.000000000000000222, 1.000000000000000444, 1.000000000000000000, 1.000000000000000222, 1.000000000000000444, 1.000000000000000444, 1.000000000000000222, 1.000000000000000444, 1.000000000000000444, 1.000000000000000222, 1.000000000000000222, 1.000000000000000222, 1.000000000000000222, 1.000000000000000000, 1.000000000000000222, 1.000000000000000222, 1.000000000000000222, 1.000000000000000444, 1.000000000000000000, 1.000000000000000444, 0.9999999999999997780, 1.000000000000000666, 1.000000000000000222, 1.000000000000000444, 1.000000000000000000, 1.000000000000000444, 1.000000000000000222, 1.000000000000000222, 1.000000000000000444, 1.000000000000000000, 1.000000000000000000, 1.000000000000000444, 1.000000000000000000, 1.000000000000000444, 1.000000000000000000, 1.000000000000000444, 1.000000000000000222, 1.000000000000000444, 1.000000000000000222, 1.000000000000000444, 1.000000000000000222, 1.000000000000000444, 1.000000000000000000, 1.000000000000000444, 1.000000000000000222, 1.000000000000000444, 1.000000000000000000, 1.000000000000000444, 1.000000000000000000, 1.000000000000000444, 1.000000000000000000, 1.000000000000000444, 1.000000000000000222, 1.000000000000000444, 1.000000000000000222, 1.000000000000000444, 0.9999999999999997780, 1.000000000000000444, 1.000000000000000000, 1.000000000000000444, 1.000000000000000222, 1.000000000000000222, 1.000000000000000222, 1.000000000000000222, 1.000000000000000444, 0.9999999999999997780, 1.000000000000000444, 1.000000000000000000, 1.000000000000000000, 1.000000000000000222, 1.000000000000000222, 1.000000000000000666, 0.9999999999999997780, 1.000000000000000000, 1.000000000000000444, 1.000000000000000222, 1.000000000000000444, 1.000000000000000000, 1.000000000000000222, 1.000000000000000444, 1.000000000000000222, 1.000000000000000000, 1.000000000000000444, 1.000000000000000222, 1.000000000000000222, 1.000000000000000444, 1.000000000000000222, 1.000000000000000000, 1.000000000000000444, 1.000000000000000000, 1.000000000000000444, 1.000000000000000222, 1.000000000000000222, 1.000000000000000444, 0.9999999999999997780, 1.000000000000000444, 0.9999999999999997780, 1.000000000000000444, 1.000000000000000222, 1.000000000000000444, 1.000000000000000222, 1.000000000000000222, 1.000000000000000444, 1.000000000000000000, 1.000000000000000222, 1.000000000000000444, 1.000000000000000000, 1.000000000000000444, 1.000000000000000000, 1.000000000000000222, 1.000000000000000444, 1.000000000000000000, 1.000000000000000444, 0.9999999999999997780, 1.000000000000000444, 1.000000000000000222, 1.000000000000000444, 1.000000000000000000, 1.000000000000000000, 1.000000000000000444, 1.000000000000000000, 1.000000000000000222, 1.000000000000000444, 1.000000000000000222, 1.000000000000000444, 1.000000000000000222, 1.000000000000000444, 1.000000000000000444, 1.000000000000000444, 1.000000000000000000, 1.000000000000000444, 1.000000000000000222, 1.000000000000000444, 1.000000000000000222, 1.000000000000000000, 1.000000000000000222, 1.000000000000000444, 1.000000000000000222, 1.000000000000000444, 1.000000000000000000, 1.000000000000000222, 1.000000000000000000, 1.000000000000000444, 1.000000000000000000, 1.000000000000000444, 1.000000000000000444, 1.000000000000000444, 1.000000000000000444, 1.000000000000000000, 1.000000000000000222, 1.000000000000000444, 1.000000000000000000, 1.000000000000000444, 1.000000000000000444, 1.000000000000000444, 1.000000000000000222, 1.000000000000000222, 1.000000000000000222, 0.9999999999999997780, 1.000000000000000444, 1.000000000000000222, 1.000000000000000222, 1.000000000000000000, 1.000000000000000444, 1.000000000000000000, 1.000000000000000444, 1.000000000000000000, 1.000000000000000000, 1.000000000000000666, 1.000000000000000000, 1.000000000000000444, 1.000000000000000000, 1.000000000000000444, 1.000000000000000222, 0.9999999999999997780, 1.000000000000000444, 1.000000000000000000, 1.000000000000000444, 1.000000000000000222, 1.000000000000000444, 1.000000000000000222, 1.000000000000000222, 1.000000000000000444, 1.000000000000000000, 1.000000000000000222, 1.000000000000000444, 1.000000000000000222, 1.000000000000000000, 1.000000000000000444, 0.9999999999999997780, 1.000000000000000444, 1.000000000000000222, 1.000000000000000222, 1.000000000000000222, 1.000000000000000000, 1.000000000000000444, 1.000000000000000222, 1.000000000000000666, 0.9999999999999997780, 1.000000000000000444, 1.000000000000000222, 1.000000000000000000, 1.000000000000000222, 1.000000000000000444, 1.000000000000000222, 1.000000000000000000, 1.000000000000000444, 1.000000000000000222, 1.000000000000000444, 1.000000000000000000, 1.000000000000000444, 1.000000000000000222, 1.000000000000000444, 1.000000000000000222, 1.000000000000000222, 1.000000000000000444, 1.000000000000000222, 1.000000000000000444, 1.000000000000000000, 1.000000000000000444, 1.000000000000000222, 1.000000000000000222, 1.000000000000000000, 1.000000000000000666, 0.9999999999999997780, 1.000000000000000444, 1.000000000000000222, 1.000000000000000444, 1.000000000000000222, 1.000000000000000444, 1.000000000000000000, 1.000000000000000444, 1.000000000000000222, 1.000000000000000222, 1.000000000000000444, 1.000000000000000222, 1.000000000000000444, 1.000000000000000000, 1.000000000000000444, 1.000000000000000444, 0.9999999999999997780, 1.000000000000000444, 1.000000000000000000, 1.000000000000000444, 1.000000000000000444, 1.000000000000000222, 1.000000000000000000, 1.000000000000000444, 1.000000000000000222, 1.000000000000000444, 1.000000000000000000, 1.000000000000000444, 1.000000000000000222, 1.000000000000000444, 1.000000000000000222, 1.000000000000000444, 1.000000000000000222, 1.000000000000000222, 1.000000000000000444, 1.000000000000000444, 1.000000000000000000, 1.000000000000000444, 0.9999999999999997780, 1.000000000000000444, 1.000000000000000222, 1.000000000000000222, 1.000000000000000222, 1.000000000000000444, 1.000000000000000222, 1.000000000000000222, 1.000000000000000444, 1.000000000000000000, 1.000000000000000444, 1.000000000000000000, 1.000000000000000444, 1.000000000000000222, 1.000000000000000000, 1.000000000000000222, 1.000000000000000444, 1.000000000000000000, 1.000000000000000444, 1.000000000000000000, 1.000000000000000444, 1.000000000000000444, 1.000000000000000000, 1.000000000000000444, 1.000000000000000000, 1.000000000000000444, 1.000000000000000000, 1.000000000000000444, 1.000000000000000000, 1.000000000000000444, 1.000000000000000000, 1.000000000000000444, 1.000000000000000000, 1.000000000000000444, 1.000000000000000222, 1.000000000000000222, 1.000000000000000222, 1.000000000000000222) ) ) 
 REPRESENTATION_ITEM ( '' )  SURFACE ( )  );
#176950 = CARTESIAN_POINT ( 'NONE',  ( 3.796581652666820350, 1.495729193744433028, -1.498731062137735437 ) ) ;
#176951 = CARTESIAN_POINT ( 'NONE',  ( 5.542585869888291938, 5.360771691158120689, -0.7998128361456211532 ) ) ;
#176952 = CARTESIAN_POINT ( 'NONE',  ( 6.753933077901968396, 11.03133902419432566, 0.7998128361456462443 ) ) ;
#176953 = CARTESIAN_POINT ( 'NONE',  ( 0.3819399096430804441, 6.573892064833275484, 3.228863705805710804 ) ) ;
#176954 = CARTESIAN_POINT ( 'NONE',  ( 0.5495732465782035003, 1.455460699200894270, 1.326940832280040450 ) ) ;
#176955 = CARTESIAN_POINT ( 'NONE',  ( 5.008269389056229315, 6.794162766424465261, 1.424127363233711252 ) ) ;
#176956 = CARTESIAN_POINT ( 'NONE',  ( 4.202664430556247055, 6.886563688082179446, 1.082531754730558626 ) ) ;
#176958 = CARTESIAN_POINT ( 'NONE',  ( 4.991989969715248776, 4.726297878971393196, -2.420000000000000373 ) ) ;
#176957 = CARTESIAN_POINT ( 'NONE',  ( -3.475000000000000533, -1.399999999999998579, 0.000000000000000000 ) ) ;
#176959 = CARTESIAN_POINT ( 'NONE',  ( 3.205313226950608385, -0.4470181708258395004, 2.248096707283386841 ) ) ;
#176960 = CARTESIAN_POINT ( 'NONE',  ( 0.8733498553583609603, 1.760202786292342170, -0.4843115980177821744 ) ) ;
#176961 = CARTESIAN_POINT ( 'NONE',  ( 3.463059065379545221, -1.560675823418774533, 1.104941681961457256 ) ) ;
#176962 = CARTESIAN_POINT ( 'NONE',  ( 5.234329823327693809, 8.264412672927770487, 1.199719254218451159 ) ) ;
#176963 = CARTESIAN_POINT ( 'NONE',  ( 6.277061933002777927, 8.346324893301817482, 1.443375672974076540 ) ) ;
#176964 = CARTESIAN_POINT ( 'NONE',  ( -9.643927338022246332, 10.14567007064778004, -0.7998128361456291469 ) ) ;
#176965 = CARTESIAN_POINT ( 'NONE',  ( 2.056891478215248981, 0.4451058530966587323, 1.963224067645082949 ) ) ;
#176966 = CARTESIAN_POINT ( 'NONE',  ( 2.606241817087478374, 1.961221450604538008, 0.05310280016677935283 ) ) ;
#176967 = CARTESIAN_POINT ( 'NONE',  ( -9.969323024750229578, 10.52529837183042716, -0.7998128361456291469 ) ) ;
#176968 = CARTESIAN_POINT ( 'NONE',  ( -6.191269702934848240, 10.37489842006599616, 0.000000000000000000 ) ) ;
#176969 = CARTESIAN_POINT ( 'NONE',  ( -11.43204722947019825, 9.944072459738260150, -3.649275849833183649 ) ) ;
#176971 = CARTESIAN_POINT ( 'NONE',  ( 3.115802406598367824, -0.8709184464271730874, -1.540630773470308190 ) ) ;
#176970 = CARTESIAN_POINT ( 'NONE',  ( 5.578101482107681974, -2.039469400243614672, -0.4589526871568836430 ) ) ;
#176972 = CARTESIAN_POINT ( 'NONE',  ( 1.000000047849762153, 14.00000000000000533, 11.64874984998672325 ) ) ;
#176974 = CARTESIAN_POINT ( 'NONE',  ( 6.070342170859510667, -2.174803699615239783, -0.7246130948556377405 ) ) ;
#176973 = LINE ( 'NONE', #212647, #148908 ) ;
#176975 = CARTESIAN_POINT ( 'NONE',  ( 3.907932343763017347, 1.228949333998660798, -1.232512660115521408 ) ) ;
#176976 = CARTESIAN_POINT ( 'NONE',  ( 8.378048858240820351, 11.86180853700128601, -1.199719254218446718 ) ) ;
#176977 = CARTESIAN_POINT ( 'NONE',  ( -1.416786528094066355, 7.999640415717691688, 11.00953083556809275 ) ) ;
#176978 = CARTESIAN_POINT ( 'NONE',  ( 3.883936887208380373, -0.1284340723075507729, 1.729154583330833272 ) ) ;
#176979 = CARTESIAN_POINT ( 'NONE',  ( 4.703694880604158968, -1.675542544088706620, -1.380765677988102791 ) ) ;
#176980 = CARTESIAN_POINT ( 'NONE',  ( 4.383363735919856730, 4.008345868194933104, -0.7998128361456211532 ) ) ;
#176981 = CARTESIAN_POINT ( 'NONE',  ( 6.298064597363540074, -0.9548514761729166578, -1.776169100128288658 ) ) ;
#176982 = CARTESIAN_POINT ( 'NONE',  ( 5.593750000000004441, -1.895863743164200921, -0.7852924748296893354 ) ) ;
#176983 = DIRECTION ( 'NONE',  ( -0.000000000000000000, -8.546850786086437571E-32, -1.000000000000000000 ) ) ;
#176984 = CARTESIAN_POINT ( 'NONE',  ( 2.907156789938716290, 1.626457378340099069, 1.032021673995666911 ) ) ;
#176985 = CARTESIAN_POINT ( 'NONE',  ( -1.500000000000015099, 10.26041666734946034, -0.8660254037844309360 ) ) ;
#176986 = CARTESIAN_POINT ( 'NONE',  ( 0.2588218971089132348, 2.215798623493638875, 0.1571155685827912152 ) ) ;
#176987 = ORIENTED_EDGE ( 'NONE', *, *, #172459, .T. ) ;
#176988 = CARTESIAN_POINT ( 'NONE',  ( -0.1409997244346088141, 1.357410162930408504, -2.254437325861287533 ) ) ;
#176989 = CARTESIAN_POINT ( 'NONE',  ( -1.499999999999997780, 3.150000000000020783, 1.214306433183764966E-14 ) ) ;
#176990 = CARTESIAN_POINT ( 'NONE',  ( 4.788000803920411386, 8.737751371215816576, 1.040834085586084257E-14 ) ) ;
#176991 = CARTESIAN_POINT ( 'NONE',  ( 2.491161192834326688, -2.126536535197431022, -0.6419364700022185399 ) ) ;
#176992 = CARTESIAN_POINT ( 'NONE',  ( -2.550000000000000266, 1.000000000000000888, -1.849324200890692271 ) ) ;
#176993 = CARTESIAN_POINT ( 'NONE',  ( 7.944714827928056167, 8.371181508778631652, 0.7216878364870458196 ) ) ;
#176994 = CARTESIAN_POINT ( 'NONE',  ( 0.4897149945007785443, 7.513091487862237017, 2.015070445391641041 ) ) ;
#176995 = AXIS2_PLACEMENT_3D ( 'NONE', #16189, #98541, #26330 ) ;
#176996 = CARTESIAN_POINT ( 'NONE',  ( 5.076602173674213070, 4.887400388900169368, 0.000000000000000000 ) ) ;
#176997 = CARTESIAN_POINT ( 'NONE',  ( 0.8619541869999207684, -0.05229984143813663777, -2.015912905633105101 ) ) ;
#176999 = CARTESIAN_POINT ( 'NONE',  ( 5.881316448893678661, -0.05433346072863074611, 2.062130925675903725 ) ) ;
#176998 = CARTESIAN_POINT ( 'NONE',  ( 9.565441069641300587, 11.11843498845840905, -1.199719254218440723 ) ) ;
#177000 = DIRECTION ( 'NONE',  ( 5.578564026256490882E-16, 1.000000000000000000, 9.066213480720158442E-32 ) ) ;
#177001 = CARTESIAN_POINT ( 'NONE',  ( -3.846762897975357198, 5.510976019103107859, -1.599625672291256295 ) ) ;
#177002 = CARTESIAN_POINT ( 'NONE',  ( -0.7500000000000215383, 5.472916667349482900, 1.299038105676671107 ) ) ;
#177003 = CARTESIAN_POINT ( 'NONE',  ( -1.364683531250000748, 0.7593750003414210248, 0.000000000000000000 ) ) ;
#177004 = CARTESIAN_POINT ( 'NONE',  ( 0.2273421782777407807, -1.081390543313685226, -1.401283913643845969 ) ) ;
#177005 = CARTESIAN_POINT ( 'NONE',  ( 5.590364566445758854, -0.4131642248683431440, 1.684076740667529881 ) ) ;
#177006 = CARTESIAN_POINT ( 'NONE',  ( 5.917484386527373630, -0.9743193633129590969, -1.441955756940280997 ) ) ;
#177007 = CARTESIAN_POINT ( 'NONE',  ( 3.474455725741688372, -2.209678783342132746, -0.6099929035564675139 ) ) ;
#177008 = CARTESIAN_POINT ( 'NONE',  ( -1.364683531250014514, -1.011458332991911568, -0.7879004041258359514 ) ) ;
#177009 = CARTESIAN_POINT ( 'NONE',  ( 2.325889007780062023, 1.785771638016835361, 0.4476198290149570602 ) ) ;
#177010 = EDGE_CURVE ( 'NONE', #150994, #213399, #41547, .T. ) ;
#177011 = CARTESIAN_POINT ( 'NONE',  ( 7.913155211870404493, 12.38376484715752213, 0.7998128361456462443 ) ) ;
#177012 = CARTESIAN_POINT ( 'NONE',  ( -12.00071372354016752, 8.501427447926152681, -1.132741196307404330 ) ) ;
#177013 = CARTESIAN_POINT ( 'NONE',  ( 2.168725436055967570, -1.667931858681595880, -0.7425449061374129744 ) ) ;
#177014 = CARTESIAN_POINT ( 'NONE',  ( 2.373672848961404735, -0.3474683332905931232, -1.986100487175908258 ) ) ;
#177015 = CARTESIAN_POINT ( 'NONE',  ( -4.419594887930571758, 4.258541578781506409, 1.214306433183764966E-14 ) ) ;
#177016 = CARTESIAN_POINT ( 'NONE',  ( 6.743451144134843922, 15.00000000000000000, -9.536680065235831449 ) ) ;
#177017 = CARTESIAN_POINT ( 'NONE',  ( 4.172956468465331525, -1.964154803760146617, -0.7601757144085323770 ) ) ;
#177018 = CARTESIAN_POINT ( 'NONE',  ( -7.009729113465285266, 8.136771039586342624, -1.199719254218446718 ) ) ;
#177019 = CARTESIAN_POINT ( 'NONE',  ( 7.457859969268502809, 13.90606279126528300, 8.983713841573639058 ) ) ;
#177020 = CARTESIAN_POINT ( 'NONE',  ( 2.928250347896840022, 1.105370970781336837, 1.750397071514836478 ) ) ;
#177021 = CARTESIAN_POINT ( 'NONE',  ( 4.867540842506059562, 5.637551390133895168, -1.199719254218452047 ) ) ;
#177022 = CARTESIAN_POINT ( 'NONE',  ( -1.360316468750028651, -0.8281249996586054207, -3.469446951953614189E-14 ) ) ;
#177023 = CARTESIAN_POINT ( 'NONE',  ( 4.793665170694914046, 1.978287127071875151, -0.7638792978137476375 ) ) ;
#177024 = CARTESIAN_POINT ( 'NONE',  ( 6.340460056601358474, 1.806591233369018834, 0.2625940548972791611 ) ) ;
#177025 = VERTEX_POINT ( 'NONE', #147635 ) ;
#177026 = CARTESIAN_POINT ( 'NONE',  ( -3.955946960137363799, 7.837298230127379917, 0.7998128361456352531 ) ) ;
#177027 = CARTESIAN_POINT ( 'NONE',  ( 8.374132434735052755, 12.92157160716627295, -0.7998128361456352531 ) ) ;
#177028 = CARTESIAN_POINT ( 'NONE',  ( 4.841670253411575864, 8.662716039039905169, -0.7216878364870458196 ) ) ;
#177029 = CARTESIAN_POINT ( 'NONE',  ( 1.737500000000001155, -1.589583332377419334, 3.009438278150922130 ) ) ;
#177030 = CARTESIAN_POINT ( 'NONE',  ( -4.218558352146454915, 8.073401844146177453, 1.040834085586084257E-14 ) ) ;
#177031 = CARTESIAN_POINT ( 'NONE',  ( 6.469000917296717112, -1.638331675554663747, 1.346054232038436105 ) ) ;
#177032 = CARTESIAN_POINT ( 'NONE',  ( 1.378104160372157994, 1.254256560567709622, 1.691567388252762649 ) ) ;
#177033 = CARTESIAN_POINT ( 'NONE',  ( -5.815521545619021460, 5.749472989502435460, -0.7998128361456362523 ) ) ;
#177034 = CARTESIAN_POINT ( 'NONE',  ( 9.402743226277308963, 10.92862083786708816, -1.199719254218446718 ) ) ;
#177035 = CARTESIAN_POINT ( 'NONE',  ( 5.190230013454653069, 0.9586131782086585451, -1.594917819662385883 ) ) ;
#177036 = CARTESIAN_POINT ( 'NONE',  ( 7.889955328148847258, 11.29236608522730911, -1.199719254218446718 ) ) ;
#177037 = ADVANCED_FACE ( 'NONE', ( #19739 ), #198480, .F. ) ;
#177038 = CARTESIAN_POINT ( 'NONE',  ( -10.49167095263961613, 5.343775707538777731, -5.730694126968513658 ) ) ;
#177039 = CARTESIAN_POINT ( 'NONE',  ( -2.810282979782591006, 6.500690253046801814, 0.000000000000000000 ) ) ;
#177040 = CARTESIAN_POINT ( 'NONE',  ( -9.653042183249970876, 11.32459930428888306, -1.082531754730539753 ) ) ;
#177041 =( BOUNDED_SURFACE ( )  B_SPLINE_SURFACE ( 1, 2, ( 
 ( #45465, #145121, #176518, #206868, #208988, #92092, #44397, #142988, #174407, #191675, #43337, #175463, #27048, #159194, #60624, #74753, #126786, #58499, #210059, #160264, #144064, #124655, #110518, #190611, #140855, #77943, #61698, #127867, #193817, #42270, #111582, #177592, #29204, #41205, #211127, #62751, #173336, #150156, #85134, #84067, #69922, #19055, #20119, #136033, #178660, #167460, #184749, #166387, #46530, #179726, #31345, #51584, #100321, #113722, #17979, #151221, #153340, #112651, #1725, #13989, #30272, #37449, #96357, #202046, #117709, #195975, #133932, #3849, #67782, #129987, #199937, #101385, #183700, #4912, #194892, #146176, #35308, #86204, #47608, #2789, #103527, #70989, #68861, #134980, #200990, #52636, #162412, #80073, #169586, #118764, #36377, #212191, #63829, #53706, #102454, #168520, #152276, #119839, #185818, #21169, #87272, #121993, #125191, #156553, #92638, #8148, #138171, #137102, #120920, #205265, #10277, #191154, #42821, #186893, #190095, #39587, #172805, #187959, #204181, #7058, #203131, #124134, #107861, #105689, #104602, #189036, #91570, #171717, #55837, #88347, #157622, #41749, #108927, #23316, #54773, #38525, #56906, #170649, #174948, #26530, #22236, #173887, #89424, #24377, #155475, #73131, #139234, #154411, #25462, #9219, #123079, #5990, #40674, #75291, #106777, #90490, #72061, #141406, #207414, #158679, #74232, #140325, #206343, #57970, #59033, #44948, #143537, #127334, #111056, #193303, #60103, #28679, #27600, #30827, #211670, #179203, #93700, #177063, #11339, #192219, #13479, #46013, #94766, #63306, #77420, #160814, #209531, #159741, #76352, #12405, #113197, #61173, #78485, #178136, #144602, #162955, #112133, #96904, #14533, #210617, #79555, #129467, #62244, #142459, #128403, #194370, #43882, #114267, #164022, #31887, #97964, #29751, #130521, #80630, #95836, #146722, #161892, #145673, #195451, #47079, #208467, #212740, #64375, #196511, #109996, #48154, #180263, #126262, #176008, #165070, #116377, #167208, #18796, #148820, #201804, #133675, #68608, #84881, #150968, #2532, #16662 ),
 ( #99013, #49201, #66464, #32940, #82747, #199680, #53446, #393, #3598, #35049, #185568, #101120, #132605, #81683, #182365, #115322, #147769, #69675, #131556, #102203, #83807, #198611, #166131, #36119, #33995, #50258, #100069, #51323, #17718, #37198, #15597, #181312, #149899, #52388, #1467, #67533, #135781, #103272, #117451, #183445, #134731, #200738, #197557, #118516, #119585, #184500, #168269, #19869, #85954, #152029, #213785, #65408, #5728, #186643, #104346, #72886, #207164, #154162, #157372, #188784, #124943, #40420, #170390, #169335, #153086, #23058, #42569, #8967, #75040, #4662, #7885, #71807, #205014, #137918, #21979, #39336, #20919, #156302, #140068, #203938, #136848, #6808, #123883, #55586, #88089, #120665, #189848, #73973, #141156, #121741, #172549, #138993, #187708, #105433, #171469, #89175, #155227, #56660, #122823, #70734, #106523, #38269, #41494, #90236, #57725, #24134, #206091, #107607, #202872, #173638, #25211, #91315, #58787, #190905, #87014, #54520, #59852, #108672, #127080, #145425, #126004, #60923, #210359, #209276, #195197, #144358, #96655, #95593, #46834, #109746, #161641, #77164, #174700, #93450, #159488, #176809, #11087, #27348, #143285, #78236, #64131, #146470, #193043, #162708, #128155, #130275, #194115, #175756, #26275, #92391, #28425, #196263, #14280, #80375, #158427, #13236, #44697, #61999, #110804, #94518, #160556, #10027, #79309, #211426, #12164, #76102, #45765, #63056, #111883, #177887, #191965, #129223, #112948, #212489, #29500, #178959, #30574, #142205, #208220, #43631, #115072, #98766, #82493, #164822, #31637, #149, #213542, #2282, #183196, #150722, #65165, #16413, #197313, #163772, #199431, #17475, #148580, #34802, #48954, #66215, #181068, #131320, #47910, #132363, #84631, #32686, #198365, #149641, #50005, #134491, #83559, #35877, #100877, #200494, #116129, #166964, #182117, #114020, #33746, #99824, #165890, #1223, #67285, #133424, #51073, #3355, #180016, #117198, #81443, #97714, #101952, #15350, #52138, #18554, #68358, #118266, #184250, #168019, #19623, #85694, #151782 ) ),
 .UNSPECIFIED., .F., .F., .F. ) 
 B_SPLINE_SURFACE_WITH_KNOTS ( ( 2, 2 ),
 ( 3, 2, 2, 2, 2, 2, 2, 2, 2, 2, 2, 2, 2, 2, 2, 2, 2, 2, 2, 2, 2, 2, 2, 2, 2, 2, 2, 2, 2, 2, 2, 2, 2, 2, 2, 2, 2, 2, 2, 2, 2, 2, 2, 2, 2, 2, 2, 2, 2, 2, 2, 2, 2, 2, 2, 2, 2, 2, 2, 2, 2, 2, 2, 2, 2, 2, 2, 2, 2, 2, 2, 2, 2, 2, 2, 2, 2, 2, 2, 2, 2, 2, 2, 2, 2, 2, 2, 2, 2, 2, 2, 2, 2, 2, 2, 2, 2, 2, 2, 2, 2, 2, 2, 2, 2, 2, 2, 2, 2, 2, 2, 2, 2, 2, 2, 2, 2, 2, 2, 2, 3 ),
 ( 0.000000000000000000, 1.000000000000000000 ),
 ( 0.000000000000000000, 0.008333333333333333218, 0.01666666666666666644, 0.02500000000000000139, 0.03333333333333333287, 0.04166666666666666435, 0.05000000000000000278, 0.05833333333333333426, 0.06666666666666666574, 0.07499999999999999722, 0.08333333333333332871, 0.09166666666666666019, 0.1000000000000000056, 0.1083333333333333370, 0.1166666666666666685, 0.1250000000000000000, 0.1333333333333333315, 0.1416666666666666630, 0.1499999999999999944, 0.1583333333333333259, 0.1666666666666666574, 0.1749999999999999889, 0.1833333333333333204, 0.1916666666666666796, 0.2000000000000000111, 0.2083333333333333426, 0.2166666666666666741, 0.2250000000000000056, 0.2333333333333333370, 0.2416666666666666685, 0.2500000000000000000, 0.2583333333333333592, 0.2666666666666666630, 0.2750000000000000222, 0.2833333333333333259, 0.2916666666666666852, 0.2999999999999999889, 0.3083333333333333481, 0.3166666666666666519, 0.3250000000000000111, 0.3333333333333333148, 0.3416666666666666741, 0.3499999999999999778, 0.3583333333333333370, 0.3666666666666666408, 0.3750000000000000000, 0.3833333333333333592, 0.3916666666666666630, 0.4000000000000000222, 0.4083333333333333259, 0.4166666666666666852, 0.4249999999999999889, 0.4333333333333333481, 0.4416666666666666519, 0.4500000000000000111, 0.4583333333333333148, 0.4666666666666666741, 0.4749999999999999778, 0.4833333333333333370, 0.4916666666666666408, 0.5000000000000000000, 0.5083333333333333037, 0.5166666666666667185, 0.5250000000000000222, 0.5333333333333333259, 0.5416666666666666297, 0.5500000000000000444, 0.5583333333333333481, 0.5666666666666666519, 0.5749999999999999556, 0.5833333333333333703, 0.5916666666666666741, 0.5999999999999999778, 0.6083333333333332815, 0.6166666666666666963, 0.6250000000000000000, 0.6333333333333333037, 0.6416666666666667185, 0.6500000000000000222, 0.6583333333333333259, 0.6666666666666666297, 0.6750000000000000444, 0.6833333333333333481, 0.6916666666666666519, 0.6999999999999999556, 0.7083333333333333703, 0.7166666666666666741, 0.7249999999999999778, 0.7333333333333332815, 0.7416666666666666963, 0.7500000000000000000, 0.7583333333333333037, 0.7666666666666667185, 0.7750000000000000222, 0.7833333333333333259, 0.7916666666666666297, 0.8000000000000000444, 0.8083333333333333481, 0.8166666666666666519, 0.8249999999999999556, 0.8333333333333333703, 0.8416666666666666741, 0.8499999999999999778, 0.8583333333333332815, 0.8666666666666666963, 0.8750000000000000000, 0.8833333333333333037, 0.8916666666666667185, 0.9000000000000000222, 0.9083333333333333259, 0.9166666666666666297, 0.9250000000000000444, 0.9333333333333333481, 0.9416666666666666519, 0.9499999999999999556, 0.9583333333333333703, 0.9666666666666666741, 0.9749999999999999778, 0.9833333333333332815, 0.9916666666666666963, 1.000000000000000000 ),
 .UNSPECIFIED. ) 
 GEOMETRIC_REPRESENTATION_ITEM ( )  RATIONAL_B_SPLINE_SURFACE ( (
 ( 1.000000000000000000, 0.8660254037844387076, 1.000000000000000000, 0.8660254037844387076, 1.000000000000000000, 0.8660254037844387076, 1.000000000000000000, 0.8660254037844387076, 1.000000000000000000, 0.8660254037844387076, 1.000000000000000000, 0.8660254037844387076, 1.000000000000000000, 0.8660254037844387076, 1.000000000000000000, 0.8660254037844387076, 1.000000000000000000, 0.8660254037844387076, 1.000000000000000000, 0.8660254037844387076, 1.000000000000000000, 0.8660254037844387076, 1.000000000000000000, 0.8660254037844387076, 1.000000000000000000, 0.8660254037844387076, 1.000000000000000000, 0.8660254037844387076, 1.000000000000000000, 0.8660254037844387076, 1.000000000000000000, 0.8660254037844387076, 1.000000000000000000, 0.8660254037844387076, 1.000000000000000000, 0.8660254037844387076, 1.000000000000000000, 0.8660254037844387076, 1.000000000000000000, 0.8660254037844387076, 1.000000000000000000, 0.8660254037844387076, 1.000000000000000000, 0.8660254037844387076, 1.000000000000000000, 0.8660254037844387076, 1.000000000000000000, 0.8660254037844387076, 1.000000000000000000, 0.8660254037844387076, 1.000000000000000000, 0.8660254037844387076, 1.000000000000000000, 0.8660254037844387076, 1.000000000000000000, 0.8660254037844387076, 1.000000000000000000, 0.8660254037844387076, 1.000000000000000000, 0.8660254037844387076, 1.000000000000000000, 0.8660254037844387076, 1.000000000000000000, 0.8660254037844387076, 1.000000000000000000, 0.8660254037844387076, 1.000000000000000000, 0.8660254037844387076, 1.000000000000000000, 0.8660254037844387076, 1.000000000000000000, 0.8660254037844387076, 1.000000000000000000, 0.8660254037844387076, 1.000000000000000000, 0.8660254037844387076, 1.000000000000000000, 0.8660254037844387076, 1.000000000000000000, 0.8660254037844387076, 1.000000000000000000, 0.8660254037844387076, 1.000000000000000000, 0.8660254037844387076, 1.000000000000000000, 0.8660254037844387076, 1.000000000000000000, 0.8660254037844387076, 1.000000000000000000, 0.8660254037844387076, 1.000000000000000000, 0.8660254037844387076, 1.000000000000000000, 0.8660254037844387076, 1.000000000000000000, 0.8660254037844387076, 1.000000000000000000, 0.8660254037844387076, 1.000000000000000000, 0.8660254037844387076, 1.000000000000000000, 0.8660254037844387076, 1.000000000000000000, 0.8660254037844387076, 1.000000000000000000, 0.8660254037844387076, 1.000000000000000000, 0.8660254037844387076, 1.000000000000000000, 0.8660254037844387076, 1.000000000000000000, 0.8660254037844387076, 1.000000000000000000, 0.8660254037844387076, 1.000000000000000000, 0.8660254037844387076, 1.000000000000000000, 0.8660254037844387076, 1.000000000000000000, 0.8660254037844387076, 1.000000000000000000, 0.8660254037844387076, 1.000000000000000000, 0.8660254037844387076, 1.000000000000000000, 0.8660254037844387076, 1.000000000000000000, 0.8660254037844387076, 1.000000000000000000, 0.8660254037844387076, 1.000000000000000000, 0.8660254037844387076, 1.000000000000000000, 0.8660254037844387076, 1.000000000000000000, 0.8660254037844387076, 1.000000000000000000, 0.8660254037844387076, 1.000000000000000000, 0.8660254037844387076, 1.000000000000000000, 0.8660254037844387076, 1.000000000000000000, 0.8660254037844387076, 1.000000000000000000, 0.8660254037844387076, 1.000000000000000000, 0.8660254037844387076, 1.000000000000000000, 0.8660254037844387076, 1.000000000000000000, 0.8660254037844387076, 1.000000000000000000, 0.8660254037844387076, 1.000000000000000000, 0.8660254037844387076, 1.000000000000000000, 0.8660254037844387076, 1.000000000000000000, 0.8660254037844387076, 1.000000000000000000, 0.8660254037844387076, 1.000000000000000000, 0.8660254037844387076, 1.000000000000000000, 0.8660254037844387076, 1.000000000000000000, 0.8660254037844387076, 1.000000000000000000, 0.8660254037844387076, 1.000000000000000000, 0.8660254037844387076, 1.000000000000000000, 0.8660254037844387076, 1.000000000000000000, 0.8660254037844387076, 1.000000000000000000, 0.8660254037844387076, 1.000000000000000000, 0.8660254037844387076, 1.000000000000000000, 0.8660254037844387076, 1.000000000000000000, 0.8660254037844387076, 1.000000000000000000, 0.8660254037844387076, 1.000000000000000000, 0.8660254037844387076, 1.000000000000000000, 0.8660254037844387076, 1.000000000000000000, 0.8660254037844387076, 1.000000000000000000, 0.8660254037844387076, 1.000000000000000000, 0.8660254037844387076, 1.000000000000000000, 0.8660254037844387076, 1.000000000000000000, 0.8660254037844387076, 1.000000000000000000, 0.8660254037844387076, 1.000000000000000000, 0.8660254037844387076, 1.000000000000000000, 0.8660254037844387076, 1.000000000000000000, 0.8660254037844387076, 1.000000000000000000, 0.8660254037844387076, 1.000000000000000000, 0.8660254037844387076, 1.000000000000000000, 0.8660254037844387076, 1.000000000000000000, 0.8660254037844387076, 1.000000000000000000, 0.8660254037844387076, 1.000000000000000000, 0.8660254037844387076, 1.000000000000000000, 0.8660254037844387076, 1.000000000000000000, 0.8660254037844387076, 1.000000000000000000, 0.8660254037844387076, 1.000000000000000000, 0.8660254037844387076, 1.000000000000000000, 0.8660254037844387076, 1.000000000000000000, 0.8660254037844387076, 1.000000000000000000, 0.8660254037844387076, 1.000000000000000000, 0.8660254037844387076, 1.000000000000000000, 0.8660254037844387076, 1.000000000000000000, 0.8660254037844387076, 1.000000000000000000),
 ( 1.000000000000000000, 0.8660254037844387076, 1.000000000000000000, 0.8660254037844387076, 1.000000000000000000, 0.8660254037844387076, 1.000000000000000000, 0.8660254037844387076, 1.000000000000000000, 0.8660254037844387076, 1.000000000000000000, 0.8660254037844387076, 1.000000000000000000, 0.8660254037844387076, 1.000000000000000000, 0.8660254037844387076, 1.000000000000000000, 0.8660254037844387076, 1.000000000000000000, 0.8660254037844387076, 1.000000000000000000, 0.8660254037844387076, 1.000000000000000000, 0.8660254037844387076, 1.000000000000000000, 0.8660254037844387076, 1.000000000000000000, 0.8660254037844387076, 1.000000000000000000, 0.8660254037844387076, 1.000000000000000000, 0.8660254037844387076, 1.000000000000000000, 0.8660254037844387076, 1.000000000000000000, 0.8660254037844387076, 1.000000000000000000, 0.8660254037844387076, 1.000000000000000000, 0.8660254037844387076, 1.000000000000000000, 0.8660254037844387076, 1.000000000000000000, 0.8660254037844387076, 1.000000000000000000, 0.8660254037844387076, 1.000000000000000000, 0.8660254037844387076, 1.000000000000000000, 0.8660254037844387076, 1.000000000000000000, 0.8660254037844387076, 1.000000000000000000, 0.8660254037844387076, 1.000000000000000000, 0.8660254037844387076, 1.000000000000000000, 0.8660254037844387076, 1.000000000000000000, 0.8660254037844387076, 1.000000000000000000, 0.8660254037844387076, 1.000000000000000000, 0.8660254037844387076, 1.000000000000000000, 0.8660254037844387076, 1.000000000000000000, 0.8660254037844387076, 1.000000000000000000, 0.8660254037844387076, 1.000000000000000000, 0.8660254037844387076, 1.000000000000000000, 0.8660254037844387076, 1.000000000000000000, 0.8660254037844387076, 1.000000000000000000, 0.8660254037844387076, 1.000000000000000000, 0.8660254037844387076, 1.000000000000000000, 0.8660254037844387076, 1.000000000000000000, 0.8660254037844387076, 1.000000000000000000, 0.8660254037844387076, 1.000000000000000000, 0.8660254037844387076, 1.000000000000000000, 0.8660254037844387076, 1.000000000000000000, 0.8660254037844387076, 1.000000000000000000, 0.8660254037844387076, 1.000000000000000000, 0.8660254037844387076, 1.000000000000000000, 0.8660254037844387076, 1.000000000000000000, 0.8660254037844387076, 1.000000000000000000, 0.8660254037844387076, 1.000000000000000000, 0.8660254037844387076, 1.000000000000000000, 0.8660254037844387076, 1.000000000000000000, 0.8660254037844387076, 1.000000000000000000, 0.8660254037844387076, 1.000000000000000000, 0.8660254037844387076, 1.000000000000000000, 0.8660254037844387076, 1.000000000000000000, 0.8660254037844387076, 1.000000000000000000, 0.8660254037844387076, 1.000000000000000000, 0.8660254037844387076, 1.000000000000000000, 0.8660254037844387076, 1.000000000000000000, 0.8660254037844387076, 1.000000000000000000, 0.8660254037844387076, 1.000000000000000000, 0.8660254037844387076, 1.000000000000000000, 0.8660254037844387076, 1.000000000000000000, 0.8660254037844387076, 1.000000000000000000, 0.8660254037844387076, 1.000000000000000000, 0.8660254037844387076, 1.000000000000000000, 0.8660254037844387076, 1.000000000000000000, 0.8660254037844387076, 1.000000000000000000, 0.8660254037844387076, 1.000000000000000000, 0.8660254037844387076, 1.000000000000000000, 0.8660254037844387076, 1.000000000000000000, 0.8660254037844387076, 1.000000000000000000, 0.8660254037844387076, 1.000000000000000000, 0.8660254037844387076, 1.000000000000000000, 0.8660254037844387076, 1.000000000000000000, 0.8660254037844387076, 1.000000000000000000, 0.8660254037844387076, 1.000000000000000000, 0.8660254037844387076, 1.000000000000000000, 0.8660254037844387076, 1.000000000000000000, 0.8660254037844387076, 1.000000000000000000, 0.8660254037844387076, 1.000000000000000000, 0.8660254037844387076, 1.000000000000000000, 0.8660254037844387076, 1.000000000000000000, 0.8660254037844387076, 1.000000000000000000, 0.8660254037844387076, 1.000000000000000000, 0.8660254037844387076, 1.000000000000000000, 0.8660254037844387076, 1.000000000000000000, 0.8660254037844387076, 1.000000000000000000, 0.8660254037844387076, 1.000000000000000000, 0.8660254037844387076, 1.000000000000000000, 0.8660254037844387076, 1.000000000000000000, 0.8660254037844387076, 1.000000000000000000, 0.8660254037844387076, 1.000000000000000000, 0.8660254037844387076, 1.000000000000000000, 0.8660254037844387076, 1.000000000000000000, 0.8660254037844387076, 1.000000000000000000, 0.8660254037844387076, 1.000000000000000000, 0.8660254037844387076, 1.000000000000000000, 0.8660254037844387076, 1.000000000000000000, 0.8660254037844387076, 1.000000000000000000, 0.8660254037844387076, 1.000000000000000000, 0.8660254037844387076, 1.000000000000000000, 0.8660254037844387076, 1.000000000000000000, 0.8660254037844387076, 1.000000000000000000, 0.8660254037844387076, 1.000000000000000000, 0.8660254037844387076, 1.000000000000000000, 0.8660254037844387076, 1.000000000000000000, 0.8660254037844387076, 1.000000000000000000, 0.8660254037844387076, 1.000000000000000000, 0.8660254037844387076, 1.000000000000000000, 0.8660254037844387076, 1.000000000000000000, 0.8660254037844387076, 1.000000000000000000, 0.8660254037844387076, 1.000000000000000000, 0.8660254037844387076, 1.000000000000000000, 0.8660254037844387076, 1.000000000000000000, 0.8660254037844387076, 1.000000000000000000, 0.8660254037844387076, 1.000000000000000000, 0.8660254037844387076, 1.000000000000000000) ) ) 
 REPRESENTATION_ITEM ( '' )  SURFACE ( )  );
#177042 = CARTESIAN_POINT ( 'NONE',  ( -10.39320420135713263, 4.932286138528427344, 5.331284845095887626 ) ) ;
#177043 =( NAMED_UNIT ( * ) SI_UNIT ( $, .STERADIAN. ) SOLID_ANGLE_UNIT ( ) );
#177045 = CARTESIAN_POINT ( 'NONE',  ( 2.418345249890076154, 0.8361516037145629854, 1.774881043358336630 ) ) ;
#177044 = CARTESIAN_POINT ( 'NONE',  ( -6.507023659554960204, 9.678945805201045971, 1.199719254218452047 ) ) ;
#177046 = CARTESIAN_POINT ( 'NONE',  ( 1.006953172832128152, 1.636353683469338183, -1.412668763314451903 ) ) ;
#177048 = CARTESIAN_POINT ( 'NONE',  ( -5.891600325674557048, 6.152103933748189313, 0.8728944348482190474 ) ) ;
#177047 = CARTESIAN_POINT ( 'NONE',  ( -5.529746549527323474, 7.544733289238903851, -1.599625672291271394 ) ) ;
#177049 = CARTESIAN_POINT ( 'NONE',  ( -1.364683531250012516, 1.780208333674757615, 0.7879004041258379498 ) ) ;
#177050 = CARTESIAN_POINT ( 'NONE',  ( 2.477566078851959563, 1.547001316009195548, 0.7831083592614047628 ) ) ;
#177051 = CARTESIAN_POINT ( 'NONE',  ( 2.378492463385312394, 1.591508763844831531, -0.7045900751257595518 ) ) ;
#177052 = CARTESIAN_POINT ( 'NONE',  ( 6.466876084038451822, 10.48851316477946582, 1.040834085586084257E-14 ) ) ;
#177053 = CARTESIAN_POINT ( 'NONE',  ( -12.40359606095370992, 6.583381993447835256, -3.463844519762692364 ) ) ;
#177054 = CARTESIAN_POINT ( 'NONE',  ( 1.018907413236518789, 2.013924516646655949, -0.09611688112247382398 ) ) ;
#177055 = CARTESIAN_POINT ( 'NONE',  ( 6.825078400183550720, 7.629137130509051623, 2.644348168701659674 ) ) ;
#177056 = CARTESIAN_POINT ( 'NONE',  ( -4.553559489343377287, 6.405848385690952718, -1.599625672291271394 ) ) ;
#177057 = CARTESIAN_POINT ( 'NONE',  ( 1.428526753364509627, 1.899469058273341338, 0.5276583995704342556 ) ) ;
#177060 = ADVANCED_FACE ( 'NONE', ( #2399 ), #111692, .T. ) ;
#177059 = CARTESIAN_POINT ( 'NONE',  ( -5.316205630334263965, 7.295602216847000498, -1.443375672974066548 ) ) ;
#177058 = CARTESIAN_POINT ( 'NONE',  ( 5.467032840998240495, -1.503656711810175350, 1.181500457595338505 ) ) ;
#177061 = CARTESIAN_POINT ( 'NONE',  ( -4.434925645001610128, 8.188180662561590495, 0.7216878364870338292 ) ) ;
#177062 = CARTESIAN_POINT ( 'NONE',  ( 6.496291879603339758, 7.608037276739255006, 1.199719254218452935 ) ) ;
#177063 = CARTESIAN_POINT ( 'NONE',  ( -6.282224075085783177, 8.422623735723785643, 1.599625672291269396 ) ) ;
#177064 = CARTESIAN_POINT ( 'NONE',  ( 1.611979286579327431, -0.6784349324776539625, 1.902464779174169562 ) ) ;
#177065 = EDGE_CURVE ( 'NONE', #176800, #144861, #177342, .T. ) ;
#177066 = CARTESIAN_POINT ( 'NONE',  ( 4.296143005555221883, -0.8870401112092487494, 2.130475988740585080 ) ) ;
#177067 = CARTESIAN_POINT ( 'NONE',  ( 5.652778587040098834, -0.4750822840141955550, -1.903360745478323679 ) ) ;
#177068 = CARTESIAN_POINT ( 'NONE',  ( 2.975390029205774223, -0.1970676810524821243, 1.951864085487287959 ) ) ;
#177069 = CARTESIAN_POINT ( 'NONE',  ( 8.289920859751990889, 11.75899253876431416, 1.199719254218450271 ) ) ;
#177070 = CARTESIAN_POINT ( 'NONE',  ( -9.508835372460842095, 14.89852095282139643, 7.212874380408685226 ) ) ;
#177071 = ORIENTED_EDGE ( 'NONE', *, *, #130371, .T. ) ;
#177072 = CARTESIAN_POINT ( 'NONE',  ( 1.640021805331920213, 2.111262888970814267, -0.1616085204505824935 ) ) ;
#177074 = CARTESIAN_POINT ( 'NONE',  ( -6.184490626128011925, 10.36698949712469364, -0.7998128361456291469 ) ) ;
#177073 = CARTESIAN_POINT ( 'NONE',  ( -4.959585264500673496, 4.680604318205876524, 1.214306433183764966E-14 ) ) ;
#177075 = CARTESIAN_POINT ( 'NONE',  ( 2.255570300226293234, 0.7868700230135963203, 1.664660379391752043 ) ) ;
#177076 = VERTEX_POINT ( 'NONE', #18669 ) ;
#177077 = CARTESIAN_POINT ( 'NONE',  ( 11.94521494846196319, 7.576335522585334381, -0.4351009623805371374 ) ) ;
#177078 = CARTESIAN_POINT ( 'NONE',  ( 2.760144723603759065, 0.7592700852765141839, -1.980205354017528840 ) ) ;
#177079 = CARTESIAN_POINT ( 'NONE',  ( -1.500000000000011324, 4.910416667349486453, -0.8660254037844313801 ) ) ;
#177080 = CARTESIAN_POINT ( 'NONE',  ( 8.762647353133951711, 9.117510088278095282, 1.040834085586084257E-14 ) ) ;
#177081 = CARTESIAN_POINT ( 'NONE',  ( -0.3282377607281428689, 2.511164550367429804, -1.225000000000032285 ) ) ;
#177082 = CARTESIAN_POINT ( 'NONE',  ( 3.391920509712963661, -0.8384013316644415292, 1.882726026762149285 ) ) ;
#177084 = CARTESIAN_POINT ( 'NONE',  ( 0.1867156058280826092, 1.363667594142993877, 1.237386390646778578 ) ) ;
#177083 = CARTESIAN_POINT ( 'NONE',  ( -8.474009703741204547, 9.845098394908269768, -1.199719254218446718 ) ) ;
#177085 = CARTESIAN_POINT ( 'NONE',  ( -1.201851678989727383E-14, 3.446875000341421469, -1.575800808251660134 ) ) ;
#177086 = CARTESIAN_POINT ( 'NONE',  ( -0.02224634325196857970, 6.946779003630102700, -2.884187630258818302 ) ) ;
#177087 = CARTESIAN_POINT ( 'NONE',  ( 1.264550565627409195, 3.910972709771358247, 0.5006333728358396407 ) ) ;
#177088 = VECTOR ( 'NONE', #4340, 1000.000000000000000 ) ;
#177089 = CARTESIAN_POINT ( 'NONE',  ( 0.1181803206181560040, -2.163391993613572151, 0.4351206515559591370 ) ) ;
#177090 = CARTESIAN_POINT ( 'NONE',  ( 2.302381833152538082, -2.261912932826372735, 0.05377845686085034466 ) ) ;
#177091 = AXIS2_PLACEMENT_3D ( 'NONE', #163640, #160427, #14149 ) ;
#177092 = CARTESIAN_POINT ( 'NONE',  ( -8.676855123066019360, 11.14608361504227574, -1.443375672974059665 ) ) ;
#177093 = CARTESIAN_POINT ( 'NONE',  ( 2.847713089995526303, -1.219902489354685038, -1.339422833384727118 ) ) ;
#177094 = CARTESIAN_POINT ( 'NONE',  ( 2.835059001918965649, -1.568902116443865236, -1.099054045514812117 ) ) ;
#177095 = CARTESIAN_POINT ( 'NONE',  ( 4.703616579153604427, -1.598285800263723910, -1.315984976451072930 ) ) ;
#177096 = CARTESIAN_POINT ( 'NONE',  ( -0.6823417656249969321, 3.280208333674754062, -1.181850606188749264 ) ) ;
#177097 = CARTESIAN_POINT ( 'NONE',  ( 1.639464495141579770, -1.426599704724445861, -1.360921036830293307 ) ) ;
#177098 = CARTESIAN_POINT ( 'NONE',  ( 0.2000540296341560831, -1.925883223908849251, -0.05090804828828016798 ) ) ;
#177099 = CARTESIAN_POINT ( 'NONE',  ( 3.344469905398727239, 0.4532862802011444758, 1.814783984445811127 ) ) ;
#177101 = CARTESIAN_POINT ( 'NONE',  ( 4.639288533706844575, 8.435234533841581950, -0.4270733708018232822 ) ) ;
#177100 = CARTESIAN_POINT ( 'NONE',  ( 2.297912027771050081, 1.785232721601331507, 1.462330537539487496 ) ) ;
#177102 = CARTESIAN_POINT ( 'NONE',  ( 2.998338655031260735, 1.846661096025622228, 0.2305314943511579950 ) ) ;
#177103 = CARTESIAN_POINT ( 'NONE',  ( -1.364683531250012516, 3.488541667008085767, -0.7879004041258300672 ) ) ;
#177104 = CARTESIAN_POINT ( 'NONE',  ( 6.707491137888100141, -1.654371308887558234, -1.231747576844913539 ) ) ;
#177105 = CARTESIAN_POINT ( 'NONE',  ( -4.574986769607567894, 7.424902766929059261, 1.199719254218464037 ) ) ;
#177106 = CARTESIAN_POINT ( 'NONE',  ( 6.938021921891177612, 9.117444880338284818, -1.599625672291262513 ) ) ;
#177107 = CARTESIAN_POINT ( 'NONE',  ( -1.392249819062528760, 3.364685323634090341, 0.1369250707803940370 ) ) ;
#177108 = CARTESIAN_POINT ( 'NONE',  ( 6.036178822307518566, 1.040974378708346526, -1.830621892639591630 ) ) ;
#177109 = CARTESIAN_POINT ( 'NONE',  ( 1.364683531249988535, 3.967708333674751842, -0.7879004041258239610 ) ) ;
#177110 = CARTESIAN_POINT ( 'NONE',  ( 6.116527240895272222, 1.456737685447502262, -1.597155580871166602 ) ) ;
#177111 = CARTESIAN_POINT ( 'NONE',  ( 6.322916996384010169, 1.495059732148263487, -1.358068445443241457 ) ) ;
#177112 = CARTESIAN_POINT ( 'NONE',  ( 1.364683531249986537, -0.5947916663252456049, -0.7879004041258309554 ) ) ;
#177113 = CARTESIAN_POINT ( 'NONE',  ( -3.795919822146277767, 7.372397525905215687, -0.7216878364870267237 ) ) ;
#177116 = CARTESIAN_POINT ( 'NONE',  ( 3.551873057100274789, 7.087676300018221021, 0.7216878364870298324 ) ) ;
#177115 = CARTESIAN_POINT ( 'NONE',  ( 1.642778471875001811, -0.6927083328553753638, 2.845375778867859751 ) ) ;
#177114 = CARTESIAN_POINT ( 'NONE',  ( 5.417364897112183719, 8.477953592343014932, 1.199719254218451159 ) ) ;
#177117 = CARTESIAN_POINT ( 'NONE',  ( -3.318713740295064163, 7.093859473644694269, 0.000000000000000000 ) ) ;
#177118 = CARTESIAN_POINT ( 'NONE',  ( 4.733611406029458735, 0.6279933214467496860, -1.916352419866963697 ) ) ;
#177119 = CARTESIAN_POINT ( 'NONE',  ( -6.852756576703439961, 10.08230087520760954, 1.199719254218453823 ) ) ;
#177121 = CARTESIAN_POINT ( 'NONE',  ( -7.390603132780795725, 8.755363422066633206, -1.082531754730549967 ) ) ;
#177120 = CARTESIAN_POINT ( 'NONE',  ( -9.503902493499651882, 10.19023378527882784, 1.040834085586084257E-14 ) ) ;
#177122 = CYLINDRICAL_SURFACE ( 'NONE', #212368, 0.3999999999999997446 ) ;
#177124 = CARTESIAN_POINT ( 'NONE',  ( 1.364683531249997417, 9.734375000341396245, 2.602085213965210642E-15 ) ) ;
#177123 = CARTESIAN_POINT ( 'NONE',  ( 5.559502693676295237, 0.4258712887980077300, -2.119171757835013548 ) ) ;
#177125 =( NAMED_UNIT ( * ) PLANE_ANGLE_UNIT ( ) SI_UNIT ( $, .RADIAN. ) );
#177126 = CARTESIAN_POINT ( 'NONE',  ( -11.33112879397343065, 6.585244639288670321, 3.816637121560833013 ) ) ;
#177128 = CARTESIAN_POINT ( 'NONE',  ( 0.05214973123207015254, -1.250902960675448483, 1.450897702916327248 ) ) ;
#177127 = CARTESIAN_POINT ( 'NONE',  ( -5.870317324592811303, 8.832158731124840401, -1.082531754730537976 ) ) ;
#177129 = CARTESIAN_POINT ( 'NONE',  ( -0.6823417656250246877, -0.8864583329919115684, 1.181850606188755259 ) ) ;
#177130 = CARTESIAN_POINT ( 'NONE',  ( -15.75000000000000000, 11.29999999999998117, 1.799999999999999600 ) ) ;
#177131 = CARTESIAN_POINT ( 'NONE',  ( 1.717014342725260656, -0.2134408525867482198, 1.711538560699257916 ) ) ;
#177132 = CARTESIAN_POINT ( 'NONE',  ( 3.573456005653643519, 6.326726552307992080, -1.199719254218453823 ) ) ;
#177133 = AXIS2_PLACEMENT_3D ( 'NONE', #181923, #165692, #1024 ) ;
#177134 = CARTESIAN_POINT ( 'NONE',  ( 5.825163275726873202, 6.825053905550038991, 1.199719254218452047 ) ) ;
#177135 = CARTESIAN_POINT ( 'NONE',  ( -11.71930699919508356, 8.545276028816752856, 2.376758398160924379 ) ) ;
#177136 = CARTESIAN_POINT ( 'NONE',  ( 0.8601951712396675997, -1.287299901140761316, 1.214705651989380852 ) ) ;
#177137 =( NAMED_UNIT ( * ) SI_UNIT ( $, .STERADIAN. ) SOLID_ANGLE_UNIT ( ) );
#177138 = EDGE_CURVE ( 'NONE', #73749, #123257, #184269, .T. ) ;
#177139 = CARTESIAN_POINT ( 'NONE',  ( 3.786314268594536347, -1.089870966172037825, 1.918795532666245363 ) ) ;
#177140 = CARTESIAN_POINT ( 'NONE',  ( 5.506739464099510428, 0.6230791789904217559, 2.079776831526482628 ) ) ;
#177141 = EDGE_LOOP ( 'NONE', ( #100690, #112756, #27456, #150692 ) ) ;
#177142 = CARTESIAN_POINT ( 'NONE',  ( 5.083381250481017410, 4.895309311841474553, 0.7998128361456352531 ) ) ;
#177143 = CARTESIAN_POINT ( 'NONE',  ( 7.741342523278698096, 10.05465224862374285, 1.443375672974076540 ) ) ;
#177145 = CARTESIAN_POINT ( 'NONE',  ( 2.706657832681820697, 1.899625987897411772, 0.6766965020792228280 ) ) ;
#177144 = CARTESIAN_POINT ( 'NONE',  ( 2.824977599723184074, 1.534285384246200090, -1.463936014953904463 ) ) ;
#177147 = ORIENTED_EDGE ( 'NONE', *, *, #43686, .F. ) ;
#177146 = CARTESIAN_POINT ( 'NONE',  ( 2.847713089995526303, -1.219902489354685038, -1.339422833384727118 ) ) ;
#177148 = CARTESIAN_POINT ( 'NONE',  ( 6.710359684120930091, 6.793450817754725257, 0.7998128361456352531 ) ) ;
#177149 = VERTEX_POINT ( 'NONE', #185438 ) ;
#177150 = CARTESIAN_POINT ( 'NONE',  ( 0.5670072068131201126, 0.1877032549213939472, -1.861219751863735672 ) ) ;
#177151 = CARTESIAN_POINT ( 'NONE',  ( 5.666418135507635512, 8.698239360479199433, 1.199719254218462483 ) ) ;
#177152 = AXIS2_PLACEMENT_3D ( 'NONE', #121478, #81686, #103012 ) ;
#177154 = CARTESIAN_POINT ( 'NONE',  ( 1.639701460626964868, 1.910339084310968660, -0.1447352371885517186 ) ) ;
#177153 = CARTESIAN_POINT ( 'NONE',  ( -3.958090780185743451, 6.705190779270287393, -1.199719254218452047 ) ) ;
#177155 = CARTESIAN_POINT ( 'NONE',  ( -11.94105721237523099, 12.69999999999999929, -1.187919463087249827 ) ) ;
#177156 = CARTESIAN_POINT ( 'NONE',  ( -1.402160292154681736E-14, 2.009375000341422801, -1.575800808251660134 ) ) ;
#177157 = CARTESIAN_POINT ( 'NONE',  ( 0.000000000000000000, 0.000000000000000000, -2.000000000000000000 ) ) ;
#177158 = CARTESIAN_POINT ( 'NONE',  ( -8.565000355531095622, 11.01558638625153286, -1.599625672291263179 ) ) ;
#177159 = CARTESIAN_POINT ( 'NONE',  ( 4.803922858132807505, -1.082837210388952309, -1.700963621564715700 ) ) ;
#177160 = CARTESIAN_POINT ( 'NONE',  ( 4.961884481312108797, 2.138711985806662330, -0.3135959325617638238 ) ) ;
#177161 = CARTESIAN_POINT ( 'NONE',  ( -5.804299160426242388, 6.904675454319632699, -1.082531754730549967 ) ) ;
#177162 = CARTESIAN_POINT ( 'NONE',  ( -5.101610940492132151, 9.173906207207963348, -0.7998128361456362523 ) ) ;
#177163 = CARTESIAN_POINT ( 'NONE',  ( 3.094099843433151253, 1.348383549611749332, 1.636666742212993686 ) ) ;
#177164 = EDGE_CURVE ( 'NONE', #143545, #92745, #182236, .T. ) ;
#177166 = CARTESIAN_POINT ( 'NONE',  ( -11.33520460194134394, 5.279085700950885141, -5.677819296561938955 ) ) ;
#177165 = DIRECTION ( 'NONE',  ( -0.008295560218253903231, 0.000000000000000000, -0.9999655912483516040 ) ) ;
#177167 = CARTESIAN_POINT ( 'NONE',  ( 4.815676612163926507, -1.933897303736350270, 0.3816649536505806184 ) ) ;
#177168 = CARTESIAN_POINT ( 'NONE',  ( 6.258066496116281741, 0.7254575739856858885, -1.769658340881982816 ) ) ;
#177169 = EDGE_LOOP ( 'NONE', ( #51444, #67401, #73406, #91704 ) ) ;
#177170 = CARTESIAN_POINT ( 'NONE',  ( 6.069547426979996274, 1.461697874074740389, 1.532048495917796016 ) ) ;
#177171 =( NAMED_UNIT ( * ) PLANE_ANGLE_UNIT ( ) SI_UNIT ( $, .RADIAN. ) );
#177172 = CARTESIAN_POINT ( 'NONE',  ( 0.4321921490204432281, 1.190796696626210682, 1.693455153822187587 ) ) ;
#177173 = CARTESIAN_POINT ( 'NONE',  ( 2.501813746025891128, -0.7434988463325925556, -1.794173334931578712 ) ) ;
#177174 = ORIENTED_EDGE ( 'NONE', *, *, #118655, .T. ) ;
#177175 = CARTESIAN_POINT ( 'NONE',  ( -4.343881772442427014, 7.212430371758029146, -1.015018499812924135 ) ) ;
#177176 = CARTESIAN_POINT ( 'NONE',  ( 6.119526231721748033, 8.232809585132461194, 1.599625672291269396 ) ) ;
#177177 = B_SPLINE_CURVE_WITH_KNOTS ( 'NONE', 3,
 ( #107739, #203004, #169459, #56781, #204057, #121863, #53578, #104475, #173763, #88217, #87143, #106651, #3725, #120792, #119712, #6932, #205138, #186769, #55710, #187834, #38396, #122948, #170522, #103399, #22104, #138044, #188906, #40547, #63184, #176939 ),
 .UNSPECIFIED., .F., .F.,
 ( 4, 2, 2, 2, 2, 2, 2, 2, 2, 2, 2, 2, 2, 2, 4 ),
 ( 0.000000000000000000, 0.001872196198237568955, 0.002808294297356353324, 0.003744392396475137910, 0.004680490495593922495, 0.005616588594712706647, 0.007488784792950275819, 0.008424882892069060839, 0.009360980991187844991, 0.01029707909030662914, 0.01123317718942541329, 0.01216927528854419745, 0.01310537338766298333, 0.01404147148678176749, 0.01497756958590055164 ),
 .UNSPECIFIED. ) ;
#177179 = CARTESIAN_POINT ( 'NONE',  ( 5.849453209292126310, 8.911780279894442103, 1.199719254218462483 ) ) ;
#177178 = CARTESIAN_POINT ( 'NONE',  ( 3.064484987736408872, -1.931880230092865025, -0.7996142226951181708 ) ) ;
#177180 = CARTESIAN_POINT ( 'NONE',  ( 5.045042557616584489, 5.058506870073687267, 0.000000000000000000 ) ) ;
#177182 = ORIENTED_EDGE ( 'NONE', *, *, #178292, .F. ) ;
#177181 = CARTESIAN_POINT ( 'NONE',  ( 0.4163052458206939477, -0.6087807487058238820, -1.706225765549937545 ) ) ;
#177183 = CARTESIAN_POINT ( 'NONE',  ( 5.901041445831935128, 1.806360628843254768, -1.267562117129708454 ) ) ;
#177184 = CARTESIAN_POINT ( 'NONE',  ( -0.4694063952341900881, -6.893137084989856334, -10.98997987423602751 ) ) ;
#177186 = EDGE_CURVE ( 'NONE', #33524, #78562, #206908, .T. ) ;
#177185 = CIRCLE ( 'NONE', #166823, 0.08000000000000020983 ) ;
#177187 = CARTESIAN_POINT ( 'NONE',  ( 2.802037382575186975, -0.6933082239683820980, 2.095089865402133267 ) ) ;
#177188 = CARTESIAN_POINT ( 'NONE',  ( 1.910667195161031007, -0.5113573046386342691, -1.842555643073694238 ) ) ;
#177189 = CARTESIAN_POINT ( 'NONE',  ( 10.26082332744404368, 10.86538205830655279, -0.7998128361456281477 ) ) ;
#177190 = CARTESIAN_POINT ( 'NONE',  ( 4.861816338261779613, -0.5554421346023461492, 1.994381909410049891 ) ) ;
#177192 = CARTESIAN_POINT ( 'NONE',  ( 3.292016909520224743, -0.8776455207864016783, 1.975710135277891633 ) ) ;
#177191 = CARTESIAN_POINT ( 'NONE',  ( -3.952365473583647315, 4.569846793057691592, 1.199719254218462483 ) ) ;
#177193 = CARTESIAN_POINT ( 'NONE',  ( 4.564136437409766600, -1.431273618155091576, 1.659743667367798103 ) ) ;
#177194 = ORIENTED_EDGE ( 'NONE', *, *, #26695, .T. ) ;
#177195 = CARTESIAN_POINT ( 'NONE',  ( -4.858757509019059562, 5.629766575900002401, 2.499999999999999556 ) ) ;
#177196 = ADVANCED_FACE ( 'NONE', ( #156171 ), #187577, .T. ) ;
#177197 = CARTESIAN_POINT ( 'NONE',  ( 4.002706559696581401, 7.742679268553477101, 0.2606817014456235815 ) ) ;
#177198 = CARTESIAN_POINT ( 'NONE',  ( -4.373855720720293050, 15.44734568083558912, 11.13580561285369264 ) ) ;
#177199 = CARTESIAN_POINT ( 'NONE',  ( 6.710359684120930091, 6.793450817754725257, 0.7998128361456352531 ) ) ;
#177200 = CARTESIAN_POINT ( 'NONE',  ( 3.285556943749998737, -2.442708332855375364, -1.896917185911906722 ) ) ;
#177201 = CARTESIAN_POINT ( 'NONE',  ( -7.462104991928524278, -5.166862915010159263, -8.081892667527526442 ) ) ;
#177202 = EDGE_CURVE ( 'NONE', #512, #83383, #157769, .T. ) ;
#177203 = CARTESIAN_POINT ( 'NONE',  ( 0.2818752512256904597, 1.674885806461807958, -1.122501178855893400 ) ) ;
#177204 = CARTESIAN_POINT ( 'NONE',  ( -9.815740026613967828, 10.55404424057886636, -0.7216878364870267237 ) ) ;
#177205 = CARTESIAN_POINT ( 'NONE',  ( 4.362691568547328202, 8.311833606605697256, -0.7998128361456381397 ) ) ;
#177206 = CARTESIAN_POINT ( 'NONE',  ( 5.049704560591026237, 1.530381825397047812, 1.394388655583590042 ) ) ;
#177207 = CARTESIAN_POINT ( 'NONE',  ( 3.422408909100621344, 1.221451249705886477, -1.489789856891531761 ) ) ;
#177208 = CARTESIAN_POINT ( 'NONE',  ( 6.556269899348222907, -1.302956475595556496, 1.669668561148303976 ) ) ;
#177209 = CARTESIAN_POINT ( 'NONE',  ( 5.606460214450851964, 6.499623990736163037, 1.199719254218462483 ) ) ;
#177210 = CARTESIAN_POINT ( 'NONE',  ( 9.681420877353911436, 3.865149423709368648, 7.090140323037526393 ) ) ;
#177211 = CARTESIAN_POINT ( 'NONE',  ( 4.416829296269289884, -1.462161721869711384, 1.319618631580289581 ) ) ;
#177212 = CARTESIAN_POINT ( 'NONE',  ( 0.7268461993804631316, 0.1648446022758827123, 2.185306563462440899 ) ) ;
#177213 = CARTESIAN_POINT ( 'NONE',  ( 3.545350327189537687, -1.383302465072188792, -1.191577590537174158 ) ) ;
#177214 = CARTESIAN_POINT ( 'NONE',  ( 7.241463443474815520, 8.581367117876336437, -1.082531754730548412 ) ) ;
#177215 = CARTESIAN_POINT ( 'NONE',  ( 3.511198595814932766, 5.119484333249288532, 1.443375672974066548 ) ) ;
#177216 = CARTESIAN_POINT ( 'NONE',  ( -7.618755976236585958, 7.853246491889623648, 0.000000000000000000 ) ) ;
#177217 = CARTESIAN_POINT ( 'NONE',  ( 5.890091390494168522, 5.836471141856793388, 0.000000000000000000 ) ) ;
#177218 =( BOUNDED_CURVE ( )  B_SPLINE_CURVE ( 2, ( #23662, #168854, #22584, #57247, #41014, #20457, #202394 ),
 .UNSPECIFIED., .F., .T. ) 
 B_SPLINE_CURVE_WITH_KNOTS ( ( 3, 2, 2, 3 ),
 ( 0.03571428571428574700, 0.04166666666666662272, 0.04761904761904750538, 0.05357142857142838110 ),
 .UNSPECIFIED. ) 
 CURVE ( )  GEOMETRIC_REPRESENTATION_ITEM ( )  RATIONAL_B_SPLINE_CURVE ( ( 0.9999999999999992228, 0.8660254037844394848, 1.000000000000000000, 0.8660254037844387076, 1.000000000000000000, 0.8660254037844429265, 0.9999999999999957812 ) ) 
 REPRESENTATION_ITEM ( '' )  );
#177219 = ORIENTED_EDGE ( 'NONE', *, *, #178292, .T. ) ;
#177221 = CARTESIAN_POINT ( 'NONE',  ( 4.588143835816930860, 1.162566388618992308, 1.643413508355499708 ) ) ;
#177220 = CARTESIAN_POINT ( 'NONE',  ( 1.839159199666509981, 0.7036077657225293658, -1.701706503975081830 ) ) ;
#177222 = CARTESIAN_POINT ( 'NONE',  ( 1.441203352352852463, 1.369654091668540241, 1.845602877388529572 ) ) ;
#177223 = CARTESIAN_POINT ( 'NONE',  ( 4.996903459272755477, 0.3314677610860050083, 1.933379042443456486 ) ) ;
#177224 = CARTESIAN_POINT ( 'NONE',  ( -6.018930129462987999, 9.109503353427070849, 1.199719254218452047 ) ) ;
#177225 = CARTESIAN_POINT ( 'NONE',  ( 0.2333690889706717397, 6.947499272388762748, -2.648434294982876303 ) ) ;
#177226 = CARTESIAN_POINT ( 'NONE',  ( -2.137381772448751605, 5.645362501165475777, -0.7998128361456281477 ) ) ;
#177227 = LINE ( 'NONE', #163115, #144088 ) ;
#177228 = CARTESIAN_POINT ( 'NONE',  ( -5.123001941117347080, 7.070197912760590064, 1.599625672291263179 ) ) ;
#177230 = CARTESIAN_POINT ( 'NONE',  ( 0.3736316133628528879, 1.073300769168658908, 1.531925686032776124 ) ) ;
#177229 = CARTESIAN_POINT ( 'NONE',  ( 1.821934285652214935, 1.201201420651318630, -1.711045060523497030 ) ) ;
#177231 = CARTESIAN_POINT ( 'NONE',  ( 0.2939347205469426960, 8.204283511488981162, -1.979604457746027446 ) ) ;
#177232 = CARTESIAN_POINT ( 'NONE',  ( -0.1104750535120268828, 4.084583917300320444, -2.658209514912849514 ) ) ;
#177233 = CARTESIAN_POINT ( 'NONE',  ( 2.331276520414362174, 0.8190846186081652824, -1.535621120930601213 ) ) ;
#177234 = CARTESIAN_POINT ( 'NONE',  ( 4.638861114170084399, 8.563755066507100722, 0.7998128361456462443 ) ) ;
#177236 = DIRECTION ( 'NONE',  ( -0.000000000000000000, 1.000000000000000000, 0.000000000000000000 ) ) ;
#177235 = CARTESIAN_POINT ( 'NONE',  ( 1.734723475976807094E-15, 14.55305236562695193, 11.95586206896570580 ) ) ;
#177237 = CARTESIAN_POINT ( 'NONE',  ( 2.174029202910219283, -1.062355927555928226, 1.358808029953484597 ) ) ;
#177238 = CARTESIAN_POINT ( 'NONE',  ( 1.681448347407452193, 1.514353137444489406, 1.584415833815432162 ) ) ;
#177239 = CARTESIAN_POINT ( 'NONE',  ( 4.213639274598267370, -0.3785452818781535611, 2.174016619501429215 ) ) ;
#177240 = CARTESIAN_POINT ( 'NONE',  ( -9.645406396194509568, 4.042443384815813445, -6.587269312116742270 ) ) ;
#177241 = AXIS2_PLACEMENT_3D ( 'NONE', #171768, #157670, #191201 ) ;
#177242 = CARTESIAN_POINT ( 'NONE',  ( 2.571331741745811250, 1.937545498039330960, 0.9797267027546376905 ) ) ;
#177243 = CARTESIAN_POINT ( 'NONE',  ( 0.6799654140086827114, -1.016662149479659494, 1.516215539243186639 ) ) ;
#177244 = CARTESIAN_POINT ( 'NONE',  ( 3.292305547686771305, -0.8622227623886582482, -1.934024985413025810 ) ) ;
#177245 = VECTOR ( 'NONE', #92417, 1000.000000000000114 ) ;
#177246 = CARTESIAN_POINT ( 'NONE',  ( 6.539320575229245591, 2.459069921018588900, 2.280790101157427419 ) ) ;
#177247 = VERTEX_POINT ( 'NONE', #24004 ) ;
#177249 = CARTESIAN_POINT ( 'NONE',  ( -1.364683531250014514, -0.1989583329919157317, -0.7879004041258359514 ) ) ;
#177248 = CARTESIAN_POINT ( 'NONE',  ( 3.597495906037956992, -0.6642907406799610781, 2.194031518130711067 ) ) ;
#177250 = FACE_OUTER_BOUND ( 'NONE', #88466, .T. ) ;
#177251 = CARTESIAN_POINT ( 'NONE',  ( 4.878236342818665250, 4.585697242910212523, 1.040834085586084257E-14 ) ) ;
#177252 = CARTESIAN_POINT ( 'NONE',  ( 6.375645204974608404, 0.3829637424261604361, -2.187886986038441339 ) ) ;
#177253 = CARTESIAN_POINT ( 'NONE',  ( -7.388830529767770550, 7.722649827591604677, 1.040834085586084257E-14 ) ) ;
#177254 = CARTESIAN_POINT ( 'NONE',  ( 4.907688418466886304, 5.788353245375237321, -1.082531754730548412 ) ) ;
#177255 = CARTESIAN_POINT ( 'NONE',  ( -8.337901282280023807, 8.829899038855916871, 0.7216878364870438212 ) ) ;
#177256 = CARTESIAN_POINT ( 'NONE',  ( 4.909461021924244051, 6.821066840368686712, 1.443375672974065660 ) ) ;
#177257 = ORIENTED_EDGE ( 'NONE', *, *, #73951, .T. ) ;
#177258 = CARTESIAN_POINT ( 'NONE',  ( 3.815077410725797424, 1.076317812134291119, -1.704938119663282903 ) ) ;
#177260 = CARTESIAN_POINT ( 'NONE',  ( 2.641531011850445143, 1.887532825382558066, -0.8318756707885038848 ) ) ;
#177259 = CARTESIAN_POINT ( 'NONE',  ( 7.298366762858032430, 7.409182732956175244, 1.040834085586084257E-14 ) ) ;
#177261 = DIRECTION ( 'NONE',  ( 0.000000000000000000, -0.000000000000000000, -1.000000000000000000 ) ) ;
#177262 = CARTESIAN_POINT ( 'NONE',  ( 5.248414861821569133, 6.256143772614186638, -1.082531754730548412 ) ) ;
#177263 = CARTESIAN_POINT ( 'NONE',  ( -1.642778471875000035, -2.617708332855375186, -2.845375778867859751 ) ) ;
#177264 = CARTESIAN_POINT ( 'NONE',  ( 1.364683531249988535, 4.405208333674754506, -0.7879004041258300672 ) ) ;
#177265 = CARTESIAN_POINT ( 'NONE',  ( 5.437503290160631941, 0.8905978969957989433, -2.002497223260243153 ) ) ;
#177266 = CARTESIAN_POINT ( 'NONE',  ( 2.883435573726996548, -0.5880205015329244000, -1.928751729079546173 ) ) ;
#177267 = CARTESIAN_POINT ( 'NONE',  ( 1.698526806778306586, 1.531337151408303621, 1.022036240780115346 ) ) ;
#177268 = ADVANCED_FACE ( 'NONE', ( #25077 ), #38142, .T. ) ;
#177269 = CARTESIAN_POINT ( 'NONE',  ( 5.795220594837462436, 8.848508896363995291, -1.199719254218440723 ) ) ;
#177270 =( LENGTH_UNIT ( ) NAMED_UNIT ( * ) SI_UNIT ( .MILLI., .METRE. ) );
#177271 = CARTESIAN_POINT ( 'NONE',  ( 5.438443955714742373, 1.798867289239113987, 0.3102399082220568816 ) ) ;
#177272 = CARTESIAN_POINT ( 'NONE',  ( 5.889296118903345700, -0.7283762112263308941, -1.880435897373772258 ) ) ;
#177273 = CARTESIAN_POINT ( 'NONE',  ( -7.527801604085656351, 9.805521176231838609, 1.599625672291295375 ) ) ;
#177275 = CARTESIAN_POINT ( 'NONE',  ( -5.306037014901836990, 7.283738832175834510, 1.599625672291263179 ) ) ;
#177274 = CARTESIAN_POINT ( 'NONE',  ( 5.858358025671378755, 0.9108227554960802719, 2.071263147418811013 ) ) ;
#177276 = CARTESIAN_POINT ( 'NONE',  ( 0.5574226275508349371, -1.780365264567655759, -1.124781644112993417 ) ) ;
#177277 = CARTESIAN_POINT ( 'NONE',  ( -6.343235766347277149, 8.493804042195527870, -1.599625672291271394 ) ) ;
#177278 = CARTESIAN_POINT ( 'NONE',  ( 7.228468454380276853, 11.58496363008569574, 1.040834085586084257E-14 ) ) ;
#177279 = CARTESIAN_POINT ( 'NONE',  ( 7.526184668917440312, 8.913541880892736913, -1.082531754730548412 ) ) ;
#177280 = DIRECTION ( 'NONE',  ( -5.838456228536615828E-18, 0.9999999999999998890, 2.399974822839792562E-17 ) ) ;
#177281 = CARTESIAN_POINT ( 'NONE',  ( -6.527360889975461156, 9.702672574024962415, 1.199719254218452047 ) ) ;
#177282 = UNCERTAINTY_MEASURE_WITH_UNIT (LENGTH_MEASURE( 1.000000000000000082E-05 ), #210372, 'distance_accuracy_value', 'NONE');
#177283 = CARTESIAN_POINT ( 'NONE',  ( -3.816847834374289317, 7.349700740952370914, -0.7361462914088554577 ) ) ;
#177284 = CARTESIAN_POINT ( 'NONE',  ( 6.114364089638775646, 10.07724917131317355, 0.7216878364870438212 ) ) ;
#177285 = CARTESIAN_POINT ( 'NONE',  ( 4.088248116760357931, 7.710168519003287813, -0.6407031029972446445 ) ) ;
#177286 = CARTESIAN_POINT ( 'NONE',  ( -7.849807752632384172, 12.10193344480572897, 0.000000000000000000 ) ) ;
#177288 = CARTESIAN_POINT ( 'NONE',  ( 2.935994361307178391, -2.139806239105252583, 0.5962572732955830901 ) ) ;
#177287 = CARTESIAN_POINT ( 'NONE',  ( 1.670341986359990205, 2.114562342887704283, -0.1611296783964668855 ) ) ;
#177289 = VECTOR ( 'NONE', #65012, 1000.000000000000000 ) ;
#177290 = CARTESIAN_POINT ( 'NONE',  ( -3.188928480291426837, 8.980740528189164351, -2.451733079074508659 ) ) ;
#177291 = CARTESIAN_POINT ( 'NONE',  ( -6.286140498591554326, 7.362860665558790707, 1.199719254218452047 ) ) ;
#177292 = CARTESIAN_POINT ( 'NONE',  ( 6.796715079152391148, 6.823922435299587974, 0.7998128361456341429 ) ) ;
#177293 = CARTESIAN_POINT ( 'NONE',  ( 3.894932841003693191, 0.2855096342280309396, 1.940843471192068570 ) ) ;
#177294 = CARTESIAN_POINT ( 'NONE',  ( 10.22692794340986921, 10.82583744360002243, 0.000000000000000000 ) ) ;
#177295 = CARTESIAN_POINT ( 'NONE',  ( -4.609732581575539889, 6.945374051331699938, 1.198810113796699328 ) ) ;
#177296 = CARTESIAN_POINT ( 'NONE',  ( 4.467575310902914154, 5.170924936596891008, 1.199719254218464037 ) ) ;
#177297 = CARTESIAN_POINT ( 'NONE',  ( -5.817857314039913241, 5.960124085900898372, 0.000000000000000000 ) ) ;
#177299 = VERTEX_POINT ( 'NONE', #89040 ) ;
#177298 = CARTESIAN_POINT ( 'NONE',  ( -5.897433632264490910, 9.824163637709826702, 0.000000000000000000 ) ) ;
#177300 = CARTESIAN_POINT ( 'NONE',  ( 3.480829117359967917, -1.421471314662653196, 1.573842340227212366 ) ) ;
#177301 = CARTESIAN_POINT ( 'NONE',  ( -5.808742468812186033, 5.741564066561132940, 0.000000000000000000 ) ) ;
#177302 = CARTESIAN_POINT ( 'NONE',  ( 4.364260218091946975, 1.016419123106377276, 1.907829002176253175 ) ) ;
#177303 = CARTESIAN_POINT ( 'NONE',  ( 3.632213977189250098, 0.2737156317273430894, 1.820677940640710979 ) ) ;
#177304 = CARTESIAN_POINT ( 'NONE',  ( -4.446147712686649989, 7.104319146577407373, 1.107073289137233241 ) ) ;
#177305 = CARTESIAN_POINT ( 'NONE',  ( -1.402160292154681736E-14, 0.5093750003414236893, -1.575800808251659024 ) ) ;
#177306 = CARTESIAN_POINT ( 'NONE',  ( 5.296709758707953242, 1.425846067417353868, 0.9975513609157842243 ) ) ;
#177307 = CARTESIAN_POINT ( 'NONE',  ( 4.446711195602238931, 6.210915699667823198, -1.443375672974051449 ) ) ;
#177308 = CARTESIAN_POINT ( 'NONE',  ( 11.01135777277262306, 10.19999999999999929, -1.400000000000001910 ) ) ;
#177309 = CARTESIAN_POINT ( 'NONE',  ( 3.309602206082487008, -0.4233974974612622066, 2.119663826602156131 ) ) ;
#177310 = AXIS2_PLACEMENT_3D ( 'NONE', #143089, #64970, #129012 ) ;
#177311 = CARTESIAN_POINT ( 'NONE',  ( 5.167342215279058237, -0.6766115767681828430, -1.899327316215810857 ) ) ;
#177312 = CARTESIAN_POINT ( 'NONE',  ( -8.798878505144649864, 11.28844422746735532, -1.443375672974058777 ) ) ;
#177314 = VECTOR ( 'NONE', #37477, 1000.000000000000000 ) ;
#177313 = CARTESIAN_POINT ( 'NONE',  ( 2.852577672069932735, 0.7271573612388192442, 2.035869728763760378 ) ) ;
#177315 = CARTESIAN_POINT ( 'NONE',  ( 3.778557292509187260, -1.899022758751211182, -0.5288098451153611101 ) ) ;
#177316 = CARTESIAN_POINT ( 'NONE',  ( 4.915543477551369556, -1.042145293856342914, -1.638595356941417114 ) ) ;
#177320 = VERTEX_POINT ( 'NONE', #104214 ) ;
#177319 = EDGE_CURVE ( 'NONE', #46947, #43590, #155074, .T. ) ;
#177318 = DIRECTION ( 'NONE',  ( -1.000000000000000000, 5.459311322609750190E-16, 0.000000000000000000 ) ) ;
#177317 = CARTESIAN_POINT ( 'NONE',  ( -7.497295758232712437, 11.69066945133944380, -0.7216878364870267237 ) ) ;
#177321 = CARTESIAN_POINT ( 'NONE',  ( -5.607179047703544583, 8.699403434699558346, 1.199719254218454489 ) ) ;
#177322 = LINE ( 'NONE', #61428, #168356 ) ;
#177324 = ORIENTED_EDGE ( 'NONE', *, *, #91508, .F. ) ;
#177323 = CARTESIAN_POINT ( 'NONE',  ( -5.113360211009450040, 5.994616996712990975, -1.199719254218453823 ) ) ;
#177325 = CARTESIAN_POINT ( 'NONE',  ( -7.822691444960700125, 11.10992853822074444, -1.082531754730543083 ) ) ;
#177326 = CARTESIAN_POINT ( 'NONE',  ( 1.800138458411651765, -0.7431416638853625134, 2.077998897882806784 ) ) ;
#177327 = CARTESIAN_POINT ( 'NONE',  ( -3.285556943749998737, -1.830208332855373987, 1.896917185911908499 ) ) ;
#177328 = CARTESIAN_POINT ( 'NONE',  ( 6.491066726104213203, 0.1889763263339637456, 1.952597990788194959 ) ) ;
#177329 = CARTESIAN_POINT ( 'NONE',  ( 0.6823417656249917140, 5.405208333674749177, 1.181850606188765695 ) ) ;
#177330 = CARTESIAN_POINT ( 'NONE',  ( 1.499999999999989120, 3.785416667349481123, 0.8660254037844524744 ) ) ;
#177331 = CARTESIAN_POINT ( 'NONE',  ( 6.050032868414796816, 6.056328681155354055, -0.4621489055621590403 ) ) ;
#177332 = CARTESIAN_POINT ( 'NONE',  ( 0.07479286986305369589, 1.387406912293275729, -2.112587013352088317 ) ) ;
#177333 = CARTESIAN_POINT ( 'NONE',  ( 5.085823778388903982, -1.827637283562512538, -0.2220107604927607503 ) ) ;
#177334 = ORIENTED_EDGE ( 'NONE', *, *, #80448, .T. ) ;
#177335 = CARTESIAN_POINT ( 'NONE',  ( -5.157946788997579689E-14, -0.2968749996585513529, 1.570758158831766060 ) ) ;
#177336 = ADVANCED_FACE ( 'NONE', ( #122688 ), #96230, .T. ) ;
#177337 = CARTESIAN_POINT ( 'NONE',  ( -8.857554428429624593, 9.228235009456373206, 0.7998128361456462443 ) ) ;
#177338 = CARTESIAN_POINT ( 'NONE',  ( -1.734723475976807094E-15, 3.553060279300227275, -11.95586206894163617 ) ) ;
#177339 = CARTESIAN_POINT ( 'NONE',  ( 11.89197816957260301, 11.29999999999999893, 0.8055420615339542456 ) ) ;
#177340 = CARTESIAN_POINT ( 'NONE',  ( 9.444970172009428566, 11.06549187246454125, 7.331777211066839328 ) ) ;
#177341 = CARTESIAN_POINT ( 'NONE',  ( 5.172599298813543633, 5.993452922492633839, -1.199719254218452047 ) ) ;
#177342 = CIRCLE ( 'NONE', #194642, 0.07999999999999951594 ) ;
#177343 = CARTESIAN_POINT ( 'NONE',  ( 6.063760116591036642, 2.031045510622536909, -0.3477994121598385613 ) ) ;
#177346 = CARTESIAN_POINT ( 'NONE',  ( 3.333393596924072444, 0.8250370302015205271, -1.646115572170883112 ) ) ;
#177345 = CARTESIAN_POINT ( 'NONE',  ( 1.802945237480069407, -1.574492340324705753, 0.9918895310334940874 ) ) ;
#177344 =( LENGTH_UNIT ( ) NAMED_UNIT ( * ) SI_UNIT ( .MILLI., .METRE. ) );
#177347 = CARTESIAN_POINT ( 'NONE',  ( 9.257519960032755790, 9.694861462993381807, 0.7998128361456462443 ) ) ;
#177348 = CARTESIAN_POINT ( 'NONE',  ( -8.789227347474932728, 15.51892067737951741, 8.182113819008643318 ) ) ;
#177349 = CARTESIAN_POINT ( 'NONE',  ( -7.119966945832006289, 8.335658187339330283, 1.199719254218452047 ) ) ;
#177351 = ORIENTED_EDGE ( 'NONE', *, *, #103483, .F. ) ;
#177350 = CARTESIAN_POINT ( 'NONE',  ( -10.08385610902500140, -7.605490242282780144, 0.4645879755154607160 ) ) ;
#177352 = CARTESIAN_POINT ( 'NONE',  ( 3.598431038176507002, -2.204323482753521635, -0.1086902067785888437 ) ) ;
#177353 = CARTESIAN_POINT ( 'NONE',  ( 6.063815651355930036, 2.230472738441360292, -0.3779872977145922741 ) ) ;
#177354 = CARTESIAN_POINT ( 'NONE',  ( -7.063434843039784639, 7.343021526408956667, 1.040834085586084257E-14 ) ) ;
#177355 = CARTESIAN_POINT ( 'NONE',  ( 5.572461477490294968, 0.7419763400571472989, 1.652881490725614189 ) ) ;
#177356 = CARTESIAN_POINT ( 'NONE',  ( 6.210162240821837543, 1.096913934394160517, -1.570407731631766390 ) ) ;
#177357 = CARTESIAN_POINT ( 'NONE',  ( 5.355107487717867265, 5.349972945200037522, 1.040834085586084257E-14 ) ) ;
#177358 = CARTESIAN_POINT ( 'NONE',  ( 6.192256348250350761, -1.861847689568534081, -0.1814220289034565448 ) ) ;
#177359 = CARTESIAN_POINT ( 'NONE',  ( 5.725241913846256914, 1.688569718951500986, 0.8975008795490190261 ) ) ;
#177360 = CARTESIAN_POINT ( 'NONE',  ( -0.7500000000000006661, 12.95833333333333570, -1.299038105676657340 ) ) ;
#177361 = EDGE_CURVE ( 'NONE', #179291, #213175, #65795, .T. ) ;
#177362 = CARTESIAN_POINT ( 'NONE',  ( 0.5142528298564854605, 1.293200884458247657, -1.351890787750304135 ) ) ;
#177363 = CARTESIAN_POINT ( 'NONE',  ( 1.675017921984035096, 1.752138005693338441, -0.9981273289914743829 ) ) ;
#177365 = CARTESIAN_POINT ( 'NONE',  ( 3.369845833479632180, 2.054674681345913800, -0.4616683548303905926 ) ) ;
#177364 = CARTESIAN_POINT ( 'NONE',  ( -8.130085669689073313, 12.63685038127928806, 0.7998128361456481317 ) ) ;
#177366 = CARTESIAN_POINT ( 'NONE',  ( 8.503988664269582998, 10.94440607977979063, 1.599625672291281386 ) ) ;
#177368 = CARTESIAN_POINT ( 'NONE',  ( -8.503988664269602538, 10.94440607977979063, 1.599625672291269396 ) ) ;
#177367 = CARTESIAN_POINT ( 'NONE',  ( 0.7499999999999867883, -0.6833333333333135862, -1.299038105676652899 ) ) ;
#177369 = CARTESIAN_POINT ( 'NONE',  ( 11.33772463945043718, 10.19999999999997264, 3.600000000000075140 ) ) ;
#177370 = CARTESIAN_POINT ( 'NONE',  ( 2.953383392634020943, -1.779389778202213446, 0.9557246442400985087 ) ) ;
#177371 = CARTESIAN_POINT ( 'NONE',  ( 0.6823417656249917140, 3.592708333674754506, 1.181850606188765695 ) ) ;
#177372 = CARTESIAN_POINT ( 'NONE',  ( 4.142179624174931796, 4.791296635414242111, 1.199719254218464037 ) ) ;
#177373 = CARTESIAN_POINT ( 'NONE',  ( 3.198656860129048152, -0.6241516536032962748, -2.069545307505623821 ) ) ;
#177374 = CARTESIAN_POINT ( 'NONE',  ( 8.039058738260216330, 8.343599714250547805, -0.7998128361456341429 ) ) ;
#177375 = CARTESIAN_POINT ( 'NONE',  ( -0.7499999999999972244, 4.608333333333352932, -1.299038105676652011 ) ) ;
#177377 = CARTESIAN_POINT ( 'NONE',  ( 0.000000000000000000, 6.002124920821316323, 0.000000000000000000 ) ) ;
#177376 = CARTESIAN_POINT ( 'NONE',  ( 7.693325821111733021, 7.940244644243982464, -0.7998128361456341429 ) ) ;
#177378 = CARTESIAN_POINT ( 'NONE',  ( 6.914295152845067349, 11.01050207838719075, 1.040834085586084257E-14 ) ) ;
#177380 = CARTESIAN_POINT ( 'NONE',  ( 7.191817663470090771, 15.44694763254654113, -9.557497708673340142 ) ) ;
#177379 = CARTESIAN_POINT ( 'NONE',  ( 1.117902646172004522, 0.4237721370383492059, -2.129260471988907000 ) ) ;
#177381 = CARTESIAN_POINT ( 'NONE',  ( -6.399085315970151733, 7.528316292462387871, -1.082531754730544860 ) ) ;
#177382 = CARTESIAN_POINT ( 'NONE',  ( 1.364683531249986537, 0.4052083336747511200, -0.7879004041258309554 ) ) ;
#177383 = CARTESIAN_POINT ( 'NONE',  ( 2.331793494658142230, 1.030094174309360344, -1.934364310732391345 ) ) ;
#177384 = CARTESIAN_POINT ( 'NONE',  ( 6.883263157960362477, -0.004191378316371896506, 2.053658919477070910 ) ) ;
#177385 = CARTESIAN_POINT ( 'NONE',  ( 2.835161494786802461, 0.2760463380651246856, 2.245541603805699005 ) ) ;
#177386 = CARTESIAN_POINT ( 'NONE',  ( -7.477485413136760073, 8.682486722536401302, -1.199719254218446718 ) ) ;
#177387 = CARTESIAN_POINT ( 'NONE',  ( -3.673896439178936824, 5.309298483840612093, 1.443375672974064550 ) ) ;
#177388 = CARTESIAN_POINT ( 'NONE',  ( 1.364683531249990311, 4.926041667008083991, 0.7879004041258500513 ) ) ;
#177389 = CARTESIAN_POINT ( 'NONE',  ( 5.825676364550436581, 7.207913871576331566, 1.168708750232345883 ) ) ;
#177390 = CARTESIAN_POINT ( 'NONE',  ( -1.500000000000008216, 12.24999999999999645, 3.469446951953614189E-15 ) ) ;
#177391 = CARTESIAN_POINT ( 'NONE',  ( 7.512626515748113576, 7.937354821227203594, 0.7216878364870267237 ) ) ;
#177392 = CARTESIAN_POINT ( 'NONE',  ( 4.112378888775404917, 1.252788995219549895, -1.250258383314418520 ) ) ;
#177393 = AXIS2_PLACEMENT_3D ( 'NONE', #152640, #202427, #181926 ) ;
#177394 = CARTESIAN_POINT ( 'NONE',  ( 7.899597058256738968, 12.36794700127490820, 1.040834085586084257E-14 ) ) ;
#177395 = CARTESIAN_POINT ( 'NONE',  ( 0.7804679756576750060, -1.169858290841051307, 1.750926281551241415 ) ) ;
#177396 = CONICAL_SURFACE ( 'NONE', #45996, 4.500000000000000000, 0.7853981633974491672 ) ;
#177397 = CARTESIAN_POINT ( 'NONE',  ( 1.364683531250000303, 9.505208333674735499, -0.7879004041258355073 ) ) ;
#177398 = CARTESIAN_POINT ( 'NONE',  ( -3.772911886352873445, 7.623757310712140800, 0.7998128361456352531 ) ) ;
#177399 = CARTESIAN_POINT ( 'NONE',  ( 5.941029844038744123, -1.730876725876070221, -1.034150010194856417 ) ) ;
#177400 = ORIENTED_EDGE ( 'NONE', *, *, #204911, .T. ) ;
#177401 = CARTESIAN_POINT ( 'NONE',  ( 10.07387183015377197, 11.71160420905630062, -1.199719254218440723 ) ) ;
#177402 = CARTESIAN_POINT ( 'NONE',  ( 3.344469905398726794, 0.4532862802011444203, 1.814783984445810905 ) ) ;
#177403 = CARTESIAN_POINT ( 'NONE',  ( 2.817306709214098870, -1.799057772339835548, -1.024303335033532658 ) ) ;
#177404 = CARTESIAN_POINT ( 'NONE',  ( -4.936577328707246082, 8.773440960218172435, 0.000000000000000000 ) ) ;
#177405 = CARTESIAN_POINT ( 'NONE',  ( 7.540305987494599016, 11.94877408538573427, -0.7998128361456291469 ) ) ;
#177406 = CARTESIAN_POINT ( 'NONE',  ( -8.469039510030723861, 13.03229652834454733, 1.040834085586084257E-14 ) ) ;
#177407 = CARTESIAN_POINT ( 'NONE',  ( -4.000799973277850974, 7.681462069183943697, 0.02035690600471253345 ) ) ;
#177408 = B_SPLINE_CURVE_WITH_KNOTS ( 'NONE', 3,
 ( #136411, #32495, #66022, #118076, #34618, #84439, #98569, #99629, #1027, #86576, #214393, #100688, #102831, #82299, #35681, #180873 ),
 .UNSPECIFIED., .F., .F.,
 ( 4, 2, 2, 2, 2, 2, 2, 4 ),
 ( 0.4818577711483807979, 0.5128210221889952791, 0.5283026477093025752, 0.5437842732296098713, 0.5592658987499171674, 0.5747475242702243525, 0.5902291497905316486, 0.6057107753108389447 ),
 .UNSPECIFIED. ) ;
#177409 = CARTESIAN_POINT ( 'NONE',  ( 6.368072262247213899, 1.106822706796772193, 1.856716078747308263 ) ) ;
#177410 = CARTESIAN_POINT ( 'NONE',  ( -1.402160292154681736E-14, -1.178124999658576311, 1.575800808251672791 ) ) ;
#177411 = CARTESIAN_POINT ( 'NONE',  ( 2.471086628630547288, 1.751123931924388089, 0.8847596551376719631 ) ) ;
#177412 = CARTESIAN_POINT ( 'NONE',  ( 1.475935241056694380, 1.776738309990203213, 0.9528675108748105860 ) ) ;
#177413 = CARTESIAN_POINT ( 'NONE',  ( -4.067937748088393590, 7.725456827083305278, 0.6547958487484796253 ) ) ;
#177415 = SURFACE_STYLE_USAGE ( .BOTH. , #197903 ) ;
#177414 = CARTESIAN_POINT ( 'NONE',  ( 6.598014311344812199, 10.84943379654430906, 1.040834085586084257E-14 ) ) ;
#177416 = CARTESIAN_POINT ( 'NONE',  ( 1.299835797595794151, -1.870726058509405210, -0.005653028302576856845 ) ) ;
#177417 = CARTESIAN_POINT ( 'NONE',  ( -1.201851678989727383E-14, 3.321875000341421025, 1.575800808251672791 ) ) ;
#177418 = CARTESIAN_POINT ( 'NONE',  ( 3.427992945418765203, -1.982693224445150060, 0.3483943456095982549 ) ) ;
#177420 = CARTESIAN_POINT ( 'NONE',  ( 1.898220681748989280, -1.001352587523595128, -1.865485677531570685 ) ) ;
#177419 = CARTESIAN_POINT ( 'NONE',  ( -6.751597309925468693, 6.979211071108916364, 0.7216878364870317197 ) ) ;
#177421 = CARTESIAN_POINT ( 'NONE',  ( -6.608673532018475960, 6.674816973635147477, -0.7998128361456361413 ) ) ;
#177422 = CARTESIAN_POINT ( 'NONE',  ( 4.211429588753928144, -1.719575573843846072, -1.152724658989822348 ) ) ;
#177423 = CARTESIAN_POINT ( 'NONE',  ( 5.671053392266061977, 9.838255734277600695, 0.7998128361456331437 ) ) ;
#177425 = CARTESIAN_POINT ( 'NONE',  ( 4.566398809704347528, 4.221886787610169556, -0.7998128361456211532 ) ) ;
#177424 = CARTESIAN_POINT ( 'NONE',  ( 6.439408583351804438, 0.8014019654560710082, -1.931139719275380084 ) ) ;
#177427 = ORIENTED_EDGE ( 'NONE', *, *, #207501, .F. ) ;
#177426 = CARTESIAN_POINT ( 'NONE',  ( 5.016531207907320322, 1.258010867292450152, -1.323153095230594989 ) ) ;
#177428 = CARTESIAN_POINT ( 'NONE',  ( 8.483651433849084711, 10.92067931095586886, 1.599625672291281386 ) ) ;
#177429 = CARTESIAN_POINT ( 'NONE',  ( 6.539320575229233157, 0.001224430076711413356, 2.103502572931112091 ) ) ;
#177431 = AXIS2_PLACEMENT_3D ( 'NONE', #124020, #189985, #157513 ) ;
#177430 = CARTESIAN_POINT ( 'NONE',  ( 10.91047834641517689, 10.31727674668477768, -5.055935782571435055 ) ) ;
#177432 = CARTESIAN_POINT ( 'NONE',  ( 5.930760676324510428, 2.125237774816424619, 0.5940772278362898007 ) ) ;
#177433 = CARTESIAN_POINT ( 'NONE',  ( -0.6823417656250003738, 11.71354166700806765, 1.181850606188754593 ) ) ;
#177434 = CARTESIAN_POINT ( 'NONE',  ( 5.004515039866801906, -1.898294113557968510, -0.2302225566794338651 ) ) ;
#177435 = CARTESIAN_POINT ( 'NONE',  ( -9.053093885623068715, 11.58502883802551153, -1.599625672291263179 ) ) ;
#177436 = CARTESIAN_POINT ( 'NONE',  ( 5.296431564432884542, 9.330920591813708143, 1.040834085586084257E-14 ) ) ;
#177437 = CARTESIAN_POINT ( 'NONE',  ( -11.91292854676703605, 11.11481529673016233, -1.446370920797322990 ) ) ;
#177438 = CARTESIAN_POINT ( 'NONE',  ( 4.989037339704528229, 4.922891105851139315, 1.040834085586084257E-14 ) ) ;
#177439 = CARTESIAN_POINT ( 'NONE',  ( 9.498564853506497485, -8.073984524010468178, -0.1796516426515351594 ) ) ;
#177440 = CARTESIAN_POINT ( 'NONE',  ( 3.635557746758808495, 7.393234471193928847, -0.7998128361456291469 ) ) ;
#177441 = ORIENTED_EDGE ( 'NONE', *, *, #142583, .T. ) ;
#177442 = ADVANCED_FACE ( 'NONE', ( #155118 ), #104234, .F. ) ;
#177443 = DIRECTION ( 'NONE',  ( 0.000000000000000000, 1.000000000000000000, 0.000000000000000000 ) ) ;
#177444 = CARTESIAN_POINT ( 'NONE',  ( 5.008994926481016741, 1.626754543590884561, 0.9232732976792233925 ) ) ;
#177445 = CARTESIAN_POINT ( 'NONE',  ( 1.337314304668908615E-15, -2.079999999999998295, -10.91999999999999105 ) ) ;
#177446 = CARTESIAN_POINT ( 'NONE',  ( 6.530187263637528439, 7.647581891445782709, -1.199719254218452047 ) ) ;
#177447 = CARTESIAN_POINT ( 'NONE',  ( -0.3869736770896817224, 1.794419290072776896, 11.79366332131313300 ) ) ;
#177448 = VECTOR ( 'NONE', #45910, 1000.000000000000114 ) ;
#177449 = CARTESIAN_POINT ( 'NONE',  ( -6.160225556963538018, 6.983552031129079296, 0.9223575212774417498 ) ) ;
#177450 = CARTESIAN_POINT ( 'NONE',  ( -5.260200412422196159, 9.080724881227137502, -0.7216878364870207285 ) ) ;
#177451 = CARTESIAN_POINT ( 'NONE',  ( 5.007038802148489509, 4.735966778795008381, 0.7998128361456341429 ) ) ;
#177452 = CARTESIAN_POINT ( 'NONE',  ( 1.287880319801449902, -1.245359047439015932, -1.525745898539744516 ) ) ;
#177453 = CARTESIAN_POINT ( 'NONE',  ( 3.339470413395662085, 0.4871825726840799398, -1.956567533273507964 ) ) ;
#177454 = CARTESIAN_POINT ( 'NONE',  ( -6.561256274009600986, 9.742217188731485678, -1.199719254218440723 ) ) ;
#177455 = CARTESIAN_POINT ( 'NONE',  ( 4.420840606507738357, 7.315341919971147355, 1.199719254218451159 ) ) ;
#177456 = CARTESIAN_POINT ( 'NONE',  ( 6.827182134110235445, 7.051404648315344303, 2.887205390314013354 ) ) ;
#177457 = CARTESIAN_POINT ( 'NONE',  ( 3.486445073788289051, -0.4274320362823453290, -2.149191018322317515 ) ) ;
#177458 = CARTESIAN_POINT ( 'NONE',  ( -5.575940895411126697, 5.849477901847593309, -0.6286834815852658798 ) ) ;
#177459 = CARTESIAN_POINT ( 'NONE',  ( 1.993070439633041424, 1.677129747370089019, -0.9476047394562473469 ) ) ;
#177460 = CARTESIAN_POINT ( 'NONE',  ( -9.972185678051314284, 11.59297036493672017, 1.199719254218462483 ) ) ;
#177461 = CARTESIAN_POINT ( 'NONE',  ( 0.1331565106231363538, 0.2470099659030860484, -1.980838409567912572 ) ) ;
#177462 = CARTESIAN_POINT ( 'NONE',  ( -9.587917471435847716, 4.026361754648488223, -6.670783315233271615 ) ) ;
#177463 = CARTESIAN_POINT ( 'NONE',  ( 8.444030743212801227, 8.745790710036752458, 0.7998128361456462443 ) ) ;
#177464 = EDGE_CURVE ( 'NONE', #125996, #189127, #67176, .T. ) ;
#177465 = CIRCLE ( 'NONE', #180863, 11.09999999999999964 ) ;
#177466 = CARTESIAN_POINT ( 'NONE',  ( 6.823831386379729302, 6.855558127064808716, -0.7998128361456281477 ) ) ;
#177467 = CARTESIAN_POINT ( 'NONE',  ( -2.030969412800708085, 8.463209591662408826, -2.499999999999995115 ) ) ;
#177468 = CARTESIAN_POINT ( 'NONE',  ( 6.048345925472191631, 6.229027465905275562, 0.7216878364870328300 ) ) ;
#177469 = ORIENTED_EDGE ( 'NONE', *, *, #204783, .F. ) ;
#177471 = CARTESIAN_POINT ( 'NONE',  ( 1.594390828295478402, -1.075120693119306692, 1.701777395020438899 ) ) ;
#177470 = CARTESIAN_POINT ( 'NONE',  ( 5.442854017605395889, -1.455216020186438364, -1.127989967910733915 ) ) ;
#177472 = CARTESIAN_POINT ( 'NONE',  ( 4.692867332335362462, -1.408920786844407802, -1.815866644984363232 ) ) ;
#177474 = CARTESIAN_POINT ( 'NONE',  ( 2.236936919162732629, -0.08530413586980757634, -1.859100468073461965 ) ) ;
#177473 = CARTESIAN_POINT ( 'NONE',  ( -0.1290005225502433017, 0.6921039065478848951, -2.255494067288220439 ) ) ;
#177475 = CARTESIAN_POINT ( 'NONE',  ( 3.285556943750000070, -2.384374999522043126, 0.000000000000000000 ) ) ;
#177476 = CARTESIAN_POINT ( 'NONE',  ( 5.959226163113887864, -1.611951592244726950, 1.028742869173946861 ) ) ;
#177477 = CARTESIAN_POINT ( 'NONE',  ( -6.659026002606323047, 10.92061410301605662, 0.000000000000000000 ) ) ;
#177478 = CARTESIAN_POINT ( 'NONE',  ( -4.163762573172648196, 7.871823745427799501, 0.000000000000000000 ) ) ;
#177480 = CARTESIAN_POINT ( 'NONE',  ( 3.045614982896325262, 0.6747646648952825288, -1.744891315567910439 ) ) ;
#177479 = CARTESIAN_POINT ( 'NONE',  ( 4.687105897418362588, 1.550225779131916726, 1.403071992899749931 ) ) ;
#177481 = CARTESIAN_POINT ( 'NONE',  ( 6.236387472606139681, 8.298871356172400127, -1.443375672974057666 ) ) ;
#177482 = AXIS2_PLACEMENT_3D ( 'NONE', #32052, #146897, #64551 ) ;
#177483 = CARTESIAN_POINT ( 'NONE',  ( 1.734723475976807094E-15, -3.469446951953614189E-15, 0.2971265334020881110 ) ) ;
#177484 = LINE ( 'NONE', #63720, #51406 ) ;
#177485 = CARTESIAN_POINT ( 'NONE',  ( 5.338411986983877533, 1.700291985010034201, 0.2892061366746317419 ) ) ;
#177486 = CARTESIAN_POINT ( 'NONE',  ( -4.564291269294938225, 8.476756914152748124, 1.040834085586084257E-14 ) ) ;
#177487 = CARTESIAN_POINT ( 'NONE',  ( 0.9669347054478127923, -1.691490974053434959, -0.3813910478582624441 ) ) ;
#177488 = DIRECTION ( 'NONE',  ( 0.000000000000000000, 0.000000000000000000, 1.000000000000000000 ) ) ;
#177489 = CARTESIAN_POINT ( 'NONE',  ( -1.734723475976807094E-15, 2.999999999999988898, -6.938893903907228378E-15 ) ) ;
#177490 = CARTESIAN_POINT ( 'NONE',  ( 6.298064597363540074, -0.9548514761729166578, -1.776169100128288658 ) ) ;
#177491 = CARTESIAN_POINT ( 'NONE',  ( 3.563261906135761770, 6.332667919118538435, 2.500000000000011102 ) ) ;
#177492 = CARTESIAN_POINT ( 'NONE',  ( 5.612245307067635025, 2.168910047263863827, -0.09915484274719725544 ) ) ;
#177493 = CARTESIAN_POINT ( 'NONE',  ( 4.248545464119923842, 0.4890907236730773766, 1.758887239191930796 ) ) ;
#177494 = CARTESIAN_POINT ( 'NONE',  ( 2.289831844592318255, -1.277571413231039399, -1.488851726829775846 ) ) ;
#177495 = CARTESIAN_POINT ( 'NONE',  ( 6.438674896094000566, -1.635394517905249145, 1.344423162301669361 ) ) ;
#177496 = CARTESIAN_POINT ( 'NONE',  ( 9.423306279978271860, 13.09470160913627090, -7.356095995331378923 ) ) ;
#177497 = CARTESIAN_POINT ( 'NONE',  ( 4.001749955438753226, 7.811071542261023737, 0.1299566359906061952 ) ) ;
#177498 = CARTESIAN_POINT ( 'NONE',  ( 8.046927864910717432, 9.346836249606042202, 1.199719254218462483 ) ) ;
#177499 = CARTESIAN_POINT ( 'NONE',  ( 2.649219347560148208, 0.2619616101627724736, 2.104190563435456518 ) ) ;
#177500 = CARTESIAN_POINT ( 'NONE',  ( -3.090895834235680262, 5.589500325708124606, 1.082531754730560403 ) ) ;
#177501 =( LENGTH_UNIT ( ) NAMED_UNIT ( * ) SI_UNIT ( .MILLI., .METRE. ) );
#177502 = CARTESIAN_POINT ( 'NONE',  ( -5.430810130430261395, 6.303639405459422917, -1.045180951442852946 ) ) ;
#177503 = CARTESIAN_POINT ( 'NONE',  ( 1.024380955673375393, 1.017105081308821379, 1.803069775380027995 ) ) ;
#177505 = CARTESIAN_POINT ( 'NONE',  ( -0.7500000000000006661, 13.23958333401613352, -1.299038105676657340 ) ) ;
#177504 = CARTESIAN_POINT ( 'NONE',  ( -10.77520153956138138, 4.485527145162882867, 5.284729349356103612 ) ) ;
#177507 = ORIENTED_EDGE ( 'NONE', *, *, #38304, .T. ) ;
#177506 = CARTESIAN_POINT ( 'NONE',  ( 2.825082509308895151, 1.607285200359307886, -1.533455307168646975 ) ) ;
#177508 = CARTESIAN_POINT ( 'NONE',  ( 0.3351808223112633933, 0.7127874033420987798, -2.185478155228081754 ) ) ;
#177510 = CARTESIAN_POINT ( 'NONE',  ( 5.946154108440814490, -0.9325515945646453142, 1.839819606017919718 ) ) ;
#177509 = CARTESIAN_POINT ( 'NONE',  ( 3.440018289565364817, 5.036440642624797626, 1.599625672291267398 ) ) ;
#177512 = CARTESIAN_POINT ( 'NONE',  ( -3.474999999999998312, -2.420833333333334725, 2.006292185433951047 ) ) ;
#177511 = CARTESIAN_POINT ( 'NONE',  ( 6.378184920586140727, 6.405913593630768510, 0.000000000000000000 ) ) ;
#177513 = CARTESIAN_POINT ( 'NONE',  ( 0.1329588055935396196, 0.006246367379872731426, -1.846049620084761367 ) ) ;
#177514 = CARTESIAN_POINT ( 'NONE',  ( 5.056134578334451568, -1.329838508726857382, 1.273713382018211382 ) ) ;
#177515 = CARTESIAN_POINT ( 'NONE',  ( 3.704402285031850539, 5.344888637335695414, -1.599625672291262513 ) ) ;
#177516 = CARTESIAN_POINT ( 'NONE',  ( -0.2104748580754201015, 5.720428293583295520, -2.697747842008205943 ) ) ;
#177517 = CARTESIAN_POINT ( 'NONE',  ( 3.205755162861756435, -1.722880287277430478, 0.08319854473674663520 ) ) ;
#177518 = CARTESIAN_POINT ( 'NONE',  ( 1.393767942625488532, -2.000731169080074423, 0.2516357431460446992 ) ) ;
#177519 = CARTESIAN_POINT ( 'NONE',  ( 2.813438166105670657, 1.274540910030600216, -1.912834453734891804 ) ) ;
#177520 = CARTESIAN_POINT ( 'NONE',  ( -0.6823417656250212460, 4.113541667008085767, 1.181850606188767472 ) ) ;
#177521 = CARTESIAN_POINT ( 'NONE',  ( 2.513255990918183524, 2.019876067157271748, 1.019300669498679479 ) ) ;
#177522 = CARTESIAN_POINT ( 'NONE',  ( 5.373694187740483130, 2.029982003570539817, -0.5606972681787207868 ) ) ;
#177523 = CARTESIAN_POINT ( 'NONE',  ( -3.298376509874564988, 7.070132704820777825, 0.000000000000000000 ) ) ;
#177524 = CARTESIAN_POINT ( 'NONE',  ( 3.602599932655100812, 1.396742099285839256, -1.086680525292152977 ) ) ;
#177525 = CARTESIAN_POINT ( 'NONE',  ( 4.788000803920411386, 8.737751371215816576, 1.040834085586084257E-14 ) ) ;
#177527 = CARTESIAN_POINT ( 'NONE',  ( 0.2524361811976470471, 0.8832210619409311958, 2.115471854006613750 ) ) ;
#177526 = CARTESIAN_POINT ( 'NONE',  ( 5.383996397958233260, 5.453953017138946535, -0.7216878364870458196 ) ) ;
#177528 = CARTESIAN_POINT ( 'NONE',  ( 4.154132678086497776, -1.362845063541193946, 1.238102162693654584 ) ) ;
#177529 = CARTESIAN_POINT ( 'NONE',  ( -4.599240423533815125, 6.388866465587984322, 1.599625672291267398 ) ) ;
#177530 = CARTESIAN_POINT ( 'NONE',  ( 4.487385655998867406, 8.179107665399927285, 0.7216878364870438212 ) ) ;
#177531 = CARTESIAN_POINT ( 'NONE',  ( 1.499999999999987121, 3.295833333333354709, -0.8660254037844262731 ) ) ;
#177532 = CARTESIAN_POINT ( 'NONE',  ( 2.514065211524143084, -0.6609878990531635745, 2.015050547854141172 ) ) ;
#177533 = CARTESIAN_POINT ( 'NONE',  ( 4.295009486468337023, 1.759388067201245187, 1.306329983072423984 ) ) ;
#177534 = CARTESIAN_POINT ( 'NONE',  ( -4.731959306369413198, 5.479372931307791461, -1.199719254218446718 ) ) ;
#177535 = DIRECTION ( 'NONE',  ( 0.000000000000000000, -0.7999999999999973799, -0.6000000000000034195 ) ) ;
#177536 = CARTESIAN_POINT ( 'NONE',  ( 0.4642244361878632430, -7.321523296574938833, 10.36809559534897929 ) ) ;
#177537 = CIRCLE ( 'NONE', #46138, 11.09999999999999964 ) ;
#177538 = CARTESIAN_POINT ( 'NONE',  ( -1.364683531250012516, 3.988541667008088876, -0.7879004041258300672 ) ) ;
#177539 = CARTESIAN_POINT ( 'NONE',  ( 3.070836455255634423, -1.780209531678895729, -0.7368423699729318432 ) ) ;
#177540 = CARTESIAN_POINT ( 'NONE',  ( -0.6823417656250003738, 8.651041667008065872, 1.181850606188754593 ) ) ;
#177541 = CARTESIAN_POINT ( 'NONE',  ( -3.795919822146289313, 5.451659097302528068, -1.443375672974053447 ) ) ;
#177542 = CARTESIAN_POINT ( 'NONE',  ( 0.2467152807458715680, 1.134915856054707906, -1.909484979926486137 ) ) ;
#177543 = CARTESIAN_POINT ( 'NONE',  ( -5.099275172515603138, 8.002885897026576600, 1.082531754730549967 ) ) ;
#177544 = EDGE_LOOP ( 'NONE', ( #97748, #127156, #181395, #42537 ) ) ;
#177547 = VECTOR ( 'NONE', #54800, 1000.000000000000000 ) ;
#177546 = CARTESIAN_POINT ( 'NONE',  ( -1.850000000000000089, 2.265195232789710231E-16, 0.5999999999999969802 ) ) ;
#177545 = CARTESIAN_POINT ( 'NONE',  ( -3.675669043080673770, 7.302381293653823491, 0.000000000000000000 ) ) ;
#177548 = CARTESIAN_POINT ( 'NONE',  ( 5.138703914779377158, 5.953908307786102583, 1.199719254218462483 ) ) ;
#177549 = CARTESIAN_POINT ( 'NONE',  ( 4.760321332173959696, 4.726332107057286791, 0.000000000000000000 ) ) ;
#177550 = CARTESIAN_POINT ( 'NONE',  ( 11.01135777277262306, 10.90000000000000036, -1.400000000000001910 ) ) ;
#177551 = DIRECTION ( 'NONE',  ( 0.000000000000000000, 1.000000000000000000, 0.000000000000000000 ) ) ;
#177552 = CARTESIAN_POINT ( 'NONE',  ( 2.173056921186319546, 1.071630648972416333, 1.371277206274525096 ) ) ;
#177553 = CARTESIAN_POINT ( 'NONE',  ( -4.459788646379888810, 7.974764203887369618, -0.6295236818997522743 ) ) ;
#177554 = CARTESIAN_POINT ( 'NONE',  ( 0.4495626703563437299, 1.451167377975391304, 1.320406988977901985 ) ) ;
#177555 = CARTESIAN_POINT ( 'NONE',  ( -1.201851678989727383E-14, 1.634375000341421025, 1.575800808251672791 ) ) ;
#177556 = CARTESIAN_POINT ( 'NONE',  ( 5.911032513020411550, 1.904272706209766630, 1.023102869888978583 ) ) ;
#177557 = CARTESIAN_POINT ( 'NONE',  ( -9.809487834687324437, 11.40315621434539395, 1.199719254218462483 ) ) ;
#177558 = CARTESIAN_POINT ( 'NONE',  ( -5.327991180046197428, 8.199444895820425572, 1.082531754730548412 ) ) ;
#177559 = CARTESIAN_POINT ( 'NONE',  ( 5.911032513020411550, 1.904272706209766630, 1.023102869888978583 ) ) ;
#177561 = ORIENTED_EDGE ( 'NONE', *, *, #123084, .T. ) ;
#177560 = CARTESIAN_POINT ( 'NONE',  ( -8.966186108929056431, 2.441452740530747789, -7.552575952455633512 ) ) ;
#177562 = CARTESIAN_POINT ( 'NONE',  ( 1.364683531249988535, 4.655208333674755394, -0.7879004041258300672 ) ) ;
#177563 = CARTESIAN_POINT ( 'NONE',  ( 0.7548939078372005618, -1.576849831105286537, -1.005952255950369301 ) ) ;
#177564 = CARTESIAN_POINT ( 'NONE',  ( 6.591143254762334536, 0.9945565086073978600, -1.419977980273220863 ) ) ;
#177566 = CARTESIAN_POINT ( 'NONE',  ( 3.122796855005858241, 0.05607861761174406934, 2.191015320347329709 ) ) ;
#177565 = CARTESIAN_POINT ( 'NONE',  ( -0.6801582343750334214, 0.1822916670080609869, 1.178068619123799898 ) ) ;
#177567 = CARTESIAN_POINT ( 'NONE',  ( 3.645846906810937149, -1.745625206895658810, -1.509303248858377966 ) ) ;
#177568 = CARTESIAN_POINT ( 'NONE',  ( 5.835248319207797074, -1.864956875241881251, 0.8770506743334179900 ) ) ;
#177569 = CARTESIAN_POINT ( 'NONE',  ( 0.7615419678954943317, 0.9566914028362738520, 1.689878795569139891 ) ) ;
#177570 = CARTESIAN_POINT ( 'NONE',  ( -7.334597914868743018, 7.659378443542744996, -0.7216878364870267237 ) ) ;
#177571 = CARTESIAN_POINT ( 'NONE',  ( 2.275391796764376640, 5.643962577969389827, -0.5307291018262025872 ) ) ;
#177572 = CARTESIAN_POINT ( 'NONE',  ( -9.404204976007665806, 14.49017091736342167, 7.453969464079248652 ) ) ;
#177573 = CARTESIAN_POINT ( 'NONE',  ( 3.709332143218791789, 1.789599998243587731, -1.137392358348317201 ) ) ;
#177574 = CARTESIAN_POINT ( 'NONE',  ( -1.423015351387224570E-15, 0.9706168436483886275, 11.90408086427858336 ) ) ;
#177575 = CARTESIAN_POINT ( 'NONE',  ( 2.391250195717840477, -0.7743161457766101208, -1.862016636315230844 ) ) ;
#177576 = CARTESIAN_POINT ( 'NONE',  ( -6.683806541412780078, 6.900121841177441873, -0.7216878364870267237 ) ) ;
#177577 = CARTESIAN_POINT ( 'NONE',  ( 6.211994372536747022, -2.190858219723303080, 0.2640275128017176565 ) ) ;
#177578 = LINE ( 'NONE', #212179, #212063 ) ;
#177579 = CARTESIAN_POINT ( 'NONE',  ( -3.315919823527478716, -3.091870070317458197, -0.8826684162155652436 ) ) ;
#177580 = CARTESIAN_POINT ( 'NONE',  ( -1.249999999999998890, 1.530808498934190585E-16, -6.123233995736774664E-17 ) ) ;
#177581 = CARTESIAN_POINT ( 'NONE',  ( -5.912237504011027767, 9.055304967058290799, 1.199719254218454489 ) ) ;
#177583 = CARTESIAN_POINT ( 'NONE',  ( 6.825078400183518745, 4.686743419949856104, 2.806861564458093650 ) ) ;
#177582 = CARTESIAN_POINT ( 'NONE',  ( -4.785410049391000342, 8.260660143818395085, 0.8633373473483215710 ) ) ;
#177584 = CARTESIAN_POINT ( 'NONE',  ( 1.580223361175657981, 8.746992034114501990, -2.465615386491380789 ) ) ;
#177585 = ORIENTED_EDGE ( 'NONE', *, *, #90081, .F. ) ;
#177586 = CARTESIAN_POINT ( 'NONE',  ( 4.188392892783887156, -2.038203232304033108, -0.3041262925047826249 ) ) ;
#177587 = CARTESIAN_POINT ( 'NONE',  ( -1.360316468749997565, 2.890625000341401574, 1.734723475976807094E-15 ) ) ;
#177588 = EDGE_CURVE ( 'NONE', #205644, #146356, #89679, .T. ) ;
#177589 = CARTESIAN_POINT ( 'NONE',  ( -3.686287386450715076E-15, -7.473374494045017968, 9.579665964948883783 ) ) ;
#177590 = CARTESIAN_POINT ( 'NONE',  ( -4.578903193113314174, 6.365139696764064325, 1.599625672291267398 ) ) ;
#177592 = CARTESIAN_POINT ( 'NONE',  ( -5.354544322754380303, 5.211666229493680191, 0.7998128361456281477 ) ) ;
#177591 = B_SPLINE_CURVE_WITH_KNOTS ( 'NONE', 3,
 ( #32004, #147892, #213908, #197679, #194493, #111184 ),
 .UNSPECIFIED., .F., .F.,
 ( 4, 2, 4 ),
 ( 0.000000000000000000, 0.0003141553954499744596, 0.0006283107908999489193 ),
 .UNSPECIFIED. ) ;
#177593 = CARTESIAN_POINT ( 'NONE',  ( 4.037763967290787903, -1.932009543340426072, 0.5885129382087511685 ) ) ;
#177594 = CARTESIAN_POINT ( 'NONE',  ( -1.402160292154681736E-14, 1.087500000000024336, -1.732050807568863648 ) ) ;
#177596 = CARTESIAN_POINT ( 'NONE',  ( 9.463228032658635769, 11.10314946193233965, -1.082531754730543083 ) ) ;
#177595 = CARTESIAN_POINT ( 'NONE',  ( -4.359828915246279024, 7.244161613499399799, -1.199719254218455378 ) ) ;
#177597 = CARTESIAN_POINT ( 'NONE',  ( 6.795661308947685164, 8.951357498570873261, -1.599625672291262513 ) ) ;
#177598 = CARTESIAN_POINT ( 'NONE',  ( 2.817317228389113470, -0.2032538945386449802, 2.050847873933867138 ) ) ;
#177599 = CARTESIAN_POINT ( 'NONE',  ( 2.988907892087853124, -2.013985899409028946, 0.1017507309580278629 ) ) ;
#177600 = ORIENTED_EDGE ( 'NONE', *, *, #19150, .F. ) ;
#177601 = CARTESIAN_POINT ( 'NONE',  ( -10.50000000000000000, 12.69999999999998153, 3.599999999999999201 ) ) ;
#177602 = CARTESIAN_POINT ( 'NONE',  ( 3.408985558832261731, 6.064568021024562938, 1.199719254218462483 ) ) ;
#177604 = ORIENTED_EDGE ( 'NONE', *, *, #167881, .F. ) ;
#177603 = LINE ( 'NONE', #76881, #139802 ) ;
#177605 = CARTESIAN_POINT ( 'NONE',  ( 3.427111092251767133, 0.9039706872599994059, 1.802141633730186543 ) ) ;
#177606 = CARTESIAN_POINT ( 'NONE',  ( 2.536835285771392279, -1.364265644482412609, -1.236541980112846550 ) ) ;
#177607 = CARTESIAN_POINT ( 'NONE',  ( 6.252570086353132162, 0.6882034672392455255, 2.096894461246688213 ) ) ;
#177608 = CARTESIAN_POINT ( 'NONE',  ( 5.061990249855835344, 6.999017606288844284, -1.599625672291273171 ) ) ;
#177609 = CARTESIAN_POINT ( 'NONE',  ( 2.196749789412206333, -0.5742421066207163971, -2.083876772215712325 ) ) ;
#177610 = CARTESIAN_POINT ( 'NONE',  ( -6.925517538482230506, 6.974191971184389160, 0.7998128361456341429 ) ) ;
#177611 = CARTESIAN_POINT ( 'NONE',  ( 5.085217855557687905, 1.732777129288827656, 1.216576597717359931 ) ) ;
#177612 = CARTESIAN_POINT ( 'NONE',  ( 2.882471369727876542, -0.2278316040762885242, 2.287086785078895179 ) ) ;
#177613 = ORIENTED_EDGE ( 'NONE', *, *, #107860, .T. ) ;
#177614 = CARTESIAN_POINT ( 'NONE',  ( 5.951324661305081420, 4.742844146917974513, -2.438848701830601318 ) ) ;
#177615 = CIRCLE ( 'NONE', #205252, 1.872309607372811158 ) ;
#177616 = CARTESIAN_POINT ( 'NONE',  ( 1.234984068473435892, -1.692697435815498919, 0.7966027930108383615 ) ) ;
#177617 = AXIS2_PLACEMENT_3D ( 'NONE', #108566, #105323, #55482 ) ;
#177618 = ADVANCED_FACE ( 'NONE', ( #202762 ), #90914, .T. ) ;
#177619 = CARTESIAN_POINT ( 'NONE',  ( 5.155133900154169169, -1.665016652684460530, -1.055383500247959461 ) ) ;
#177621 = CARTESIAN_POINT ( 'NONE',  ( 7.226132685959389512, 11.37431253368722750, -0.7216878364870267237 ) ) ;
#177620 = CARTESIAN_POINT ( 'NONE',  ( -1.364683531249997417, 3.509375000341423245, 1.214306433183764966E-14 ) ) ;
#177623 = CARTESIAN_POINT ( 'NONE',  ( 0.4873205249028254027, -0.2742316277877173691, -2.189713876267186166 ) ) ;
#177622 = CARTESIAN_POINT ( 'NONE',  ( -7.888146445052511169, 8.097259028849730811, 1.040834085586084257E-14 ) ) ;
#177624 = CIRCLE ( 'NONE', #35816, 0.04999999999999991257 ) ;
#177625 = CARTESIAN_POINT ( 'NONE',  ( 6.039524589772497620, 1.914416561877980261, -0.7887839105886890190 ) ) ;
#177626 = CARTESIAN_POINT ( 'NONE',  ( 6.830610463186557624, 6.863467050006115677, 1.040834085586084257E-14 ) ) ;
#177627 = CARTESIAN_POINT ( 'NONE',  ( -7.074657228232555717, 7.148188275893099686, 1.040834085586084257E-14 ) ) ;
#177628 = CARTESIAN_POINT ( 'NONE',  ( 6.639320575229255894, 6.035237531390704291, 2.698156163645454964 ) ) ;
#177629 = CARTESIAN_POINT ( 'NONE',  ( 5.348493512783888626, 0.5714336785274246600, 1.886844506308351210 ) ) ;
#177630 = CARTESIAN_POINT ( 'NONE',  ( -0.03470293633787284449, -1.699275230904277789, 1.268407768021381221 ) ) ;
#177631 = CARTESIAN_POINT ( 'NONE',  ( 0.7499999999999885647, 0.5979166673494851203, -1.299038105676652899 ) ) ;
#177632 = CARTESIAN_POINT ( 'NONE',  ( 4.635575047956096206, -2.111140572116900316, 0.9323621513206108435 ) ) ;
#177633 = CARTESIAN_POINT ( 'NONE',  ( 2.430602512062591369, -1.272252061732727091, 1.623331442124707591 ) ) ;
#177634 = CARTESIAN_POINT ( 'NONE',  ( 6.643132081016111634, 9.733775946952057723, 1.082531754730558626 ) ) ;
#177636 = CARTESIAN_POINT ( 'NONE',  ( 6.204791576909545192, 7.267953590263130259, -1.199719254218452047 ) ) ;
#177635 = AXIS2_PLACEMENT_3D ( 'NONE', #89772, #107123, #204529 ) ;
#177637 = CARTESIAN_POINT ( 'NONE',  ( 3.386504508363381571, 7.172948703057747011, -0.7998128361456362523 ) ) ;
#177638 = CARTESIAN_POINT ( 'NONE',  ( -1.364683531250014514, 2.051041667008086655, -0.7879004041258289570 ) ) ;
#177639 = CARTESIAN_POINT ( 'NONE',  ( 4.577813143269636065, 5.369812084349879555, -1.199719254218450271 ) ) ;
#177640 = CARTESIAN_POINT ( 'NONE',  ( 5.788968402910805722, 7.776882441527838807, 1.443375672974062551 ) ) ;
#177641 = CARTESIAN_POINT ( 'NONE',  ( 4.545498338918555703, 1.941281163200560878, -0.9724488383844475115 ) ) ;
#177643 = CARTESIAN_POINT ( 'NONE',  ( 4.335397732480402055, 0.7831895168094182846, -1.666506522714307437 ) ) ;
#177642 = CARTESIAN_POINT ( 'NONE',  ( -3.307826292054316664, 4.882216645528547616, -1.443375672974059665 ) ) ;
#177644 = CARTESIAN_POINT ( 'NONE',  ( 6.720655732516681802, 2.481091636469245021, 2.111593894264688132 ) ) ;
#177645 = CARTESIAN_POINT ( 'NONE',  ( 5.232042516939362287, 2.159042084939459816, 0.3751777721049884273 ) ) ;
#177646 = CARTESIAN_POINT ( 'NONE',  ( 8.283668668269706714, 8.766627655843896250, 1.040834085586084257E-14 ) ) ;
#177647 = CARTESIAN_POINT ( 'NONE',  ( 5.682586732044571320, -2.206005490488979426, -0.5019008842952320526 ) ) ;
#177648 = ORIENTED_EDGE ( 'NONE', *, *, #150402, .F. ) ;
#177649 = CARTESIAN_POINT ( 'NONE',  ( -4.103765016252827635, 7.679818082383993882, -0.7602138238151506799 ) ) ;
#177650 = CARTESIAN_POINT ( 'NONE',  ( 4.930145672075521013, 8.107674077938057167, 1.051636801887654293 ) ) ;
#177651 = CARTESIAN_POINT ( 'NONE',  ( -5.763624699140883934, 6.857221916153382502, -1.082531754730549967 ) ) ;
#177652 = CARTESIAN_POINT ( 'NONE',  ( 4.312902262922978736, 5.164712407232485702, -1.082531754730548412 ) ) ;
#177653 =( BOUNDED_CURVE ( )  B_SPLINE_CURVE ( 2, ( #85798, #151877, #3452, #119430, #185417, #136696, #169177 ),
 .UNSPECIFIED., .F., .T. ) 
 B_SPLINE_CURVE_WITH_KNOTS ( ( 3, 2, 2, 3 ),
 ( 0.4249999999999999334, 0.4333333333333332926, 0.4416666666666665964, 0.4499999999999999556 ),
 .UNSPECIFIED. ) 
 CURVE ( )  GEOMETRIC_REPRESENTATION_ITEM ( )  RATIONAL_B_SPLINE_CURVE ( ( 1.000000000000000888, 0.8660254037844378194, 1.000000000000000000, 0.8660254037844387076, 1.000000000000000000, 0.8660254037844395958, 0.9999999999999991118 ) ) 
 REPRESENTATION_ITEM ( '' )  );
#177654 = CARTESIAN_POINT ( 'NONE',  ( 0.9535335928906017999, 1.768114364327963539, -0.08115213312524624523 ) ) ;
#177655 = CARTESIAN_POINT ( 'NONE',  ( 4.776043607066285723, 1.990852085817075068, -0.2977186459587366496 ) ) ;
#177656 = CARTESIAN_POINT ( 'NONE',  ( 5.632522751473472589, 8.658694745772667289, -1.199719254218440723 ) ) ;
#177657 = CARTESIAN_POINT ( 'NONE',  ( 3.997179113411051254, 1.780275165862042153, -1.124711807175354350 ) ) ;
#177658 = CARTESIAN_POINT ( 'NONE',  ( 2.425271589312021359, -1.421058436811825754, -1.284788359014801706 ) ) ;
#177659 = CARTESIAN_POINT ( 'NONE',  ( 3.928111819657337911, 5.605883094398769195, 1.599625672291267398 ) ) ;
#177660 = CARTESIAN_POINT ( 'NONE',  ( 3.455474441396837904, 1.550956523109302543, 1.213803446622195636 ) ) ;
#177661 = CARTESIAN_POINT ( 'NONE',  ( 5.097918204798724595, 1.359643563815411405, 1.493766824747685185 ) ) ;
#177662 = CARTESIAN_POINT ( 'NONE',  ( 1.832664747978371533, 0.1804508633567840359, 1.861920966532565336 ) ) ;
#177665 = ORIENTED_EDGE ( 'NONE', *, *, #156430, .F. ) ;
#177664 = CARTESIAN_POINT ( 'NONE',  ( 1.705181254219298115, 1.662258477346746588, -0.9455041445245655485 ) ) ;
#177663 = CARTESIAN_POINT ( 'NONE',  ( 5.074679841287068172, -1.625846828454122983, -0.5764380256386961721 ) ) ;
#177667 = CARTESIAN_POINT ( 'NONE',  ( 4.365362273920244007, 6.116008624372160973, 1.443375672974062551 ) ) ;
#177666 = CARTESIAN_POINT ( 'NONE',  ( 0.9091299924109221831, 1.668792687453458878, -1.444214864661397035 ) ) ;
#177668 = CARTESIAN_POINT ( 'NONE',  ( -1.201851678989727383E-14, 2.384375000341416584, 1.575800808251672791 ) ) ;
#177669 = CARTESIAN_POINT ( 'NONE',  ( 7.889955328148847258, 11.29236608522730911, -1.199719254218446718 ) ) ;
#177670 = CARTESIAN_POINT ( 'NONE',  ( -5.608349667956210816, 5.604589570211684801, -0.4131542205010517166 ) ) ;
#177671 = DIRECTION ( 'NONE',  ( 1.224646799147355426E-16, 0.000000000000000000, -1.000000000000000000 ) ) ;
#177672 = CARTESIAN_POINT ( 'NONE',  ( 0.4849360239999983557, 1.980737741294085419, 0.6024896509310638804 ) ) ;
#177673 = CARTESIAN_POINT ( 'NONE',  ( 1.499999999999987121, 1.754166666666691521, 0.8660254037844524744 ) ) ;
#177674 = CARTESIAN_POINT ( 'NONE',  ( 6.810273232766058449, 6.839740281182199233, 1.040834085586084257E-14 ) ) ;
#177675 = CARTESIAN_POINT ( 'NONE',  ( -7.725448601688521322, 7.907444878258402809, 1.040834085586084257E-14 ) ) ;
#177676 = CARTESIAN_POINT ( 'NONE',  ( 5.204350862799327793, 7.165104988056252289, -1.599625672291281386 ) ) ;
#177677 = CARTESIAN_POINT ( 'NONE',  ( 6.375647721065083928, 0.3630326626483972308, -2.089014862189771726 ) ) ;
#177678 = CARTESIAN_POINT ( 'NONE',  ( -1.402160292154681736E-14, 2.196875000341423689, -1.575800808251660134 ) ) ;
#177679 = CARTESIAN_POINT ( 'NONE',  ( -1.201851678989727383E-14, 3.337500000000019007, -1.732050807568863648 ) ) ;
#177681 = CARTESIAN_POINT ( 'NONE',  ( 4.383363735919856730, 4.008345868194933104, -0.7998128361456211532 ) ) ;
#177680 = CARTESIAN_POINT ( 'NONE',  ( -11.48788097203293823, 11.33043054397690241, -3.469500700354831491 ) ) ;
#177682 = CARTESIAN_POINT ( 'NONE',  ( 4.675157572021750418, -0.8594996001172333644, -1.823839583407538267 ) ) ;
#177683 = CARTESIAN_POINT ( 'NONE',  ( 4.715990674440117658, 0.9792849278024118309, -1.646335200727979897 ) ) ;
#177684 = CARTESIAN_POINT ( 'NONE',  ( -0.6170404364503375705, 3.466143782776612170, 1.902435570468860027 ) ) ;
#177685 = CARTESIAN_POINT ( 'NONE',  ( 2.331793494658142230, 1.030094174309360344, -1.934364310732391345 ) ) ;
#177686 = CARTESIAN_POINT ( 'NONE',  ( -11.06298660227979802, 11.25680399625266936, -0.9087478855431304625 ) ) ;
#177687 = CARTESIAN_POINT ( 'NONE',  ( -1.500000000000013101, 0.7020833340161545255, 0.8660254037844403729 ) ) ;
#177688 = CARTESIAN_POINT ( 'NONE',  ( 5.203390118303760303, 1.773417465902687562, -0.9529421280250712778 ) ) ;
#177689 = CARTESIAN_POINT ( 'NONE',  ( -5.669280788808708671, 9.765911353585494226, 0.7998128361456481317 ) ) ;
#177691 = CARTESIAN_POINT ( 'NONE',  ( 5.536746206892352085, -1.668647081869235826, 1.303048207008510317 ) ) ;
#177690 = CARTESIAN_POINT ( 'NONE',  ( -3.714570900464290393, 5.356752022006865843, 1.443375672974064550 ) ) ;
#177692 = CARTESIAN_POINT ( 'NONE',  ( -1.364683531250014514, 9.651041667008064096, -0.7879004041258335089 ) ) ;
#177694 = CARTESIAN_POINT ( 'NONE',  ( -7.391130018105325661, 8.652015104991543026, -1.199719254218452047 ) ) ;
#177693 = CARTESIAN_POINT ( 'NONE',  ( 3.808215996505484036, 1.477046120823837683, -1.479981065426434483 ) ) ;
#177696 = ORIENTED_EDGE ( 'NONE', *, *, #97685, .F. ) ;
#177695 = CARTESIAN_POINT ( 'NONE',  ( 1.430204257492089903, 1.660765249891223316, 0.4652242431656942179 ) ) ;
#177697 = CARTESIAN_POINT ( 'NONE',  ( 4.763993809689464065, 0.6627061821620899851, -2.014485251161435286 ) ) ;
#177698 = CARTESIAN_POINT ( 'NONE',  ( 4.964256800898067645, 8.943383367689749619, 0.7998128361456462443 ) ) ;
#177699 = SURFACE_STYLE_FILL_AREA ( #210168 ) ;
#177700 = CARTESIAN_POINT ( 'NONE',  ( 0.3282377607281237730, 0.9263354503153991004, -1.225000000000000311 ) ) ;
#177701 = CARTESIAN_POINT ( 'NONE',  ( -9.361980464089073806, 14.57101365722899899, 7.422930886903910341 ) ) ;
#177702 = CARTESIAN_POINT ( 'NONE',  ( 6.307567778855705853, 8.381915046796901692, -1.599625672291262513 ) ) ;
#177703 = ORIENTED_EDGE ( 'NONE', *, *, #28884, .F. ) ;
#177705 = TOROIDAL_SURFACE ( 'NONE', #205347, 11.92000000000000171, 0.08000000000000000167 ) ;
#177704 = LINE ( 'NONE', #29315, #89209 ) ;
#177707 = CARTESIAN_POINT ( 'NONE',  ( 1.699580558467077118, 1.249458034614457702, 1.311817296177042902 ) ) ;
#177706 = CARTESIAN_POINT ( 'NONE',  ( 5.825163275726873202, 6.825053905550038991, 1.199719254218452047 ) ) ;
#177708 = CARTESIAN_POINT ( 'NONE',  ( -5.208303565944065738, 9.228104593576741621, -0.7998128361456231517 ) ) ;
#177709 = ORIENTED_EDGE ( 'NONE', *, *, #124222, .F. ) ;
#177710 = CARTESIAN_POINT ( 'NONE',  ( 2.517010073631369860, 6.088262185878572375, -0.7998128361456281477 ) ) ;
#177711 = CIRCLE ( 'NONE', #205351, 0.5000000000000008882 ) ;
#177712 = VERTEX_POINT ( 'NONE', #160439 ) ;
#177713 = CARTESIAN_POINT ( 'NONE',  ( 4.213551878797002992, 8.137837301896977849, 0.000000000000000000 ) ) ;
#177714 = CARTESIAN_POINT ( 'NONE',  ( 2.560951022220711248, -1.505102882618135629, 1.007669420338821675 ) ) ;
#177715 = CARTESIAN_POINT ( 'NONE',  ( 6.639320575229255894, 7.053084031878349869, 2.494893166485531388 ) ) ;
#177716 = CARTESIAN_POINT ( 'NONE',  ( 0.4019237886466778820, 9.104914550367427140, 1.500000000000001554 ) ) ;
#177717 = CARTESIAN_POINT ( 'NONE',  ( 4.532311885504772597, 6.983620743164907552, 1.170841521963662091 ) ) ;
#177718 = EDGE_CURVE ( 'NONE', #113990, #35662, #39107, .T. ) ;
#177719 = CARTESIAN_POINT ( 'NONE',  ( 4.562867621930529971, 1.439169320343157921, -1.179982364782502069 ) ) ;
#177720 = CARTESIAN_POINT ( 'NONE',  ( 1.774859612008858667, 1.665787454739732221, -0.9457685036825744795 ) ) ;
#177721 = CARTESIAN_POINT ( 'NONE',  ( 6.299827777084090918, -0.6482784301091691903, 1.814149458844191320 ) ) ;
#177722 = CARTESIAN_POINT ( 'NONE',  ( 1.355377658251181394, 3.933662881449785598, 0.6426130056881899089 ) ) ;
#177723 = VECTOR ( 'NONE', #68856, 1000.000000000000000 ) ;
#177724 = CARTESIAN_POINT ( 'NONE',  ( 4.625518323863472503, 8.335144253906971556, 0.3473850511846506839 ) ) ;
#177725 = CARTESIAN_POINT ( 'NONE',  ( -4.636525346193588248, 4.511627113421689650, 0.7216878364870317197 ) ) ;
#177726 = CARTESIAN_POINT ( 'NONE',  ( 6.954969614130424027, 11.05795561655343384, 1.040834085586084257E-14 ) ) ;
#177727 = CARTESIAN_POINT ( 'NONE',  ( 5.875830846898042914, -1.922239612846994294, 0.4278824943488717114 ) ) ;
#177728 = CARTESIAN_POINT ( 'NONE',  ( -6.091691091241777656, 6.001394449403842479, 0.7998128361456341429 ) ) ;
#177729 = CARTESIAN_POINT ( 'NONE',  ( -11.94651559118242901, 9.948693441210181732, -1.135242698369575587 ) ) ;
#177730 = CARTESIAN_POINT ( 'NONE',  ( 0.4454078864507329816, 0.6539998520847762897, -1.985780399853773526 ) ) ;
#177731 = CARTESIAN_POINT ( 'NONE',  ( 5.895520149318425496, 1.459072380863110530, 1.257889585189754023 ) ) ;
#177732 = CARTESIAN_POINT ( 'NONE',  ( -8.044065211609668253, 8.279164256499745633, 0.7998128361456602331 ) ) ;
#177733 = CARTESIAN_POINT ( 'NONE',  ( 0.8151338971811080691, -0.2727355552937099636, 1.804975678908596226 ) ) ;
#177734 = CARTESIAN_POINT ( 'NONE',  ( 1.840723031453334935, 2.183200880077686978, 0.3216222850719457349 ) ) ;
#177735 = CARTESIAN_POINT ( 'NONE',  ( 0.1758378621803426134, 1.891278220088285833, -0.2826890867150752551 ) ) ;
#177736 = ORIENTED_EDGE ( 'NONE', *, *, #4291, .F. ) ;
#177737 = CARTESIAN_POINT ( 'NONE',  ( 0.3265233526151562482, -1.289390354768883862, 1.488895225407897538 ) ) ;
#177738 = CARTESIAN_POINT ( 'NONE',  ( 2.507286712376335824, -1.920573583173491139, 0.2874136252781610001 ) ) ;
#177739 = EDGE_LOOP ( 'NONE', ( #170059, #158362, #26381, #31101, #142467, #95515, #4006, #210253, #197388, #51921 ) ) ;
#177740 = CARTESIAN_POINT ( 'NONE',  ( 0.5970295589228531430, 1.038836743281198238, -1.727736137786803461 ) ) ;
#177742 = CARTESIAN_POINT ( 'NONE',  ( 5.207777014082533462, 0.5861155943000575519, -1.766266804033526094 ) ) ;
#177741 = CARTESIAN_POINT ( 'NONE',  ( -4.620296487206990932, 8.612372678375294299, 0.000000000000000000 ) ) ;
#177743 = CARTESIAN_POINT ( 'NONE',  ( 6.384963997392946844, 6.413822516572072807, 0.7998128361456352531 ) ) ;
#177744 = CARTESIAN_POINT ( 'NONE',  ( -9.606148981167596190, -6.583980363595129504, 0.4355862708379978354 ) ) ;
#177745 = CARTESIAN_POINT ( 'NONE',  ( 6.509000000000038533, 4.695815278351551214, 2.562658139094180942 ) ) ;
#177746 = CARTESIAN_POINT ( 'NONE',  ( -5.362413449404877852, 6.214902764849178141, -1.199719254218446718 ) ) ;
#177747 = CARTESIAN_POINT ( 'NONE',  ( -6.882699257592852504, 8.058845884393651460, -1.199719254218452047 ) ) ;
#177748 = CARTESIAN_POINT ( 'NONE',  ( 1.628746693258641853, 0.2190750365392846177, 2.180598679842937759 ) ) ;
#177749 = CARTESIAN_POINT ( 'NONE',  ( 2.399429999938675007, 5.743159399996332404, 0.000000000000000000 ) ) ;
#177750 = CARTESIAN_POINT ( 'NONE',  ( 10.90688615205259104, -6.291672674598550508, 1.452407135538879159E-15 ) ) ;
#177751 = DIRECTION ( 'NONE',  ( 0.000000000000000000, 0.000000000000000000, 1.000000000000000000 ) ) ;
#177752 = CARTESIAN_POINT ( 'NONE',  ( 3.281694405262673087, 1.158851912627656189, 1.410738560442346801 ) ) ;
#177753 = CARTESIAN_POINT ( 'NONE',  ( -4.471491734408701291, 4.111161866431900513, 1.214306433183764966E-14 ) ) ;
#177754 = CARTESIAN_POINT ( 'NONE',  ( -4.464712657601869417, 4.103252943490596216, 0.7998128361456341429 ) ) ;
#177755 = CARTESIAN_POINT ( 'NONE',  ( -6.117836340636773507, 7.096790560477957754, -1.125390141808879196 ) ) ;
#177756 = CARTESIAN_POINT ( 'NONE',  ( 6.609000000000047947, 7.629137130509099585, 2.699999999999993516 ) ) ;
#177757 = CARTESIAN_POINT ( 'NONE',  ( 10.24048609702354717, 10.84165528948263457, -0.7998128361456281477 ) ) ;
#177758 = CARTESIAN_POINT ( 'NONE',  ( 0.7504602152685091454, 0.5580118324238073635, 1.843911685078497120 ) ) ;
#177759 = CARTESIAN_POINT ( 'NONE',  ( 5.823093080589802462, -1.771997608643091304, -0.8420800316405114838 ) ) ;
#177760 = CARTESIAN_POINT ( 'NONE',  ( -8.199983978166823562, 8.461069484149769337, -0.7998128361456291469 ) ) ;
#177761 = CARTESIAN_POINT ( 'NONE',  ( 6.484877546038077867, 6.460111979999551224, 1.040834085586084257E-14 ) ) ;
#177762 = CARTESIAN_POINT ( 'NONE',  ( 4.862908538974716421, 0.2148362657848035262, -2.180980218048253150 ) ) ;
#177763 = AXIS2_PLACEMENT_3D ( 'NONE', #36609, #132029, #182860 ) ;
#177764 = CARTESIAN_POINT ( 'NONE',  ( 3.161022370280501814, 6.839609865302569425, 0.000000000000000000 ) ) ;
#177765 = EDGE_CURVE ( 'NONE', #199393, #147848, #75990, .T. ) ;
#177766 = CARTESIAN_POINT ( 'NONE',  ( 3.977443466873982203, -0.1572589350618114057, 2.064370724987254047 ) ) ;
#177768 = CARTESIAN_POINT ( 'NONE',  ( -1.364683531250014514, 0.8010416670080889867, -0.7879004041258289570 ) ) ;
#177767 = CARTESIAN_POINT ( 'NONE',  ( 8.633889707083076459, 13.74036372393864447, 8.268811287266492727 ) ) ;
#177770 = EDGE_LOOP ( 'NONE', ( #8779, #23927 ) ) ;
#177769 = TOROIDAL_SURFACE ( 'NONE', #87933, 0.8300000000000010703, 0.08000000000000000167 ) ;
#177771 = CARTESIAN_POINT ( 'NONE',  ( 3.815287691547566418, 1.229174737571071541, -1.942296044024049761 ) ) ;
#177773 = ORIENTED_EDGE ( 'NONE', *, *, #52019, .F. ) ;
#177772 = CARTESIAN_POINT ( 'NONE',  ( 6.480434237652115570, 10.50433101066207442, 0.7216878364870438212 ) ) ;
#177775 = CARTESIAN_POINT ( 'NONE',  ( 3.285556943750000070, -0.6343749995220415716, 0.000000000000000000 ) ) ;
#177774 = CARTESIAN_POINT ( 'NONE',  ( 5.560252395380206991, 7.580323442733986283, 1.443375672974065660 ) ) ;
#177776 = CARTESIAN_POINT ( 'NONE',  ( -7.462104991928527831, -5.200000000000006395, -8.081892667527538876 ) ) ;
#177777 = CARTESIAN_POINT ( 'NONE',  ( -1.432341765624997709, 5.860937500170720682, 1.214306433183764966E-14 ) ) ;
#177778 = CARTESIAN_POINT ( 'NONE',  ( 4.294824717068760123, 1.560567246164183519, 1.155581451937383930 ) ) ;
#177779 = ORIENTED_EDGE ( 'NONE', *, *, #191715, .F. ) ;
#177780 = CARTESIAN_POINT ( 'NONE',  ( 9.612367721964607981, 12.23751498042398289, -1.443375672974058777 ) ) ;
#177781 = ORIENTED_EDGE ( 'NONE', *, *, #198277, .F. ) ;
#177782 = CARTESIAN_POINT ( 'NONE',  ( 4.781465250580236415, 0.1816826923375300662, -1.903719681147630016 ) ) ;
#177783 = CARTESIAN_POINT ( 'NONE',  ( 2.550000000000000266, -7.105553651663779391, -1.849324200890695824 ) ) ;
#177784 = CARTESIAN_POINT ( 'NONE',  ( 5.790025292147505276, -0.7713913475298206368, 1.542752225890047679 ) ) ;
#177785 = CARTESIAN_POINT ( 'NONE',  ( 4.276577519141481432, -0.4465006364167342645, -1.966305148836451577 ) ) ;
#177786 = CARTESIAN_POINT ( 'NONE',  ( -2.456316247939693387, 8.205176026796133115, 2.499999999999998668 ) ) ;
#177787 = CARTESIAN_POINT ( 'NONE',  ( 1.577102763248950046, -2.096353118739826993, -0.6898709473643764856 ) ) ;
#177789 = DIRECTION ( 'NONE',  ( 0.8003905289055504024, -4.396526966619893387E-05, 0.5994789398347104559 ) ) ;
#177788 = CARTESIAN_POINT ( 'NONE',  ( 0.000000000000000000, 0.000000000000000000, -11.00000000000000000 ) ) ;
#177791 = CARTESIAN_POINT ( 'NONE',  ( 0.5668360377511200143, 0.1796360565177144708, -1.760708420565498589 ) ) ;
#177790 = CARTESIAN_POINT ( 'NONE',  ( 2.027394857466585432, -1.366561296588153063, -1.582253647643002914 ) ) ;
#177792 = CARTESIAN_POINT ( 'NONE',  ( 5.379529795981254914, -0.4926393568372189335, -1.955173248319847845 ) ) ;
#177794 = CARTESIAN_POINT ( 'NONE',  ( 3.117397163603967680, -2.209095822378583929, 0.6116082133489489925 ) ) ;
#177793 = CARTESIAN_POINT ( 'NONE',  ( 3.901714345682657292, 7.774026846596938434, 0.7998128361456271485 ) ) ;
#177795 = CARTESIAN_POINT ( 'NONE',  ( 1.604977476713872697, -1.727474156022209328, 0.2105546776469246206 ) ) ;
#177796 = CARTESIAN_POINT ( 'NONE',  ( 11.84104725192624130, 11.10983537451419778, -1.443823348526961814 ) ) ;
#177797 = CARTESIAN_POINT ( 'NONE',  ( 1.264529683829066498, -1.734034291683920426, -0.006956266631255938158 ) ) ;
#177798 = CARTESIAN_POINT ( 'NONE',  ( -0.6801582343750438575, 0.1302083336747333897, -1.178068619123883165 ) ) ;
#177799 = CARTESIAN_POINT ( 'NONE',  ( -11.45846087878745756, 12.50688399218583235, 3.566076377698269351 ) ) ;
#177800 = CARTESIAN_POINT ( 'NONE',  ( 1.750661792711872611, -2.160631921778751519, -0.2139166996905516871 ) ) ;
#177801 = CARTESIAN_POINT ( 'NONE',  ( 1.850796360583713884, -1.845628094615419768, -0.8128149310912060610 ) ) ;
#177802 = CARTESIAN_POINT ( 'NONE',  ( 4.656250000000003553, -1.895863743163975101, 0.7852924748302414493 ) ) ;
#177803 = B_SPLINE_CURVE_WITH_KNOTS ( 'NONE', 3,
 ( #34337, #198952, #17007, #739, #118860, #100412, #49530, #115654 ),
 .UNSPECIFIED., .F., .F.,
 ( 4, 2, 2, 4 ),
 ( 0.0003136881264510900055, 0.0009048594355810645352, 0.001200445090146051936, 0.001496030744711039119 ),
 .UNSPECIFIED. ) ;
#177804 = CARTESIAN_POINT ( 'NONE',  ( 0.7499999999999885647, 1.097916667349485564, -1.299038105676652899 ) ) ;
#177805 = CARTESIAN_POINT ( 'NONE',  ( 0.1473221176215748218, -1.486828977120215001, -1.224531343831699592 ) ) ;
#177806 = CARTESIAN_POINT ( 'NONE',  ( -8.012344526598182026E-15, 13.04687500034139980, -1.575800808251669460 ) ) ;
#177807 = CARTESIAN_POINT ( 'NONE',  ( 3.621504738650199950, 1.906737781736141280, 1.139490138724685853 ) ) ;
#177808 = EDGE_LOOP ( 'NONE', ( #4119, #188131, #53236, #199364 ) ) ;
#177809 = CARTESIAN_POINT ( 'NONE',  ( 6.505896022970779846, -8.148356111791681400, 6.958662999125761139 ) ) ;
#177810 = CARTESIAN_POINT ( 'NONE',  ( -0.7500000000000249800, -0.3083333333333132531, 1.299038105676659116 ) ) ;
#177811 = CARTESIAN_POINT ( 'NONE',  ( 6.903072767652295383, 11.20533532890304684, 1.040834085586084257E-14 ) ) ;
#177812 = CARTESIAN_POINT ( 'NONE',  ( -1.602468905319636405E-14, -1.053124999658583638, -1.575800808251665908 ) ) ;
#177813 = CARTESIAN_POINT ( 'NONE',  ( 5.548340067360077121, -1.366870494764490296, 1.077293122972399431 ) ) ;
#177814 = CARTESIAN_POINT ( 'NONE',  ( 3.982823771651412770, 1.862158852298421152, 0.6176278068941787325 ) ) ;
#177816 = CARTESIAN_POINT ( 'NONE',  ( -7.226132686403777150, 7.532835677000276675, 1.040834085586084257E-14 ) ) ;
#177815 = CARTESIAN_POINT ( 'NONE',  ( 3.816783937446950770, 4.411668334231586996, 1.199719254218464037 ) ) ;
#177817 = CARTESIAN_POINT ( 'NONE',  ( -1.465018125636653901, 4.370054533944408348, -0.3314627765801590464 ) ) ;
#177818 = CARTESIAN_POINT ( 'NONE',  ( 4.235799883310053637, -1.556133899351975103, -1.642472060615452589 ) ) ;
#177819 = CARTESIAN_POINT ( 'NONE',  ( 1.750508186522087062, -2.052535545683041196, -0.2044793282457678107 ) ) ;
#177820 = CARTESIAN_POINT ( 'NONE',  ( -5.910464900553636269, 8.982960586366182554, -1.199719254218440723 ) ) ;
#177821 = CARTESIAN_POINT ( 'NONE',  ( 2.167197484064213420, -2.068651741926224474, -0.9167319039211866416 ) ) ;
#177822 = VERTEX_POINT ( 'NONE', #145300 ) ;
#177823 = CARTESIAN_POINT ( 'NONE',  ( 0.7499999999999885647, 1.597916667349486008, -1.299038105676652899 ) ) ;
#177824 = CARTESIAN_POINT ( 'NONE',  ( 3.919104170388473030, -0.1403237101727794756, 1.865361397874479632 ) ) ;
#177825 = CARTESIAN_POINT ( 'NONE',  ( 2.830371795882984820, 0.6218406304432465559, -1.619021885657184745 ) ) ;
#177826 = CARTESIAN_POINT ( 'NONE',  ( 6.093348126157794198, -0.7399906200981146709, 2.062998119606203939 ) ) ;
#177827 = CARTESIAN_POINT ( 'NONE',  ( 0.2884678563945877738, -1.037960011796670523, 1.947446179978419512 ) ) ;
#177828 = CARTESIAN_POINT ( 'NONE',  ( 4.012696165952275962, 1.530467462299599513, -1.526897427004340280 ) ) ;
#177829 = CARTESIAN_POINT ( 'NONE',  ( 4.787022420419578594, 1.440143517293355879, 1.302930595787118895 ) ) ;
#177830 = CARTESIAN_POINT ( 'NONE',  ( -3.104453987404963478, 5.605318171072321221, -1.082531754730549078 ) ) ;
#177833 = VERTEX_POINT ( 'NONE', #110692 ) ;
#177832 = UNCERTAINTY_MEASURE_WITH_UNIT (LENGTH_MEASURE( 1.000000000000000082E-05 ), #82587, 'distance_accuracy_value', 'NONE');
#177831 = CARTESIAN_POINT ( 'NONE',  ( 7.055228938194279209, -8.176568542494891290, -6.396834479292358822 ) ) ;
#177834 =( LENGTH_UNIT ( ) NAMED_UNIT ( * ) SI_UNIT ( .MILLI., .METRE. ) );
#177835 = CARTESIAN_POINT ( 'NONE',  ( 4.097125688280337741, 7.463757567055806064, 0.6283840521477540575 ) ) ;
#177836 = CARTESIAN_POINT ( 'NONE',  ( -3.812211943230557213E-13, -7.217909409572238033, 9.581972888692771306 ) ) ;
#177837 = DIRECTION ( 'NONE',  ( -0.000000000000000000, -0.000000000000000000, -1.000000000000000000 ) ) ;
#177838 = CARTESIAN_POINT ( 'NONE',  ( 1.360316468749992236, 2.015625000341400685, -1.040834085586084257E-14 ) ) ;
#177839 = CARTESIAN_POINT ( 'NONE',  ( 5.309220276109914316, 1.198862193007979471, -1.621181151826488254 ) ) ;
#177840 = CARTESIAN_POINT ( 'NONE',  ( -4.433153041544240835, 4.274359424664112339, 0.7216878364870317197 ) ) ;
#177841 =( BOUNDED_CURVE ( )  B_SPLINE_CURVE ( 2, ( #16257, #198218, #99670, #113871, #2131, #67137, #165739, #17326, #68206 ),
 .UNSPECIFIED., .F., .T. ) 
 B_SPLINE_CURVE_WITH_KNOTS ( ( 3, 2, 2, 2, 3 ),
 ( 0.6517857142857143016, 0.6547619047619047672, 0.6607142857142856984, 0.6666666666666666297, 0.6696428571428570953 ),
 .UNSPECIFIED. ) 
 CURVE ( )  GEOMETRIC_REPRESENTATION_ITEM ( )  RATIONAL_B_SPLINE_CURVE ( ( 0.9330127018922194093, 0.9330127018922194093, 1.000000000000000000, 0.8660254037844387076, 1.000000000000000000, 0.8660254037844387076, 1.000000000000000000, 0.9330127018922206306, 0.9330127018922194093 ) ) 
 REPRESENTATION_ITEM ( '' )  );
#177842 = CARTESIAN_POINT ( 'NONE',  ( 6.435316467980822353, 10.65961964595298817, 1.040834085586084257E-14 ) ) ;
#177843 = LINE ( 'NONE', #210314, #164169 ) ;
#177844 = CARTESIAN_POINT ( 'NONE',  ( 2.789462663364688844, 1.291185895303394116, 1.290987730777813702 ) ) ;
#177845 = CARTESIAN_POINT ( 'NONE',  ( 2.098912041516465266, -0.5885267676426220174, -2.126790307141281033 ) ) ;
#177846 = ORIENTED_EDGE ( 'NONE', *, *, #63620, .F. ) ;
#177847 = CARTESIAN_POINT ( 'NONE',  ( -4.082413651046300274, 6.816547455312373494, 1.082531754730549967 ) ) ;
#177848 = EDGE_CURVE ( 'NONE', #60775, #179068, #132311, .T. ) ;
#177849 = CARTESIAN_POINT ( 'NONE',  ( 0.000000000000000000, -7.154544010627095219, 0.000000000000000000 ) ) ;
#177850 = CARTESIAN_POINT ( 'NONE',  ( -7.832860060393135093, 10.16142270859057462, 1.599625672291295375 ) ) ;
#177851 = CARTESIAN_POINT ( 'NONE',  ( 0.9143263792395848188, -2.019972748253701322, 0.004280675582559247648 ) ) ;
#177852 = CARTESIAN_POINT ( 'NONE',  ( 1.260569961473339440, 2.118219532560499996, 0.1004958096475216667 ) ) ;
#177853 = CARTESIAN_POINT ( 'NONE',  ( -4.502189528189771472, 7.410248995266807803, -1.199719254218453823 ) ) ;
#177854 = CARTESIAN_POINT ( 'NONE',  ( 1.990827601993300666, 0.1760917813397035736, 1.852568099299256366 ) ) ;
#177855 = CARTESIAN_POINT ( 'NONE',  ( 5.379888026524302980, 5.170957540566797128, -0.7998128361456211532 ) ) ;
#177856 = CARTESIAN_POINT ( 'NONE',  ( 6.649297902391459125, -1.653525193404258742, -1.229868563883255828 ) ) ;
#177857 = DIRECTION ( 'NONE',  ( 0.000000000000000000, 0.000000000000000000, -1.000000000000000000 ) ) ;
#177858 = ORIENTED_EDGE ( 'NONE', *, *, #207366, .F. ) ;
#177859 = EDGE_LOOP ( 'NONE', ( #174120, #14131, #63102, #107195 ) ) ;
#177860 = ORIENTED_EDGE ( 'NONE', *, *, #165043, .F. ) ;
#177861 = CARTESIAN_POINT ( 'NONE',  ( -7.960608749518247151, 12.43912730774665576, 0.000000000000000000 ) ) ;
#177862 = CARTESIAN_POINT ( 'NONE',  ( 4.477060521952030747, -0.002618581577289170060, -1.825872481161804561 ) ) ;
#177864 = CARTESIAN_POINT ( 'NONE',  ( -5.470032677541931676, 6.438256155886466381, -1.298486150373518999 ) ) ;
#177863 = CARTESIAN_POINT ( 'NONE',  ( -3.793249116773374396, 7.647484079536056356, 0.7998128361456352531 ) ) ;
#177865 = CARTESIAN_POINT ( 'NONE',  ( 5.703612580814390043, 7.410739916031705121, 1.319003781635886163 ) ) ;
#177866 = CARTESIAN_POINT ( 'NONE',  ( 6.011092252151500226, 2.013677719867816851, 0.1017325769363253418 ) ) ;
#177867 = CARTESIAN_POINT ( 'NONE',  ( 5.876868881424701208, 1.699447150514224125, -0.7087742222662285485 ) ) ;
#177868 = CARTESIAN_POINT ( 'NONE',  ( 0.07680821025393863577, 2.892152076732486421, -2.299782885777381658 ) ) ;
#177869 = CARTESIAN_POINT ( 'NONE',  ( 4.617980755673473325, -2.263821322725892315, 0.4470779566097658475 ) ) ;
#177870 = CARTESIAN_POINT ( 'NONE',  ( 5.611095471209277541, 7.639640364534566075, 1.599625672291268286 ) ) ;
#177871 = CARTESIAN_POINT ( 'NONE',  ( 6.327428285124779173, -2.037722512857220725, 0.7216720553550812767 ) ) ;
#177872 = CARTESIAN_POINT ( 'NONE',  ( 1.136160399770862250, 0.3804006922196729867, 1.904278901077125052 ) ) ;
#177873 = ORIENTED_EDGE ( 'NONE', *, *, #194552, .F. ) ;
#177874 = ADVANCED_FACE ( 'NONE', ( #141038 ), #176691, .T. ) ;
#177875 = CARTESIAN_POINT ( 'NONE',  ( 4.569826555773855326, 1.780639694173843823, -1.453273832002010213 ) ) ;
#177876 = CARTESIAN_POINT ( 'NONE',  ( -4.858757509019083543, 5.629766575900002401, -2.500000000000000444 ) ) ;
#177877 = CARTESIAN_POINT ( 'NONE',  ( -4.679499295372141709, 5.488445928469455559, 1.199719254218452935 ) ) ;
#177878 = CARTESIAN_POINT ( 'NONE',  ( 4.293723057671197552, -0.7160966649314598476, 1.728361679364013748 ) ) ;
#177881 = CARTESIAN_POINT ( 'NONE',  ( -4.450819567036169211, 8.414649604842665553, -0.7998128361456362523 ) ) ;
#177880 = CARTESIAN_POINT ( 'NONE',  ( -1.500000000000001332, 0.1812500006828157706, 0.000000000000000000 ) ) ;
#177879 = CARTESIAN_POINT ( 'NONE',  ( 2.355592738034977263, -1.419685808644566949, -1.281520755053264571 ) ) ;
#177882 = CARTESIAN_POINT ( 'NONE',  ( 3.791807063958370971, 1.597966631936774684, 1.522356218736670153 ) ) ;
#177883 = CARTESIAN_POINT ( 'NONE',  ( 6.883263157960370471, 7.053006342242538196, 2.444342378444531949 ) ) ;
#177884 = CARTESIAN_POINT ( 'NONE',  ( 3.728655938958122196, 4.308852335994623139, -1.199719254218446718 ) ) ;
#177885 = CARTESIAN_POINT ( 'NONE',  ( 7.146556367734776316, 7.510272981878305387, 0.7216878364870267237 ) ) ;
#177886 = CARTESIAN_POINT ( 'NONE',  ( -3.273404022695637572, 5.906389562198459231, 1.199719254218462483 ) ) ;
#177887 = CARTESIAN_POINT ( 'NONE',  ( -5.275531169048895741, 9.168887107283438809, -0.7216878364870338292 ) ) ;
#177888 = CARTESIAN_POINT ( 'NONE',  ( 1.159376733683295191, 0.3886980088604417016, -1.932498344103703136 ) ) ;
#177889 = CARTESIAN_POINT ( 'NONE',  ( 0.9741375256873509025, 2.223107509294399264, -0.6184994596578182735 ) ) ;
#177890 = CARTESIAN_POINT ( 'NONE',  ( 2.242563829109287088, -1.923402688547710904, -0.3857071251459272543 ) ) ;
#177891 = CARTESIAN_POINT ( 'NONE',  ( -4.773352600463090845, 7.726605912919016106, 1.199719254218452935 ) ) ;
#177892 = CARTESIAN_POINT ( 'NONE',  ( 4.750865691763131338, -0.4467450692671371959, -2.013472809446889666 ) ) ;
#177893 = CARTESIAN_POINT ( 'NONE',  ( 4.934804725694211136, 6.780358151441803649, -1.443375672974051449 ) ) ;
#177894 = CARTESIAN_POINT ( 'NONE',  ( 6.364626766972446781, 6.390095747748157251, 0.7998128361456352531 ) ) ;
#177895 = ORIENTED_EDGE ( 'NONE', *, *, #158451, .F. ) ;
#177896 = CARTESIAN_POINT ( 'NONE',  ( -1.364683531250010295, 5.801041667008088432, -0.7879004041258300672 ) ) ;
#177897 = LINE ( 'NONE', #98777, #31680 ) ;
#177898 = CARTESIAN_POINT ( 'NONE',  ( 10.73535870392234237, 11.41900666419791399, 0.000000000000000000 ) ) ;
#177899 = CARTESIAN_POINT ( 'NONE',  ( 1.165147980530324201, 1.645521545068162617, -1.416405498411864583 ) ) ;
#177900 = CARTESIAN_POINT ( 'NONE',  ( 4.342354338126830804, 8.288106837781777259, -0.7998128361456381397 ) ) ;
#177901 = CARTESIAN_POINT ( 'NONE',  ( 11.09544190643661210, 2.974000657017507709, -3.605127613804859799 ) ) ;
#177902 = CARTESIAN_POINT ( 'NONE',  ( -10.44245235073009326, 1.000000000000000888, 5.695529491621741158 ) ) ;
#177903 = CARTESIAN_POINT ( 'NONE',  ( 2.319419987651088810, -1.815478447740950685, 0.4500915571382518854 ) ) ;
#177904 = CARTESIAN_POINT ( 'NONE',  ( 6.661405305706385782, 0.3767857563467743032, -2.128362917677539379 ) ) ;
#177906 = PRESENTATION_STYLE_ASSIGNMENT (( #111903 ) ) ;
#177905 = FACE_OUTER_BOUND ( 'NONE', #82270, .T. ) ;
#177907 = CARTESIAN_POINT ( 'NONE',  ( 1.364683531249988757, -0.8656249996585805295, 0.000000000000000000 ) ) ;
#177908 = CARTESIAN_POINT ( 'NONE',  ( 2.613799471529183460, -0.5979904443059110841, 1.816458080996792068 ) ) ;
#177909 = CARTESIAN_POINT ( 'NONE',  ( 4.697990591988738807, -1.769527177957382680, -0.04185004791794690038 ) ) ;
#177910 = CARTESIAN_POINT ( 'NONE',  ( 1.998553653897700011, -1.875654816251038248, -0.3715787057524469472 ) ) ;
#177911 = CARTESIAN_POINT ( 'NONE',  ( -4.904298879841297421, 6.744767997946721216, 1.599625672291267398 ) ) ;
#177913 = CARTESIAN_POINT ( 'NONE',  ( 5.483970141128155618, -1.915793143390194242, 0.004843307671191510178 ) ) ;
#177912 = CARTESIAN_POINT ( 'NONE',  ( -11.07790593930098311, 11.29999999999999893, 0.6999999999999992895 ) ) ;
#177914 = CARTESIAN_POINT ( 'NONE',  ( 1.499999999999987121, -0.4958333333333110882, 0.8660254037844524744 ) ) ;
#177915 = CARTESIAN_POINT ( 'NONE',  ( 6.619592842669682398, 0.3380432134332654881, -1.940159576567195288 ) ) ;
#177916 = CARTESIAN_POINT ( 'NONE',  ( -1.001543065824772872E-14, 4.212500000000023448, 1.732050807568877637 ) ) ;
#177917 = CARTESIAN_POINT ( 'NONE',  ( 5.450602278258352307, 7.609395523180757515, -1.379288001542776865 ) ) ;
#177918 = CARTESIAN_POINT ( 'NONE',  ( 5.453920962983416665, 1.868457504587007545, -0.09292587778651077712 ) ) ;
#177920 = ORIENTED_EDGE ( 'NONE', *, *, #146436, .F. ) ;
#177919 = CARTESIAN_POINT ( 'NONE',  ( 2.244514701088017539, 0.3993153960501935051, 1.781317584591130432 ) ) ;
#177922 = CARTESIAN_POINT ( 'NONE',  ( 4.597294405107005488, 8.370805622008914426, 0.1071034531749150143 ) ) ;
#177921 = CARTESIAN_POINT ( 'NONE',  ( 4.336686996305870068, 2.164023489887345164, 0.4319772483800735086 ) ) ;
#177923 = CARTESIAN_POINT ( 'NONE',  ( -1.402160292154681736E-14, -0.8031249996585825279, -1.575800808251665908 ) ) ;
#177924 = CARTESIAN_POINT ( 'NONE',  ( 1.873554394494097997, -0.2548139927673950256, 2.046832928722150058 ) ) ;
#177925 = CARTESIAN_POINT ( 'NONE',  ( 5.015626762051672571, 7.938982758113895422, 1.199719254218462483 ) ) ;
#177927 = CARTESIAN_POINT ( 'NONE',  ( -8.259941899223614215, 10.65968485389279508, -1.599625672291263179 ) ) ;
#177926 = CIRCLE ( 'NONE', #25755, 1.850000000000000089 ) ;
#177928 = CARTESIAN_POINT ( 'NONE',  ( 1.392969482149218452, 3.541472066643499783, 0.5575990067801355199 ) ) ;
#177929 = DIRECTION ( 'NONE',  ( 0.000000000000000000, -1.000000000000000000, 0.000000000000000000 ) ) ;
#177930 = CARTESIAN_POINT ( 'NONE',  ( 6.017840079619279692, 8.114175741012878973, -1.599625672291281386 ) ) ;
#177931 = ORIENTED_EDGE ( 'NONE', *, *, #197101, .T. ) ;
#177932 = CARTESIAN_POINT ( 'NONE',  ( 5.002425025097493538, 2.064580399062130311, 0.1557331365308264881 ) ) ;
#177934 = CARTESIAN_POINT ( 'NONE',  ( -1.500000000000011324, 5.879166666666686858, -0.8660254037844313801 ) ) ;
#177933 = AXIS2_PLACEMENT_3D ( 'NONE', #180625, #771, #50627 ) ;
#177935 = CARTESIAN_POINT ( 'NONE',  ( 2.214359598146302677, -1.016813397907929239, -1.907474440234188995 ) ) ;
#177936 = CARTESIAN_POINT ( 'NONE',  ( -4.619186966818853435, 8.364647258818639131, 0.2498820228645174391 ) ) ;
#177937 = CARTESIAN_POINT ( 'NONE',  ( 3.264323853713008816, 2.019862492602925386, -0.002211735406987268802 ) ) ;
#177938 = CARTESIAN_POINT ( 'NONE',  ( -5.692136587293105343, 5.855332880448205657, 2.499999999999999112 ) ) ;
#177939 = ORIENTED_EDGE ( 'NONE', *, *, #31233, .F. ) ;
#177940 = VERTEX_POINT ( 'NONE', #191854 ) ;
#177942 = CARTESIAN_POINT ( 'NONE',  ( 7.510853912290742507, 8.825379654836435606, -1.082531754730537976 ) ) ;
#177941 = CARTESIAN_POINT ( 'NONE',  ( 1.001543065824772753E-15, -0.9624999999999998002, 4.012584370867899430 ) ) ;
#177943 = CARTESIAN_POINT ( 'NONE',  ( -5.451787166026575981, 5.533042246551999277, 0.000000000000000000 ) ) ;
#177944 = CARTESIAN_POINT ( 'NONE',  ( 1.675017921984035096, 1.752138005693338441, -0.9981273289914743829 ) ) ;
#177945 = CARTESIAN_POINT ( 'NONE',  ( 6.409741707328596938, -1.031184584194230647, -1.933826218581576439 ) ) ;
#177946 = CARTESIAN_POINT ( 'NONE',  ( 1.499999999999989120, 4.577083334016148974, -0.8660254037844323793 ) ) ;
#177947 = CARTESIAN_POINT ( 'NONE',  ( 4.429883728109570207, -1.874397765517330061, 0.3784635845696313061 ) ) ;
#177948 = CARTESIAN_POINT ( 'NONE',  ( -4.440459003675619520, 5.139289244831666714, 1.199719254218462483 ) ) ;
#177949 = CARTESIAN_POINT ( 'NONE',  ( 6.521108698048765362, 8.631046119188804155, -1.443375672974058777 ) ) ;
#177951 = CARTESIAN_POINT ( 'NONE',  ( 1.687125285987755019, 1.678019391100945779, 1.117813378161469418 ) ) ;
#177950 = CARTESIAN_POINT ( 'NONE',  ( -9.503902493055310430, 11.15060299906175167, 1.082531754730558626 ) ) ;
#177952 = CARTESIAN_POINT ( 'NONE',  ( 1.364683531249997417, 14.29687500034140157, 2.602085213965210642E-15 ) ) ;
#177953 = CARTESIAN_POINT ( 'NONE',  ( -5.503684012504701961, 5.385662534202396934, 0.000000000000000000 ) ) ;
#177954 = CARTESIAN_POINT ( 'NONE',  ( 4.735197965344590365, -1.576124854778211626, 0.7008788178320748408 ) ) ;
#177955 = FACE_BOUND ( 'NONE', #165497, .T. ) ;
#177956 = CARTESIAN_POINT ( 'NONE',  ( 3.871016551901614200, 4.474939717762034697, -1.199719254218446718 ) ) ;
#177957 = CARTESIAN_POINT ( 'NONE',  ( -1.500000000000031530, 4.670833333333352932, 0.8660254037844287156 ) ) ;
#177958 = CARTESIAN_POINT ( 'NONE',  ( 3.005103603723342953, 6.657704637652544832, -0.7998128361456291469 ) ) ;
#177959 = CARTESIAN_POINT ( 'NONE',  ( 1.419999999999989049, 6.280000000000042881, -2.873333333333328632 ) ) ;
#177960 = CARTESIAN_POINT ( 'NONE',  ( 0.4970418144054839504, 0.3504251219754518365, 2.040211723117946629 ) ) ;
#177961 = DIRECTION ( 'NONE',  ( 8.638326563840814399E-31, -0.000000000000000000, 1.000000000000000000 ) ) ;
#177962 = VERTEX_POINT ( 'NONE', #74927 ) ;
#177963 = CARTESIAN_POINT ( 'NONE',  ( 5.602179418825736334, -0.8085942178241835032, 1.621059995222628780 ) ) ;
#177964 = COLOUR_RGB ( '', 0.40784314, 0.44705882, 0.49803922) ;
#177965 = CARTESIAN_POINT ( 'NONE',  ( 5.876533236880477240, 5.820653295974182129, 0.7998128361456352531 ) ) ;
#177966 = CARTESIAN_POINT ( 'NONE',  ( 6.890000000000009450, -0.01081285896028029957, 2.279840171838914298 ) ) ;
#177967 = CARTESIAN_POINT ( 'NONE',  ( 6.481129863841750272, -1.659422710288318115, -0.7269172754736009656 ) ) ;
#177968 = CARTESIAN_POINT ( 'NONE',  ( 5.844973620822844218, 6.952128991449046502, 1.082531754730549967 ) ) ;
#177969 = CARTESIAN_POINT ( 'NONE',  ( -1.123270288250318494, 3.297697346350006331, -0.7749999999993562039 ) ) ;
#177970 = CARTESIAN_POINT ( 'NONE',  ( 2.923975034273151419, 1.216836049711809586, -1.822369523680394066 ) ) ;
#177971 = ORIENTED_EDGE ( 'NONE', *, *, #133575, .T. ) ;
#177972 = ADVANCED_FACE ( 'NONE', ( #209165 ), #12044, .T. ) ;
#177974 = CARTESIAN_POINT ( 'NONE',  ( 9.901532256681887745, 10.44620914241737530, 0.000000000000000000 ) ) ;
#177973 = CARTESIAN_POINT ( 'NONE',  ( 0.6077679335219284829, 0.6189715888181289705, -1.861716921216026055 ) ) ;
#177975 = CARTESIAN_POINT ( 'NONE',  ( 5.149962951811881240, 0.9480454039230011842, 1.664493911490998679 ) ) ;
#177976 = CARTESIAN_POINT ( 'NONE',  ( -1.499999999973776532, 7.854386371694295654, 3.680172642290445939 ) ) ;
#177977 = CARTESIAN_POINT ( 'NONE',  ( -1.500000000000015099, 11.97916666666666785, -0.8660254037844309360 ) ) ;
#177978 = CARTESIAN_POINT ( 'NONE',  ( -1.402160292154681736E-14, -0.8031249996585825279, -1.575800808251665908 ) ) ;
#177980 = ORIENTED_EDGE ( 'NONE', *, *, #199113, .F. ) ;
#177979 = CARTESIAN_POINT ( 'NONE',  ( 3.863710590214593399, 7.451486755318259547, 1.040834085586084257E-14 ) ) ;
#177981 = CARTESIAN_POINT ( 'NONE',  ( -9.192064960385334160, 9.826423329978791088, 0.7216878364870438212 ) ) ;
#177982 = CARTESIAN_POINT ( 'NONE',  ( 1.622176833581047806, -1.201014165160016356, -1.797165035535647659 ) ) ;
#177983 = CARTESIAN_POINT ( 'NONE',  ( -5.659602779061863487, 5.567567761852417085, 0.7998128361456281477 ) ) ;
#177985 = EDGE_CURVE ( 'NONE', #3126, #211239, #205630, .T. ) ;
#177984 =( GEOMETRIC_REPRESENTATION_CONTEXT ( 3 ) GLOBAL_UNCERTAINTY_ASSIGNED_CONTEXT ( ( #63826 ) ) GLOBAL_UNIT_ASSIGNED_CONTEXT ( ( #58068, #123174, #189134 ) ) REPRESENTATION_CONTEXT ( 'NONE', 'WORKASPACE' ) );
#177986 = CARTESIAN_POINT ( 'NONE',  ( 4.309512724297349884, 6.121127159803966933, 1.599625672291261402 ) ) ;
#177987 = CARTESIAN_POINT ( 'NONE',  ( 2.063248287022978467, 0.3151258922809499485, -1.798016661460503984 ) ) ;
#177988 = CARTESIAN_POINT ( 'NONE',  ( -4.302014814237876017, 3.913438792899272212, 0.7998128361456341429 ) ) ;
#177989 = CARTESIAN_POINT ( 'NONE',  ( 4.559475717982610199, 0.3993622990657343941, -1.781190812766835441 ) ) ;
#177990 = CARTESIAN_POINT ( 'NONE',  ( 12.64922964589999843, 7.339083607935379838, 3.660861416055261497 ) ) ;
#177991 = VERTEX_POINT ( 'NONE', #183076 ) ;
#177992 = CARTESIAN_POINT ( 'NONE',  ( 3.842214238857721842, -0.9727578572899638898, 1.712498773813153408 ) ) ;
#177993 = ORIENTED_EDGE ( 'NONE', *, *, #115408, .F. ) ;
#177994 = CARTESIAN_POINT ( 'NONE',  ( 5.847205921155025798, 0.5594960185140216424, -1.859740419532672773 ) ) ;
#177995 = ORIENTED_EDGE ( 'NONE', *, *, #112332, .F. ) ;
#177996 = CARTESIAN_POINT ( 'NONE',  ( -5.315678745009726924, 8.359319748223434487, -1.199719254218453823 ) ) ;
#177998 = CARTESIAN_POINT ( 'NONE',  ( 5.396778611113259849, -2.069399493756381769, -0.4625044129713885011 ) ) ;
#177997 = CARTESIAN_POINT ( 'NONE',  ( 5.993586425693011144, 9.150212042353954800, -1.199719254218452047 ) ) ;
#177999 = CARTESIAN_POINT ( 'NONE',  ( 7.485510208076452621, 7.905719128943566432, 0.000000000000000000 ) ) ;
#178000 = ORIENTED_EDGE ( 'NONE', *, *, #60399, .T. ) ;
#178001 = CARTESIAN_POINT ( 'NONE',  ( 4.333225684176827741, 7.421547172477886534, -1.117180756173659084 ) ) ;
#178002 = DIRECTION ( 'NONE',  ( 0.000000000000000000, -1.000000000000000000, 0.000000000000000000 ) ) ;
#178003 = CARTESIAN_POINT ( 'NONE',  ( 5.076602173674213070, 4.887400388900169368, 0.000000000000000000 ) ) ;
#178004 = CARTESIAN_POINT ( 'NONE',  ( 5.320952465583661528, 1.522972439820569956, -1.316545952364375438 ) ) ;
#178005 = CARTESIAN_POINT ( 'NONE',  ( 0.08506230894391486608, -9.914238990527385553, 9.499619272424267180 ) ) ;
#178006 = CARTESIAN_POINT ( 'NONE',  ( 6.006453938882227561, -0.6616566355047011072, -1.701761020394356283 ) ) ;
#178007 = CARTESIAN_POINT ( 'NONE',  ( 1.363825363374836286, -0.5049007678423790280, 2.007717453658082629 ) ) ;
#178008 = CARTESIAN_POINT ( 'NONE',  ( -7.293923454472094114, 9.532663335016016148, 1.443375672974090751 ) ) ;
#178009 = CARTESIAN_POINT ( 'NONE',  ( -5.095330737579740976, 7.839774693193753308, -1.136590250493845877 ) ) ;
#178010 = CARTESIAN_POINT ( 'NONE',  ( 6.262560305340551636, -1.321439916381482060, 1.324322166508178356 ) ) ;
#178011 = CARTESIAN_POINT ( 'NONE',  ( 7.447506452608354088, 7.583179037664891098, 0.7998128361456341429 ) ) ;
#178012 = EDGE_CURVE ( 'NONE', #115982, #60692, #108283, .T. ) ;
#178013 = FILL_AREA_STYLE_COLOUR ( '', #162695 ) ;
#178014 = CARTESIAN_POINT ( 'NONE',  ( 0.6823417656249969321, 11.08854166700806765, -1.181850606188757036 ) ) ;
#178015 = CARTESIAN_POINT ( 'NONE',  ( -3.598799709423620374, 6.286017863381107240, 1.199719254218464037 ) ) ;
#178016 = CARTESIAN_POINT ( 'NONE',  ( -6.583366107887490770, 9.838288338247510367, 1.199719254218452935 ) ) ;
#178017 = CARTESIAN_POINT ( 'NONE',  ( 3.691823404346205706, 1.489760995587570358, 0.8873103889329400085 ) ) ;
#178018 = CLOSED_SHELL ( 'NONE', ( #173572, #146650, #10350, #138953, #60966, #127024, #184142, #108424, #214066, #31651, #150285, #62911, #2815, #101437, #79513, #70615, #150097, #185809, #135063, #188529, #14148, #165575, #68192, #18073, #174942, #88503, #162207, #109335, #96090, #199788, #112721, #112220, #132444, #148035, #130104, #204395, #140167, #177037, #8547, #152330, #133230, #136931, #93576, #10529, #10163, #166231, #146847, #19187, #90413, #183942, #123417, #157273, #29030, #36655, #113000, #200931, #18648, #148466, #35524, #125542, #129165, #26724, #32927, #8930, #168174, #53530, #121136, #135454, #137205, #136942, #161446, #22394, #174137, #5977, #149310, #18054, #146525, #96533, #43845, #185265, #196966, #52291, #60659, #178947, #29993, #26131, #32415, #161887, #140198, #160915, #186401, #133729, #46262, #26060, #194972, #105458, #211551, #284, #210040, #199820, #187943, #105120, #120938, #136283, #141783, #182121, #131184, #96023, #205607, #150808, #46010, #21265, #25227, #84626, #169236, #35989, #125024, #176546, #166099, #98501, #194799, #142290, #98552, #94644, #122029, #134905, #26513, #12454, #38129, #209792, #86006, #74977, #59965, #141658, #53763, #142167, #172649, #105343, #47228, #112572, #38043, #92463, #111267, #50809, #167101, #45192, #49901, #63112, #32070, #75296, #95113, #69803, #172707, #19967, #45896, #32761, #5813, #41084, #9958, #167239, #148874, #44213, #3359, #181290, #127277, #126894, #177336, #8692, #141676, #161053, #127887, #187695, #204668, #6871, #26171, #3901, #157014, #64763, #191981, #207203, #112458, #538, #5639, #208311, #93188, #206435, #174759, #104445, #69102, #149156, #181348, #163201, #174336, #168539, #36421, #13279, #180955, #129443, #48043, #128940, #194460, #68001, #138115, #91946, #109383, #32846, #46304, #27352, #99069, #53929, #154702, #95335, #48017, #69427, #42255, #172330, #34317, #194172, #630, #89741, #261, #193210, #138155, #50160, #163759, #77517, #155457, #210987, #27534, #7197, #153732, #146332, #99767, #51150, #150872, #162897, #51257, #184157, #162386, #34190, #42657, #21656, #70423, #25753, #45710, #39591, #162694, #152016, #109523, #118610, #61736, #164251, #145570, #78323, #20889, #131545, #201267, #146772, #49872, #88174, #201546, #152132, #70832, #67001, #23060, #164816, #202861, #168401, #144238, #92730, #171928, #185799, #90747, #189175, #66657 ) ) ;
#178019 = CARTESIAN_POINT ( 'NONE',  ( -4.334856428067329404, 6.080418470877079429, -1.599625672291256295 ) ) ;
#178020 = CARTESIAN_POINT ( 'NONE',  ( 1.674760025662187735, 1.393346669028448392, -1.531324272915953744 ) ) ;
#178021 = CARTESIAN_POINT ( 'NONE',  ( 2.320046401798322222, 0.9952771033397389555, -1.868693074688542843 ) ) ;
#178022 = CARTESIAN_POINT ( 'NONE',  ( 3.194917754314666514, 6.879154480009089134, 0.7998128361456321445 ) ) ;
#178023 = CARTESIAN_POINT ( 'NONE',  ( 9.237182729612253951, 9.671134694169463586, 0.7998128361456462443 ) ) ;
#178025 = ADVANCED_FACE ( 'NONE', ( #98644 ), #50953, .T. ) ;
#178024 = CARTESIAN_POINT ( 'NONE',  ( 1.499999999999989120, 3.535416667349488229, 0.8660254037844522523 ) ) ;
#178026 = CARTESIAN_POINT ( 'NONE',  ( 0.6550501802922055195, 1.640498656168420943, -1.089389633329050033 ) ) ;
#178027 = CARTESIAN_POINT ( 'NONE',  ( 4.161918892217930654, 7.618187422415517496, 0.8381857273355892701 ) ) ;
#178028 = CARTESIAN_POINT ( 'NONE',  ( 5.178851490740205676, 6.104710163027444736, 1.082531754730558626 ) ) ;
#178030 = CARTESIAN_POINT ( 'NONE',  ( -2.788906526875773208E-15, 8.468750000682796042, -1.499999999999998446 ) ) ;
#178029 = CARTESIAN_POINT ( 'NONE',  ( 3.475000000000000533, -2.245833333333331350, -2.006292185433951047 ) ) ;
#178031 = CARTESIAN_POINT ( 'NONE',  ( 2.607731988003787915, -2.267127051869659571, 0.3377934734241551662 ) ) ;
#178032 = CARTESIAN_POINT ( 'NONE',  ( 0.7326872660318054509, 0.1314506862302306234, 1.821024990000128296 ) ) ;
#178033 = CARTESIAN_POINT ( 'NONE',  ( 2.953266587970606150, -1.684550232849800544, 0.9053361341156559439 ) ) ;
#178034 = EDGE_CURVE ( 'NONE', #46524, #190431, #106014, .T. ) ;
#178035 = CARTESIAN_POINT ( 'NONE',  ( 6.866278450678116485, 6.975356045404744521, 0.000000000000000000 ) ) ;
#178036 = CARTESIAN_POINT ( 'NONE',  ( 7.090551149822728938, 10.25576486055978442, 1.082531754730558626 ) ) ;
#178037 = CARTESIAN_POINT ( 'NONE',  ( -7.458957065812611198, 11.85386701009007204, 0.7998128361456481317 ) ) ;
#178038 = CARTESIAN_POINT ( 'NONE',  ( 1.986589674187682064, -1.235133946311824049, 1.589746892572386994 ) ) ;
#178039 = CARTESIAN_POINT ( 'NONE',  ( 2.500770564479499303, 0.4249116886347775179, 1.915039037836663738 ) ) ;
#178040 = CARTESIAN_POINT ( 'NONE',  ( -8.890396042259075315, 11.39521468743417998, -1.599625672291263179 ) ) ;
#178041 = CARTESIAN_POINT ( 'NONE',  ( -7.714753101375940503, 8.959299025482085455, 1.199719254218462483 ) ) ;
#178042 = CARTESIAN_POINT ( 'NONE',  ( -10.94892088761405802, 5.391493950907642940, -4.806431146316898051 ) ) ;
#178044 = CARTESIAN_POINT ( 'NONE',  ( 3.344378923012015115, 0.4290688666262321149, 1.716912437317794415 ) ) ;
#178043 = CARTESIAN_POINT ( 'NONE',  ( 5.314434061427068201, 1.931386623266003078, 0.8008058956679960927 ) ) ;
#178045 = CARTESIAN_POINT ( 'NONE',  ( -3.796053574492273874, 15.00000000000182077, 12.24940615670316468 ) ) ;
#178046 = CARTESIAN_POINT ( 'NONE',  ( 6.685440801012543233, -0.9854850593251741619, 2.067252628450669594 ) ) ;
#178047 = B_SPLINE_CURVE_WITH_KNOTS ( 'NONE', 3,
 ( #29480, #209258, #56899, #60903, #96632, #93430, #130252, #176790 ),
 .UNSPECIFIED., .F., .F.,
 ( 4, 2, 2, 4 ),
 ( 0.000000000000000000, 0.0004970278158210380409, 0.0007455417237315570614, 0.0009940556316420760818 ),
 .UNSPECIFIED. ) ;
#178048 = CARTESIAN_POINT ( 'NONE',  ( 4.259493880088534468, 0.8231460567260719952, 1.533345966155388540 ) ) ;
#178049 = CARTESIAN_POINT ( 'NONE',  ( 9.562578416340237197, 10.05076299535211781, 0.7998128361456462443 ) ) ;
#178050 = CARTESIAN_POINT ( 'NONE',  ( 4.059675810253587258, 1.465203325174119664, -0.9266335502581940498 ) ) ;
#178051 = CARTESIAN_POINT ( 'NONE',  ( 5.231008634329041840, -2.042658762482005841, -0.7362343983412369397 ) ) ;
#178052 = CARTESIAN_POINT ( 'NONE',  ( 3.602716132929354664, 5.226254793216122074, 1.599625672291267398 ) ) ;
#178053 = CARTESIAN_POINT ( 'NONE',  ( 5.594935472981866553, 1.780666063871166882, 0.9463038388278843804 ) ) ;
#178054 = CARTESIAN_POINT ( 'NONE',  ( 5.062500000000005329, -1.451031289061317064, -1.451031289060909168 ) ) ;
#178055 = DIRECTION ( 'NONE',  ( 2.949029909160572061E-17, 1.000000000000000000, -8.673600428462354978E-15 ) ) ;
#178056 = CARTESIAN_POINT ( 'NONE',  ( 2.766527970621732724, -1.329674337952547303, 1.394112488825666851 ) ) ;
#178057 = CARTESIAN_POINT ( 'NONE',  ( -0.7500000000000006661, 9.239583334016129967, -1.299038105676657340 ) ) ;
#178058 = CARTESIAN_POINT ( 'NONE',  ( 6.433822955411669930, -2.155103329387221933, 0.5382066023030105395 ) ) ;
#178059 = ORIENTED_EDGE ( 'NONE', *, *, #195779, .T. ) ;
#178060 = CARTESIAN_POINT ( 'NONE',  ( 6.883263157960371359, 7.052674735402435502, 2.544342468817725855 ) ) ;
#178061 = CARTESIAN_POINT ( 'NONE',  ( -1.500000000000013101, 3.379166666666691299, -0.8660254037844313801 ) ) ;
#178062 = CARTESIAN_POINT ( 'NONE',  ( 6.335737856287750880, 6.286115675290828264, -0.7998128361456281477 ) ) ;
#178063 = CARTESIAN_POINT ( 'NONE',  ( 3.018465837578692579, -2.218647833171137673, 0.1111532960578337226 ) ) ;
#178064 = CARTESIAN_POINT ( 'NONE',  ( -0.02900071798685524560, -0.004641455105012376459, -2.173770343569726649 ) ) ;
#178065 = CARTESIAN_POINT ( 'NONE',  ( 6.141480397310468575, 10.10888486359680982, 1.040834085586084257E-14 ) ) ;
#178066 = CARTESIAN_POINT ( 'NONE',  ( -8.622622508166983835, 13.00355065959610279, 1.040834085586084257E-14 ) ) ;
#178067 = CIRCLE ( 'NONE', #63792, 11.05000000000000426 ) ;
#178068 = CARTESIAN_POINT ( 'NONE',  ( 3.054329744828568227, 6.785411478933790264, 0.000000000000000000 ) ) ;
#178069 = CARTESIAN_POINT ( 'NONE',  ( 1.143204175302305670, 0.8197749522141674072, 1.842446510343001442 ) ) ;
#178071 = CARTESIAN_POINT ( 'NONE',  ( 5.652800580869365099, -0.4976084531597444460, -2.001653870753268283 ) ) ;
#178070 = CARTESIAN_POINT ( 'NONE',  ( 9.576136569953906275, 10.06658084123472641, 0.000000000000000000 ) ) ;
#178072 = FACE_OUTER_BOUND ( 'NONE', #18760, .T. ) ;
#178073 = CARTESIAN_POINT ( 'NONE',  ( -4.223528545856940042, 4.886203710709899006, -1.199719254218446718 ) ) ;
#178074 = CIRCLE ( 'NONE', #22494, 0.04999999999999991257 ) ;
#178075 = CARTESIAN_POINT ( 'NONE',  ( -1.500000000000011324, 5.160416667349487341, -0.8660254037844313801 ) ) ;
#178076 = CARTESIAN_POINT ( 'NONE',  ( 1.364683531249988757, 1.634375000341421691, 0.000000000000000000 ) ) ;
#178077 = CARTESIAN_POINT ( 'NONE',  ( 0.3152201331171593512, -1.737291786998166332, 0.3363950369540784080 ) ) ;
#178078 = CARTESIAN_POINT ( 'NONE',  ( 5.520041967268690897, -1.564255855279505836, 0.7489400339724672229 ) ) ;
#178079 = CARTESIAN_POINT ( 'NONE',  ( 6.110887277445514520, -0.2035749799894230883, 1.728432721540203998 ) ) ;
#178080 = B_SPLINE_CURVE_WITH_KNOTS ( 'NONE', 3,
 ( #111839, #178912, #160513, #61950, #59811, #130225, #159443, #112901, #125966, #12116, #179969, #9985, #44649, #46787, #113972, #144316 ),
 .UNSPECIFIED., .F., .F.,
 ( 4, 3, 3, 3, 3, 4 ),
 ( 5.987702205360377997E-19, 5.045320844149813800E-05, 9.514731479431012807E-05, 0.0001285019506257865799, 0.0001554096905453329267, 0.0001737658007497178494 ),
 .UNSPECIFIED. ) ;
#178081 = CARTESIAN_POINT ( 'NONE',  ( 3.316269524717931017, 1.452881069417772730, -1.773186822121583184 ) ) ;
#178082 = CARTESIAN_POINT ( 'NONE',  ( 0.6823417656249882723, 0.1760416670080894308, -1.181850606188749264 ) ) ;
#178083 = CARTESIAN_POINT ( 'NONE',  ( 1.200829095903386046, -0.4490931065196464012, 1.785404219219708377 ) ) ;
#178084 = CARTESIAN_POINT ( 'NONE',  ( -0.4500000000000409228, 3.999999999999974243, 0.8338124244295310739 ) ) ;
#178085 = CARTESIAN_POINT ( 'NONE',  ( -10.62722285141355094, 4.751451743136023254, 5.577054254164887759 ) ) ;
#178086 = CARTESIAN_POINT ( 'NONE',  ( 1.694096453153286497, -1.816434584207878622, -0.1825648128309723117 ) ) ;
#178087 = CARTESIAN_POINT ( 'NONE',  ( 2.971327447312217984, -1.987046587055636637, -0.3419355124290662240 ) ) ;
#178088 = CARTESIAN_POINT ( 'NONE',  ( 0.9025786099917804117, 1.657183926254527595, -1.434042119274607563 ) ) ;
#178089 = CARTESIAN_POINT ( 'NONE',  ( 9.599742726594369557, 13.73983281947659840, -8.263962686181493211 ) ) ;
#178090 = CARTESIAN_POINT ( 'NONE',  ( 4.102637100452250607, -0.6586339671014628250, -2.000395093806975222 ) ) ;
#178091 = CARTESIAN_POINT ( 'NONE',  ( -6.039267359883488950, 9.133230122250985517, 1.199719254218452047 ) ) ;
#178092 = CARTESIAN_POINT ( 'NONE',  ( 6.939993127879787060, 13.99500908125960663, 9.397576848110693604 ) ) ;
#178093 = CONICAL_SURFACE ( 'NONE', #174558, 1.219999999999999751, 0.7853981633974463916 ) ;
#178094 = CARTESIAN_POINT ( 'NONE',  ( 1.662640112210824306, -0.7432673875312334477, -1.932532381715674097 ) ) ;
#178095 = CARTESIAN_POINT ( 'NONE',  ( 6.491656622844908853, 6.468020902940851968, 0.7998128361456341429 ) ) ;
#178096 = CARTESIAN_POINT ( 'NONE',  ( -0.6801582343750022241, -0.6197916663252672764, -1.178068619123841643 ) ) ;
#178097 = CARTESIAN_POINT ( 'NONE',  ( 4.354221869268804390, 0.9056986662851628234, -1.917456963280273818 ) ) ;
#178098 = CARTESIAN_POINT ( 'NONE',  ( 0.04732232356348483465, -1.488192626783080952, -1.223051670295220994 ) ) ;
#178099 = ORIENTED_EDGE ( 'NONE', *, *, #18312, .F. ) ;
#178100 = CARTESIAN_POINT ( 'NONE',  ( -3.969505113751027547, 7.853116076009993840, 1.214306433183764966E-14 ) ) ;
#178101 = EDGE_CURVE ( 'NONE', #144460, #58716, #83440, .T. ) ;
#178102 = CARTESIAN_POINT ( 'NONE',  ( -11.44791656467458552, 11.29999999999999716, -3.303228920649581291 ) ) ;
#178103 = CARTESIAN_POINT ( 'NONE',  ( 6.333067150914816423, 7.521571443223021625, 1.082531754730549967 ) ) ;
#178104 = CARTESIAN_POINT ( 'NONE',  ( 3.475000000000000533, -1.881249999044085186, 0.000000000000000000 ) ) ;
#178105 = CARTESIAN_POINT ( 'NONE',  ( -5.901876940650454095, 5.779944607047298177, -0.7998128361456291469 ) ) ;
#178106 = CARTESIAN_POINT ( 'NONE',  ( -0.1575499713504755483, -1.374138184231291415, -1.746309953600865716 ) ) ;
#178107 = CARTESIAN_POINT ( 'NONE',  ( 0.7101633350218137242, -2.095805943121428427, 0.2063731196077517871 ) ) ;
#178108 = CARTESIAN_POINT ( 'NONE',  ( -6.330731382938325602, 6.350551133041632212, 0.7998128361456281477 ) ) ;
#178109 = CARTESIAN_POINT ( 'NONE',  ( 8.540746701604824409, 12.05162268759261224, -1.199719254218446718 ) ) ;
#178110 = CARTESIAN_POINT ( 'NONE',  ( 4.821077630544555070, -1.661119493813640657, -0.8391380156763434961 ) ) ;
#178111 = CARTESIAN_POINT ( 'NONE',  ( 7.377608144130607393, 11.75895993479440982, -0.7998128361456291469 ) ) ;
#178112 = CARTESIAN_POINT ( 'NONE',  ( 4.143606928732548766, 3.973957532277850646, -0.5173101462927472971 ) ) ;
#178113 = ORIENTED_EDGE ( 'NONE', *, *, #72642, .T. ) ;
#178114 = CARTESIAN_POINT ( 'NONE',  ( -3.797165540279144214, 6.587721009371067638, 1.199719254218452935 ) ) ;
#178115 = CARTESIAN_POINT ( 'NONE',  ( -8.839552966430002101, 12.29626697993494666, -1.082531754730543971 ) ) ;
#178117 = CARTESIAN_POINT ( 'NONE',  ( 2.488659587246494276, 1.902222718079676689, 0.4795239450603656084 ) ) ;
#178116 = CARTESIAN_POINT ( 'NONE',  ( -6.073162743917628781, 9.172774736957510555, -1.199719254218440723 ) ) ;
#178118 = CARTESIAN_POINT ( 'NONE',  ( 1.059701713109785670, 0.4209238396889224965, -2.120155868012041811 ) ) ;
#178120 = CARTESIAN_POINT ( 'NONE',  ( -5.679923764332232672, 6.292470487948599533, 1.134535232271353999 ) ) ;
#178119 = CARTESIAN_POINT ( 'NONE',  ( -4.613517410400161722, 8.604463755433990002, -0.7998128361456362523 ) ) ;
#178121 = CARTESIAN_POINT ( 'NONE',  ( -1.402160292154681736E-14, 0.1968750003414221628, -1.575800808251665908 ) ) ;
#178122 = CARTESIAN_POINT ( 'NONE',  ( 2.442404235307413796, 1.063479746408531046, 1.369289251230455751 ) ) ;
#178123 = CARTESIAN_POINT ( 'NONE',  ( 2.642201187982503363, -1.446964261146063802, 0.9666251106823405825 ) ) ;
#178124 = CARTESIAN_POINT ( 'NONE',  ( 7.971831135155394321, 8.402817200543854170, -0.7216878364870267237 ) ) ;
#178125 = CARTESIAN_POINT ( 'NONE',  ( -10.45911050446410506, 5.175404930453152197, 5.201426885097844455 ) ) ;
#178126 = CARTESIAN_POINT ( 'NONE',  ( 2.020846523693183627, 1.921700534952670791, 0.7446803044362272361 ) ) ;
#178127 = CARTESIAN_POINT ( 'NONE',  ( 1.440779594245532369, 1.198675164295496920, 1.620935466883965503 ) ) ;
#178128 = CARTESIAN_POINT ( 'NONE',  ( 6.925078400183534377, -0.01048729610059369148, 2.244148362790527429 ) ) ;
#178129 = CARTESIAN_POINT ( 'NONE',  ( -5.808742468812186033, 5.741564066561132940, 0.000000000000000000 ) ) ;
#178130 = CARTESIAN_POINT ( 'NONE',  ( 1.129686040349969556, -1.248873030102001902, -1.525460987127578605 ) ) ;
#178131 = STYLED_ITEM ( 'NONE', ( #108369 ), #86095 ) ;
#178133 = CARTESIAN_POINT ( 'NONE',  ( -4.990809943606269172, 8.836712344267034780, -0.7216878364870338292 ) ) ;
#178132 = CARTESIAN_POINT ( 'NONE',  ( 5.396708386617175890, -1.867154475869851504, -0.4128305108781898936 ) ) ;
#178134 = CARTESIAN_POINT ( 'NONE',  ( -7.729556973122450714, 8.190440354830551328, 0.000000000000000000 ) ) ;
#178135 = CARTESIAN_POINT ( 'NONE',  ( 5.840530312436913007, 10.03597880781023299, 0.000000000000000000 ) ) ;
#178136 = CARTESIAN_POINT ( 'NONE',  ( -5.447343857640614573, 9.577261277214532242, -0.7998128361456362523 ) ) ;
#178137 = CARTESIAN_POINT ( 'NONE',  ( 1.313155450441779726, 1.649776782055782709, -1.164742093282441937 ) ) ;
#178138 = CARTESIAN_POINT ( 'NONE',  ( 0.4999999999999709677, 3.949999999999967315, 0.4499999999999590994 ) ) ;
#178139 = EDGE_CURVE ( 'NONE', #111937, #155317, #140539, .T. ) ;
#178140 = CARTESIAN_POINT ( 'NONE',  ( 4.489522129203258771, 2.063289974401757654, -1.033470928033096037 ) ) ;
#178141 = CARTESIAN_POINT ( 'NONE',  ( 5.740667459973674447, -1.913685094937540132, -0.4313615418530327150 ) ) ;
#178142 = CARTESIAN_POINT ( 'NONE',  ( 1.903102209365503894, -1.660057620245494636, 1.045011325395063251 ) ) ;
#178143 = CARTESIAN_POINT ( 'NONE',  ( 9.073431116043567002, 11.60875560684942265, -1.599625672291262513 ) ) ;
#178144 = CARTESIAN_POINT ( 'NONE',  ( -0.08726289061519039436, -1.242903867559573161, -1.588418431006669351 ) ) ;
#178145 = ORIENTED_EDGE ( 'NONE', *, *, #181839, .T. ) ;
#178146 = CARTESIAN_POINT ( 'NONE',  ( 1.393934723748765814, -2.100642827862955198, 0.2651745403093440090 ) ) ;
#178148 = CARTESIAN_POINT ( 'NONE',  ( -7.832860060393135093, 10.16142270859057462, 1.599625672291295375 ) ) ;
#178147 = CARTESIAN_POINT ( 'NONE',  ( -4.406563619641430840, 5.099744630125142564, -1.199719254218446718 ) ) ;
#178149 = CARTESIAN_POINT ( 'NONE',  ( 0.7965151530783078915, 1.503791256141374211, 1.061989520254283281 ) ) ;
#178150 = ORIENTED_EDGE ( 'NONE', *, *, #116730, .T. ) ;
#178151 = CARTESIAN_POINT ( 'NONE',  ( 11.87811798030312005, 7.788899244876387407, 1.760824057802017784 ) ) ;
#178152 = CARTESIAN_POINT ( 'NONE',  ( 2.707414796094851361, 1.816601298730673220, -1.093838055662835096 ) ) ;
#178153 = B_SPLINE_CURVE_WITH_KNOTS ( 'NONE', 3,
 ( #184162, #35783, #180974, #101859, #199335, #19526, #83467, #66122, #151691, #167927, #50981, #3260, #117103, #69328, #49915, #116036, #135439, #201460, #17383, #149546, #53104, #81348, #119237, #185220, #163679, #147428, #106180, #40069, #139721, #121394, #6467, #172205, #124599, #154883, #71464, #8614, #37929, #152740, #23795, #168988, #88828, #123540, #72543, #137577, #89900, #104003, #157028, #155952, #170047, #153816, #203595, #21632, #120317, #70391, #7537, #73621, #55247, #36844, #20587, #204664, #205744, #87740, #5387, #57376, #74696, #188435, #189504, #41150, #202528, #107259, #138641, #173279, #22714, #54177, #24861, #90962, #56313, #122474, #140800, #38997, #206811, #105082, #58445, #102926, #187367, #86673, #171120, #136508, #4321, #186292, #92038, #45410, #190559, #80016, #42215, #208933, #111527, #158095, #108331, #46469, #12869, #207878, #174351, #44341, #60567, #191620, #194835, #109403, #28076, #175409, #59501, #30213, #128854, #43282, #161283, #10742, #94170, #110463, #145067, #146119, #212132, #78942, #211070, #112592, #126726, #125658, #192687, #176463, #162353, #127810, #26992, #25930, #93099, #9683, #141869, #63768, #159140, #193764, #76813, #177533, #142932, #61642, #29145, #178604, #160210, #11811, #75760, #95234, #77887, #62693, #144008, #210000, #96298, #13933, #18204, #134146, #130977, #98410, #166614, #101608, #66937, #164474, #14995, #167675, #183920, #16061, #81088, #34468, #82145, #84288, #33402, #1944, #179667, #148237, #147176, #133079, #198028, #99481, #149291, #114723, #31286, #151440, #196968, #100539, #199077, #68006, #51808, #35532, #150374, #200154, #872, #48605, #115780, #50723, #214239, #116848, #213202, #129927, #49657, #65869, #180720, #132018, #83208, #117926, #181769, #97362, #163420, #182849, #19276, #165539, #17132, #113663, #85358, #3011, #195915, #32344, #47552, #64831, #205497, #87506, #152495, #23540, #104831, #73361, #170876, #69081, #71215, #137332, #139467, #20344, #203348, #118992, #107004, #38749, #55001, #121152, #171951, #22468, #173029, #56067, #120069, #136260, #202280, #204413, #153570, #138395, #72287, #89649, #5139, #88579, #122224, #156782, #187117, #103757, #40899, #70149, #184971, #188184, #201218, #154637, #39819, #6218, #105927, #155703, #7284, #57130, #123297, #36596, #102683, #189260, #24611, #90719, #135201, #52859, #168741, #86430, #4078, #186045, #53933, #37680, #169806, #21395, #210566, #180217, #47033, #15550, #113148, #8368, #13432, #79508, #81637, #174110, #145626, #58196, #49156, #195403, #211623, #63258, #114218, #179154, #115272, #196464, #31839, #128356, #78436, #25682, #129420, #30778, #96857, #97915, #147722, #74451, #146675, #181265, #62200, #162905, #45966, #144556, #157847, #14487, #163974, #80577, #212690, #12357, #194324, #213739, #65362, #140555, #64332, #130473, #131509, #112087, #178088, #32891, #48106, #29706, #197512, #206569, #91791, #108081, #98969, #124354, #190312, #41970, #95787, #161844, #68563, #134690, #133633, #50213, #136803, #4618, #51281, #116332, #69629, #199635, #119539, #200694, #37149, #347, #117406, #52345, #135738, #83763, #167166, #38226, #16615, #53401, #186599, #166089, #201760, #19824, #103229, #86973, #70690, #185524, #169289, #184458, #17677, #150927, #36076, #20874, #85909, #118473, #165021, #66420, #18753 ),
 .UNSPECIFIED., .F., .F.,
 ( 4, 1, 1, 1, 1, 1, 1, 1, 1, 1, 1, 1, 1, 1, 1, 1, 1, 1, 1, 1, 1, 1, 1, 1, 1, 1, 1, 1, 1, 1, 1, 1, 1, 1, 1, 1, 1, 1, 1, 1, 1, 1, 1, 1, 1, 1, 1, 1, 1, 1, 1, 1, 1, 1, 1, 1, 1, 1, 1, 1, 1, 1, 1, 1, 1, 1, 1, 1, 1, 1, 1, 1, 1, 1, 1, 1, 1, 1, 1, 1, 1, 1, 1, 1, 1, 1, 1, 1, 1, 1, 1, 1, 1, 1, 1, 1, 1, 1, 1, 1, 1, 1, 1, 1, 1, 1, 1, 1, 1, 1, 1, 1, 1, 1, 1, 1, 1, 1, 1, 1, 1, 1, 1, 1, 1, 1, 1, 1, 1, 1, 1, 1, 1, 1, 1, 1, 1, 1, 1, 1, 1, 1, 1, 1, 1, 1, 1, 1, 1, 1, 1, 1, 1, 1, 1, 1, 1, 1, 1, 1, 1, 1, 1, 1, 1, 1, 1, 1, 1, 1, 1, 1, 1, 1, 1, 1, 1, 1, 1, 1, 1, 1, 1, 1, 1, 1, 1, 1, 1, 1, 1, 1, 1, 1, 1, 1, 1, 1, 1, 1, 1, 1, 1, 1, 1, 1, 1, 1, 1, 1, 1, 1, 1, 1, 1, 1, 1, 1, 1, 1, 1, 1, 1, 1, 1, 1, 1, 1, 1, 1, 1, 1, 1, 1, 1, 1, 1, 1, 1, 1, 1, 1, 1, 1, 1, 1, 1, 1, 1, 1, 1, 1, 1, 1, 1, 1, 1, 1, 1, 1, 1, 1, 1, 1, 1, 1, 1, 1, 1, 1, 1, 1, 1, 1, 1, 1, 1, 1, 1, 1, 1, 1, 1, 1, 1, 1, 1, 1, 1, 1, 1, 1, 1, 1, 1, 1, 1, 1, 1, 1, 1, 1, 1, 1, 1, 1, 1, 1, 1, 1, 1, 1, 1, 1, 1, 1, 1, 1, 1, 1, 1, 1, 1, 1, 1, 1, 1, 1, 1, 1, 1, 1, 1, 1, 1, 1, 1, 1, 1, 1, 1, 1, 1, 1, 1, 1, 1, 1, 1, 1, 1, 1, 1, 1, 1, 1, 1, 1, 1, 1, 1, 1, 1, 1, 1, 1, 1, 1, 1, 1, 1, 1, 1, 1, 1, 1, 1, 1, 1, 1, 1, 1, 1, 1, 4 ),
 ( 0.000000000000000000, 0.002599888508634240914, 0.005208754120092145765, 0.007813069968323356138, 0.01041690100177071650, 0.01302019566086259385, 0.01562517182793091500, 0.01822893254318404960, 0.02083328139698771564, 0.02343764900838959594, 0.02604139750447371365, 0.02864615928571910553, 0.03124958462592061434, 0.03385442086835698666, 0.03645794792899405279, 0.03906256697173399878, 0.04166661757251870907, 0.04427067912273281725, 0.04687528696281444140, 0.04947881815967773017, 0.05208365228821221909, 0.05468707701066444909, 0.05729184299815447134, 0.05989557646906591704, 0.06249996333325048142, 0.06510433798480201595, 0.06770807906337909798, 0.07031283757201339801, 0.07291626355048291819, 0.07552109983967189577, 0.07812462590386089201, 0.08072924387304455940, 0.08333329402460390445, 0.08593735478041557296, 0.08854196204427712547, 0.09114549249794960672, 0.09375032597506528786, 0.09635375006294695510, 0.09895851527076646170, 0.1015622481948881828, 0.1041666342325376776, 0.1067710083972730206, 0.1093747487337090180, 0.1119795066911244419, 0.1145829320296284648, 0.1171877676425944481, 0.1197912931610935483, 0.1223959103579086161, 0.1249999600491941698, 0.1276040200539713398, 0.1302086268569593308, 0.1328121566649932417, 0.1354169895755736042, 0.1380204131161003600, 0.1406251776355303407, 0.1432289101024236955, 0.1458332954032181272, 0.1484376691708411133, 0.1510414088543486633, 0.1536461663508109643, 0.1562495911381983071, 0.1588544261652600487, 0.1614579512270202244, 0.1640625677415503691, 0.1666666170620310916, 0.1692706764052687440, 0.1718752828374313091, 0.1744788120887783289, 0.1770836445231302458, 0.1796870676051354199, 0.1822918315264069888, 0.1848955636252137269, 0.1874999482789682093, 0.1901043217392619777, 0.1927080608589964439, 0.1953128179847096746, 0.1979162423098047296, 0.2005210768412587219, 0.2031246015352002054, 0.2057292174574958665, 0.2083332664966131842, 0.2109373252677763377, 0.2135419314191336626, 0.2161454602027163274, 0.2187502922511180836, 0.2213537149634070833, 0.2239584783767220588, 0.2265622101965570623, 0.2291665942930569411, 0.2317709675357785548, 0.2343747061808670040, 0.2369794630260087243, 0.2395828869776091552, 0.2421877211037245237, 0.2447912455187418734, 0.2473958609388257068, 0.2499999097859964270, 0.2526039680745227334, 0.2552085740350705789, 0.2578121024397855843, 0.2604169341924902348, 0.2630203566238439872, 0.2656251196193780695, 0.2682288512493328225, 0.2708332348783377697, 0.2734376079932215875, 0.2760413462527663842, 0.2786461029074911444, 0.2812495265743710227, 0.2838543603853929120, 0.2864578846103582599, 0.2890624996182282747, 0.2916665483628478883, 0.2942706062581511572, 0.2968752121178640513, 0.2994787402325856385, 0.3020835717798243114, 0.3046869940190023440, 0.3072917566869088346, 0.3098954882160545599, 0.3124998714673014044, 0.3151042445440625506, 0.3177079825071445485, 0.3203127390615869707, 0.3229161625325003282, 0.3255209961186533163, 0.3281245202424198926, 0.3307291349280532256, 0.3333331836594992104, 0.3359372412509727956, 0.3385418470998076690, 0.3411453750133909280, 0.3437502064453764050, 0.3463536285811206206, 0.3489583910115333087, 0.3515621225289245477, 0.3541665054921307454, 0.3567708786204680238, 0.3593746163761498691, 0.3619793729204284771, 0.3645827962841124981, 0.3671876297356038710, 0.3697911538470093351, 0.3723957683003653041, 0.3749998171080005105, 0.3776038744850206963, 0.3802084804129200468, 0.3828120082142042468, 0.3854168396211344327, 0.3880202617421720235, 0.3906250240252089334, 0.3932287556198868494, 0.3958331383847540352, 0.3984375116543538153, 0.4010412492916836102, 0.4036460059159037717, 0.4062494292610819846, 0.4088542626681055392, 0.4114577868559751161, 0.4140624011669984950, 0.4166664501401745602, 0.4192705073921035863, 0.4218751134889988097, 0.4244786412668108966, 0.4270834727388717056, 0.4296868949339185950, 0.4322916571596854274, 0.4348953889206810253, 0.4374997715768980666, 0.4401041450774376140, 0.4427078826854516369, 0.4453126394797092824, 0.4479160628950952239, 0.4505208963478340434, 0.4531244207009840763, 0.4557290349596088697, 0.4583330841876695483, 0.4609371414038593850, 0.4635417477596745495, 0.4661452756028321986, 0.4687501072302013849, 0.4713535295879656695, 0.4739582918465587991, 0.4765620238628961447, 0.4791664065001429718, 0.4817707803212932793, 0.4843745179890200370, 0.4869792750434049911, 0.4895826986177053142, 0.4921875322063354874, 0.4947910568135764908, 0.4973956711097291539, 0.4999997206820134821, 0.5026037779518089943, 0.5052083846564635605, 0.5078119126537786743, 0.5104167445266291070, 0.5130201671358142201, 0.5156249295173244152, 0.5182286618780244103, 0.5208330445859747915, 0.5234374188174044651, 0.5260411566338674128, 0.5286459140384663913, 0.5312493378603841965, 0.5338541716750782040, 0.5364576966252184720, 0.5390623110488209635, 0.5416663610546670338, 0.5442704184674093115, 0.5468750256108222407, 0.5494785538511040013, 0.5520833860596070508, 0.5546868090089153158, 0.5572915716034309019, 0.5598953043975141153, 0.5624996872658396541, 0.5651040619972180767, 0.5677078000514395040, 0.5703125578963399445, 0.5729159820545779436, 0.5755208161855079885, 0.5781243415673570363, 0.5807289562083304268, 0.5833330067370782190, 0.5859370643821081304, 0.5885416720542003821, 0.5911452006262593040, 0.5937500332605881725, 0.5963534566387238556, 0.5989582195363342132, 0.6015619528528246551, 0.6041663359711972880, 0.6067707112921981727, 0.6093744496732020899, 0.6119792080484952601, 0.6145826326317597177, 0.6171874671691013337, 0.6197909930714722293, 0.6223956080197403651, 0.6249996591607356322, 0.6276037171273963766, 0.6302083254180952387, 0.6328118544107458332, 0.6354166875610788301, 0.6380201114567515264, 0.6406248747475506988, 0.6432286086754787080, 0.6458329921335752566, 0.6484373681338796436, 0.6510411069306952792, 0.6536458659264798854, 0.6562492910234830612, 0.6588541260574176661, 0.6614576525691320263, 0.6640622679146246377, 0.6666663197572214594, 0.6692703781348633418, 0.6718749871341050950, 0.6744785166361690898, 0.6770833503926931840, 0.6796867748946214816, 0.6822915386687108397, 0.6848952732971168578, 0.6874996571846213600, 0.6901040339539210589, 0.6927077732555863010, 0.6953125329619718187, 0.6979159586614360755, 0.7005207942821553013, 0.7031243214920454010, 0.7057289373247008779, 0.7083329899582661016, 0.7109370488362486418, 0.7135416586339821121, 0.7161451887342924483, 0.7187500231872065992, 0.7213534483841206324, 0.7239582127316128712, 0.7265619481495508847, 0.7291663325561579256, 0.7317707101841592898, 0.7343744500797240171, 0.7369792105868335774, 0.7395826369774940456, 0.7421874732752028470, 0.7447910012721150608, 0.7473956176818850050, 0.7499996711958007989, 0.7526037306634962842, 0.7552083413496862851, 0.7578118721370898925, 0.7604167073766084917, 0.7630201333572542710, 0.7656248983682768516, 0.7682286346648167230, 0.7708330196802359868, 0.7734373982566630223, 0.7760411388351919904, 0.7786459002331664880, 0.7812493274037752844, 0.7838541644686951582, 0.7864576933414935134, 0.7890623104183455139, 0.7916663649020125870, 0.7942704250488100692, 0.7968750367134410650, 0.7994785682768023038, 0.8020834043931583945, 0.8046868312463003603, 0.8072915970109983963, 0.8098953342752303053, 0.8124997199891885735, 0.8151040996037859365, 0.8177078409543626636, 0.8203126033333638656, 0.8229160313726919806, 0.8255208692950642968, 0.8281243991326340259, 0.8307290169665545454, 0.8333330725093962554, 0.8359371334247044372, 0.8385417461577832077, 0.8411452785859873105, 0.8437501156694361404, 0.8463535434838604932, 0.8489583100924004144, 0.8515620484134380774, 0.8541664349156833369, 0.8567708156582201084, 0.8593745578699503174, 0.8619793213201638604, 0.8645827503170061545, 0.8671875891870957087, 0.8697911200783463581, 0.8723957387593448409, 0.8749997954508100806, 0.8776038572240605351, 0.8802084711156200614, 0.8828120044975765746, 0.8854168426383988155, 0.8880202715029178462, 0.8906250390454908406, 0.8932287785124739532, 0.8958331658927787267, 0.8984375478530519654, 0.9010412910150662480, 0.9036460556267057465, 0.9062494856698833923, 0.9088543255779816255, 0.9114578576118502751, 0.9140624772299625889, 0.9166665351595286726, 0.9192705978801787303, 0.9218752130202838568, 0.9244787474449313036, 0.9270835867334279445, 0.9296870167368762594, 0.9322917853037333558, 0.9348955260058576799, 0.9374999143539141100, 0.9401042976215825409, 0.9427080418234272674, 0.9453128076877782560, 0.9479162388645026027, 0.9505210798953250828, 0.9531246131693177359, 0.9557292338404025367, 0.9583332930514818493, 0.9609373567081632705, 0.9635419734050364449, 0.9661455093234165847, 0.9687503490003109841, 0.9713537788664922124, 0.9739585512809396661, 0.9765622998769101226, 0.9791666815729623830, 0.9817710277688282972, 0.9843747994658795797, 0.9869797739623470401, 0.9895830763955310028, 0.9921869177308453303, 0.9947912343601759133, 0.9974001139318913189, 1.000000000000000000 ),
 .UNSPECIFIED. ) ;
#178154 = CARTESIAN_POINT ( 'NONE',  ( -1.500000000000011324, 4.952083334016150751, 0.8660254037844403729 ) ) ;
#178155 = CARTESIAN_POINT ( 'NONE',  ( 7.052212457402625922, 11.37933163361175382, -0.7998128361456291469 ) ) ;
#178156 = DIRECTION ( 'NONE',  ( 0.000000000000000000, -1.000000000000000000, 0.000000000000000000 ) ) ;
#178157 = CARTESIAN_POINT ( 'NONE',  ( 3.180987545930415106, -0.1479678519747235910, -2.055505606019301990 ) ) ;
#178159 = DIRECTION ( 'NONE',  ( 1.214306433183764966E-17, 1.000000000000000000, 5.200010849845536803E-32 ) ) ;
#178158 = CARTESIAN_POINT ( 'NONE',  ( -7.018317073368468328, 11.33978701890523233, -0.7998128361456291469 ) ) ;
#178160 = CARTESIAN_POINT ( 'NONE',  ( -1.201851678989727383E-14, 3.946875000341423689, -1.575800808251660134 ) ) ;
#178161 = CARTESIAN_POINT ( 'NONE',  ( 0.3423093779009924731, 3.000000000000002665, -0.3423093779010306092 ) ) ;
#178162 = CARTESIAN_POINT ( 'NONE',  ( 1.272106862006046057, 3.977462442649445151, 0.4878970607599459886 ) ) ;
#178163 = DIRECTION ( 'NONE',  ( -0.000000000000000000, -1.000000000000000000, -0.000000000000000000 ) ) ;
#178164 = CARTESIAN_POINT ( 'NONE',  ( 2.548426268707996822, 2.261836392764454473, 0.05785012348054861114 ) ) ;
#178165 = CARTESIAN_POINT ( 'NONE',  ( -9.653042183249970876, 11.32459930428888306, -1.082531754730539753 ) ) ;
#178166 = CARTESIAN_POINT ( 'NONE',  ( 2.074188967152798657, 0.7772732722058082189, 1.636524323399509928 ) ) ;
#178167 = CARTESIAN_POINT ( 'NONE',  ( 2.008866915445167045, 0.004233813517278902337, 1.915903396628533706 ) ) ;
#178168 = CARTESIAN_POINT ( 'NONE',  ( 2.893098739488662030, 0.2508700648995808025, 2.055025655848155886 ) ) ;
#178169 = CARTESIAN_POINT ( 'NONE',  ( -0.6823417656250212460, 3.113541667008084879, 1.181850606188767472 ) ) ;
#178170 = CARTESIAN_POINT ( 'NONE',  ( 1.903138372489954655, 1.638015138609005383, 1.096796735940619660 ) ) ;
#178171 = CARTESIAN_POINT ( 'NONE',  ( 6.164670984062957437, -1.360496472042394656, 1.364235590486153837 ) ) ;
#178172 = CARTESIAN_POINT ( 'NONE',  ( 3.309304339999539657, -0.3661640501408692794, 1.834289908569000538 ) ) ;
#178173 = EDGE_CURVE ( 'NONE', #124966, #213513, #205458, .T. ) ;
#178175 = CARTESIAN_POINT ( 'NONE',  ( 4.596911992430688265, 8.487755744900498556, -0.08351877912710949092 ) ) ;
#178174 = CARTESIAN_POINT ( 'NONE',  ( 1.014821436393667398, -1.042085040243752481, -2.059081925104982336 ) ) ;
#178176 = CARTESIAN_POINT ( 'NONE',  ( 2.611566863951066519, 0.4996721132001956112, -1.792629727676842144 ) ) ;
#178177 = CARTESIAN_POINT ( 'NONE',  ( 0.6823417656249882723, 2.676041667008084879, -1.181850606188749264 ) ) ;
#178178 = CARTESIAN_POINT ( 'NONE',  ( 5.863753151201884783, -0.5045919461894343705, 1.999881752496771359 ) ) ;
#178179 = CLOSED_SHELL ( 'NONE', ( #69786, #69800, #79500, #177618, #85539, #212878, #81445, #33425 ) ) ;
#178180 = CARTESIAN_POINT ( 'NONE',  ( -4.412288926243578935, 7.235088616337731260, 1.199719254218464037 ) ) ;
#178181 = CARTESIAN_POINT ( 'NONE',  ( 5.940443861082012944, 10.08226827123770697, 0.7998128361456462443 ) ) ;
#178182 = CARTESIAN_POINT ( 'NONE',  ( -1.392936117481092140, 3.541413949887021406, -0.5577005436123527726 ) ) ;
#178183 = CARTESIAN_POINT ( 'NONE',  ( 5.930723256393157783, 2.028624516890007445, 0.5651790528119063906 ) ) ;
#178184 = CARTESIAN_POINT ( 'NONE',  ( -0.6823417656249969321, 4.280208333674755394, -1.181850606188749264 ) ) ;
#178185 = CARTESIAN_POINT ( 'NONE',  ( 5.764953170560049855, -1.951456690425241947, -0.9300186209130756332 ) ) ;
#178186 = CARTESIAN_POINT ( 'NONE',  ( 5.971354884044596467, -1.733367664992270685, -1.036320259733174209 ) ) ;
#178187 = CARTESIAN_POINT ( 'NONE',  ( -1.364683531250000748, -0.7406249996585803075, 0.000000000000000000 ) ) ;
#178188 = CARTESIAN_POINT ( 'NONE',  ( -4.772106882330227506, 7.550913215151819458, -1.082531754730549967 ) ) ;
#178191 = CARTESIAN_POINT ( 'NONE',  ( 4.934804725694211136, 6.780358151441803649, -1.443375672974051449 ) ) ;
#178190 = CARTESIAN_POINT ( 'NONE',  ( -3.285556943750000514, -0.1385416661887106660, -1.896917185911906500 ) ) ;
#178189 = CARTESIAN_POINT ( 'NONE',  ( 7.035755370848908896, 7.173079118937375931, 0.7998128361456352531 ) ) ;
#178192 = CARTESIAN_POINT ( 'NONE',  ( -4.573896719763875574, 6.429575154514868274, -1.599625672291271394 ) ) ;
#178193 = CARTESIAN_POINT ( 'NONE',  ( 4.663296154398564042, 1.879804967172087782, -0.7303043177912388328 ) ) ;
#178195 = B_SPLINE_CURVE_WITH_KNOTS ( 'NONE', 3,
 ( #213133, #81020, #195842, #12801, #13869, #47483 ),
 .UNSPECIFIED., .F., .F.,
 ( 4, 2, 4 ),
 ( 0.3194375178873440357, 0.4097251701830488813, 0.5000128224787536713 ),
 .UNSPECIFIED. ) ;
#178194 = CARTESIAN_POINT ( 'NONE',  ( -7.609150525767646833, 9.900428251527500834, -1.599625672291263179 ) ) ;
#178197 = CARTESIAN_POINT ( 'NONE',  ( -7.227905289416814760, 7.605180057173966723, -0.7216878364870338292 ) ) ;
#178196 = CARTESIAN_POINT ( 'NONE',  ( -8.514157279702020631, 11.91663867875229776, -1.082531754730543971 ) ) ;
#178198 = CARTESIAN_POINT ( 'NONE',  ( 0.6823417656249899377, 5.176041667008086655, -1.181850606188754593 ) ) ;
#178200 = CARTESIAN_POINT ( 'NONE',  ( -0.6823417656250039265, 8.817708333674733723, -1.181850606188755259 ) ) ;
#178199 = CARTESIAN_POINT ( 'NONE',  ( 5.594645800149128156, -0.5210773734287167391, -2.097845705497362712 ) ) ;
#178201 = CARTESIAN_POINT ( 'NONE',  ( -11.94105721237523099, 10.19999999999999929, -1.187919463087249827 ) ) ;
#178202 = CARTESIAN_POINT ( 'NONE',  ( -11.56409840263781597, 7.060128173693748010, 3.212945948728421541 ) ) ;
#178204 = CARTESIAN_POINT ( 'NONE',  ( 0.3334082175802362547, 0.6002418569295930872, -1.819223357073847636 ) ) ;
#178203 = CARTESIAN_POINT ( 'NONE',  ( -5.355107487273497391, 9.191449801886996340, 0.7216878364870458196 ) ) ;
#178205 = CARTESIAN_POINT ( 'NONE',  ( -1.402160292154681736E-14, -0.6156249996585817508, 1.575800808251672791 ) ) ;
#178206 = ADVANCED_FACE ( 'NONE', ( #57091 ), #42998, .F. ) ;
#178207 = CARTESIAN_POINT ( 'NONE',  ( 6.639320575229286092, 4.689090874229541406, 2.765823994384248419 ) ) ;
#178208 = CARTESIAN_POINT ( 'NONE',  ( 1.435739417030171605, 0.8527202394775310612, -1.499263083578871836 ) ) ;
#178209 = CARTESIAN_POINT ( 'NONE',  ( 3.562760505341037831, 7.378580699531681830, -1.734723475976807094E-15 ) ) ;
#178210 = CARTESIAN_POINT ( 'NONE',  ( 7.028976294042106332, 7.165170195996068969, 0.000000000000000000 ) ) ;
#178211 = CARTESIAN_POINT ( 'NONE',  ( -11.41530515461175455, 7.844461421556668590, -3.709416182095576442 ) ) ;
#178212 = CARTESIAN_POINT ( 'NONE',  ( 6.485618507650338316, 1.290063292742931633, 1.354747167150817333 ) ) ;
#178213 = CARTESIAN_POINT ( 'NONE',  ( 1.102198380138383449, -0.9033151347564006839, 1.799099544393264472 ) ) ;
#178214 = PLANE ( 'NONE',  #161335 ) ;
#178215 = CARTESIAN_POINT ( 'NONE',  ( 3.267151830768944443, 4.834763107362302748, -1.443375672974058777 ) ) ;
#178216 = CARTESIAN_POINT ( 'NONE',  ( 3.487540646120320442, 1.995909124301387116, -0.9416478298167814120 ) ) ;
#178217 = CARTESIAN_POINT ( 'NONE',  ( 5.840740439281987051, -2.116473627201011620, -0.4831736825232531007 ) ) ;
#178218 = ORIENTED_EDGE ( 'NONE', *, *, #76938, .F. ) ;
#178219 = CARTESIAN_POINT ( 'NONE',  ( 1.499999999999987566, -0.4749999999999823808, 0.000000000000000000 ) ) ;
#178220 = CARTESIAN_POINT ( 'NONE',  ( 9.205623113554615600, 11.76297960394566466, 1.443375672974076540 ) ) ;
#178222 = CARTESIAN_POINT ( 'NONE',  ( 2.425407844734633223, -1.496065234337567329, -1.352141214786584777 ) ) ;
#178221 = CARTESIAN_POINT ( 'NONE',  ( 3.475340844119988226, -1.870931441966826148, -0.9980012987173056960 ) ) ;
#178224 = ORIENTED_EDGE ( 'NONE', *, *, #141380, .F. ) ;
#178223 = CARTESIAN_POINT ( 'NONE',  ( 1.898416112216103624, -1.777124406008349533, -0.3506645682890742743 ) ) ;
#178225 = CARTESIAN_POINT ( 'NONE',  ( 6.713222337422018349, 7.861122810861019161, -1.199719254218452047 ) ) ;
#178226 = VERTEX_POINT ( 'NONE', #123256 ) ;
#178227 = AXIS2_PLACEMENT_3D ( 'NONE', #75717, #58405, #124560 ) ;
#178228 = CARTESIAN_POINT ( 'NONE',  ( 4.788000803920411386, 8.737751371215816576, 1.040834085586084257E-14 ) ) ;
#178230 = CARTESIAN_POINT ( 'NONE',  ( 1.340887447446635017, -1.644988140609974225, -0.9815275998622545739 ) ) ;
#178229 = CARTESIAN_POINT ( 'NONE',  ( -4.009460741339347045, 5.700790169694431420, -1.599625672291256295 ) ) ;
#178231 = CARTESIAN_POINT ( 'NONE',  ( -11.97929049433705373, 12.22000000000000064, -0.7046979865771834106 ) ) ;
#178232 =( BOUNDED_CURVE ( )  B_SPLINE_CURVE ( 2, ( #35971, #5572, #70578, #71652, #4507, #137766, #39183 ),
 .UNSPECIFIED., .F., .T. ) 
 B_SPLINE_CURVE_WITH_KNOTS ( ( 3, 2, 2, 3 ),
 ( 0.3780836810543342641, 0.3809523809523809312, 0.3869047619047619180, 0.3897734618028085851 ),
 .UNSPECIFIED. ) 
 CURVE ( )  GEOMETRIC_REPRESENTATION_ITEM ( )  RATIONAL_B_SPLINE_CURVE ( ( 0.9331000818465633451, 0.9354320710352566071, 1.000000000000000000, 0.8660254037844387076, 1.000000000000000000, 0.9354320710352564960, 0.9331000818465632340 ) ) 
 REPRESENTATION_ITEM ( '' )  );
#178233 = VECTOR ( 'NONE', #8333, 1000.000000000000000 ) ;
#178234 = CARTESIAN_POINT ( 'NONE',  ( -1.364683531250014514, 0.3427083336747508424, 0.7879004041258379498 ) ) ;
#178235 = CARTESIAN_POINT ( 'NONE',  ( 11.86145016429273191, 10.90000000000000036, 1.099999999999996758 ) ) ;
#178236 = CARTESIAN_POINT ( 'NONE',  ( -10.48453286206953727, 11.12637651536962125, 0.7998128361456462443 ) ) ;
#178237 = CARTESIAN_POINT ( 'NONE',  ( 4.873979933848565871, 1.241796773192262116, 1.769252301715443565 ) ) ;
#178238 = CARTESIAN_POINT ( 'NONE',  ( -5.804299160426249493, 5.944306240018289778, -0.7216878364870338292 ) ) ;
#178239 = EDGE_CURVE ( 'NONE', #164712, #17249, #70146, .T. ) ;
#178240 = CARTESIAN_POINT ( 'NONE',  ( 4.258669648468268676, 7.982548666606070320, 0.7216878364870257245 ) ) ;
#178241 = CARTESIAN_POINT ( 'NONE',  ( 2.672263739372262137, 2.109986773948614225, -0.2121620573234672125 ) ) ;
#178243 = CARTESIAN_POINT ( 'NONE',  ( -11.76695491367977375, 4.673720869072629291, 4.995412848167406494 ) ) ;
#178242 = CARTESIAN_POINT ( 'NONE',  ( -4.888341132428297264, 4.880200397354325759, 0.5250896534725345566 ) ) ;
#178244 = CARTESIAN_POINT ( 'NONE',  ( 3.585193993258027678, 1.783571249345828003, -0.8399556444593555549 ) ) ;
#178245 =( BOUNDED_SURFACE ( )  B_SPLINE_SURFACE ( 3, 3, ( 
 ( #175113, #10443, #46179, #113366, #14703, #110163, #93871, #143709, #45119, #47252 ),
 ( #146887, #142627, #130684, #127504, #212907, #64540, #159909, #79716, #78645, #179371 ),
 ( #209701, #211837, #196673, #112293, #30993, #178309, #11515, #60269, #77586, #126426 ),
 ( #61345, #192389, #193475, #160982, #94933, #111229, #177232, #28845, #144771, #29918 ),
 ( #96000, #12573, #62404, #162054, #13644, #63475, #129629, #195616, #160235, #159166 ),
 ( #94195, #92062, #157054, #76840, #192712, #140827, #211097, #127836, #191644, #29172 ),
 ( #111551, #78973, #175434, #145093, #8643, #77912, #46496, #12894, #10765, #45437 ) ),
 .UNSPECIFIED., .T., .F., .F. ) 
 B_SPLINE_SURFACE_WITH_KNOTS ( ( 4, 3, 4 ),
 ( 4, 1, 1, 1, 1, 1, 1, 4 ),
 ( 0.000000000000000000, 0.5000000000000000000, 1.000000000000000000 ),
 ( 0.000000000000000000, 0.09272347919791326665, 0.1850049962306132278, 0.2567072177207115891, 0.3610482009861257779, 0.5209239196176974618, 0.7336689415868371533, 1.000000000000000000 ),
 .UNSPECIFIED. ) 
 GEOMETRIC_REPRESENTATION_ITEM ( )  RATIONAL_B_SPLINE_SURFACE ( (
 ( 1.000000000000000444, 1.000000000000000444, 1.000000000000000222, 1.000000000000000444, 1.000000000000000222, 1.000000000000000444, 1.000000000000000222, 1.000000000000000222, 1.000000000000000222, 1.000000000000000222),
 ( 0.3333333333333334814, 0.3333333333333335369, 0.3333333333333334814, 0.3333333333333334259, 0.3333333333333334259, 0.3333333333333334259, 0.3333333333333334259, 0.3333333333333334259, 0.3333333333333334259, 0.3333333333333334259),
 ( 0.3333333333333334814, 0.3333333333333335369, 0.3333333333333334814, 0.3333333333333334259, 0.3333333333333334259, 0.3333333333333334259, 0.3333333333333334259, 0.3333333333333334259, 0.3333333333333334259, 0.3333333333333334259),
 ( 1.000000000000000444, 1.000000000000000444, 1.000000000000000222, 1.000000000000000444, 1.000000000000000222, 1.000000000000000444, 1.000000000000000222, 1.000000000000000222, 1.000000000000000222, 1.000000000000000222),
 ( 0.3333333333333334814, 0.3333333333333335369, 0.3333333333333334814, 0.3333333333333334259, 0.3333333333333334259, 0.3333333333333334259, 0.3333333333333334259, 0.3333333333333334259, 0.3333333333333334259, 0.3333333333333334259),
 ( 0.3333333333333334814, 0.3333333333333335369, 0.3333333333333334814, 0.3333333333333334259, 0.3333333333333334259, 0.3333333333333334259, 0.3333333333333334259, 0.3333333333333334259, 0.3333333333333334259, 0.3333333333333334259),
 ( 1.000000000000000444, 1.000000000000000444, 1.000000000000000222, 1.000000000000000444, 1.000000000000000222, 1.000000000000000444, 1.000000000000000222, 1.000000000000000222, 1.000000000000000222, 1.000000000000000222) ) ) 
 REPRESENTATION_ITEM ( '' )  SURFACE ( )  );
#178246 = CARTESIAN_POINT ( 'NONE',  ( 5.326388512780113160, -0.8654452107222168067, -1.705464787417856787 ) ) ;
#178247 = ORIENTED_EDGE ( 'NONE', *, *, #188328, .F. ) ;
#178248 = DIRECTION ( 'NONE',  ( -1.000000000000000000, 0.000000000000000000, 1.665334536937734811E-16 ) ) ;
#178249 = CARTESIAN_POINT ( 'NONE',  ( 0.6079806153083644471, 0.6509857562557037625, -1.965403638620793147 ) ) ;
#178250 = CARTESIAN_POINT ( 'NONE',  ( 3.134642302965468641, -1.712256071497103349, 0.9161664635699683368 ) ) ;
#178251 = ORIENTED_EDGE ( 'NONE', *, *, #110028, .F. ) ;
#178252 = CARTESIAN_POINT ( 'NONE',  ( 2.275435306267621804, 5.643409308550367598, 0.5316758947214432762 ) ) ;
#178254 = CARTESIAN_POINT ( 'NONE',  ( 7.095713291905693332, 9.371694488680407886, 1.599625672291268286 ) ) ;
#178253 = CARTESIAN_POINT ( 'NONE',  ( -5.478903473698241378, 9.406154796041011679, -0.7216878364870338292 ) ) ;
#178256 = CARTESIAN_POINT ( 'NONE',  ( 7.142447996300871793, 7.227277505306155092, 0.7998128361456341429 ) ) ;
#178255 = CARTESIAN_POINT ( 'NONE',  ( 3.029325995398450821, -1.404573224648179242, -1.548692548079745546 ) ) ;
#178257 = CARTESIAN_POINT ( 'NONE',  ( 4.923019175093585886, 5.876515471431535076, -1.082531754730548412 ) ) ;
#178259 = VERTEX_POINT ( 'NONE', #156738 ) ;
#178258 = CARTESIAN_POINT ( 'NONE',  ( -0.07596920688733227456, -0.7732221873907207943, -1.636987988057141852 ) ) ;
#178260 = CARTESIAN_POINT ( 'NONE',  ( 4.002700589841681200, -0.6913439845411989415, -2.095861086919461602 ) ) ;
#178261 = CARTESIAN_POINT ( 'NONE',  ( 3.311752114541001379, -0.4323003076652854326, 2.163846791405985570 ) ) ;
#178262 = CARTESIAN_POINT ( 'NONE',  ( 6.936968151686458306, 11.24487994360957188, 0.7998128361456462443 ) ) ;
#178264 =( BOUNDED_SURFACE ( )  B_SPLINE_SURFACE ( 3, 3, ( 
 ( #146169, #45459, #212184, #180767, #98461, #95286, #149342, #111575, #164525, #82194, #49705 ),
 ( #181820, #921, #66989, #177583, #211120, #62744, #194885, #112644, #178653, #30264, #96350 ),
 ( #70194, #101656, #199126, #167724, #119036, #20391, #182899, #38794, #36645, #104875, #35576 ),
 ( #153616, #121196, #3057, #68052, #69127, #52902, #170918, #136306, #152539, #18252, #150424 ),
 ( #1989, #88625, #51852, #202328, #103803, #19325, #84336, #137377, #87548, #100588, #200199 ),
 ( #4125, #71263, #53978, #187165, #135249, #102729, #120114, #5188, #201262, #168786, #186094 ),
 ( #37724, #169852, #134190, #34515, #117972, #22514, #50770, #154680, #183965, #86475, #85402 ) ),
 .UNSPECIFIED., .T., .F., .F. ) 
 B_SPLINE_SURFACE_WITH_KNOTS ( ( 4, 3, 4 ),
 ( 4, 1, 1, 1, 1, 1, 1, 1, 4 ),
 ( 0.000000000000000000, 0.5000000000000000000, 1.000000000000000000 ),
 ( 0.000000000000000000, 0.2256337125576066971, 0.3978389261578171299, 0.5257960283851228489, 0.6187025735204009225, 0.6856790771877526725, 0.7354782194756434022, 0.7762620033627533056, 0.9999999999999998890 ),
 .UNSPECIFIED. ) 
 GEOMETRIC_REPRESENTATION_ITEM ( )  RATIONAL_B_SPLINE_SURFACE ( (
 ( 1.000000000000000000, 1.000000000000000000, 1.000000000000000222, 1.000000000000000000, 0.9999999999999997780, 1.000000000000000222, 0.9999999999999997780, 1.000000000000000222, 0.9999999999999992228, 1.000000000000000000, 1.000000000000000000),
 ( 0.3333333333333333703, 0.3333333333333334259, 0.3333333333333334259, 0.3333333333333333703, 0.3333333333333333148, 0.3333333333333334259, 0.3333333333333333703, 0.3333333333333334259, 0.3333333333333330928, 0.3333333333333333703, 0.3333333333333333703),
 ( 0.3333333333333333703, 0.3333333333333334259, 0.3333333333333334259, 0.3333333333333333703, 0.3333333333333333148, 0.3333333333333334259, 0.3333333333333333703, 0.3333333333333334259, 0.3333333333333330928, 0.3333333333333333703, 0.3333333333333333703),
 ( 1.000000000000000000, 1.000000000000000000, 1.000000000000000222, 1.000000000000000000, 0.9999999999999997780, 1.000000000000000222, 0.9999999999999997780, 1.000000000000000222, 0.9999999999999992228, 1.000000000000000000, 1.000000000000000000),
 ( 0.3333333333333333703, 0.3333333333333334259, 0.3333333333333334259, 0.3333333333333333703, 0.3333333333333333148, 0.3333333333333334259, 0.3333333333333333703, 0.3333333333333334259, 0.3333333333333330928, 0.3333333333333333703, 0.3333333333333333703),
 ( 0.3333333333333333703, 0.3333333333333334259, 0.3333333333333334259, 0.3333333333333333703, 0.3333333333333333148, 0.3333333333333334259, 0.3333333333333333703, 0.3333333333333334259, 0.3333333333333330928, 0.3333333333333333703, 0.3333333333333333703),
 ( 1.000000000000000000, 1.000000000000000000, 1.000000000000000222, 1.000000000000000000, 0.9999999999999997780, 1.000000000000000222, 0.9999999999999997780, 1.000000000000000222, 0.9999999999999992228, 1.000000000000000000, 1.000000000000000000) ) ) 
 REPRESENTATION_ITEM ( '' )  SURFACE ( )  );
#178263 = FACE_OUTER_BOUND ( 'NONE', #173331, .T. ) ;
#178265 = EDGE_CURVE ( 'NONE', #87461, #35700, #187676, .T. ) ;
#178266 = CARTESIAN_POINT ( 'NONE',  ( 1.559083858985313542, -1.614856622157490929, 1.023943737511850083 ) ) ;
#178267 = CARTESIAN_POINT ( 'NONE',  ( 11.45842088241064793, 13.59306470877039885, -3.566211699757709574 ) ) ;
#178268 = CARTESIAN_POINT ( 'NONE',  ( 4.281733463571851139, -1.982135700070002615, 0.5980053909793591194 ) ) ;
#178269 = AXIS2_PLACEMENT_3D ( 'NONE', #31707, #146546, #163842 ) ;
#178271 = CARTESIAN_POINT ( 'NONE',  ( 3.327187652246216931, 0.05129554954072869377, 2.161254785723889515 ) ) ;
#178270 = CARTESIAN_POINT ( 'NONE',  ( -5.608757509019071108, 5.629766575900002401, 7.500000000000000000 ) ) ;
#178272 = CARTESIAN_POINT ( 'NONE',  ( 4.862908538974716421, 0.2148362657848035262, -2.180980218048253150 ) ) ;
#178273 = CARTESIAN_POINT ( 'NONE',  ( -6.111939103702986209, 6.385007292916157873, 0.4240853425246626229 ) ) ;
#178274 = FACE_OUTER_BOUND ( 'NONE', #9076, .T. ) ;
#178275 = CARTESIAN_POINT ( 'NONE',  ( -0.4942023283147200519, 7.349555083878085426, 1.940391385854319806 ) ) ;
#178276 = CARTESIAN_POINT ( 'NONE',  ( 4.766573523656222555, 7.718696989977711809, 1.199719254218452047 ) ) ;
#178277 = CARTESIAN_POINT ( 'NONE',  ( 1.364683531249996529, 15.27604166700806587, 0.7879004041258405033 ) ) ;
#178278 = CARTESIAN_POINT ( 'NONE',  ( -3.820365424000704557, 7.679119771301277098, -0.7998128361456481317 ) ) ;
#178279 = CARTESIAN_POINT ( 'NONE',  ( 0.2994542103806375200, 1.388483683912977495, -1.462447666687356485 ) ) ;
#178281 = CARTESIAN_POINT ( 'NONE',  ( -8.351459436338037889, 10.76645531385962862, -1.443375672974059665 ) ) ;
#178280 = STYLED_ITEM ( 'NONE', ( #68956 ), #87889 ) ;
#178282 = CARTESIAN_POINT ( 'NONE',  ( 4.170806909802426965, 1.467596682293986765, -1.460439952253207663 ) ) ;
#178283 = CARTESIAN_POINT ( 'NONE',  ( 2.807156881705831442, 1.627618881652561411, 1.030384643589934646 ) ) ;
#178284 = CARTESIAN_POINT ( 'NONE',  ( 5.466459189643565253, -2.065842013452086956, -0.4630074653421185071 ) ) ;
#178285 = CARTESIAN_POINT ( 'NONE',  ( 4.462605117192430804, 8.358123070033169455, 1.040834085586084257E-14 ) ) ;
#178287 = EDGE_CURVE ( 'NONE', #14390, #121817, #28747, .T. ) ;
#178286 = CARTESIAN_POINT ( 'NONE',  ( 9.651614352920402595, 4.121347559867366783, 7.130841425383052545 ) ) ;
#178288 = CARTESIAN_POINT ( 'NONE',  ( 3.432427499664345127, -1.176894005904068896, 1.578936197102176031 ) ) ;
#178289 = CARTESIAN_POINT ( 'NONE',  ( 6.351568543859240634, 2.286598795830016684, -0.1622092447367465551 ) ) ;
#178290 = CARTESIAN_POINT ( 'NONE',  ( 4.230939532379584200, 0.09184734775685020336, 1.823503176236190404 ) ) ;
#178291 = CIRCLE ( 'NONE', #202514, 0.1599999999999999756 ) ;
#178292 = EDGE_CURVE ( 'NONE', #193052, #103348, #91752, .T. ) ;
#178293 = CARTESIAN_POINT ( 'NONE',  ( 6.536439455564155843, 8.719208346281938304, 1.443375672974065660 ) ) ;
#178294 = CARTESIAN_POINT ( 'NONE',  ( 3.511198595814921219, 7.040222761851976152, 0.7216878364870317197 ) ) ;
#178295 = CARTESIAN_POINT ( 'NONE',  ( -6.095272577795516789, 9.268845886473535245, 1.199719254218452047 ) ) ;
#178296 = CARTESIAN_POINT ( 'NONE',  ( 4.518610335104485287, 8.493738834255713854, 0.000000000000000000 ) ) ;
#178297 = ORIENTED_EDGE ( 'NONE', *, *, #46978, .F. ) ;
#178299 = CARTESIAN_POINT ( 'NONE',  ( 5.431894621915298593, -1.963206642400895374, 0.4451836139030879713 ) ) ;
#178298 = CARTESIAN_POINT ( 'NONE',  ( 2.085277916773973228, -0.7859315772556186852, 1.665205719185464561 ) ) ;
#178300 = CARTESIAN_POINT ( 'NONE',  ( 6.592461167385279097, -0.5184713896582182624, 2.248443398875634269 ) ) ;
#178301 = CARTESIAN_POINT ( 'NONE',  ( 5.119951393648711324, 1.940949770148656661, -0.2839766199017114690 ) ) ;
#178302 = CARTESIAN_POINT ( 'NONE',  ( -5.506582945444718824, 9.576097202994168001, 0.7998128361456481317 ) ) ;
#178303 = CARTESIAN_POINT ( 'NONE',  ( -5.122283107864663343, 4.870418468797203637, 0.000000000000000000 ) ) ;
#178304 = DIRECTION ( 'NONE',  ( 0.000000000000000000, -1.000000000000000000, 0.000000000000000000 ) ) ;
#178305 = CARTESIAN_POINT ( 'NONE',  ( -4.610654757099099221, 7.536791762327691657, 1.199719254218452935 ) ) ;
#178307 = CARTESIAN_POINT ( 'NONE',  ( 6.350471991779750525, 0.5597436608810264502, 1.679089333223187985 ) ) ;
#178306 = CARTESIAN_POINT ( 'NONE',  ( 1.259447021655529797, 2.059213905598542116, -0.3608319165549890295 ) ) ;
#178308 = CARTESIAN_POINT ( 'NONE',  ( -9.000007961041697868, 1.000000000000000888, -7.937244906211844864 ) ) ;
#178309 = CARTESIAN_POINT ( 'NONE',  ( -0.1102773484824119410, 2.860927498608015984, -2.691535809252169731 ) ) ;
#178310 = CARTESIAN_POINT ( 'NONE',  ( 1.065484398342542383, -1.105240684350906610, 1.344476687319878794 ) ) ;
#178311 = CARTESIAN_POINT ( 'NONE',  ( 7.122110765880372618, 7.203550736482235095, 0.7998128361456341429 ) ) ;
#178313 = DIRECTION ( 'NONE',  ( -0.000000000000000000, -1.000000000000000000, -0.000000000000000000 ) ) ;
#178312 = DIRECTION ( 'NONE',  ( -1.000000000000000000, 0.000000000000000000, 0.000000000000000000 ) ) ;
#178314 = CARTESIAN_POINT ( 'NONE',  ( 1.910387937834428174, 1.279409190829815746, -1.157040217339623034 ) ) ;
#178315 = CARTESIAN_POINT ( 'NONE',  ( 1.663894474538109236, 1.130263417742288112, 1.877492182091732076 ) ) ;
#178316 = CARTESIAN_POINT ( 'NONE',  ( -0.07027205189932134166, -1.338084538058325279, -1.103043951268277478 ) ) ;
#178317 = CARTESIAN_POINT ( 'NONE',  ( 4.547634279845023109, -1.704780727694398479, -1.401453192282381188 ) ) ;
#178318 = CARTESIAN_POINT ( 'NONE',  ( -1.734723475976807094E-15, 4.000007913748543587, -12.17999999982603399 ) ) ;
#178319 =( BOUNDED_SURFACE ( )  B_SPLINE_SURFACE ( 3, 2, ( 
 ( #108075, #174105, #143757 ),
 ( #94983, #25677, #157841 ),
 ( #209752, #142676, #10492 ),
 ( #61393, #71480, #75507 ) ),
 .UNSPECIFIED., .F., .F., .T. ) 
 B_SPLINE_SURFACE_WITH_KNOTS ( ( 4, 4 ),
 ( 3, 3 ),
 ( 0.04893088146668654603, 0.05137248493452926945 ),
 ( 0.000000000000000000, 1.000000000000000000 ),
 .UNSPECIFIED. ) 
 GEOMETRIC_REPRESENTATION_ITEM ( )  RATIONAL_B_SPLINE_SURFACE ( (
 ( 1.000000000000000000, 0.7169884966214681299, 1.000000000000000000),
 ( 1.000000000000000000, 0.7174883642158058628, 1.000000000000000000),
 ( 1.000000000000000000, 0.7180610417773378717, 1.000000000000000000),
 ( 1.000000000000000000, 0.7187540717311196037, 1.000000000000000000) ) ) 
 REPRESENTATION_ITEM ( '' )  SURFACE ( )  );
#178320 = CARTESIAN_POINT ( 'NONE',  ( 1.077284259287077495, 2.005170101804130578, 0.8328141809181826005 ) ) ;
#178321 = CARTESIAN_POINT ( 'NONE',  ( 0.2229205655521030172, -0.09321834626660817358, 1.823428419517532983 ) ) ;
#178322 = CARTESIAN_POINT ( 'NONE',  ( 3.380171168471556520, -2.115091482053657934, -0.09962960183704583361 ) ) ;
#178323 = CARTESIAN_POINT ( 'NONE',  ( 6.639320575229255006, 0.6011172813700341733, 1.850849092781511107 ) ) ;
#178324 = ORIENTED_EDGE ( 'NONE', *, *, #108284, .F. ) ;
#178326 = CARTESIAN_POINT ( 'NONE',  ( 1.364683531249986537, -0.5739583329919174526, 0.7879004041258500513 ) ) ;
#178325 = CARTESIAN_POINT ( 'NONE',  ( 3.720531229262864947, 2.177046216224611364, 0.7181995365407625176 ) ) ;
#178327 = CARTESIAN_POINT ( 'NONE',  ( 4.356247428692526569, 3.976710176429713250, 0.7998128361456341429 ) ) ;
#178328 = CARTESIAN_POINT ( 'NONE',  ( 5.691725559638619814, 5.534767995866836543, 1.040834085586084257E-14 ) ) ;
#178329 = CARTESIAN_POINT ( 'NONE',  ( 6.498696386931579028, -2.177790866848747342, -0.4366942510913833231 ) ) ;
#178330 = CARTESIAN_POINT ( 'NONE',  ( -7.212574532790110737, 7.517017831117667193, -0.7216878364870278340 ) ) ;
#178331 = CARTESIAN_POINT ( 'NONE',  ( 4.609409038966229666, 6.400729850259146758, -1.443375672974051449 ) ) ;
#178332 = CARTESIAN_POINT ( 'NONE',  ( -7.009202228140751778, 9.200488570962775725, -1.443375672974058777 ) ) ;
#178333 = CARTESIAN_POINT ( 'NONE',  ( 4.828112100242277549, 6.726159765073026264, -1.443375672974068769 ) ) ;
#178334 = EDGE_LOOP ( 'NONE', ( #93309, #193675, #97596, #190496, #72119, #80450, #64178, #131908, #32030, #7909, #194124, #195080 ) ) ;
#178335 = CARTESIAN_POINT ( 'NONE',  ( 3.604138833494671346, -0.1455340571130462057, 2.011204217620660817 ) ) ;
#178337 = CARTESIAN_POINT ( 'NONE',  ( 1.762625871119470000, -0.7384422231204194054, -1.926036706659232323 ) ) ;
#178336 = CARTESIAN_POINT ( 'NONE',  ( 5.503720292143644777, 8.508425209887878538, 1.199719254218462483 ) ) ;
#178338 = FACE_BOUND ( 'NONE', #133939, .T. ) ;
#178339 = CARTESIAN_POINT ( 'NONE',  ( 4.543390873910903238, 7.354354215321133204, 1.082531754730548412 ) ) ;
#178340 = DIRECTION ( 'NONE',  ( 1.000000000000000000, -5.578564026256503701E-16, -1.479114197289397135E-31 ) ) ;
#178341 = CARTESIAN_POINT ( 'NONE',  ( 1.364683531249988535, 4.905208333674756283, -0.7879004041258300672 ) ) ;
#178342 = CARTESIAN_POINT ( 'NONE',  ( 4.962908505822443139, 0.2168217322565080263, -2.180687389885840322 ) ) ;
#178343 = CARTESIAN_POINT ( 'NONE',  ( 2.514296259408643319, -1.880434619097739013, 0.7283795345095490648 ) ) ;
#178344 = CARTESIAN_POINT ( 'NONE',  ( 2.173174093899932657, 1.133995793187540180, 1.450494936146892622 ) ) ;
#178345 = CARTESIAN_POINT ( 'NONE',  ( 6.771407655021410399, 9.987393799911945536, -1.199719254218441611 ) ) ;
#178346 =( LENGTH_UNIT ( ) NAMED_UNIT ( * ) SI_UNIT ( .MILLI., .METRE. ) );
#178347 = CARTESIAN_POINT ( 'NONE',  ( 5.016531207907320322, 1.258010867292450152, -1.323153095230594989 ) ) ;
#178348 = CARTESIAN_POINT ( 'NONE',  ( 6.240861317752083970, 2.010826688392798101, -0.1511364921914087889 ) ) ;
#178349 = CARTESIAN_POINT ( 'NONE',  ( -8.202846631467911820, 9.528741477256060577, 1.199719254218462483 ) ) ;
#178351 = CARTESIAN_POINT ( 'NONE',  ( -5.712781623311813384, 7.758274208654143855, -1.599625672291271394 ) ) ;
#178350 = CARTESIAN_POINT ( 'NONE',  ( 5.524405971769074775, 1.352560167130362867, -1.813582142078016712 ) ) ;
#178352 = CARTESIAN_POINT ( 'NONE',  ( 1.242952776902699785, 0.4124841525564198474, 2.065099357090140586 ) ) ;
#178353 = CARTESIAN_POINT ( 'NONE',  ( -7.425025402139490360, 8.691559719698066289, 1.199719254218452047 ) ) ;
#178354 = CARTESIAN_POINT ( 'NONE',  ( 8.890396042259068210, 11.39521468743417998, -1.599625672291257406 ) ) ;
#178355 = CARTESIAN_POINT ( 'NONE',  ( 5.510910596163088569E-16, 6.999999999999992006, 4.500000000000000000 ) ) ;
#178356 = CARTESIAN_POINT ( 'NONE',  ( 8.378074386687000441, 9.508151349768592553, 15.76159487570644480 ) ) ;
#178357 = CARTESIAN_POINT ( 'NONE',  ( -6.340409392685171674, 10.54889472477470846, 0.7998128361456481317 ) ) ;
#178358 = CARTESIAN_POINT ( 'NONE',  ( 5.908535366262987587, 4.807949608181238510, -2.499999999999995115 ) ) ;
#178359 = CARTESIAN_POINT ( 'NONE',  ( 8.011942431032855083, 8.311964022485323511, 0.7998128361456291469 ) ) ;
#178360 = CARTESIAN_POINT ( 'NONE',  ( 5.237746300327911442, 6.405127287353401755, -1.156737470277836355 ) ) ;
#178361 = CARTESIAN_POINT ( 'NONE',  ( 2.571500236035813902, 1.429449181443824823, 1.422607194786096541 ) ) ;
#178362 = CARTESIAN_POINT ( 'NONE',  ( -9.083599731475995753, 11.62061899152058686, 1.443375672974064550 ) ) ;
#178363 = CARTESIAN_POINT ( 'NONE',  ( 2.637233524875877588, 2.093239256532848369, 0.7440790952397638991 ) ) ;
#178364 = CARTESIAN_POINT ( 'NONE',  ( 3.271032962906592179, 6.410358100530189951, -0.9347865144461321441 ) ) ;
#178365 = CARTESIAN_POINT ( 'NONE',  ( -5.098748287191073203, 8.106234214101666780, 1.199719254218452935 ) ) ;
#178366 = CARTESIAN_POINT ( 'NONE',  ( 5.425234023762710578, 9.481190127698507553, -0.7998128361456291469 ) ) ;
#178367 = CARTESIAN_POINT ( 'NONE',  ( 3.560947883890089649, 1.548132398191165882, -1.204989647596923508 ) ) ;
#178368 = CARTESIAN_POINT ( 'NONE',  ( 4.774442650306744085, 8.721933525333202653, -0.7998128361456281477 ) ) ;
#178369 = CARTESIAN_POINT ( 'NONE',  ( -4.059747316280317264, 7.561585642977368238, -0.4325785229164439416 ) ) ;
#178370 = CARTESIAN_POINT ( 'NONE',  ( 3.659811400685081040, 6.357198169852855685, -1.199719254218446718 ) ) ;
#178371 = CARTESIAN_POINT ( 'NONE',  ( -4.448483799059637533, 7.243629294661272588, 1.082531754730549967 ) ) ;
#178372 = CARTESIAN_POINT ( 'NONE',  ( -6.941411460516810017, 8.161030127766803588, 1.082531754730549967 ) ) ;
#178373 = CARTESIAN_POINT ( 'NONE',  ( 2.848016566918720294, -1.427295477286108394, -1.568503593382633454 ) ) ;
#178374 = CARTESIAN_POINT ( 'NONE',  ( -5.309953438407606363, 6.223975762010839574, 1.199719254218452935 ) ) ;
#178375 = CARTESIAN_POINT ( 'NONE',  ( 4.012696165952275962, 1.530467462299599513, -1.526897427004340280 ) ) ;
#178376 = CARTESIAN_POINT ( 'NONE',  ( 2.384105128782065819, -0.3166398734758494315, -1.813660976904336808 ) ) ;
#178377 = CARTESIAN_POINT ( 'NONE',  ( -4.932365459154965492, 6.668011768565191844, 1.248136097290372337 ) ) ;
#178378 = CARTESIAN_POINT ( 'NONE',  ( 1.364683531249986537, 0.1760416670080860446, 0.7879004041258500513 ) ) ;
#178379 = CARTESIAN_POINT ( 'NONE',  ( 6.140530580581591735, -1.466303750465405065, 0.9370796520578956734 ) ) ;
#178380 = LINE ( 'NONE', #29989, #25378 ) ;
#178381 = CARTESIAN_POINT ( 'NONE',  ( 3.714570900464274850, 6.317121236308204324, 1.082531754730558626 ) ) ;
#178382 = CARTESIAN_POINT ( 'NONE',  ( 2.817419395390472037, -0.2130390993498078311, 2.151187356804876050 ) ) ;
#178383 = CARTESIAN_POINT ( 'NONE',  ( 4.552111140598270822, 1.802141083034415781, -0.9039717811075360654 ) ) ;
#178384 = CARTESIAN_POINT ( 'NONE',  ( -8.134528978075012517, 12.43410820782212767, 1.040834085586084257E-14 ) ) ;
#178385 = CARTESIAN_POINT ( 'NONE',  ( 2.360439101503517101, 0.9236781337260314695, 1.954550705658316456 ) ) ;
#178386 = CARTESIAN_POINT ( 'NONE',  ( 2.846899755239293839, -1.641009487379685217, 1.092116875444639090 ) ) ;
#178387 = AXIS2_PLACEMENT_3D ( 'NONE', #170140, #150718, #54271 ) ;
#178388 = CARTESIAN_POINT ( 'NONE',  ( 6.509000000000014552, 2.444259026362519904, 2.383015625331697862 ) ) ;
#178389 = CARTESIAN_POINT ( 'NONE',  ( 4.177243316516196181, 1.270932653052879502, 1.468510540936379671 ) ) ;
#178392 = VERTEX_POINT ( 'NONE', #140513 ) ;
#178391 = LINE ( 'NONE', #211926, #160396 ) ;
#178390 = CARTESIAN_POINT ( 'NONE',  ( -8.392133896734675247, 10.81390885098904420, 1.443375672974064550 ) ) ;
#178393 = CARTESIAN_POINT ( 'NONE',  ( -3.146901051703345331, 6.685485303713597283, 0.000000000000000000 ) ) ;
#178394 = FACE_OUTER_BOUND ( 'NONE', #49459, .T. ) ;
#178396 = ORIENTED_EDGE ( 'NONE', *, *, #27277, .F. ) ;
#178395 = CARTESIAN_POINT ( 'NONE',  ( -3.983063267364693960, 7.868933921892603323, -0.7998128361456481317 ) ) ;
#178397 = CARTESIAN_POINT ( 'NONE',  ( -7.632877294369372123, 11.84884791016554573, 0.7216878364870458196 ) ) ;
#178398 = CARTESIAN_POINT ( 'NONE',  ( 1.501302152069685425, 1.803625081967351829, -1.271268654958551014 ) ) ;
#178399 = CARTESIAN_POINT ( 'NONE',  ( -1.642778471875000035, -1.567708332855376252, -2.845375778867859751 ) ) ;
#178400 = CARTESIAN_POINT ( 'NONE',  ( 5.823093080589802462, -1.771997608643091304, -0.8420800316405114838 ) ) ;
#178401 = CARTESIAN_POINT ( 'NONE',  ( -0.6823417656249969321, 5.030208333674755394, -1.181850606188749264 ) ) ;
#178402 = CARTESIAN_POINT ( 'NONE',  ( 1.499999999999989120, 4.035416667349482012, 0.8660254037844524744 ) ) ;
#178403 = CARTESIAN_POINT ( 'NONE',  ( 5.490304984925487908, 6.429369728800919503, -1.257259817782523381 ) ) ;
#178404 = CARTESIAN_POINT ( 'NONE',  ( -9.333041836230016486, 15.44694763438214125, 7.472413793098208856 ) ) ;
#178405 = CARTESIAN_POINT ( 'NONE',  ( 3.855264089065893351, 1.827008581971893530, -0.2271198879545410221 ) ) ;
#178406 = ORIENTED_EDGE ( 'NONE', *, *, #133034, .F. ) ;
#178407 = CARTESIAN_POINT ( 'NONE',  ( -5.508486862036250636E-15, -0.6718749996586012019, -1.570758158831788265 ) ) ;
#178408 = CARTESIAN_POINT ( 'NONE',  ( -6.835281999583978418, 11.12624609948998966, -0.7998128361456291469 ) ) ;
#178409 =( NAMED_UNIT ( * ) SI_UNIT ( $, .STERADIAN. ) SOLID_ANGLE_UNIT ( ) );
#178410 = CARTESIAN_POINT ( 'NONE',  ( 6.533471381225442798, -0.1521382079053348602, 2.086446650026114735 ) ) ;
#178411 = CARTESIAN_POINT ( 'NONE',  ( -0.007473969438217894709, 8.279395425053857949, -1.999986034896452880 ) ) ;
#178412 = CARTESIAN_POINT ( 'NONE',  ( 5.503720292143644777, 8.508425209887878538, 1.199719254218462483 ) ) ;
#178413 = EDGE_CURVE ( 'NONE', #33049, #112763, #146437, .T. ) ;
#178414 = CARTESIAN_POINT ( 'NONE',  ( 0.2509463769419334467, -1.655472276559850853, 1.227265982703225511 ) ) ;
#178417 = CARTESIAN_POINT ( 'NONE',  ( 3.386116603743833497, -0.3623624896987759914, -1.805063595765175499 ) ) ;
#178416 = CARTESIAN_POINT ( 'NONE',  ( 1.486513762117396498, 1.792272468715813138, 0.5009694556475997596 ) ) ;
#178415 = CARTESIAN_POINT ( 'NONE',  ( 6.882015208740356549, 14.48154074412736847, -9.732639244658484401 ) ) ;
#178418 = CARTESIAN_POINT ( 'NONE',  ( 8.782984583554449998, 9.141236857102018831, 1.040834085586084257E-14 ) ) ;
#178419 = CARTESIAN_POINT ( 'NONE',  ( 9.029845422049886494, 1.720726420432415082, 7.609771484012845200 ) ) ;
#178420 = CARTESIAN_POINT ( 'NONE',  ( -7.065734331377342414, 8.272386803808890576, -1.199719254218452047 ) ) ;
#178421 = CARTESIAN_POINT ( 'NONE',  ( -9.513083153069262110, -8.198316282515559550, 1.138412281109779656E-15 ) ) ;
#178422 = AXIS2_PLACEMENT_3D ( 'NONE', #195270, #145498, #11157 ) ;
#178423 = CARTESIAN_POINT ( 'NONE',  ( 3.018423772948013006, -1.088090592406821155, -1.919924466345590108 ) ) ;
#178424 = CARTESIAN_POINT ( 'NONE',  ( 6.081380179524085605, 2.093784091706856199, -0.8575614380509981594 ) ) ;
#178425 = CARTESIAN_POINT ( 'NONE',  ( -6.561783159334141580, 7.718130443053708767, -1.082531754730544860 ) ) ;
#178426 = CARTESIAN_POINT ( 'NONE',  ( 5.853729002925880387, -1.318332981873654441, -1.242799640730863464 ) ) ;
#178427 = CARTESIAN_POINT ( 'NONE',  ( 5.911341210168471250, -1.801345639624308381, 0.6523577827844198040 ) ) ;
#178428 = ADVANCED_FACE ( 'NONE', ( #206525 ), #176561, .F. ) ;
#178429 = CARTESIAN_POINT ( 'NONE',  ( 5.341549334104193747, 5.334155099317440474, 0.7216878364870371598 ) ) ;
#178430 = CARTESIAN_POINT ( 'NONE',  ( 6.596569749568344854, -0.5012203084251048990, -1.802199723311518786 ) ) ;
#178431 = EDGE_CURVE ( 'NONE', #146527, #54417, #118420, .T. ) ;
#178432 = CARTESIAN_POINT ( 'NONE',  ( 6.443805748662878585, 1.284351271648530357, 1.347085863211768819 ) ) ;
#178433 = FACE_OUTER_BOUND ( 'NONE', #180276, .T. ) ;
#178434 = CARTESIAN_POINT ( 'NONE',  ( 0.07479286986305370977, 0.004866263145587856019, -1.855573292446038414 ) ) ;
#178435 = CIRCLE ( 'NONE', #161110, 0.08000000000000020983 ) ;
#178436 = CARTESIAN_POINT ( 'NONE',  ( 1.165250339122084533, 1.861343190080061882, -0.7762330495894869120 ) ) ;
#178438 = CARTESIAN_POINT ( 'NONE',  ( 3.404997959543601294, 1.660052132133410296, -1.295932331351705935 ) ) ;
#178437 = CARTESIAN_POINT ( 'NONE',  ( -9.317477881089553549, 11.89347683273641820, 1.599625672291281386 ) ) ;
#178439 = CARTESIAN_POINT ( 'NONE',  ( 8.609591239877852686, 10.00327685373437347, -1.199719254218445830 ) ) ;
#178441 = CARTESIAN_POINT ( 'NONE',  ( -7.804689982961090955, 12.25722208009664094, 0.7998128361456481317 ) ) ;
#178440 = CARTESIAN_POINT ( 'NONE',  ( -1.402160292154681736E-14, -1.037499999999977662, 1.732050807568877637 ) ) ;
#178442 = CARTESIAN_POINT ( 'NONE',  ( 2.461199802766162570, -1.676885983773316990, 1.125551603727361627 ) ) ;
#178443 = CARTESIAN_POINT ( 'NONE',  ( -0.6823417656249969321, 3.717708333674754506, -1.181850606188749264 ) ) ;
#178444 = CARTESIAN_POINT ( 'NONE',  ( 9.490344339885973923, 12.09515436799890331, -1.443375672974057666 ) ) ;
#178445 = CARTESIAN_POINT ( 'NONE',  ( 3.550220938608072085, 2.161773192003491495, 0.003901938047633223515 ) ) ;
#178446 = CARTESIAN_POINT ( 'NONE',  ( -1.814759087649955749, 3.975067388631681187, 0.4606438099578266665 ) ) ;
#178448 = CARTESIAN_POINT ( 'NONE',  ( -8.014278199453791274, 8.522615118883788199, 1.530808498934192557E-16 ) ) ;
#178447 = CARTESIAN_POINT ( 'NONE',  ( 8.167861197590044142, 8.493869250135347215, 0.000000000000000000 ) ) ;
#178449 = CARTESIAN_POINT ( 'NONE',  ( 9.856414487010587422, 11.56186699200962487, 1.082531754730548412 ) ) ;
#178451 = CARTESIAN_POINT ( 'NONE',  ( 0.008622031262369225790, 14.55347103577515000, 11.95585889282743253 ) ) ;
#178450 = CARTESIAN_POINT ( 'NONE',  ( 1.293694231370069891, -1.962959732339657259, 0.9280293838552654551 ) ) ;
#178452 = CARTESIAN_POINT ( 'NONE',  ( -7.537970219518091319, 7.896646132300314314, -0.7216878364870278340 ) ) ;
#178453 = CARTESIAN_POINT ( 'NONE',  ( -1.402160292154681736E-14, 0.5718750003414239114, 1.575800808251672791 ) ) ;
#178454 = CARTESIAN_POINT ( 'NONE',  ( 2.226364491882920404, 2.126620374013419301, 0.5291077681483095096 ) ) ;
#178455 = CARTESIAN_POINT ( 'NONE',  ( -3.807618569100454486, 6.017853128494015991, 1.294452948159442229 ) ) ;
#178456 = CARTESIAN_POINT ( 'NONE',  ( 2.694485044408474916, -2.256396476877442492, -0.1672753843019215703 ) ) ;
#178457 = CARTESIAN_POINT ( 'NONE',  ( -6.970863535720637216, 11.28442455831609337, 0.7998128361456481317 ) ) ;
#178458 = CARTESIAN_POINT ( 'NONE',  ( -3.836594282542926226, 5.499112634431936542, 1.443375672974064550 ) ) ;
#178459 = CARTESIAN_POINT ( 'NONE',  ( -1.201851678989727383E-14, 4.009375000341416140, -1.575800808251660134 ) ) ;
#178460 = CARTESIAN_POINT ( 'NONE',  ( 5.871284023695358734, 7.173991544917035945, 1.145568358895364458 ) ) ;
#178461 = CARTESIAN_POINT ( 'NONE',  ( 1.500000000000001332, 11.12499999999999645, 0.000000000000000000 ) ) ;
#178462 = CARTESIAN_POINT ( 'NONE',  ( 7.187230829020130329, 7.557726520044554697, 0.7216878364870267237 ) ) ;
#178463 = CARTESIAN_POINT ( 'NONE',  ( 3.092752268530512438, 1.519777622694931773, -0.9064811718217934411 ) ) ;
#178464 = CARTESIAN_POINT ( 'NONE',  ( 8.072990401933337168, 11.50590700464255356, -1.199719254218446718 ) ) ;
#178465 = CARTESIAN_POINT ( 'NONE',  ( 6.493228066955544442, 1.923254169853494178, -1.081975473724585690 ) ) ;
#178466 = CARTESIAN_POINT ( 'NONE',  ( -1.364683531250014514, 9.338541667008062319, -0.7879004041258335089 ) ) ;
#178467 = CARTESIAN_POINT ( 'NONE',  ( -5.309953438407606363, 6.223975762010839574, 1.199719254218452935 ) ) ;
#178468 = CARTESIAN_POINT ( 'NONE',  ( 6.591432905763006111, -0.4393008961055907546, 1.975236973087670878 ) ) ;
#178469 = VERTEX_POINT ( 'NONE', #129644 ) ;
#178470 = CARTESIAN_POINT ( 'NONE',  ( 3.502682687546424312, 1.475339254275360279, -1.149998991230333223 ) ) ;
#178471 = CARTESIAN_POINT ( 'NONE',  ( 2.782155020660907141, -1.188329515115684076, -1.695063343828225877 ) ) ;
#178472 = CARTESIAN_POINT ( 'NONE',  ( -6.739811759324831897, 7.996106819701333634, -1.082531754730549967 ) ) ;
#178473 =( LENGTH_UNIT ( ) NAMED_UNIT ( * ) SI_UNIT ( .MILLI., .METRE. ) );
#178474 = CARTESIAN_POINT ( 'NONE',  ( -9.587917471435847716, 4.026361754648488223, -6.670783315233271615 ) ) ;
#178475 = FILL_AREA_STYLE ('',( #61516 ) ) ;
#178476 = CARTESIAN_POINT ( 'NONE',  ( 6.596550757224428629, -0.5713381284546023009, -2.084776384472402100 ) ) ;
#178477 = CARTESIAN_POINT ( 'NONE',  ( 0.6823417656249882723, -0.9072916663252494907, 1.181850606188755259 ) ) ;
#178478 = CARTESIAN_POINT ( 'NONE',  ( 2.383191274269541360, -0.003000794896521400724, 1.962046632024143866 ) ) ;
#178479 = CARTESIAN_POINT ( 'NONE',  ( 0.4388270972612972609, 1.158508728638860230, 1.649830871073371119 ) ) ;
#178480 = ADVANCED_FACE ( 'NONE', ( #195629 ), #194783, .T. ) ;
#178481 = CARTESIAN_POINT ( 'NONE',  ( -3.797165540279144214, 6.587721009371067638, 1.199719254218452935 ) ) ;
#178482 = CARTESIAN_POINT ( 'NONE',  ( 8.880754312151170282, 10.31963377138658089, 1.199719254218453823 ) ) ;
#178483 =( BOUNDED_CURVE ( )  B_SPLINE_CURVE ( 2, ( #152329, #169642, #119898, #21225, #37508, #120982, #103584 ),
 .UNSPECIFIED., .F., .T. ) 
 B_SPLINE_CURVE_WITH_KNOTS ( ( 3, 2, 2, 3 ),
 ( 0.2500000000000002776, 0.2541666666666668184, 0.2583333333333333592, 0.2624999999999999001 ),
 .UNSPECIFIED. ) 
 CURVE ( )  GEOMETRIC_REPRESENTATION_ITEM ( )  RATIONAL_B_SPLINE_CURVE ( ( 0.9999999999999911182, 0.8660254037844475894, 1.000000000000000000, 0.8660254037844387076, 1.000000000000000000, 0.8660254037844422603, 0.9999999999999964473 ) ) 
 REPRESENTATION_ITEM ( '' )  );
#178484 = CARTESIAN_POINT ( 'NONE',  ( 0.9482695043977107385, 0.5371953702461745861, 1.791772314883005146 ) ) ;
#178485 = CARTESIAN_POINT ( 'NONE',  ( -1.201851678989727383E-14, 3.196875000341420137, -1.575800808251660134 ) ) ;
#178486 = CARTESIAN_POINT ( 'NONE',  ( 2.654543897082308312, 1.998474955683330334, 0.2423782132614532570 ) ) ;
#178488 = CARTESIAN_POINT ( 'NONE',  ( 1.986098615764248398, -2.116669865667855088, 0.05555418577087371801 ) ) ;
#178487 = CARTESIAN_POINT ( 'NONE',  ( -5.897433632264490910, 9.824163637709826702, 0.000000000000000000 ) ) ;
#178489 = CARTESIAN_POINT ( 'NONE',  ( 1.403499169902376664, 7.376709478543046039, 4.304123474984473674 ) ) ;
#178490 = CARTESIAN_POINT ( 'NONE',  ( 3.701679681979888503, -1.565833156357125278, -1.354537944502069102 ) ) ;
#178491 = CARTESIAN_POINT ( 'NONE',  ( 7.126746022638799971, 8.343567110280638133, 1.199719254218452047 ) ) ;
#178493 = DIRECTION ( 'NONE',  ( 3.497202527569253358E-15, 0.000000000000000000, 1.000000000000000000 ) ) ;
#178492 = CARTESIAN_POINT ( 'NONE',  ( 5.455056007322736100, 0.4086298902603173744, -2.050129383449701415 ) ) ;
#178495 = ORIENTED_EDGE ( 'NONE', *, *, #36635, .T. ) ;
#178494 = CARTESIAN_POINT ( 'NONE',  ( 4.506759567000420574, 1.410888988908312047, -1.158519065656477220 ) ) ;
#178496 = CARTESIAN_POINT ( 'NONE',  ( 9.053093885623066939, 11.58502883802551153, -1.599625672291262513 ) ) ;
#178497 = CARTESIAN_POINT ( 'NONE',  ( 7.721398836998361936, -6.134628647623488362, -7.721398836998387694 ) ) ;
#178498 = CARTESIAN_POINT ( 'NONE',  ( 9.728550251279687089, 13.21449840343153426, 8.106492410889076794 ) ) ;
#178499 = CARTESIAN_POINT ( 'NONE',  ( 6.581111309608331794, -0.1016299978719436697, -2.204559905201553427 ) ) ;
#178500 = CARTESIAN_POINT ( 'NONE',  ( 1.364683531249997417, 10.29687500034139802, 2.602085213965210642E-15 ) ) ;
#178501 = ADVANCED_FACE ( 'NONE', ( #31005 ), #191720, .T. ) ;
#178502 = CARTESIAN_POINT ( 'NONE',  ( 5.250612361737760025, 1.884661702551674534, 0.3228764834103393100 ) ) ;
#178503 = CARTESIAN_POINT ( 'NONE',  ( -8.286004436246233951, 12.81875560892930466, 1.040834085586084257E-14 ) ) ;
#178504 = CARTESIAN_POINT ( 'NONE',  ( 7.796102023057898123, 9.054206100777749455, -1.199719254218441611 ) ) ;
#178505 = CARTESIAN_POINT ( 'NONE',  ( -0.6801582343750177673, 1.713541667008065872, 1.178068619123799898 ) ) ;
#178506 = CARTESIAN_POINT ( 'NONE',  ( 9.495223711095174934, -8.169755926620892339, -0.3080734816350358951 ) ) ;
#178507 = CARTESIAN_POINT ( 'NONE',  ( 0.7668492355173107677, 1.774547462407764842, -0.4907661837717376407 ) ) ;
#178508 = VERTEX_POINT ( 'NONE', #51497 ) ;
#178509 = DIRECTION ( 'NONE',  ( 0.000000000000000000, 0.000000000000000000, 1.000000000000000000 ) ) ;
#178510 = CARTESIAN_POINT ( 'NONE',  ( 5.255093269098372488, -1.579555527043162488, -1.001684657140684775 ) ) ;
#178511 = CARTESIAN_POINT ( 'NONE',  ( 0.07700591528351108384, 2.887024434135841755, -2.399578936219012082 ) ) ;
#178512 = CARTESIAN_POINT ( 'NONE',  ( 5.559725510055676168, 8.644040974110419384, 1.199719254218451159 ) ) ;
#178513 = CIRCLE ( 'NONE', #151008, 0.08000000000000020983 ) ;
#178514 = DIRECTION ( 'NONE',  ( 0.000000000000000000, 1.000000000000000000, 0.000000000000000000 ) ) ;
#178515 = CARTESIAN_POINT ( 'NONE',  ( -6.353279334749129426, 6.853861929151015886, 0.6383911273219675664 ) ) ;
#178516 = CARTESIAN_POINT ( 'NONE',  ( -5.043269954603569083, 7.867270132804026872, 1.082531754730560403 ) ) ;
#178517 = AXIS2_PLACEMENT_3D ( 'NONE', #78677, #198800, #182560 ) ;
#178518 = CARTESIAN_POINT ( 'NONE',  ( 4.847203612085560387, 5.613824621309978724, -1.199719254218452047 ) ) ;
#178519 = CARTESIAN_POINT ( 'NONE',  ( 0.8308272516417656295, -1.852502698908803591, -0.6688572162713811720 ) ) ;
#178520 = CARTESIAN_POINT ( 'NONE',  ( 3.444935562074178392, -1.779636981393231565, -0.9480232565319337557 ) ) ;
#178521 = CARTESIAN_POINT ( 'NONE',  ( -6.938021921891187382, 9.117444880338284818, -1.599625672291263179 ) ) ;
#178522 = CARTESIAN_POINT ( 'NONE',  ( 4.797606254389322089, 6.690569611577942943, 1.599625672291268286 ) ) ;
#178523 = EDGE_CURVE ( 'NONE', #8531, #71735, #142054, .T. ) ;
#178524 = CARTESIAN_POINT ( 'NONE',  ( 3.117305861062225958, -2.111875107304355570, 0.5849144002756587746 ) ) ;
#178525 = SURFACE_STYLE_FILL_AREA ( #49576 ) ;
#178526 = CARTESIAN_POINT ( 'NONE',  ( -8.272446282632566650, 12.80293776304669962, 0.7998128361456481317 ) ) ;
#178527 =( NAMED_UNIT ( * ) SI_UNIT ( $, .STERADIAN. ) SOLID_ANGLE_UNIT ( ) );
#178528 = CARTESIAN_POINT ( 'NONE',  ( 0.2331563151865694850, 5.724144821786467219, -2.539778028485844441 ) ) ;
#178529 = EDGE_CURVE ( 'NONE', #191858, #89507, #82545, .T. ) ;
#178530 = CARTESIAN_POINT ( 'NONE',  ( 5.099275172515607579, 5.121778254122544283, -0.7216878364870458196 ) ) ;
#178531 = CARTESIAN_POINT ( 'NONE',  ( 8.782984583554449998, 9.141236857102018831, 1.040834085586084257E-14 ) ) ;
#178532 = DIRECTION ( 'NONE',  ( -0.000000000000000000, -0.000000000000000000, -1.000000000000000000 ) ) ;
#178533 = CARTESIAN_POINT ( 'NONE',  ( 6.048345925472183637, 8.149765894507963182, 1.443375672974065660 ) ) ;
#178534 = ORIENTED_EDGE ( 'NONE', *, *, #151553, .T. ) ;
#178536 = CARTESIAN_POINT ( 'NONE',  ( 1.735022414761304921, 1.879166562360615966, 0.7224556781355166990 ) ) ;
#178535 = CARTESIAN_POINT ( 'NONE',  ( 4.511176471348508521, -1.804767551675333204, 0.3638508048048467169 ) ) ;
#178537 = CARTESIAN_POINT ( 'NONE',  ( 4.728017916497640805, -2.050086588643835750, -1.039272215941482225 ) ) ;
#178539 = CARTESIAN_POINT ( 'NONE',  ( 1.727181476345755806, 0.1432717513335572956, -1.855521175285803182 ) ) ;
#178538 = CARTESIAN_POINT ( 'NONE',  ( -0.1291982275798781443, -0.004298614154785855221, -2.073875112923003083 ) ) ;
#178540 = CARTESIAN_POINT ( 'NONE',  ( -3.285556943750000070, -2.559374999522041172, 0.000000000000000000 ) ) ;
#178541 = CARTESIAN_POINT ( 'NONE',  ( -4.134873662487946966, 3.926366815765101936, 1.214306433183764966E-14 ) ) ;
#178542 = CARTESIAN_POINT ( 'NONE',  ( 5.924064563541377559, -1.897137492723115049, 0.2407653536913647030 ) ) ;
#178543 = CARTESIAN_POINT ( 'NONE',  ( -8.025536864285518490, 11.45054454405341282, -1.199719254218446718 ) ) ;
#178544 = CARTESIAN_POINT ( 'NONE',  ( -6.794044374223859428, 7.099008989448849505, 0.000000000000000000 ) ) ;
#178546 = CARTESIAN_POINT ( 'NONE',  ( 2.869827659178546764, 0.9992216309704025079, 1.581230272166146644 ) ) ;
#178545 = CARTESIAN_POINT ( 'NONE',  ( 5.161704669080129371, 1.031500688015974054, 1.818515148517543034 ) ) ;
#178547 = CARTESIAN_POINT ( 'NONE',  ( 6.968527767744109980, 7.232296605230681408, 0.7216878364870317197 ) ) ;
#178548 = CARTESIAN_POINT ( 'NONE',  ( 5.390138975101268493, -0.4531076923771395482, -1.784498753146485539 ) ) ;
#178549 = CARTESIAN_POINT ( 'NONE',  ( 3.602716132929354664, 5.226254793216122074, 1.599625672291267398 ) ) ;
#178550 = CARTESIAN_POINT ( 'NONE',  ( 0.000000000000000000, 4.518467169708412001, 0.000000000000000000 ) ) ;
#178551 = CARTESIAN_POINT ( 'NONE',  ( 5.232891500378062943, 0.1322050776780703540, 1.719872175869048947 ) ) ;
#178552 = CARTESIAN_POINT ( 'NONE',  ( -5.228640796364566690, 9.251831362400652736, -0.7998128361456231517 ) ) ;
#178553 = CARTESIAN_POINT ( 'NONE',  ( 0.4747597223977735315, -1.720734514737034093, -0.2143409017008046646 ) ) ;
#178554 = CARTESIAN_POINT ( 'NONE',  ( 1.896367326442688350, 3.293421909012307580, 0.4056650308922344350 ) ) ;
#178555 = STYLED_ITEM ( 'NONE', ( #130086 ), #98770 ) ;
#178556 = CARTESIAN_POINT ( 'NONE',  ( 4.961888193860729324, -0.5853885669280403103, 2.090577497978749477 ) ) ;
#178557 = CARTESIAN_POINT ( 'NONE',  ( 3.703562413045482060, -0.5285312144065814621, 1.747510042522756990 ) ) ;
#178558 = CARTESIAN_POINT ( 'NONE',  ( 1.076917802502619592, 1.810449747239597951, 0.7559744942375112853 ) ) ;
#178559 = CARTESIAN_POINT ( 'NONE',  ( -0.05292715583045219663, -1.893440308637056146, -0.9475653277955156106 ) ) ;
#178560 = B_SPLINE_CURVE_WITH_KNOTS ( 'NONE', 3,
 ( #163917, #131453, #115215, #181205, #148721, #50151 ),
 .UNSPECIFIED., .F., .F.,
 ( 4, 2, 4 ),
 ( 0.000000000000000000, 0.0003239988925529259747, 0.0006479977851058519494 ),
 .UNSPECIFIED. ) ;
#178562 = CARTESIAN_POINT ( 'NONE',  ( -0.6823417656250212460, 3.613541667008085767, 1.181850606188767472 ) ) ;
#178561 = CARTESIAN_POINT ( 'NONE',  ( 0.1997390566700393277, -0.6049713359795177992, 2.210933144166931985 ) ) ;
#178563 = CARTESIAN_POINT ( 'NONE',  ( 2.487170525094572149, 8.243531156567085461, 2.499999999999998224 ) ) ;
#178564 = ADVANCED_FACE ( 'NONE', ( #152196 ), #199944, .F. ) ;
#178565 = CARTESIAN_POINT ( 'NONE',  ( 8.911787042884274257, 9.291506392986812912, 0.7998128361456462443 ) ) ;
#178566 = AXIS2_PLACEMENT_3D ( 'NONE', #89630, #37657, #87482 ) ;
#178567 = CARTESIAN_POINT ( 'NONE',  ( 2.737105750116640923, 1.997451989420237606, 0.7121958652205606644 ) ) ;
#178568 = CARTESIAN_POINT ( 'NONE',  ( -4.948362879307902418, 4.875437568721725512, 1.214306433183764966E-14 ) ) ;
#178569 = CARTESIAN_POINT ( 'NONE',  ( -4.370663978927087356, 5.060324124126027279, 2.420000000000000373 ) ) ;
#178570 = EDGE_CURVE ( 'NONE', #146442, #55162, #118658, .T. ) ;
#178571 = CARTESIAN_POINT ( 'NONE',  ( -3.416291520519271874, 6.929497840673697340, 1.040834085586084257E-14 ) ) ;
#178572 = CARTESIAN_POINT ( 'NONE',  ( 0.4091448426733998445, -1.664836780672280803, 1.230395522420650201 ) ) ;
#178574 = CARTESIAN_POINT ( 'NONE',  ( 1.499999999999997113, 14.17708333401613352, -0.8660254037844378194 ) ) ;
#178573 = LINE ( 'NONE', #65839, #68696 ) ;
#178576 = ORIENTED_EDGE ( 'NONE', *, *, #59332, .F. ) ;
#178575 = CARTESIAN_POINT ( 'NONE',  ( 2.772393654007713870, 2.210366155326251025, -0.2202761458626761870 ) ) ;
#178577 = CARTESIAN_POINT ( 'NONE',  ( 1.161203735943004300, 1.374334461307982425, 1.842484299438088557 ) ) ;
#178579 = CARTESIAN_POINT ( 'NONE',  ( 5.190308500716538376, 1.065014321051664048, -1.766232332728798538 ) ) ;
#178578 = CARTESIAN_POINT ( 'NONE',  ( 3.334415713957098681, 5.977569868670206787, -1.199719254218446718 ) ) ;
#178581 = CARTESIAN_POINT ( 'NONE',  ( -1.737499999999997824, -2.741666666666666696, 3.009438278150925683 ) ) ;
#178580 = CARTESIAN_POINT ( 'NONE',  ( 5.071631979963703962, 8.074598522336444262, 1.199719254218451159 ) ) ;
#178582 = CARTESIAN_POINT ( 'NONE',  ( 4.525389411911321602, 8.501647757197021704, -0.7998128361456381397 ) ) ;
#178583 = DIRECTION ( 'NONE',  ( 0.000000000000000000, -0.7071067811865513475, -0.7071067811865435759 ) ) ;
#178584 = CARTESIAN_POINT ( 'NONE',  ( 5.337399561049260832, 0.7408347518493042516, -1.685818907712175019 ) ) ;
#178585 = AXIS2_PLACEMENT_3D ( 'NONE', #79490, #20597, #145609 ) ;
#178586 = CARTESIAN_POINT ( 'NONE',  ( 3.354752944377597856, 6.001296637494123232, -1.199719254218446718 ) ) ;
#178587 = DIRECTION ( 'NONE',  ( -3.330669073875479482E-16, 3.330669073875479482E-16, 1.000000000000000000 ) ) ;
#178588 = CARTESIAN_POINT ( 'NONE',  ( 2.326796526899118422, -0.003300274434325441240, 1.724958192180660044 ) ) ;
#178589 = CARTESIAN_POINT ( 'NONE',  ( 1.657435761918718331, 1.928256795251210631, -0.5899901959932272177 ) ) ;
#178590 = CARTESIAN_POINT ( 'NONE',  ( 1.952162490553134955, -2.103507816325803415, -0.9273050526804761384 ) ) ;
#178591 = CARTESIAN_POINT ( 'NONE',  ( 0.6823417656249917140, 3.905208333674754950, 1.181850606188765695 ) ) ;
#178592 = CARTESIAN_POINT ( 'NONE',  ( 2.478104529052836291, 1.390129537188329101, 1.784895063601476428 ) ) ;
#178593 = CARTESIAN_POINT ( 'NONE',  ( 4.582709122986449835, -2.042650070554121733, -0.5124292222106421324 ) ) ;
#178594 = CARTESIAN_POINT ( 'NONE',  ( -6.400857919427531684, 9.521399101757175742, 1.082531754730549967 ) ) ;
#178595 = CARTESIAN_POINT ( 'NONE',  ( 2.248939020346378381, -1.418119551073221851, -1.058484587410456701 ) ) ;
#178596 = CARTESIAN_POINT ( 'NONE',  ( 6.823831386379729302, 6.855558127064808716, -0.7998128361456281477 ) ) ;
#178598 = CARTESIAN_POINT ( 'NONE',  ( 4.915721525821019178, -1.224934246408443839, -1.937497040551818150 ) ) ;
#178597 = CARTESIAN_POINT ( 'NONE',  ( 5.411112705185558092, 6.445957923205511086, -1.082531754730548412 ) ) ;
#178599 = CARTESIAN_POINT ( 'NONE',  ( 4.681507052731401330, -0.8653998779965512700, 1.625073734443114759 ) ) ;
#178600 = CARTESIAN_POINT ( 'NONE',  ( -5.935772324684618795, 5.819489221753827657, 0.000000000000000000 ) ) ;
#178601 = ADVANCED_FACE ( 'NONE', ( #207338 ), #118785, .F. ) ;
#178602 = CARTESIAN_POINT ( 'NONE',  ( 4.961921032477176752, 8.732732271291288484, 1.040834085586084257E-14 ) ) ;
#178603 = CARTESIAN_POINT ( 'NONE',  ( 1.499999999999987121, 2.545833333333351156, -0.8660254037844262731 ) ) ;
#178604 = CARTESIAN_POINT ( 'NONE',  ( 4.224703044441734612, 0.1064595904514322594, 2.188988589495489911 ) ) ;
#178605 = CARTESIAN_POINT ( 'NONE',  ( -4.680589345215810049, 6.483773540883647435, -1.599625672291256295 ) ) ;
#178606 = CARTESIAN_POINT ( 'NONE',  ( 0.2791710057859035921, 8.178600120974712340, -1.982899171337044297 ) ) ;
#178607 = CARTESIAN_POINT ( 'NONE',  ( -0.08000000000000367928, 7.849261790823902629, -9.579665964948867796 ) ) ;
#178608 = CARTESIAN_POINT ( 'NONE',  ( -0.6823417656250212460, 5.051041667008086655, 1.181850606188767472 ) ) ;
#178609 = CARTESIAN_POINT ( 'NONE',  ( 3.105993306306195301, -1.924270352051945299, 0.09518456514568535143 ) ) ;
#178610 = CARTESIAN_POINT ( 'NONE',  ( 1.364683531249996529, 8.713541667008067648, 0.7879004041258405033 ) ) ;
#178611 = CARTESIAN_POINT ( 'NONE',  ( -4.934804725694236893, 4.859619722839116918, -0.7216878364870207285 ) ) ;
#178612 = CARTESIAN_POINT ( 'NONE',  ( 6.011998765391792787, -0.7129019540204998284, 1.997330473063135381 ) ) ;
#178613 = CARTESIAN_POINT ( 'NONE',  ( -6.509323148336870091, 7.727203440215372865, 1.082531754730549078 ) ) ;
#178614 = EDGE_LOOP ( 'NONE', ( #72440, #128042, #183592, #186055 ) ) ;
#178616 = DIRECTION ( 'NONE',  ( 0.000000000000000000, 0.000000000000000000, 1.000000000000000000 ) ) ;
#178615 = CARTESIAN_POINT ( 'NONE',  ( -5.966997003790240228, 6.134120390609613338, -0.7216878364870338292 ) ) ;
#178617 = CARTESIAN_POINT ( 'NONE',  ( 5.027376032568989572, 4.759693547618927489, 0.7998128361456341429 ) ) ;
#178618 = CARTESIAN_POINT ( 'NONE',  ( 6.409700764581637067, -0.8744420883355051854, -1.620376909479949390 ) ) ;
#178619 = SURFACE_STYLE_FILL_AREA ( #96313 ) ;
#178620 = CARTESIAN_POINT ( 'NONE',  ( 1.364683531249988535, 3.676041667008087099, 0.7879004041258500513 ) ) ;
#178621 = CARTESIAN_POINT ( 'NONE',  ( 1.821426705348125230, 1.001848811563336605, -1.422965107008233643 ) ) ;
#178622 = CARTESIAN_POINT ( 'NONE',  ( 0.000000000000000000, 7.250000000000006217, 0.000000000000000000 ) ) ;
#178623 = CARTESIAN_POINT ( 'NONE',  ( 0.2210476084268316321, -1.750679471464357873, -0.8856473702157914296 ) ) ;
#178624 = CARTESIAN_POINT ( 'NONE',  ( 0.6823417656249882723, 0.1552083336747514530, 1.181850606188755259 ) ) ;
#178625 = DIRECTION ( 'NONE',  ( -3.347138415753903010E-16, -0.6000000000000018652, 0.7999999999999984901 ) ) ;
#178626 = CARTESIAN_POINT ( 'NONE',  ( 5.981359018292748075, 1.999130597612966742, -0.8229454869796914984 ) ) ;
#178627 = CARTESIAN_POINT ( 'NONE',  ( -9.541187415715041809, 12.15447128979948310, -1.599625672291263179 ) ) ;
#178628 = CARTESIAN_POINT ( 'NONE',  ( -6.860062538390436337, 7.105753837651378468, 1.040834085586084257E-14 ) ) ;
#178629 = CARTESIAN_POINT ( 'NONE',  ( 6.157120911006636277, -1.851533521339579380, -1.115484332758958974 ) ) ;
#178631 = ORIENTED_EDGE ( 'NONE', *, *, #202497, .T. ) ;
#178630 = CARTESIAN_POINT ( 'NONE',  ( -0.3540227772641141302, -5.166863022244726267, -10.99462479582585672 ) ) ;
#178632 = CARTESIAN_POINT ( 'NONE',  ( -0.6823417656250212460, 4.301041667008085767, 1.181850606188767472 ) ) ;
#178633 = CARTESIAN_POINT ( 'NONE',  ( 0.4384654110765589530, 0.3132546388123040870, 1.843968665737522050 ) ) ;
#178634 = CARTESIAN_POINT ( 'NONE',  ( 6.169268014014505752, -0.6277043665407368023, -1.616433383845305105 ) ) ;
#178636 = CARTESIAN_POINT ( 'NONE',  ( 3.087623348389135547, -0.8860277256741244667, 2.004638750299721828 ) ) ;
#178635 = CARTESIAN_POINT ( 'NONE',  ( 0.6801582343749935644, -0.02604166632526327962, 1.178068619123817218 ) ) ;
#178637 = CARTESIAN_POINT ( 'NONE',  ( 3.804037270277782490, -0.6727452520632947186, 2.207335857111696331 ) ) ;
#178638 = CARTESIAN_POINT ( 'NONE',  ( 6.011025214932095295, 1.815421535059216662, 0.9752673143463059802 ) ) ;
#178639 = CARTESIAN_POINT ( 'NONE',  ( 1.534995247775998939, -1.406442930887800813, -1.339296560326202146 ) ) ;
#178640 = CARTESIAN_POINT ( 'NONE',  ( -5.951666246274811556, 7.966696592119163256, 1.443375672974064550 ) ) ;
#178641 = PRODUCT_DEFINITION_SHAPE ( 'NONE', 'NONE',  #35864 ) ;
#178642 = CARTESIAN_POINT ( 'NONE',  ( 0.000000000000000000, -0.02876672507444791305, 0.000000000000000000 ) ) ;
#178643 = CARTESIAN_POINT ( 'NONE',  ( 5.581281513216643120, 5.830910960256830755, -0.7657042079148683733 ) ) ;
#178644 = CARTESIAN_POINT ( 'NONE',  ( 3.568700945156903614, 0.7666329941097769218, 1.977337035738421900 ) ) ;
#178645 = CARTESIAN_POINT ( 'NONE',  ( 2.795546247670523954, 1.458556481301529706, -1.392545902517070111 ) ) ;
#178646 = CARTESIAN_POINT ( 'NONE',  ( -4.392478580703220281, 8.068382744221649361, 1.040834085586084257E-14 ) ) ;
#178647 = CARTESIAN_POINT ( 'NONE',  ( 3.997267248050282884, 1.865803599355109421, -1.178106810156675843 ) ) ;
#178648 = CARTESIAN_POINT ( 'NONE',  ( 1.001543065824772753E-15, -0.4593749995220425819, 3.793834371823811669 ) ) ;
#178649 = CARTESIAN_POINT ( 'NONE',  ( -3.432104779031577735, -3.080473746885612485, 0.2707740179794877466 ) ) ;
#178650 = CARTESIAN_POINT ( 'NONE',  ( 0.0001326617329764151682, 14.56986279537652784, 11.92506549394788173 ) ) ;
#178651 = CARTESIAN_POINT ( 'NONE',  ( -7.208094944320834863, 8.438474185576302133, -1.199719254218452047 ) ) ;
#178653 = CARTESIAN_POINT ( 'NONE',  ( 6.825078400183548943, 1.222324429417048330, 2.356141576552318817 ) ) ;
#178652 = CARTESIAN_POINT ( 'NONE',  ( -4.594589183792981757, 8.486487934283967860, 0.2047448450237729367 ) ) ;
#178654 = CARTESIAN_POINT ( 'NONE',  ( -10.43230948805442893, 5.066484524551064794, 5.254757398418679060 ) ) ;
#178655 = ORIENTED_EDGE ( 'NONE', *, *, #11908, .F. ) ;
#178656 = CARTESIAN_POINT ( 'NONE',  ( 4.258703985924441326, -1.528322205979601334, 1.382770117495622397 ) ) ;
#178657 = CARTESIAN_POINT ( 'NONE',  ( -2.954552044183079750E-14, 2.578125000341414452, -1.570758158831808249 ) ) ;
#178658 = DIRECTION ( 'NONE',  ( 2.664535259100375697E-15, 0.000000000000000000, -1.000000000000000000 ) ) ;
#178659 = CARTESIAN_POINT ( 'NONE',  ( -4.822949958159302497, 6.649860922651058992, -1.599625672291256295 ) ) ;
#178660 = CARTESIAN_POINT ( 'NONE',  ( -5.004894982100124068, 5.868074229652107121, 1.199719254218452935 ) ) ;
#178661 = CARTESIAN_POINT ( 'NONE',  ( 3.510419912045096069, -2.017469964673058946, -0.09679370177045029666 ) ) ;
#178662 = CARTESIAN_POINT ( 'NONE',  ( -1.402160292154681736E-14, 0.8375000000000232259, -1.732050807568863648 ) ) ;
#178664 = CARTESIAN_POINT ( 'NONE',  ( 8.595506201383999567, 12.97191496834930113, 0.7216878364870438212 ) ) ;
#178663 = CARTESIAN_POINT ( 'NONE',  ( -3.630551273409382329, 7.457669928944732796, 0.7998128361456352531 ) ) ;
#178665 = CARTESIAN_POINT ( 'NONE',  ( 6.174848896020108668, 9.291408581077091000, 1.199719254218460707 ) ) ;
#178666 = CARTESIAN_POINT ( 'NONE',  ( 3.485278940986863638, 1.863876800102952203, -0.8796150190680316339 ) ) ;
#178667 = CARTESIAN_POINT ( 'NONE',  ( 2.567029916978436077, -1.034165006014248211, 1.730866473406714068 ) ) ;
#178668 = CARTESIAN_POINT ( 'NONE',  ( 0.000000000000000000, 3.499999999999989342, 0.000000000000000000 ) ) ;
#178669 = CARTESIAN_POINT ( 'NONE',  ( 6.667912619822566000, 6.673652899414787676, 1.040834085586084257E-14 ) ) ;
#178670 = CARTESIAN_POINT ( 'NONE',  ( -0.4782691259469663003, 7.503280781841559666, -1.943353214563636300 ) ) ;
#178671 = CARTESIAN_POINT ( 'NONE',  ( 0.9195641160042143936, 1.098457714822091091, -1.477412082521646575 ) ) ;
#178672 = CARTESIAN_POINT ( 'NONE',  ( 6.568967528192747096, -2.015767819289843388, -0.8987472251835016968 ) ) ;
#178673 = CARTESIAN_POINT ( 'NONE',  ( 4.278479993564246797, 7.149254538203735798, 1.199719254218452047 ) ) ;
#178674 = CARTESIAN_POINT ( 'NONE',  ( 2.653791512158054200, 0.5793167894731532375, -2.082426382048585101 ) ) ;
#178675 = CARTESIAN_POINT ( 'NONE',  ( -3.131570295076647525, 6.597323077657299528, 1.040834085586084257E-14 ) ) ;
#178676 = CARTESIAN_POINT ( 'NONE',  ( 4.593022152086825294, 1.843820828628543129, 1.040707789177892861 ) ) ;
#178677 = EDGE_CURVE ( 'NONE', #10457, #180001, #212080, .T. ) ;
#178678 = AXIS2_PLACEMENT_3D ( 'NONE', #132405, #99867, #167005 ) ;
#178679 = CARTESIAN_POINT ( 'NONE',  ( -11.88235317400313917, 11.25664239773029607, -0.9089793033029951452 ) ) ;
#178680 = CARTESIAN_POINT ( 'NONE',  ( 1.358040219746913024, 0.7549631825471068147, 1.711723683848711985 ) ) ;
#178681 = CARTESIAN_POINT ( 'NONE',  ( 5.032083864297879572, 1.014306426666331529, -1.690397665970795105 ) ) ;
#178682 = STYLED_ITEM ( 'NONE', ( #94128 ), #197875 ) ;
#178683 = CARTESIAN_POINT ( 'NONE',  ( 4.118375227313908482, 1.978554835517082555, 0.3886342876525810119 ) ) ;
#178685 = CARTESIAN_POINT ( 'NONE',  ( 8.880227426826630577, 12.34372051706435869, 1.082531754730546636 ) ) ;
#178684 = CARTESIAN_POINT ( 'NONE',  ( 0.6823417656249899377, 3.426041667008085323, -1.181850606188754593 ) ) ;
#178687 = CARTESIAN_POINT ( 'NONE',  ( 6.586557477600968546, -2.065026496990796101, -0.4128237726619687353 ) ) ;
#178686 = CARTESIAN_POINT ( 'NONE',  ( -6.877010230629689858, 9.046264573866535486, 1.599625672291283607 ) ) ;
#178688 = CARTESIAN_POINT ( 'NONE',  ( 6.338344951546218908, -1.110931056888088353, 1.746890944850580052 ) ) ;
#178689 = CARTESIAN_POINT ( 'NONE',  ( 7.142447996300871793, 7.227277505306155092, 0.7998128361456341429 ) ) ;
#178690 = CARTESIAN_POINT ( 'NONE',  ( -7.009729113465285266, 8.136771039586342624, -1.199719254218446718 ) ) ;
#178691 = CARTESIAN_POINT ( 'NONE',  ( -0.3689019803513007845, -6.583711573986997578, -9.609441814500801371 ) ) ;
#178692 = CARTESIAN_POINT ( 'NONE',  ( 4.715676653857135747, -1.933614719187324082, 0.3836508851736331605 ) ) ;
#178693 = CARTESIAN_POINT ( 'NONE',  ( 5.994400513263062891, -1.076938050528394308, 1.708516719617196422 ) ) ;
#178694 = CARTESIAN_POINT ( 'NONE',  ( 1.499999999999989120, 0.05625000068281565957, 0.000000000000000000 ) ) ;
#178695 = CARTESIAN_POINT ( 'NONE',  ( 4.143447727350758392, -2.008842960899869912, 1.135675674892607345 ) ) ;
#178696 = CARTESIAN_POINT ( 'NONE',  ( 2.342701370759682433, -2.021932799725610241, -0.4066214432158538616 ) ) ;
#178697 = CARTESIAN_POINT ( 'NONE',  ( 6.155038550924133212, 10.12470270947942730, 0.7216878364870438212 ) ) ;
#178698 = EDGE_CURVE ( 'NONE', #128658, #207594, #18365, .T. ) ;
#178699 = CARTESIAN_POINT ( 'NONE',  ( 6.554440917563797875, 6.611545590104705994, -0.7998128361456481317 ) ) ;
#178700 = CARTESIAN_POINT ( 'NONE',  ( 4.329849954717849947, 6.144853928627882489, 1.599625672291262513 ) ) ;
#178701 = CARTESIAN_POINT ( 'NONE',  ( -0.6823417656250003738, 1.780208333674752952, -1.181850606188749264 ) ) ;
#178702 = FACE_OUTER_BOUND ( 'NONE', #77525, .T. ) ;
#178703 = CARTESIAN_POINT ( 'NONE',  ( 5.599154252319471503, 9.476171027773981237, -0.7216878364870267237 ) ) ;
#178704 = CARTESIAN_POINT ( 'NONE',  ( 4.527882006162959883, 2.107076143796441592, -0.5232759588417631447 ) ) ;
#178706 = CARTESIAN_POINT ( 'NONE',  ( 3.509164994824386596, -1.813400730843343966, 0.3181347684400454012 ) ) ;
#178705 = CARTESIAN_POINT ( 'NONE',  ( -3.714570900464290393, 5.356752022006865843, 1.443375672974064550 ) ) ;
#178708 = DIRECTION ( 'NONE',  ( 0.000000000000000000, -1.000000000000000000, 0.000000000000000000 ) ) ;
#178707 = CARTESIAN_POINT ( 'NONE',  ( -1.364683531250012516, 4.738541667008091096, -0.7879004041258300672 ) ) ;
#178709 = CARTESIAN_POINT ( 'NONE',  ( 5.302338810847701644, 1.659911028786088538, -1.431018553749352051 ) ) ;
#178710 = CARTESIAN_POINT ( 'NONE',  ( -4.415768667553307481E-15, 0.1250000006828069499, 1.224999999999963229 ) ) ;
#178711 = CARTESIAN_POINT ( 'NONE',  ( 5.418922386936855240, 2.088194672119690676, 0.8713435986696310698 ) ) ;
#178712 = EDGE_LOOP ( 'NONE', ( #191242, #155752, #61027, #202588 ) ) ;
#178713 = CARTESIAN_POINT ( 'NONE',  ( -4.904330467487477918, 6.873893772473251396, -1.448588590679427801 ) ) ;
#178714 = CARTESIAN_POINT ( 'NONE',  ( 4.602896574056089207, 8.480248385054199645, 0.1803159889683242367 ) ) ;
#178715 = CARTESIAN_POINT ( 'NONE',  ( -6.143253000323532831, 7.300121600866474658, 1.082531754730548412 ) ) ;
#178716 = CARTESIAN_POINT ( 'NONE',  ( -6.396834479292370368, -8.176568542494905500, -7.055228938194266775 ) ) ;
#178717 = CARTESIAN_POINT ( 'NONE',  ( 0.4789242711138582687, 1.653723610832663393, -0.6310274585415026616 ) ) ;
#178718 = MECHANICAL_DESIGN_GEOMETRIC_PRESENTATION_REPRESENTATION (  '', ( #164942 ), #47315 ) ;
#178719 = CARTESIAN_POINT ( 'NONE',  ( 5.074862666803740652, -1.456563189067984876, 1.389812660683345191 ) ) ;
#178720 = CARTESIAN_POINT ( 'NONE',  ( 4.957477724091233995, 8.935474444748447098, -0.7998128361456281477 ) ) ;
#178721 = CARTESIAN_POINT ( 'NONE',  ( 3.786240212431398966, -1.039621666623831597, 1.831390154885542243 ) ) ;
#178722 = CARTESIAN_POINT ( 'NONE',  ( 1.739701290322914540, 1.910364143156467298, -0.1427236045144583687 ) ) ;
#178723 = CARTESIAN_POINT ( 'NONE',  ( 4.518945272056516416, 4.166524327021037699, 0.7998128361456341429 ) ) ;
#178724 = CARTESIAN_POINT ( 'NONE',  ( 3.613681597605075346, 0.4810616251548325284, -1.909752186315590405 ) ) ;
#178725 = CARTESIAN_POINT ( 'NONE',  ( 5.590105174118587428, 1.206514928144377441, 1.619649990711173215 ) ) ;
#178726 = CARTESIAN_POINT ( 'NONE',  ( 2.113927203836548419, -0.8795192785214582809, -1.650985937663045577 ) ) ;
#178727 = CARTESIAN_POINT ( 'NONE',  ( 1.750371521623844462, -1.952110535733902585, -0.1955497077021361163 ) ) ;
#178730 = ORIENTED_EDGE ( 'NONE', *, *, #59542, .F. ) ;
#178729 = CARTESIAN_POINT ( 'NONE',  ( 0.8438408207818194340, -1.215224102361469161, -1.476598726422105656 ) ) ;
#178728 = CARTESIAN_POINT ( 'NONE',  ( 4.336358584672225902, 1.692218828317056278, 0.3330917469099390904 ) ) ;
#178732 = CARTESIAN_POINT ( 'NONE',  ( 6.507550544879468823, 6.694489845221929691, -0.7216878364870257245 ) ) ;
#178731 = CARTESIAN_POINT ( 'NONE',  ( 1.190363680384380229, -0.9894552095768920363, 1.972713631218452557 ) ) ;
#178733 = AXIS2_PLACEMENT_3D ( 'NONE', #63808, #132055, #198066 ) ;
#178734 = CARTESIAN_POINT ( 'NONE',  ( -0.6823417656250212460, 1.863541667008083991, 1.181850606188755259 ) ) ;
#178735 = CARTESIAN_POINT ( 'NONE',  ( 8.483651433849084711, 10.92067931095586886, 1.599625672291281386 ) ) ;
#178736 = CARTESIAN_POINT ( 'NONE',  ( 11.92050416151433012, 11.15205375279633238, 1.381922468431395767 ) ) ;
#178737 = CARTESIAN_POINT ( 'NONE',  ( 0.2537734656027313962, 6.376933751358200730, -3.135911668477547654 ) ) ;
#178738 = CARTESIAN_POINT ( 'NONE',  ( -5.608478439449225306, 5.609308656285654671, -0.4224404339892348093 ) ) ;
#178739 = VERTEX_POINT ( 'NONE', #191073 ) ;
#178740 = CARTESIAN_POINT ( 'NONE',  ( 6.912946559606852226, -1.604190412254998810, 1.308348183162249434 ) ) ;
#178741 = CARTESIAN_POINT ( 'NONE',  ( 1.064989848632340363, 1.568927673159369762, -1.351003706900590018 ) ) ;
#178742 = CARTESIAN_POINT ( 'NONE',  ( 1.499999999999987121, 1.504166666666690411, 0.8660254037844524744 ) ) ;
#178743 = CARTESIAN_POINT ( 'NONE',  ( 7.070740804726770357, 8.207951346058097286, 1.199719254218462483 ) ) ;
#178744 = CARTESIAN_POINT ( 'NONE',  ( -8.474009703741204547, 9.845098394908269768, -1.199719254218446718 ) ) ;
#178745 = CARTESIAN_POINT ( 'NONE',  ( 5.391302360089590628, 6.318882837306503575, -1.199719254218452047 ) ) ;
#178746 = CARTESIAN_POINT ( 'NONE',  ( 5.971359625099014856, -1.818578809777360972, -1.090262957368436147 ) ) ;
#178747 = DIRECTION ( 'NONE',  ( -1.561251128379126077E-17, -1.301042606982605475E-17, -1.000000000000000000 ) ) ;
#178748 = CARTESIAN_POINT ( 'NONE',  ( 1.364683531249986537, 2.405208333674752286, -0.7879004041258239610 ) ) ;
#178749 = AXIS2_PLACEMENT_3D ( 'NONE', #19539, #72557, #204677 ) ;
#178750 = CARTESIAN_POINT ( 'NONE',  ( -1.001543065824772872E-14, 4.462500000000024336, 1.732050807568877637 ) ) ;
#178752 = CARTESIAN_POINT ( 'NONE',  ( 10.56143847536557878, 11.42402576412244386, 0.000000000000000000 ) ) ;
#178751 = CARTESIAN_POINT ( 'NONE',  ( 5.828557447170540584, -1.245780601409246957, 1.515539014345569147 ) ) ;
#178753 = CARTESIAN_POINT ( 'NONE',  ( 3.796249832574852601, -1.863883295361246084, 0.7690029265580224926 ) ) ;
#178754 = EDGE_CURVE ( 'NONE', #87946, #86738, #191096, .T. ) ;
#178755 = CARTESIAN_POINT ( 'NONE',  ( 4.030425823177123057, 0.5166280748541264289, 1.844641390986961671 ) ) ;
#178756 = CARTESIAN_POINT ( 'NONE',  ( -7.065207446497166366, 9.336104335703744539, 0.000000000000000000 ) ) ;
#178757 = CARTESIAN_POINT ( 'NONE',  ( 1.417800074541092137, -1.221294057239637576, -1.819523406426680090 ) ) ;
#178758 = CARTESIAN_POINT ( 'NONE',  ( -0.1405533004718755308, 0.003749010675345022196, -1.720146753850456234 ) ) ;
#178759 = CARTESIAN_POINT ( 'NONE',  ( 0.7499999999999867883, 0.09791666734948467621, -1.299038105676652899 ) ) ;
#178760 = CARTESIAN_POINT ( 'NONE',  ( 5.590095194574172588, 1.202541018705102660, 1.614423701025817115 ) ) ;
#178761 = CARTESIAN_POINT ( 'NONE',  ( -5.747767057189642870, 8.793146435774861658, -1.199719254218440723 ) ) ;
#178763 = CARTESIAN_POINT ( 'NONE',  ( 5.694942756591524713, 1.867452007164069672, 0.9975914146606623678 ) ) ;
#178762 = CARTESIAN_POINT ( 'NONE',  ( -2.629918611371007575, 6.012062780000711371, 0.7216878364870317197 ) ) ;
#178764 = DIRECTION ( 'NONE',  ( 0.000000000000000000, 1.000000000000000000, 0.000000000000000000 ) ) ;
#178766 = CARTESIAN_POINT ( 'NONE',  ( -6.583366107887490770, 9.838288338247510367, 1.199719254218452935 ) ) ;
#178765 = CARTESIAN_POINT ( 'NONE',  ( 2.595357119365874432, -0.6533576199754445035, 1.986123937679643348 ) ) ;
#178768 = ORIENTED_EDGE ( 'NONE', *, *, #211218, .F. ) ;
#178767 = CARTESIAN_POINT ( 'NONE',  ( 2.063112832053456636, 0.2986308487272717471, -1.698545238003341673 ) ) ;
#178769 = CARTESIAN_POINT ( 'NONE',  ( 5.818629517237746462, -0.7649446623404360102, -1.977987144599784086 ) ) ;
#178770 = CARTESIAN_POINT ( 'NONE',  ( 6.205881626753210867, 8.263281202677319470, 1.599625672291281386 ) ) ;
#178771 = FACE_OUTER_BOUND ( 'NONE', #91856, .T. ) ;
#178772 = DIRECTION ( 'NONE',  ( -5.578564026256490882E-16, -1.000000000000000000, -9.066213480720158442E-32 ) ) ;
#178773 = DIRECTION ( 'NONE',  ( -0.6483454320283799088, 0.000000000000000000, 0.7613463080411786432 ) ) ;
#178775 = CARTESIAN_POINT ( 'NONE',  ( 9.869972640624258275, 10.61731562359089587, 0.000000000000000000 ) ) ;
#178774 = CARTESIAN_POINT ( 'NONE',  ( 5.472687561410540802, 9.536552588287639409, 0.7998128361456462443 ) ) ;
#178776 = ORIENTED_EDGE ( 'NONE', *, *, #177765, .F. ) ;
#178777 = DIRECTION ( 'NONE',  ( 0.000000000000000000, 1.000000000000000000, 2.168404344971034112E-15 ) ) ;
#178779 = CARTESIAN_POINT ( 'NONE',  ( 2.209342481274043646, 1.400903122447524796, 1.148441741360214152 ) ) ;
#178778 = CARTESIAN_POINT ( 'NONE',  ( 4.505052181490820651, 8.477920988373101707, -0.7998128361456381397 ) ) ;
#178780 = CARTESIAN_POINT ( 'NONE',  ( -6.008234629150358330, 10.16135750065076060, 0.000000000000000000 ) ) ;
#178781 = ORIENTED_EDGE ( 'NONE', *, *, #130972, .T. ) ;
#178782 = CARTESIAN_POINT ( 'NONE',  ( 2.920892028740289081, 5.495125569250587816, 1.199719254218452047 ) ) ;
#178783 = CARTESIAN_POINT ( 'NONE',  ( 6.062430963966053632, 7.101866208495718702, -1.199719254218452047 ) ) ;
#178784 = CARTESIAN_POINT ( 'NONE',  ( 2.297251093426439628, 1.655750149966995544, -0.7352264245090130990 ) ) ;
#178785 = CARTESIAN_POINT ( 'NONE',  ( 6.539320575229279342, 6.038407674219216759, 2.491644695858772796 ) ) ;
#178786 = DIRECTION ( 'NONE',  ( 0.000000000000000000, 0.000000000000000000, 1.000000000000000000 ) ) ;
#178787 = CARTESIAN_POINT ( 'NONE',  ( 4.464323212750023195, 7.049731028713583925, 1.131627047429624167 ) ) ;
#178788 = ORIENTED_EDGE ( 'NONE', *, *, #117333, .F. ) ;
#178789 = CARTESIAN_POINT ( 'NONE',  ( 4.404655029226283602, 0.4953248787317258706, 1.793866421858918869 ) ) ;
#178790 = CARTESIAN_POINT ( 'NONE',  ( 0.1752026701883572513, 1.419887415397131925, 1.286083148499452600 ) ) ;
#178791 = CARTESIAN_POINT ( 'NONE',  ( 0.3580656308817787292, 0.6935259069400134813, 1.688922952486398454 ) ) ;
#178792 = CARTESIAN_POINT ( 'NONE',  ( 1.456203110946918677, 4.349935091901982354, 0.3915051095678068194 ) ) ;
#178793 = CARTESIAN_POINT ( 'NONE',  ( 4.596835240751270035, 8.371391889155539445, -0.09823007671119071693 ) ) ;
#178794 = LINE ( 'NONE', #47739, #157507 ) ;
#178795 = CARTESIAN_POINT ( 'NONE',  ( 0.000000000000000000, 0.4330127018922214077, 0.000000000000000000 ) ) ;
#178796 = CARTESIAN_POINT ( 'NONE',  ( 7.700668062882064291, 10.00719871149432549, -1.443375672974057666 ) ) ;
#178797 = CARTESIAN_POINT ( 'NONE',  ( 4.364079147461279895, -1.964463519307905193, 0.1404744649011815116 ) ) ;
#178798 = CARTESIAN_POINT ( 'NONE',  ( -5.148345644887285744, 7.029489223833707001, -1.599625672291256295 ) ) ;
#178799 = CARTESIAN_POINT ( 'NONE',  ( -11.97929049433705551, 9.719999999999998863, -0.7046979865771821894 ) ) ;
#178800 = EDGE_CURVE ( 'NONE', #110911, #109059, #156779, .T. ) ;
#178801 = CARTESIAN_POINT ( 'NONE',  ( 0.1817335109410072314, -0.9834369453871127931, 1.844881371607492326 ) ) ;
#178802 = CARTESIAN_POINT ( 'NONE',  ( 5.368162667233546514, 0.9496366811117643580, 1.675975028240711540 ) ) ;
#178803 = CARTESIAN_POINT ( 'NONE',  ( -7.528855374290365887, 7.678086112960552434, -0.7998128361456291469 ) ) ;
#178804 = CARTESIAN_POINT ( 'NONE',  ( 0.6041866639863550104, -0.6101368697832668664, -1.720745249832649870 ) ) ;
#178805 = CARTESIAN_POINT ( 'NONE',  ( 2.016531038934398445, -1.041976349804032642, -1.945408382319254503 ) ) ;
#178806 =( NAMED_UNIT ( * ) SI_UNIT ( $, .STERADIAN. ) SOLID_ANGLE_UNIT ( ) );
#178807 = CARTESIAN_POINT ( 'NONE',  ( -0.1054227091227821350, -1.855472971956134920, -0.4628026090111520552 ) ) ;
#178808 = ORIENTED_EDGE ( 'NONE', *, *, #210828, .T. ) ;
#178809 = EDGE_LOOP ( 'NONE', ( #50042, #124417, #62603, #42090 ) ) ;
#178810 = CARTESIAN_POINT ( 'NONE',  ( 0.6429344911094649895, -0.2373986304471594755, -1.955105650238073478 ) ) ;
#178811 = CARTESIAN_POINT ( 'NONE',  ( 1.188897196845212445, 1.471763766255501427, 1.267211023470141695 ) ) ;
#178812 = AXIS2_PLACEMENT_3D ( 'NONE', #148502, #117115, #19541 ) ;
#178813 = EDGE_LOOP ( 'NONE', ( #181798, #77273, #41572, #149797 ) ) ;
#178814 = CARTESIAN_POINT ( 'NONE',  ( 1.124374798274978104, 0.3960433595797500095, -1.976652716225081097 ) ) ;
#178816 = CARTESIAN_POINT ( 'NONE',  ( 5.401151054173385369, -1.597185415876556158, 0.9547389691558528790 ) ) ;
#178815 = CARTESIAN_POINT ( 'NONE',  ( -4.796552484184649856, 8.818004674849227342, -0.7998128361456362523 ) ) ;
#178817 = CARTESIAN_POINT ( 'NONE',  ( 6.412080304620304538, 6.445458208337293549, -0.7998128361456481317 ) ) ;
#178819 = EDGE_CURVE ( 'NONE', #6713, #25036, #139338, .T. ) ;
#178818 = CARTESIAN_POINT ( 'NONE',  ( -1.115562610750309283E-14, 11.31249999999999822, 1.500000000000001554 ) ) ;
#178820 = CARTESIAN_POINT ( 'NONE',  ( 2.449293598294706414E-16, 0.08000000000000020983, 2.000000000000000000 ) ) ;
#178821 = CARTESIAN_POINT ( 'NONE',  ( -4.218558352146454915, 8.073401844146177453, 1.040834085586084257E-14 ) ) ;
#178822 = CARTESIAN_POINT ( 'NONE',  ( -5.399890319992785237, 9.521898816625391504, 0.7998128361456291469 ) ) ;
#178823 = CARTESIAN_POINT ( 'NONE',  ( 1.189316404147572337, 1.662717542896676504, 1.427817766309902314 ) ) ;
#178824 = CARTESIAN_POINT ( 'NONE',  ( 2.575685996916329046, 5.948791396470269888, 0.7216878364870438212 ) ) ;
#178825 = ORIENTED_EDGE ( 'NONE', *, *, #64968, .T. ) ;
#178826 = CARTESIAN_POINT ( 'NONE',  ( 0.4123176713737303767, 3.999999999999973799, -0.8977835139438099521 ) ) ;
#178827 = FILL_AREA_STYLE_COLOUR ( '', #16581 ) ;
#178828 = CARTESIAN_POINT ( 'NONE',  ( 2.121465551170404140, -1.771062468586531047, 0.4427346646293239818 ) ) ;
#178829 = CARTESIAN_POINT ( 'NONE',  ( -3.460355519985875983, 5.060167411448709629, 1.599625672291267398 ) ) ;
#178830 = CARTESIAN_POINT ( 'NONE',  ( 6.609000000000012420, 4.697979799133416456, 2.462673521647487540 ) ) ;
#178831 = CARTESIAN_POINT ( 'NONE',  ( 8.353795204314554468, 12.89784483834236184, -0.7998128361456352531 ) ) ;
#178832 = CARTESIAN_POINT ( 'NONE',  ( 1.172347479525590375, -1.222655876604409553, 1.488804252732379485 ) ) ;
#178833 = CARTESIAN_POINT ( 'NONE',  ( 4.926587646396720643, -1.284401507782207963, 1.482881906352449874 ) ) ;
#178834 = CARTESIAN_POINT ( 'NONE',  ( -8.877891658850122880, 9.251961778280284321, 0.7998128361456462443 ) ) ;
#178835 = ADVANCED_FACE ( 'NONE', ( #158600 ), #46080, .T. ) ;
#178836 = CARTESIAN_POINT ( 'NONE',  ( 3.825371897350130723, 7.614684313550482031, 0.7998128361456321445 ) ) ;
#178837 = CARTESIAN_POINT ( 'NONE',  ( 4.581673536070863584, -1.032772929490553215, 1.932928240684625099 ) ) ;
#178838 = EDGE_CURVE ( 'NONE', #194636, #165662, #181033, .T. ) ;
#178839 = TOROIDAL_SURFACE ( 'NONE', #9360, 9.559451093910105612, 0.08000000000000000167 ) ;
#178840 = CARTESIAN_POINT ( 'NONE',  ( 5.335297142177534369, 6.183267073083954735, -1.199719254218452047 ) ) ;
#178841 = CARTESIAN_POINT ( 'NONE',  ( 4.293848342403890683, -1.423947089648310849, -1.503027170334819029 ) ) ;
#178843 = CARTESIAN_POINT ( 'NONE',  ( -1.201851678989727383E-14, 1.884375000341422135, 1.575800808251672791 ) ) ;
#178842 = CARTESIAN_POINT ( 'NONE',  ( 5.303878726007847710, 4.755038592612019777, 2.500000000000000000 ) ) ;
#178844 = ORIENTED_EDGE ( 'NONE', *, *, #13805, .F. ) ;
#178845 = CARTESIAN_POINT ( 'NONE',  ( 4.166792231569245608, 1.501215554499458982, 1.740835934941728169 ) ) ;
#178847 = ORIENTED_EDGE ( 'NONE', *, *, #32535, .T. ) ;
#178846 = CARTESIAN_POINT ( 'NONE',  ( 6.805829924380105034, 9.923590097543378619, 1.082531754730558626 ) ) ;
#178849 = CARTESIAN_POINT ( 'NONE',  ( -3.285556943750000070, -1.159374999522042815, 0.000000000000000000 ) ) ;
#178848 = CARTESIAN_POINT ( 'NONE',  ( 4.584065335196252811, 8.362176967788721882, 0.7216878364870328300 ) ) ;
#178850 = CARTESIAN_POINT ( 'NONE',  ( 6.620655732516679493, 2.454579131793722002, 2.310038015908893350 ) ) ;
#178851 = CARTESIAN_POINT ( 'NONE',  ( -10.52211599421018740, 5.354012650763445791, -5.769493145238627108 ) ) ;
#178852 = CARTESIAN_POINT ( 'NONE',  ( 3.310425057758420664, 1.755882755489517999, 0.8297573096471222431 ) ) ;
#178853 = ORIENTED_EDGE ( 'NONE', *, *, #65319, .F. ) ;
#178854 = CARTESIAN_POINT ( 'NONE',  ( 10.01911233037457905, 11.75168114260095109, 1.082531754730548412 ) ) ;
#178855 = CARTESIAN_POINT ( 'NONE',  ( 4.746305163667582150, 0.9781546018433548983, -1.643150005489722787 ) ) ;
#178856 = CARTESIAN_POINT ( 'NONE',  ( 4.716110169385688167, 5.239146042535265835, -0.9347783054772640376 ) ) ;
#178857 = CARTESIAN_POINT ( 'NONE',  ( 5.420820933352582749, 1.595050213381223214, 0.6567411224575621098 ) ) ;
#178858 = CARTESIAN_POINT ( 'NONE',  ( 4.434779938697545276, -1.616694733667634942, 1.205040202231236091 ) ) ;
#178859 = CARTESIAN_POINT ( 'NONE',  ( 5.045646660657260973, -1.666335398280174074, 1.583644221457411794 ) ) ;
#178860 = CARTESIAN_POINT ( 'NONE',  ( -1.500000000000008216, 9.750000000000001776, 3.469446951953614189E-15 ) ) ;
#178861 = CARTESIAN_POINT ( 'NONE',  ( 0.6455096168876961471, -1.890800792967793686, 1.137844069391671820 ) ) ;
#178863 = CARTESIAN_POINT ( 'NONE',  ( -4.909461021924285795, 6.821066840368686712, 1.443375672974058777 ) ) ;
#178862 = CARTESIAN_POINT ( 'NONE',  ( -10.31505594189871111, 10.92865344183699428, -0.7998128361456291469 ) ) ;
#178864 = CARTESIAN_POINT ( 'NONE',  ( 5.747242073547443653, -1.395821259116083013, -1.087781934379092874 ) ) ;
#178865 = CARTESIAN_POINT ( 'NONE',  ( 6.363907750917786821, -0.1017471579566435469, -2.013986097687201049 ) ) ;
#178867 = CARTESIAN_POINT ( 'NONE',  ( 1.939794425703120995, 0.8746495868690505882, -2.119022276272637839 ) ) ;
#178866 = CARTESIAN_POINT ( 'NONE',  ( 5.086243903782109221, 5.962981304947771122, -1.199719254218452047 ) ) ;
#178868 = CARTESIAN_POINT ( 'NONE',  ( 0.9897393536978270623, -0.4193350815317981040, -1.688907716811594240 ) ) ;
#178869 = CARTESIAN_POINT ( 'NONE',  ( 5.133733721068893807, 9.141106441222381918, 1.040834085586084257E-14 ) ) ;
#178870 = FACE_OUTER_BOUND ( 'NONE', #116913, .T. ) ;
#178871 = CARTESIAN_POINT ( 'NONE',  ( 1.405166929871915604, 0.3316955492517637549, 1.701605581617445129 ) ) ;
#178872 = CARTESIAN_POINT ( 'NONE',  ( 1.360316468749989793, 0.5677083336747246189, -0.7853790794158941324 ) ) ;
#178873 = CARTESIAN_POINT ( 'NONE',  ( 7.654042494670958593E-16, 0.03624871340549007392, -6.250000000000000000 ) ) ;
#178874 = CARTESIAN_POINT ( 'NONE',  ( 1.293694231370069891, -1.962959732339657259, 0.9280293838552654551 ) ) ;
#178875 = CARTESIAN_POINT ( 'NONE',  ( 2.202361591730035428, 1.313542931311746598, -1.530159205979222170 ) ) ;
#178876 = CARTESIAN_POINT ( 'NONE',  ( -1.201851678989727383E-14, 1.743750000682815493, 1.732050807568877637 ) ) ;
#178877 = CARTESIAN_POINT ( 'NONE',  ( 0.3582593949469566885, 0.7340744485371183403, 1.781236698655277895 ) ) ;
#178878 = CARTESIAN_POINT ( 'NONE',  ( -0.6823417656250003738, 12.65104166700806232, 1.181850606188754593 ) ) ;
#178879 = CARTESIAN_POINT ( 'NONE',  ( 3.726986581234917661, 1.568921747024876634, -1.572872013324580154 ) ) ;
#178880 = ORIENTED_EDGE ( 'NONE', *, *, #45059, .F. ) ;
#178881 = CARTESIAN_POINT ( 'NONE',  ( 6.381095703207996017, -8.233137084989849086, 7.037870247915945399 ) ) ;
#178882 = CARTESIAN_POINT ( 'NONE',  ( 1.499999999999985123, -0.9541666666666493990, -0.8660254037844323793 ) ) ;
#178883 = CARTESIAN_POINT ( 'NONE',  ( 9.023114925094663619, 10.48572115315399245, 1.199719254218453823 ) ) ;
#178884 = CARTESIAN_POINT ( 'NONE',  ( 7.526184668917440312, 8.913541880892736913, -1.082531754730548412 ) ) ;
#178885 = CARTESIAN_POINT ( 'NONE',  ( 5.724081574600810463, 1.679587015112851578, 0.4559996917168698261 ) ) ;
#178887 = CARTESIAN_POINT ( 'NONE',  ( 3.385159196556942085, 0.04556868695702701727, 1.961494628812537444 ) ) ;
#178886 = MECHANICAL_DESIGN_GEOMETRIC_PRESENTATION_REPRESENTATION (  '', ( #64742 ), #37072 ) ;
#178889 = CARTESIAN_POINT ( 'NONE',  ( -6.480434237652138663, 8.583592582059388576, 1.443375672974078761 ) ) ;
#178888 = CARTESIAN_POINT ( 'NONE',  ( 4.844340958784499662, 4.546152628203684820, 0.7998128361456341429 ) ) ;
#178890 = CARTESIAN_POINT ( 'NONE',  ( 4.288523069895104456, -2.236996925053718055, -0.3375187357864944393 ) ) ;
#178891 = B_SPLINE_CURVE_WITH_KNOTS ( 'NONE', 3,
 ( #207119, #72843, #204969, #175706, #122779, #93403 ),
 .UNSPECIFIED., .F., .F.,
 ( 4, 2, 4 ),
 ( 0.000000000000000000, 0.0003157158648874024685, 0.0006314317297748052622 ),
 .UNSPECIFIED. ) ;
#178892 = CARTESIAN_POINT ( 'NONE',  ( 2.506364121320878713, 2.062161341495666100, 0.05312637652370164748 ) ) ;
#178893 = CARTESIAN_POINT ( 'NONE',  ( -5.845536785786364931, 9.971543350059432598, 0.000000000000000000 ) ) ;
#178894 = CARTESIAN_POINT ( 'NONE',  ( 2.132027182898531326, -1.478040878648724465, -1.713098503734461708 ) ) ;
#178895 = ORIENTED_EDGE ( 'NONE', *, *, #154810, .F. ) ;
#178896 = CARTESIAN_POINT ( 'NONE',  ( -1.500000000000001332, 1.181250000682816603, 0.000000000000000000 ) ) ;
#178897 = CARTESIAN_POINT ( 'NONE',  ( 4.147608549738549755, 0.6325110726591242072, -1.760471310998643624 ) ) ;
#178898 = CARTESIAN_POINT ( 'NONE',  ( 2.250263858207638634, 1.700335624809163004, -0.3396627995243851061 ) ) ;
#178899 = CARTESIAN_POINT ( 'NONE',  ( -0.04093971525966337566, -2.051586291785143512, -1.022954789973041123 ) ) ;
#178900 = CARTESIAN_POINT ( 'NONE',  ( 6.510760317505348560, 1.716126801009032032, -1.542884448788630625 ) ) ;
#178901 = CARTESIAN_POINT ( 'NONE',  ( 3.678741886385179072, -2.082744454470350615, -0.5786317199799119182 ) ) ;
#178902 = CARTESIAN_POINT ( 'NONE',  ( 4.453030731839799472, 0.4239971928432215154, -1.894948383050964580 ) ) ;
#178903 = CARTESIAN_POINT ( 'NONE',  ( -2.440104460335327463, 5.790612937125752424, 1.040834085586084257E-14 ) ) ;
#178904 = CARTESIAN_POINT ( 'NONE',  ( 6.397708313642382905, -0.6301307688901837123, 1.761319926792910495 ) ) ;
#178905 = CARTESIAN_POINT ( 'NONE',  ( 5.086710258240730198, 6.515995995190169587, 1.216687342998038934 ) ) ;
#178906 = CARTESIAN_POINT ( 'NONE',  ( -0.1224325501351306023, -0.4448023855274513272, -1.973852191825019364 ) ) ;
#178907 = CARTESIAN_POINT ( 'NONE',  ( 3.607878275012313285, 6.262922849939428716, 1.082531754730549078 ) ) ;
#178908 = CARTESIAN_POINT ( 'NONE',  ( -5.758872628492442907E-14, 2.203125000341452200, 1.570758158831754070 ) ) ;
#178909 = CARTESIAN_POINT ( 'NONE',  ( 6.276017556857773627, 1.753032240926259311, -0.9962986157117934560 ) ) ;
#178910 = CARTESIAN_POINT ( 'NONE',  ( -9.130526383799315582, 12.73969898348616070, 1.199719254218462483 ) ) ;
#178911 = CARTESIAN_POINT ( 'NONE',  ( 7.853197290813620945, 10.18514947741448573, 1.599625672291281386 ) ) ;
#178912 = CARTESIAN_POINT ( 'NONE',  ( 2.621219598810454965, -0.3864874759363098877, -0.1754412237054647494 ) ) ;
#178914 = FACE_OUTER_BOUND ( 'NONE', #59404, .T. ) ;
#178913 = CARTESIAN_POINT ( 'NONE',  ( 3.475057130574196407, 0.04366187338752242769, -1.825333387291371512 ) ) ;
#178915 = CARTESIAN_POINT ( 'NONE',  ( -3.147653791585729444, 8.999999999999998224, -2.419999999999998597 ) ) ;
#178916 = ORIENTED_EDGE ( 'NONE', *, *, #212859, .T. ) ;
#178917 = CARTESIAN_POINT ( 'NONE',  ( -5.790741006368224753, 5.928488393617260321, 0.7216878364870257245 ) ) ;
#178918 = CARTESIAN_POINT ( 'NONE',  ( 4.580108180932601414, 8.499999999999996447, -0.1719113009628105149 ) ) ;
#178919 = CARTESIAN_POINT ( 'NONE',  ( -6.333630315878337136, 10.54098580183340772, 0.000000000000000000 ) ) ;
#178920 = CARTESIAN_POINT ( 'NONE',  ( 6.322916996384010169, 1.495059732148263487, -1.358068445443241457 ) ) ;
#178921 = CARTESIAN_POINT ( 'NONE',  ( 0.8387270772249322270, 1.259995426201226953, -1.705408266269872630 ) ) ;
#178922 = ORIENTED_EDGE ( 'NONE', *, *, #155922, .F. ) ;
#178923 = CARTESIAN_POINT ( 'NONE',  ( -6.771371375382467583, 6.864631124226471037, -0.7998128361456362523 ) ) ;
#178924 = CARTESIAN_POINT ( 'NONE',  ( 2.236936919162732629, -0.08530413586980757634, -1.859100468073461965 ) ) ;
#178925 = CARTESIAN_POINT ( 'NONE',  ( 3.408985558832261731, 6.064568021024562938, 1.199719254218462483 ) ) ;
#178926 = CARTESIAN_POINT ( 'NONE',  ( 6.227427239534573999, -1.941376443541954488, 0.6920112976290059281 ) ) ;
#178927 = CARTESIAN_POINT ( 'NONE',  ( 6.082657761774012961, -0.6767167302549758068, 1.899617564980569773 ) ) ;
#178928 = VERTEX_POINT ( 'NONE', #130444 ) ;
#178929 = CARTESIAN_POINT ( 'NONE',  ( -4.042302355168801320, 7.867769847672247074, 0.7998128361456341429 ) ) ;
#178930 =( BOUNDED_CURVE ( )  B_SPLINE_CURVE ( 2, ( #107669, #91375, #203995, #189911, #157435, #154219, #192028 ),
 .UNSPECIFIED., .F., .T. ) 
 B_SPLINE_CURVE_WITH_KNOTS ( ( 3, 2, 2, 3 ),
 ( 0.2250000000000001998, 0.2291666666666669072, 0.2333333333333336701, 0.2375000000000003775 ),
 .UNSPECIFIED. ) 
 CURVE ( )  GEOMETRIC_REPRESENTATION_ITEM ( )  RATIONAL_B_SPLINE_CURVE ( ( 0.9999999999999937828, 0.8660254037844449249, 1.000000000000000000, 0.8660254037844387076, 1.000000000000000000, 0.8660254037844261621, 1.000000000000012434 ) ) 
 REPRESENTATION_ITEM ( '' )  );
#178931 = PLANE ( 'NONE',  #15171 ) ;
#178932 = CARTESIAN_POINT ( 'NONE',  ( 5.982890925380405456, 10.20206618957764100, 0.000000000000000000 ) ) ;
#178935 = ORIENTED_EDGE ( 'NONE', *, *, #115968, .T. ) ;
#178934 = CARTESIAN_POINT ( 'NONE',  ( -1.203941962966161627, 3.197768152887754844, -0.7749999999999883649 ) ) ;
#178933 = CARTESIAN_POINT ( 'NONE',  ( -5.991777542596674166, 5.955104985976372944, 0.000000000000000000 ) ) ;
#178936 = CARTESIAN_POINT ( 'NONE',  ( 6.308853223578811509, 6.964933332891984463, 0.9108697706533327443 ) ) ;
#178937 = CARTESIAN_POINT ( 'NONE',  ( 6.028672669474048007, 1.986741788447304646, -0.3418859329693338944 ) ) ;
#178938 = CARTESIAN_POINT ( 'NONE',  ( 4.224425198852012286, 0.09258891237720960621, 1.838934309869838968 ) ) ;
#178939 = CARTESIAN_POINT ( 'NONE',  ( 0.07700591528354226722, 2.040803078245361224, -2.328119179575589559 ) ) ;
#178940 = CARTESIAN_POINT ( 'NONE',  ( 3.475486094516122115, 0.05728489528775136674, -2.307140494302026390 ) ) ;
#178941 = CARTESIAN_POINT ( 'NONE',  ( 6.204791576909545192, 7.267953590263130259, -1.199719254218452047 ) ) ;
#178942 = CARTESIAN_POINT ( 'NONE',  ( 5.764953170560049855, -1.951456690425241947, -0.9300186209130756332 ) ) ;
#178943 = CARTESIAN_POINT ( 'NONE',  ( 7.796102023057898123, 9.054206100777749455, -1.199719254218441611 ) ) ;
#178944 = CARTESIAN_POINT ( 'NONE',  ( 0.8197486350577835035, 1.155594189952107609, -1.560708653158059622 ) ) ;
#178945 = CARTESIAN_POINT ( 'NONE',  ( -5.122283107864663343, 4.870418468797203637, 0.000000000000000000 ) ) ;
#178946 = ORIENTED_EDGE ( 'NONE', *, *, #163335, .F. ) ;
#178947 = ADVANCED_FACE ( 'NONE', ( #43804 ), #162658, .F. ) ;
#178948 = CARTESIAN_POINT ( 'NONE',  ( 4.622621100999918298, 0.5092349069827777353, -2.241135911243127055 ) ) ;
#178949 = DIRECTION ( 'NONE',  ( 0.000000000000000000, 0.000000000000000000, -1.000000000000000000 ) ) ;
#178950 = CARTESIAN_POINT ( 'NONE',  ( -5.655686355556086120, 6.627330832017406692, 1.199719254218452935 ) ) ;
#178951 = CARTESIAN_POINT ( 'NONE',  ( 4.715616592392388284, -1.834479983729628616, 0.3652084810651031743 ) ) ;
#178954 = CARTESIAN_POINT ( 'NONE',  ( -5.822300622425855110, 5.757381912443740646, 0.7998128361456281477 ) ) ;
#178953 = CARTESIAN_POINT ( 'NONE',  ( 1.499999999999987121, -0.2145833326505137972, 0.8660254037844524744 ) ) ;
#178952 = CARTESIAN_POINT ( 'NONE',  ( 1.845825534506392085, -1.251752223804462272, -1.445855903880132631 ) ) ;
#178955 = CARTESIAN_POINT ( 'NONE',  ( 3.158999515626020216, -1.670948785577108797, 1.441709373268922123 ) ) ;
#178956 = FACE_OUTER_BOUND ( 'NONE', #85753, .T. ) ;
#178957 = CARTESIAN_POINT ( 'NONE',  ( 7.336370518326124746, 7.731722824234849689, -0.7216878364870317197 ) ) ;
#178958 = CARTESIAN_POINT ( 'NONE',  ( -3.164938793786285842, 5.779846795137578930, -1.199719254218452935 ) ) ;
#178959 = CARTESIAN_POINT ( 'NONE',  ( -7.255021596644144921, 7.636815748939187465, 0.7216878364870317197 ) ) ;
#178960 = CARTESIAN_POINT ( 'NONE',  ( 1.633988421434044325, 0.9753176276560069358, -1.713140426071022349 ) ) ;
#178961 = CARTESIAN_POINT ( 'NONE',  ( 1.044460364342413072, 0.9324277726035223868, -2.110995228001291579 ) ) ;
#178962 = CARTESIAN_POINT ( 'NONE',  ( 2.910546574502240968, 0.6583626327048962557, 1.848246418561696913 ) ) ;
#178963 = CARTESIAN_POINT ( 'NONE',  ( 5.190308500716538376, 1.065014321051664048, -1.766232332728798538 ) ) ;
#178964 = CARTESIAN_POINT ( 'NONE',  ( 4.690757960648231695, 5.535267711253469614, 1.082531754730560403 ) ) ;
#178965 = CARTESIAN_POINT ( 'NONE',  ( 5.391302360089590628, 6.318882837306503575, -1.199719254218452047 ) ) ;
#178966 = EDGE_LOOP ( 'NONE', ( #89127, #82427, #8066, #120837 ) ) ;
#178967 = CARTESIAN_POINT ( 'NONE',  ( -1.201851678989727383E-14, 5.759375000341417028, -1.575800808251660801 ) ) ;
#178968 = CARTESIAN_POINT ( 'NONE',  ( 6.658747417465789908, -6.682123388833677069, 6.935047222998400152 ) ) ;
#178969 = CARTESIAN_POINT ( 'NONE',  ( 3.890826896997583884, 4.602014803661035103, -1.082531754730543083 ) ) ;
#178971 = AXIS2_PLACEMENT_3D ( 'NONE', #212953, #130730, #165281 ) ;
#178970 = CARTESIAN_POINT ( 'NONE',  ( 0.7081837076810155729, 0.6824709381345904768, -2.061040276042750641 ) ) ;
#178973 = CARTESIAN_POINT ( 'NONE',  ( 4.854701522145073334, 7.821512988214679218, -1.199719254218450271 ) ) ;
#178972 = FACE_OUTER_BOUND ( 'NONE', #116819, .T. ) ;
#178974 = CARTESIAN_POINT ( 'NONE',  ( 11.41126283316785361, 11.25874606908454645, -3.405403429622925415 ) ) ;
#178975 = CARTESIAN_POINT ( 'NONE',  ( -3.474999999999997868, -1.720833333333333659, 2.006292185433951047 ) ) ;
#178976 = CARTESIAN_POINT ( 'NONE',  ( 2.530351333283612281, 1.813318468827030072, 0.4585936022679508728 ) ) ;
#178977 = CARTESIAN_POINT ( 'NONE',  ( 6.555963963954187790, 2.156316573842661732, -0.1517529999496904924 ) ) ;
#178979 = CARTESIAN_POINT ( 'NONE',  ( 6.827182134110200806, 7.053609659044731472, 2.309100207511079805 ) ) ;
#178978 = CARTESIAN_POINT ( 'NONE',  ( -0.02264175331115856130, 5.720791440175713838, -2.683188945093956335 ) ) ;
#178980 = CARTESIAN_POINT ( 'NONE',  ( 0.6823417656249882723, -0.3239583329919110133, -1.181850606188749264 ) ) ;
#178981 = CARTESIAN_POINT ( 'NONE',  ( 2.191926089937683564, 1.177725938178806997, 1.506473034612793693 ) ) ;
#178982 = CARTESIAN_POINT ( 'NONE',  ( 3.695971326421595204, -1.767833007231565334, -0.08711813594433276409 ) ) ;
#178983 = CARTESIAN_POINT ( 'NONE',  ( 2.350135150926917493, 0.8998847150011926033, -1.687291145760522859 ) ) ;
#178984 = CARTESIAN_POINT ( 'NONE',  ( -5.850506979496850057, 6.784345216623154151, -1.199719254218446718 ) ) ;
#178986 = CARTESIAN_POINT ( 'NONE',  ( 5.079654255714375566, -0.6853159911496645718, 1.789018848640187231 ) ) ;
#178985 = CARTESIAN_POINT ( 'NONE',  ( 6.905598479220742547, -7.287292266636080207, -6.905598479220769192 ) ) ;
#178987 = CARTESIAN_POINT ( 'NONE',  ( 6.877413706903859669, -0.1509731808640407125, 1.936391978998742269 ) ) ;
#178988 = CARTESIAN_POINT ( 'NONE',  ( -1.499999999999997780, 5.150000000000022560, 1.214306433183764966E-14 ) ) ;
#178989 = CARTESIAN_POINT ( 'NONE',  ( 1.933984528066152953, -2.055706711753771287, 0.5200354980386610038 ) ) ;
#178990 = CARTESIAN_POINT ( 'NONE',  ( 4.627732503263369601, -1.150995203733524930, -1.474563928533303869 ) ) ;
#178992 = ORIENTED_EDGE ( 'NONE', *, *, #173979, .T. ) ;
#178991 = CARTESIAN_POINT ( 'NONE',  ( 2.103868193876055503, -1.825329726703457833, 0.04394198290156441783 ) ) ;
#178994 = CARTESIAN_POINT ( 'NONE',  ( -1.999999999999988010, -0.09816220177715248574, 0.5999999999999945377 ) ) ;
#178993 = CARTESIAN_POINT ( 'NONE',  ( 4.670673364294657404, -1.443042178620690841, 1.669811033208345341 ) ) ;
#178995 = CARTESIAN_POINT ( 'NONE',  ( -1.364683531250010295, 5.801041667008088432, -0.7879004041258300672 ) ) ;
#178996 = CARTESIAN_POINT ( 'NONE',  ( 1.469262158920743966, 1.818092299969736425, 0.9742969159239748267 ) ) ;
#178997 = CARTESIAN_POINT ( 'NONE',  ( 5.276094334012385367, 9.307193822989793475, 1.040834085586084257E-14 ) ) ;
#178998 = CARTESIAN_POINT ( 'NONE',  ( -7.340850106795412167, 10.65174332698158643, 1.199719254218453823 ) ) ;
#178999 =( NAMED_UNIT ( * ) PLANE_ANGLE_UNIT ( ) SI_UNIT ( $, .RADIAN. ) );
#179000 = CARTESIAN_POINT ( 'NONE',  ( 1.478151113144027251, 3.421726889910780667, 0.2686735943296981177 ) ) ;
#179001 = CARTESIAN_POINT ( 'NONE',  ( -1.000000000000017097, 8.600000000000013856, 0.4000000000000026867 ) ) ;
#179002 = CARTESIAN_POINT ( 'NONE',  ( 7.856023664475727308, 8.130058794835305136, -0.7998128361456341429 ) ) ;
#179003 = CIRCLE ( 'NONE', #5917, 0.09999999999999986677 ) ;
#179004 = EDGE_LOOP ( 'NONE', ( #17409, #161632, #109033, #25449 ) ) ;
#179005 = CARTESIAN_POINT ( 'NONE',  ( 4.615722581382986967, 0.4567890626981512270, -2.019179087418949692 ) ) ;
#179006 = CARTESIAN_POINT ( 'NONE',  ( 0.7499999999999902300, 5.816666666666685082, -1.299038105676658228 ) ) ;
#179007 = CARTESIAN_POINT ( 'NONE',  ( 2.460438939752376708, 0.9218109643280817389, 1.955300211207489980 ) ) ;
#179008 = CARTESIAN_POINT ( 'NONE',  ( -6.329889402343163773, 6.869280899661572626, -0.6830204514151876349 ) ) ;
#179009 = CARTESIAN_POINT ( 'NONE',  ( 1.682291859507994092, 1.040098842697153136, 1.731126528333865933 ) ) ;
#179010 = FACE_OUTER_BOUND ( 'NONE', #187361, .T. ) ;
#179011 = VERTEX_POINT ( 'NONE', #135743 ) ;
#179013 = CARTESIAN_POINT ( 'NONE',  ( 6.141480397310468575, 10.10888486359680982, 1.040834085586084257E-14 ) ) ;
#179012 = CARTESIAN_POINT ( 'NONE',  ( 6.928203230275514990, 14.48195938056239385, 9.797958971132711525 ) ) ;
#179014 = CARTESIAN_POINT ( 'NONE',  ( -3.621436428181653788, 7.239109909604962922, 0.7216878364870338292 ) ) ;
#179015 = CARTESIAN_POINT ( 'NONE',  ( 0.4093891192313535710, -1.913260280790154866, 0.6371585790938688598 ) ) ;
#179016 = CARTESIAN_POINT ( 'NONE',  ( 4.599289333468261631, -0.5842463895667610041, 2.112197083089427885 ) ) ;
#179017 = CARTESIAN_POINT ( 'NONE',  ( 1.499999999999990896, 4.056250000682819490, 1.214306433183764966E-14 ) ) ;
#179018 = CARTESIAN_POINT ( 'NONE',  ( 4.183787391381143195, 1.853651273288700718, -0.4697857328580385960 ) ) ;
#179019 = CARTESIAN_POINT ( 'NONE',  ( -4.548924232584923288, 5.265832011892554121, -1.199719254218446718 ) ) ;
#179020 = CARTESIAN_POINT ( 'NONE',  ( 7.266807146800403849, 7.580289214129690478, 1.040834085586084257E-14 ) ) ;
#179022 = CARTESIAN_POINT ( 'NONE',  ( 2.671500097371417137, 1.427951006967288272, 1.423949442620517702 ) ) ;
#179021 = CARTESIAN_POINT ( 'NONE',  ( -8.473482818416670170, 10.90881592628469932, -1.443375672974058777 ) ) ;
#179023 = CARTESIAN_POINT ( 'NONE',  ( -8.012344526598182026E-15, 12.60937500034139802, -1.575800808251669460 ) ) ;
#179024 = CARTESIAN_POINT ( 'NONE',  ( -3.980200614063634568, 6.801261928786307642, 1.199719254218452935 ) ) ;
#179025 = CARTESIAN_POINT ( 'NONE',  ( 5.368053323270940425, 0.8530656342727646058, 1.498931087277301843 ) ) ;
#179026 = CARTESIAN_POINT ( 'NONE',  ( 7.635176783151273128, 8.936736330878529699, 1.199719254218452935 ) ) ;
#179027 = CARTESIAN_POINT ( 'NONE',  ( 2.171277156482887882, 5.684907115872006145, -0.7998128361456291469 ) ) ;
#179028 = CARTESIAN_POINT ( 'NONE',  ( 1.499999999999987121, 3.827083334016153415, -0.8660254037844323793 ) ) ;
#179029 = VERTEX_POINT ( 'NONE', #201766 ) ;
#179030 = VECTOR ( 'NONE', #67109, 1000.000000000000114 ) ;
#179031 = CARTESIAN_POINT ( 'NONE',  ( 0.8837443060279138729, -1.967007789996034095, 0.6459356165888497925 ) ) ;
#179032 = EDGE_LOOP ( 'NONE', ( #13985, #170472, #48255, #24643, #129004, #71075, #71526, #126366 ) ) ;
#179033 = CARTESIAN_POINT ( 'NONE',  ( 4.547391301494094762, -1.654308909395687310, 0.7384720232115218330 ) ) ;
#179034 = CARTESIAN_POINT ( 'NONE',  ( 6.039231080244466199, 6.010467446565510130, 0.7998128361456352531 ) ) ;
#179035 = DIRECTION ( 'NONE',  ( -3.451266460341926649E-31, -5.200009205990155575E-32, 1.000000000000000000 ) ) ;
#179036 = CARTESIAN_POINT ( 'NONE',  ( 6.147087800311862971, 0.1847020338378597137, 1.802040927518679281 ) ) ;
#179037 = CARTESIAN_POINT ( 'NONE',  ( 6.522881301506172846, 6.782652071278222117, -0.7216878364870458196 ) ) ;
#179038 = CARTESIAN_POINT ( 'NONE',  ( 9.605376611548043897, 12.69998406307712457, 7.195705270794549691 ) ) ;
#179039 = CARTESIAN_POINT ( 'NONE',  ( 3.310656966840678894, 1.981231107410564851, 0.9368519390955745152 ) ) ;
#179040 = VERTEX_POINT ( 'NONE', #53406 ) ;
#179041 = AXIS2_PLACEMENT_3D ( 'NONE', #152039, #3609, #69687 ) ;
#179043 = CARTESIAN_POINT ( 'NONE',  ( 9.250740883225924804, 9.686952540052077509, 1.040834085586084257E-14 ) ) ;
#179042 = CARTESIAN_POINT ( 'NONE',  ( 0.9417639971489067952, 1.314929008279978495, 1.456166070238865018 ) ) ;
#179044 = CARTESIAN_POINT ( 'NONE',  ( 5.185127790529111991, 1.568658432645179124, 1.099198482053822534 ) ) ;
#179045 = CARTESIAN_POINT ( 'NONE',  ( 0.000000000000000000, -9.999999999999994671, 0.000000000000000000 ) ) ;
#179046 = FACE_OUTER_BOUND ( 'NONE', #124215, .T. ) ;
#179047 = CARTESIAN_POINT ( 'NONE',  ( -1.402160292154681736E-14, -0.3031249996585801965, -1.575800808251665908 ) ) ;
#179048 = CARTESIAN_POINT ( 'NONE',  ( 5.883875478650832491, 6.927238148923188454, -1.082531754730543083 ) ) ;
#179049 = CARTESIAN_POINT ( 'NONE',  ( -9.327646496521992958, 9.984601788804893019, -0.7216878364870267237 ) ) ;
#179050 = CARTESIAN_POINT ( 'NONE',  ( 2.149508875876861236, -1.735919364271593546, -1.288018159417112729 ) ) ;
#179051 = CARTESIAN_POINT ( 'NONE',  ( -5.309953438407606363, 6.223975762010839574, 1.199719254218452935 ) ) ;
#179052 = CARTESIAN_POINT ( 'NONE',  ( 3.366167277942881064, 7.149221934233827014, -0.7998128361456362523 ) ) ;
#179053 = CARTESIAN_POINT ( 'NONE',  ( 1.992912282819898850, 1.589903476415389871, -0.8970392876451321884 ) ) ;
#179054 = CARTESIAN_POINT ( 'NONE',  ( -2.916975605234527702, 6.554888639415577423, 1.040834085586084257E-14 ) ) ;
#179055 = CARTESIAN_POINT ( 'NONE',  ( 4.383705365265609721, 1.192707349210776036, 1.382196219385352309 ) ) ;
#179056 = CARTESIAN_POINT ( 'NONE',  ( 12.21012343519211285, 8.048746090400854314, -4.966865933635960850 ) ) ;
#179057 = CARTESIAN_POINT ( 'NONE',  ( 2.882959773793275726, -1.768624019741386277, -0.7279546805132871556 ) ) ;
#179058 = ORIENTED_EDGE ( 'NONE', *, *, #213686, .T. ) ;
#179059 = CARTESIAN_POINT ( 'NONE',  ( 3.754321382136751595, -1.967203782747016128, -0.09899598954335629697 ) ) ;
#179060 = VERTEX_POINT ( 'NONE', #119544 ) ;
#179061 = CARTESIAN_POINT ( 'NONE',  ( 4.915543477551369556, -1.042145293856342914, -1.638595356941417114 ) ) ;
#179062 = ORIENTED_EDGE ( 'NONE', *, *, #152080, .F. ) ;
#179063 = CARTESIAN_POINT ( 'NONE',  ( -5.855142236255304944, 7.924361590421551860, -1.599625672291271394 ) ) ;
#179065 = CARTESIAN_POINT ( 'NONE',  ( 5.256147377898004791, 0.8573370980917979223, -1.939729252509444279 ) ) ;
#179064 = CARTESIAN_POINT ( 'NONE',  ( 6.692885107001518286, 7.837396042037102717, -1.199719254218452047 ) ) ;
#179066 = ADVANCED_FACE ( 'NONE', ( #185529 ), #153048, .T. ) ;
#179068 = VERTEX_POINT ( 'NONE', #72846 ) ;
#179067 = CARTESIAN_POINT ( 'NONE',  ( 3.211475575234080004, 1.509012206799903666, 1.174515185244667581 ) ) ;
#179069 = CARTESIAN_POINT ( 'NONE',  ( 4.808669324434905690, 6.961940934708692019, -1.409791361277392241 ) ) ;
#179070 = CARTESIAN_POINT ( 'NONE',  ( 6.983263157960373668, 7.629137130509066722, 2.546189081643289942 ) ) ;
#179071 = CARTESIAN_POINT ( 'NONE',  ( -11.84668730067608600, 10.89999999999998259, 1.399999999999998579 ) ) ;
#179072 = CARTESIAN_POINT ( 'NONE',  ( 4.951819039462027838, -1.425199631963388391, -1.421988410718623586 ) ) ;
#179073 = CARTESIAN_POINT ( 'NONE',  ( 11.04536101718726293, 12.59418840193640854, -1.100000000000000311 ) ) ;
#179074 = CARTESIAN_POINT ( 'NONE',  ( 4.811078068098579408, 1.589968679568127596, 0.8971634079883783475 ) ) ;
#179075 = CARTESIAN_POINT ( 'NONE',  ( 1.240778115703184303, -2.019486815914430355, -0.4554155650244652853 ) ) ;
#179076 = CARTESIAN_POINT ( 'NONE',  ( -7.537970219518075332, 10.77775377520434574, -1.082531754730543971 ) ) ;
#179077 = CARTESIAN_POINT ( 'NONE',  ( -6.449404147558570166, 6.867377544759197150, 0.7074503392771516186 ) ) ;
#179078 = CARTESIAN_POINT ( 'NONE',  ( 1.464175926609780964E-14, -2.843749999044085541, -3.475000000000000533 ) ) ;
#179079 = CARTESIAN_POINT ( 'NONE',  ( 5.928550619183988957, 1.803260976426118489, 0.4972845834502263584 ) ) ;
#179080 = CARTESIAN_POINT ( 'NONE',  ( 7.070740804726770357, 8.207951346058097286, 1.199719254218462483 ) ) ;
#179081 = CARTESIAN_POINT ( 'NONE',  ( -5.298539104842322267, 5.076050465271134016, 0.7998128361456341429 ) ) ;
#179082 = CARTESIAN_POINT ( 'NONE',  ( 1.364683531249997417, 9.796875000341396245, 2.602085213965210642E-15 ) ) ;
#179083 = CARTESIAN_POINT ( 'NONE',  ( -4.900382456335551140, 7.804531068111707270, 1.199719254218464037 ) ) ;
#179085 = CARTESIAN_POINT ( 'NONE',  ( -4.678972410047611774, 5.591794245544547515, 1.082531754730549078 ) ) ;
#179084 = DIRECTION ( 'NONE',  ( 0.7592566023652995710, 0.6507913734559650498, 0.000000000000000000 ) ) ;
#179086 = CARTESIAN_POINT ( 'NONE',  ( -6.417086777969760902, 6.381022750586497594, 0.7998128361456341429 ) ) ;
#179087 = CARTESIAN_POINT ( 'NONE',  ( 1.077107760077404830, 1.911388382048292645, 0.7958064784282170567 ) ) ;
#179088 = EDGE_CURVE ( 'NONE', #184190, #32206, #208689, .T. ) ;
#179089 = CARTESIAN_POINT ( 'NONE',  ( 2.337658655405081110, 0.5614262474852428353, -2.041391482465891194 ) ) ;
#179090 = CARTESIAN_POINT ( 'NONE',  ( 6.903072767652295383, 11.20533532890304684, 1.040834085586084257E-14 ) ) ;
#179091 = CARTESIAN_POINT ( 'NONE',  ( 0.3914079065635613919, 3.043201908700355229, 0.4248930002254733829 ) ) ;
#179092 = CARTESIAN_POINT ( 'NONE',  ( 0.2683110675134177669, -0.8374301267611580224, -1.781048649993026700 ) ) ;
#179093 = CARTESIAN_POINT ( 'NONE',  ( 5.079507498475252625, 6.736975590279616455, 1.417308049988776020 ) ) ;
#179094 = CARTESIAN_POINT ( 'NONE',  ( 3.524756749872944628, 7.056040608253000279, -0.7216878364870267237 ) ) ;
#179096 = CARTESIAN_POINT ( 'NONE',  ( 6.670655732516626912, 7.629137130509076492, 2.426260288887295502 ) ) ;
#179095 = CARTESIAN_POINT ( 'NONE',  ( 1.737500000000001155, -3.733333333333331616, 3.009438278150922130 ) ) ;
#179097 = CARTESIAN_POINT ( 'NONE',  ( 2.554944377107245757, -1.995129818168206226, -1.128553997664314412 ) ) ;
#179098 = CARTESIAN_POINT ( 'NONE',  ( 0.3811277156573149583, 1.704729334087114578, -0.6539457117896372296 ) ) ;
#179099 = CARTESIAN_POINT ( 'NONE',  ( 1.880979024232478425, -1.749874716401520036, -0.7718601483891265325 ) ) ;
#179100 = CARTESIAN_POINT ( 'NONE',  ( 5.318541398310776103, 9.426991741329731056, -0.7998128361456481317 ) ) ;
#179101 = CARTESIAN_POINT ( 'NONE',  ( 6.439759776366765998, 9.496508258194486629, 1.082531754730558626 ) ) ;
#179102 =( BOUNDED_CURVE ( )  B_SPLINE_CURVE ( 2, ( #86636, #152703, #70356, #139683, #203556, #21597, #75718 ),
 .UNSPECIFIED., .F., .T. ) 
 B_SPLINE_CURVE_WITH_KNOTS ( ( 3, 2, 2, 3 ),
 ( 0.3571428571428574283, 0.3630952380952382486, 0.3690476190476191243, 0.3719163189456657359 ),
 .UNSPECIFIED. ) 
 CURVE ( )  GEOMETRIC_REPRESENTATION_ITEM ( )  RATIONAL_B_SPLINE_CURVE ( ( 0.9999999999999937828, 0.8660254037844449249, 1.000000000000000000, 0.8660254037844387076, 1.000000000000000000, 0.9354320710352564960, 0.9331000818465632340 ) ) 
 REPRESENTATION_ITEM ( '' )  );
#179103 = CARTESIAN_POINT ( 'NONE',  ( 2.021741635325131625, -0.4369018484469379682, 1.965087169840364245 ) ) ;
#179104 = CARTESIAN_POINT ( 'NONE',  ( 0.9538670997781794059, -0.7113550649951918547, 1.828410001767373450 ) ) ;
#179105 = CARTESIAN_POINT ( 'NONE',  ( -9.215791728987058562, 11.77484298861683598, -1.599625672291263179 ) ) ;
#179106 = CARTESIAN_POINT ( 'NONE',  ( -7.121056995675673740, 9.330985799753529264, -1.599625672291263179 ) ) ;
#179107 = CARTESIAN_POINT ( 'NONE',  ( -11.68273847554845446, 7.482503557960598961, 2.547333347333169407 ) ) ;
#179109 = CARTESIAN_POINT ( 'NONE',  ( 4.029968384200533826, 0.9465192177370416182, -1.495271383057869441 ) ) ;
#179108 = CARTESIAN_POINT ( 'NONE',  ( 4.558587588987070838, -1.867386427489168055, -0.9401465391167336261 ) ) ;
#179110 = CARTESIAN_POINT ( 'NONE',  ( 0.7124089920922128671, 16.00000000000000000, 12.66466791154580207 ) ) ;
#179112 = CARTESIAN_POINT ( 'NONE',  ( 6.210887435761151210, -0.2868632742878024500, 2.274177813689901573 ) ) ;
#179111 = FACE_OUTER_BOUND ( 'NONE', #72148, .T. ) ;
#179113 = CARTESIAN_POINT ( 'NONE',  ( 4.839680888265717407, 1.736017449284636527, 0.1234091131117609486 ) ) ;
#179114 = CARTESIAN_POINT ( 'NONE',  ( 8.809047120577066181, 11.30030761213851953, 1.599625672291281386 ) ) ;
#179115 =( LENGTH_UNIT ( ) NAMED_UNIT ( * ) SI_UNIT ( .MILLI., .METRE. ) );
#179116 = CARTESIAN_POINT ( 'NONE',  ( 4.288270029534011485, -1.659180151977168283, 0.5033209731903751649 ) ) ;
#179117 = CARTESIAN_POINT ( 'NONE',  ( 4.439989079487234314, 1.414935287217274684, 1.646911713943682409 ) ) ;
#179118 = CARTESIAN_POINT ( 'NONE',  ( 2.686486993802192913, 6.285985259411197568, 0.7998128361456362523 ) ) ;
#179119 = CARTESIAN_POINT ( 'NONE',  ( 5.471888747823221877, -0.9023485654677811940, 1.803414228490702209 ) ) ;
#179120 = CARTESIAN_POINT ( 'NONE',  ( 5.437500000000002665, 1.451031289060892737, -1.451031289061332608 ) ) ;
#179121 = VECTOR ( 'NONE', #174572, 1000.000000000000000 ) ;
#179122 = CARTESIAN_POINT ( 'NONE',  ( 1.499999999999990896, 5.056250000682820378, 1.214306433183764966E-14 ) ) ;
#179123 = CARTESIAN_POINT ( 'NONE',  ( 3.329043352767379282, 0.04595412404927168293, 1.925998307505512486 ) ) ;
#179124 = CARTESIAN_POINT ( 'NONE',  ( -1.500000000000008216, 10.03125000068279959, 3.469446951953614189E-15 ) ) ;
#179125 = CARTESIAN_POINT ( 'NONE',  ( 0.04794026018281431767, -2.028123841075918588, 0.9064578031776747702 ) ) ;
#179126 = VERTEX_POINT ( 'NONE', #71767 ) ;
#179127 = CARTESIAN_POINT ( 'NONE',  ( 6.883263157960382905, 3.691751545928231959, 2.560365603790202282 ) ) ;
#179128 = CARTESIAN_POINT ( 'NONE',  ( -1.500000000000013101, 3.129166666666689967, -0.8660254037844313801 ) ) ;
#179129 = CARTESIAN_POINT ( 'NONE',  ( 5.178324605415663306, 8.128796908705222535, 1.199719254218462483 ) ) ;
#179130 = CARTESIAN_POINT ( 'NONE',  ( 6.602011099637477010, 0.7519813002578833450, -1.812223124677159181 ) ) ;
#179131 = CARTESIAN_POINT ( 'NONE',  ( 8.432808358020029260, 8.940623960552603222, 0.7216878364870438212 ) ) ;
#179132 = CARTESIAN_POINT ( 'NONE',  ( -9.368320956918621434, 11.95279375453699622, 1.443375672974076540 ) ) ;
#179133 = CARTESIAN_POINT ( 'NONE',  ( 3.932747076415766596, 6.745899468197171345, 1.199719254218451159 ) ) ;
#179135 = AXIS2_PLACEMENT_3D ( 'NONE', #74107, #140200, #110935 ) ;
#179134 = AXIS2_PLACEMENT_3D ( 'NONE', #131926, #181680, #165445 ) ;
#179136 = FACE_OUTER_BOUND ( 'NONE', #84261, .T. ) ;
#179138 = CARTESIAN_POINT ( 'NONE',  ( 5.670399732568969675, -0.9243551164253935859, -1.844019960785907797 ) ) ;
#179137 = CARTESIAN_POINT ( 'NONE',  ( 8.055515824813896941, 12.54985222892493368, 0.7998128361456462443 ) ) ;
#179139 = SURFACE_STYLE_FILL_AREA ( #126194 ) ;
#179140 = CARTESIAN_POINT ( 'NONE',  ( -3.741160322367112379, 6.452105245148518797, 1.199719254218464037 ) ) ;
#179141 = CARTESIAN_POINT ( 'NONE',  ( -1.500000000000011324, 4.952083334016150751, 0.8660254037844403729 ) ) ;
#179142 = CARTESIAN_POINT ( 'NONE',  ( -1.402160292154681736E-14, 0.07187500034142156602, 1.575800808251672791 ) ) ;
#179143 = CARTESIAN_POINT ( 'NONE',  ( 0.1745949693968693039, 0.009193469831081376581, -1.755468632744116686 ) ) ;
#179144 = CARTESIAN_POINT ( 'NONE',  ( 5.924387396467542644, -1.262448726827345435, -1.189203582418095761 ) ) ;
#179145 = CARTESIAN_POINT ( 'NONE',  ( 4.968161617874263136, -1.641142972212021656, -0.5799033918824270106 ) ) ;
#179146 = CARTESIAN_POINT ( 'NONE',  ( 4.172158584703322681, 5.890604320285754980, -1.599625672291256295 ) ) ;
#179147 = CARTESIAN_POINT ( 'NONE',  ( 3.017397247018727580, -2.208655522623126366, 0.6135670354654331193 ) ) ;
#179148 = CARTESIAN_POINT ( 'NONE',  ( 1.364683531249988535, 5.467708333674750953, -0.7879004041258300672 ) ) ;
#179149 = CARTESIAN_POINT ( 'NONE',  ( 1.148114065366242498, -1.452583890646602205, 1.131155481815901753 ) ) ;
#179150 = CARTESIAN_POINT ( 'NONE',  ( 4.011676250333519711, 7.811283078717995210, 0.2953092252874019441 ) ) ;
#179151 = CARTESIAN_POINT ( 'NONE',  ( 1.469576158976824342E-15, 3.999999999999998224, -12.00000000000000355 ) ) ;
#179152 = CARTESIAN_POINT ( 'NONE',  ( 2.274178591966895091, -1.125271047149905890, 1.437439779654096750 ) ) ;
#179153 = CARTESIAN_POINT ( 'NONE',  ( 2.988907892087853568, -2.013985899409028946, 0.1017507309580278629 ) ) ;
#179154 = CARTESIAN_POINT ( 'NONE',  ( 1.482659311839970684, -0.3241159351022730450, -2.167229700873399612 ) ) ;
#179155 = CARTESIAN_POINT ( 'NONE',  ( 7.618117652040820253, 15.99345985719275909, -10.13859572747731264 ) ) ;
#179156 = CARTESIAN_POINT ( 'NONE',  ( 4.823321527849568469, -0.1059641466341002675, 2.103426968240690087 ) ) ;
#179157 = CARTESIAN_POINT ( 'NONE',  ( -7.739006755302186846, 7.923262724141010516, 0.7998128361456462443 ) ) ;
#179158 = CARTESIAN_POINT ( 'NONE',  ( 9.216031757539681735, 13.21158034223240918, 9.026211791306899102 ) ) ;
#179159 = CARTESIAN_POINT ( 'NONE',  ( 1.838419004579601834, -1.109345826794335688, 1.747895861591180156 ) ) ;
#179160 = CARTESIAN_POINT ( 'NONE',  ( 5.331380718671758778, 7.243030143248949670, -1.599625672291256295 ) ) ;
#179161 = CARTESIAN_POINT ( 'NONE',  ( -0.6801582343750091075, -1.036458332991943454, 1.178068619123817218 ) ) ;
#179162 = CARTESIAN_POINT ( 'NONE',  ( 3.774183692772983267, 2.104302197123971485, -0.2610650231627819062 ) ) ;
#179163 = CARTESIAN_POINT ( 'NONE',  ( 6.375623774462673587, 1.745513195383348926, -0.5351242734627087438 ) ) ;
#179164 = EDGE_LOOP ( 'NONE', ( #80342, #140673, #110079, #87123, #136485, #12529, #59153, #27283, #4374, #17286 ) ) ;
#179165 = CARTESIAN_POINT ( 'NONE',  ( -6.303615075710993665, 6.318915441276411471, -0.7998128361456362523 ) ) ;
#179166 = CARTESIAN_POINT ( 'NONE',  ( 8.224992744984721327, 12.74757530245756243, 1.040834085586084257E-14 ) ) ;
#179167 = CARTESIAN_POINT ( 'NONE',  ( 6.387299765369506055, 7.584842826753462219, -1.082531754730548412 ) ) ;
#179168 = CARTESIAN_POINT ( 'NONE',  ( -3.475000000000000533, -2.756249999044086074, 0.000000000000000000 ) ) ;
#179169 = CARTESIAN_POINT ( 'NONE',  ( -4.391951695823077984, 7.211361847513815704, 1.199719254218464037 ) ) ;
#179170 = CARTESIAN_POINT ( 'NONE',  ( 3.797132494115144308, -0.2020087959641834463, -2.009684039814496170 ) ) ;
#179171 = CARTESIAN_POINT ( 'NONE',  ( 1.026558790958994383, 1.254618057004111886, -1.691278660206218420 ) ) ;
#179172 = CARTESIAN_POINT ( 'NONE',  ( -4.956387674247580755, 7.940146832334256111, 1.199719254218452935 ) ) ;
#179173 = CARTESIAN_POINT ( 'NONE',  ( 7.727257484784855635, 11.10255193463598111, -1.199719254218446718 ) ) ;
#179174 = CARTESIAN_POINT ( 'NONE',  ( 4.856225966575771658, -1.860502807761035715, -0.04838197303517684927 ) ) ;
#179175 = CARTESIAN_POINT ( 'NONE',  ( 8.535021395002688749, 9.916278701380017324, 1.199719254218462483 ) ) ;
#179176 = CARTESIAN_POINT ( 'NONE',  ( -0.6384131795730932923, 4.335164563247821512, 0.1378994657016395786 ) ) ;
#179177 = CARTESIAN_POINT ( 'NONE',  ( -3.772911886352873445, 7.623757310712140800, 0.7998128361456352531 ) ) ;
#179179 = CARTESIAN_POINT ( 'NONE',  ( -10.15469386695561482, 10.94949038764413096, 1.040834085586084257E-14 ) ) ;
#179178 = TOROIDAL_SURFACE ( 'NONE', #23605, 3.970406073902761790, 0.08000000000000000167 ) ;
#179181 = CARTESIAN_POINT ( 'NONE',  ( 2.646866301197240645, -0.3325320220872363675, -1.933311746529025266 ) ) ;
#179180 = CARTESIAN_POINT ( 'NONE',  ( -5.682838942422375084, 9.781729199468104596, 0.000000000000000000 ) ) ;
#179182 = CARTESIAN_POINT ( 'NONE',  ( 1.323354039402934390, -0.05256100377049736927, 2.161234000603563299 ) ) ;
#179184 = CARTESIAN_POINT ( 'NONE',  ( -5.443514322282436702, 6.457176790571845792, 1.314492736914568027 ) ) ;
#179183 = CARTESIAN_POINT ( 'NONE',  ( -6.231907884136888676, 7.299589282028351001, -1.199719254218453823 ) ) ;
#179185 = CARTESIAN_POINT ( 'NONE',  ( -1.402160292154681736E-14, 0.4468750003414233563, -1.575800808251665908 ) ) ;
#179186 = CARTESIAN_POINT ( 'NONE',  ( 3.057622914094188626, 1.488722154369751083, -0.8884403576015533766 ) ) ;
#179187 = CARTESIAN_POINT ( 'NONE',  ( 1.974151807821213245, -0.08369685440555743594, -1.738446472377056740 ) ) ;
#179189 = CARTESIAN_POINT ( 'NONE',  ( 7.456621297836072415, 9.722477485607340597, 1.443375672974076540 ) ) ;
#179188 = CARTESIAN_POINT ( 'NONE',  ( 0.3765545373161778286, 1.332373789618445770, 1.883912488508274752 ) ) ;
#179190 = CARTESIAN_POINT ( 'NONE',  ( -11.37834099079384487, 6.126291437673294205, 3.408052918099385931 ) ) ;
#179191 = CARTESIAN_POINT ( 'NONE',  ( 2.723961130741957781, -1.183836802208296568, -1.686624133856133412 ) ) ;
#179192 = AXIS2_PLACEMENT_3D ( 'NONE', #18632, #33825, #133504 ) ;
#179193 = ADVANCED_FACE ( 'NONE', ( #75002 ), #124900, .T. ) ;
#179194 = CARTESIAN_POINT ( 'NONE',  ( 0.6146109705059289441, 0.6351056948852469297, -1.913509406280079705 ) ) ;
#179195 = CARTESIAN_POINT ( 'NONE',  ( 6.925078400183548588, 3.689301810296021777, 2.558360072861276979 ) ) ;
#179196 = CARTESIAN_POINT ( 'NONE',  ( -5.469788628470539926, 5.346117919495872783, -0.7998128361456362523 ) ) ;
#179197 = CARTESIAN_POINT ( 'NONE',  ( 1.604304721248978494, -0.7076282383621353977, -1.840268529672415498 ) ) ;
#179199 = CARTESIAN_POINT ( 'NONE',  ( -4.828112100242279325, 8.646898193675708555, -0.7216878364870338292 ) ) ;
#179198 = CARTESIAN_POINT ( 'NONE',  ( 4.834190613173367623, -1.027981871586785889, -1.612434056610718480 ) ) ;
#179200 = CARTESIAN_POINT ( 'NONE',  ( -7.390603132780803719, 7.794994207765291172, -0.7216878364870338292 ) ) ;
#179201 = CARTESIAN_POINT ( 'NONE',  ( 6.607619761813720238, 8.802252036906432764, 1.599625672291268286 ) ) ;
#179202 = EDGE_CURVE ( 'NONE', #117081, #11196, #122782, .T. ) ;
#179203 = CARTESIAN_POINT ( 'NONE',  ( -7.306918443122272677, 7.489436036589583345, 0.7998128361456341429 ) ) ;
#179204 = CARTESIAN_POINT ( 'NONE',  ( 1.647134723225437636, 0.2000593722277475561, 2.009751748981201569 ) ) ;
#179205 = DIRECTION ( 'NONE',  ( 0.000000000000000000, 0.000000000000000000, -1.000000000000000000 ) ) ;
#179206 = CARTESIAN_POINT ( 'NONE',  ( 4.577368073103933455, 0.004851830007264032810, -2.307758714736147798 ) ) ;
#179207 = CARTESIAN_POINT ( 'NONE',  ( 5.951606347324345236, 1.484592722905058393, 1.282605414028796353 ) ) ;
#179208 = CARTESIAN_POINT ( 'NONE',  ( 2.377722661024490147, -1.904092233959910896, 0.4717398701708991893 ) ) ;
#179209 = CYLINDRICAL_SURFACE ( 'NONE', #154246, 0.05000000000000002359 ) ;
#179210 = VERTEX_POINT ( 'NONE', #138951 ) ;
#179211 = CARTESIAN_POINT ( 'NONE',  ( 0.9193374879241524855, -1.911445915896703207, 0.9111208566532496000 ) ) ;
#179213 = CARTESIAN_POINT ( 'NONE',  ( -7.182068686937172153, 9.402166106225269715, 1.599625672291283607 ) ) ;
#179212 = CARTESIAN_POINT ( 'NONE',  ( -5.087333953625788219, 6.958308917361963886, 1.599625672291267398 ) ) ;
#179214 = CARTESIAN_POINT ( 'NONE',  ( 0.4976878544296211571, -0.6176706345307935164, -1.734562967469073014 ) ) ;
#179215 = ORIENTED_EDGE ( 'NONE', *, *, #190788, .T. ) ;
#179216 = CARTESIAN_POINT ( 'NONE',  ( 3.854478708947015164, -2.168323188329326801, -0.1120144502513506779 ) ) ;
#179217 = CARTESIAN_POINT ( 'NONE',  ( 11.92064487511310666, 7.617312143620704745, -0.8788818785119806298 ) ) ;
#179218 = CARTESIAN_POINT ( 'NONE',  ( 2.180079139336263516, 2.078761533942363737, -0.4183221158333137457 ) ) ;
#179219 = CARTESIAN_POINT ( 'NONE',  ( -1.499999999999997780, 3.431250000682818602, 1.214306433183764966E-14 ) ) ;
#179220 = CARTESIAN_POINT ( 'NONE',  ( 8.589254009457354400, 9.979550084910457031, -1.199719254218446718 ) ) ;
#179221 = CARTESIAN_POINT ( 'NONE',  ( -1.858076449550070564, 2.486042365337548521, -2.481448873923816745 ) ) ;
#179222 = CARTESIAN_POINT ( 'NONE',  ( 2.917317126705867736, -0.2052410828034083035, 2.050554836033135597 ) ) ;
#179224 = CARTESIAN_POINT ( 'NONE',  ( 0.4679805871025365382, -1.733519288248483559, -0.6209854868195128219 ) ) ;
#179223 = CARTESIAN_POINT ( 'NONE',  ( -8.341290820905609138, 10.75459192918846618, 1.599625672291269396 ) ) ;
#179225 = CARTESIAN_POINT ( 'NONE',  ( -0.6823417656249969321, 3.217708333674754062, -1.181850606188749264 ) ) ;
#179226 = CARTESIAN_POINT ( 'NONE',  ( 0.07735805125223639556, 7.629137130509110243, -2.688903128390319530 ) ) ;
#179227 = CARTESIAN_POINT ( 'NONE',  ( 1.369767765231834300, 4.288585766148679035, -0.2488260012212581695 ) ) ;
#179228 = CARTESIAN_POINT ( 'NONE',  ( 0.4170028235400899397, 1.518763190251697370, -1.601383572969114599 ) ) ;
#179229 = CARTESIAN_POINT ( 'NONE',  ( 2.864839704461724867, -1.562160111903969417, 1.636705750015782224 ) ) ;
#179230 = CARTESIAN_POINT ( 'NONE',  ( -7.849807752632384172, 12.10193344480572897, 0.000000000000000000 ) ) ;
#179232 = EDGE_CURVE ( 'NONE', #211538, #182913, #163733, .T. ) ;
#179231 = CARTESIAN_POINT ( 'NONE',  ( 2.144508837627901343, 1.757922920557394519, 0.4371675498636724000 ) ) ;
#179233 = CARTESIAN_POINT ( 'NONE',  ( 1.797909001537282503, -0.9065369449853509787, -1.687681949719927577 ) ) ;
#179234 = CIRCLE ( 'NONE', #16541, 0.08000000000000012657 ) ;
#179235 = CARTESIAN_POINT ( 'NONE',  ( 3.314952806421948672, -1.569539724514938950, 1.350292352848787569 ) ) ;
#179236 = CARTESIAN_POINT ( 'NONE',  ( -0.6823417656250003738, 1.280208333674752508, -1.181850606188749264 ) ) ;
#179237 = CARTESIAN_POINT ( 'NONE',  ( 1.305477374917118016, -0.4809445013957516779, 1.911780493352131183 ) ) ;
#179238 = CARTESIAN_POINT ( 'NONE',  ( 0.4109946218407485308, 1.674316264148696165, 0.9526004100348076653 ) ) ;
#179239 = CARTESIAN_POINT ( 'NONE',  ( 2.483090063216564669, 1.711211315118581711, -0.7561169667836544761 ) ) ;
#179241 = CARTESIAN_POINT ( 'NONE',  ( 5.213898493288036562, 7.712005038449616379, -1.200564631081424416 ) ) ;
#179240 = CARTESIAN_POINT ( 'NONE',  ( 1.313548042387347348, 2.037171730821058624, 1.084164666379479502 ) ) ;
#179242 = CARTESIAN_POINT ( 'NONE',  ( 3.086215985183130339, 1.036139677906501300, -1.545717422611452729 ) ) ;
#179243 = CARTESIAN_POINT ( 'NONE',  ( 0.6823417656249882723, 2.926041667008084879, -1.181850606188754593 ) ) ;
#179244 = CARTESIAN_POINT ( 'NONE',  ( 5.107907679073590224, 0.6501100083472023394, -1.957599679411163196 ) ) ;
#179245 = CARTESIAN_POINT ( 'NONE',  ( -6.087774667736030487, 7.061157519568837415, 1.199719254218450271 ) ) ;
#179246 = CARTESIAN_POINT ( 'NONE',  ( 6.265839547809997079, 10.46189657242035587, 0.7998128361456462443 ) ) ;
#179247 = CARTESIAN_POINT ( 'NONE',  ( -1.436275828743291516, 3.619984746957625621, -0.4487520553618166153 ) ) ;
#179248 = CARTESIAN_POINT ( 'NONE',  ( -0.02264175331115856477, -0.002534049983802035520, -2.089079740194145440 ) ) ;
#179249 = ADVANCED_FACE ( 'NONE', ( #26233 ), #137883, .T. ) ;
#179250 = CARTESIAN_POINT ( 'NONE',  ( -0.6823417656250212460, 3.113541667008084879, 1.181850606188767472 ) ) ;
#179251 = CARTESIAN_POINT ( 'NONE',  ( 6.327428285124779173, -2.037722512857220725, 0.7216720553550812767 ) ) ;
#179252 = CARTESIAN_POINT ( 'NONE',  ( 0.7492455685023796663, 1.839184785914184994, -0.09005233288367914257 ) ) ;
#179253 = CARTESIAN_POINT ( 'NONE',  ( 5.110023566311792997, -0.7249756751233800145, 1.885263354437803240 ) ) ;
#179254 = CARTESIAN_POINT ( 'NONE',  ( -1.364683531250014514, -0.2197916663252438285, 0.7879004041258379498 ) ) ;
#179255 = CARTESIAN_POINT ( 'NONE',  ( -4.284013352238250860, 7.941839977679187257, -0.7216878364870267237 ) ) ;
#179256 = EDGE_CURVE ( 'NONE', #170920, #1432, #129059, .T. ) ;
#179259 = CARTESIAN_POINT ( 'NONE',  ( 3.538314903486612817, 7.071858454135611538, 1.040834085586084257E-14 ) ) ;
#179258 = CARTESIAN_POINT ( 'NONE',  ( 6.825078400183548055, 2.475450427997231362, 2.140471860334830279 ) ) ;
#179257 = CARTESIAN_POINT ( 'NONE',  ( 6.737475991348287785, 6.825086509519945999, -0.7998128361456481317 ) ) ;
#179260 = CARTESIAN_POINT ( 'NONE',  ( -5.113360211009450040, 5.994616996712990975, -1.199719254218453823 ) ) ;
#179261 = CARTESIAN_POINT ( 'NONE',  ( 5.102750050473856547, 1.865045247124358818, 0.7672954931761333253 ) ) ;
#179262 = CARTESIAN_POINT ( 'NONE',  ( -6.340409392685171674, 10.54889472477470846, 0.7998128361456481317 ) ) ;
#179264 = CARTESIAN_POINT ( 'NONE',  ( -6.956742217143487395, 8.249192353823097790, 1.082531754730549078 ) ) ;
#179263 = CARTESIAN_POINT ( 'NONE',  ( -3.602716132929368875, 5.226254793216122074, 1.599625672291267398 ) ) ;
#179265 = CARTESIAN_POINT ( 'NONE',  ( -1.201851678989727383E-14, 4.946875000341420581, -1.575800808251660134 ) ) ;
#179267 = CARTESIAN_POINT ( 'NONE',  ( -8.012344526598182026E-15, 9.296875000341398021, -1.575800808251669460 ) ) ;
#179266 = CARTESIAN_POINT ( 'NONE',  ( 6.104392421991035711, -0.7735064434604683736, -2.018760209060527888 ) ) ;
#179268 = CARTESIAN_POINT ( 'NONE',  ( -11.84668730067608777, 13.50634727754793651, 1.399999999999998579 ) ) ;
#179269 = CARTESIAN_POINT ( 'NONE',  ( -11.86644718583810132, 7.726483972532615319, -1.803327366047848157 ) ) ;
#179271 = CARTESIAN_POINT ( 'NONE',  ( 5.343375128634678006, 0.3905785925618041610, -1.978055652833633271 ) ) ;
#179270 = CARTESIAN_POINT ( 'NONE',  ( -5.382223794500827552, 9.223085493652217082, -0.7216878364870207285 ) ) ;
#179272 = CARTESIAN_POINT ( 'NONE',  ( 1.364683531249988757, -0.3031249996585799744, 0.000000000000000000 ) ) ;
#179273 = B_SPLINE_CURVE_WITH_KNOTS ( 'NONE', 3,
 ( #194732, #14894, #112489, #159048, #161181, #12767, #80988, #110365, #78842, #60469, #196866, #128758, #144962, #210968, #47445, #178499, #114624, #146019, #95132, #30109, #31185, #209901, #62596, #147077, #11713, #96200, #213098, #10640, #63673, #180614, #143908, #13836, #193666, #61539, #94070, #195809, #179564, #44244, #113561, #126626, #32239, #97258, #64728, #76716, #130871, #192589, #176370, #127705, #27977, #160111, #45309, #111427, #177432, #98310, #49548, #119961, #99379, #68977, #167574, #36496, #20237, #202173, #164374, #116743, #182743, #34361, #200054, #168634, #135096, #19173, #1841, #185936, #214137, #100434, #134044, #166505, #51703, #201110, #18096, #183816, #761, #184870, #52750, #132971, #150272, #84184, #118884, #53831, #15959, #83105, #65765, #115673, #131911, #67900, #149186, #102574, #117826, #86322, #35426, #82042, #101504, #197920, #181668, #148136, #165432, #85247, #2905, #198973, #33295, #152394, #3973, #17028, #66828, #70040, #50618, #136156, #151336, #88474, #23438, #174011, #104725, #140456, #122116, #7185, #172930, #125314, #155600, #72184, #9343, #38647, #153464, #40799, #169702, #87397, #189160, #206467, #6113, #190213, #25582, #103652, #123199, #73257, #154533, #5037, #171845, #121047, #71112, #8268, #90618, #138292, #37571, #21292, #205394, #137229, #124255, #74352, #41873, #204307, #188081, #107984, #156675, #39710, #89549, #105819, #203250, #54894, #187015, #55964, #91693, #139363, #106905, #57032, #24507, #58094, #157746, #170773, #75416, #22362, #141529, #207537, #59156, #127457, #144724, #63431, #210736, #179328, #209655, #94885, #194491, #79675, #61296, #160937, #112250, #64496, #12532, #11466, #163077, #192340, #92755, #46134, #109048, #178261, #158800, #212860, #43999, #29874, #110117, #97023, #95958, #78604, #93823, #10397, #111183, #60222, #76471, #162012, #13602, #77539, #191273, #175067, #62361, #193428, #145790, #176129, #211794, #26654, #129584, #195570, #80752, #45072, #177187, #28800, #142581, #42939, #208587, #143661, #47206, #128522, #113321, #30949, #14659, #146840, #27728, #126381, #159864, #196630, #18912, #152143, #131676, #101244, #199801, #68724, #52499, #36234, #84996, #184617, #168386, #118632, #100186, #1585, #16781, #51446, #34114, #3710, #32003, #132723, #166251, #66581, #83926, #167326, #198728, #67646, #33060, #130638, #99138, #50374, #17841, #114384, #102312, #182486, #19982, #115439, #98084, #147891, #164139, #150015, #181430, #151087, #133793, #134846, #117566, #48271, #116497, #183560, #200850, #81809, #35167, #180379, #86066, #2651, #15723, #213907, #65530, #197678, #49323, #165188, #82865, #148941, #514, #70851, #74093, #202993, #121851, #54632, #40536, #135895, #139100, #156414, #106639, #104463, #187823, #123996, #39449, #189963, #120779, #172667, #24244, #206206, #88205, #153203, #154277, #138032, #41613, #6921, #136965, #53566, #4773, #185683, #21033, #173751, #186758, #107725, #105544, #71923, #204046, #90345, #171578, #25329, #56771, #5852, #23174, #8002, #89288, #57834, #55696, #155338, #72998, #140185, #205128, #122937, #188894, #38382, #91429, #170511, #22093, #157491, #69787, #201913, #169448, #119700, #37312, #103386, #87131, #210477, #76217, #129339, #62115, #127200, #126122, #191017, #143398, #12273, #10141, #78349, #9085, #174818, #108792 ),
 .UNSPECIFIED., .F., .F.,
 ( 4, 1, 1, 1, 1, 1, 1, 1, 1, 1, 1, 1, 1, 1, 1, 1, 1, 1, 1, 1, 1, 1, 1, 1, 1, 1, 1, 1, 1, 1, 1, 1, 1, 1, 1, 1, 1, 1, 1, 1, 1, 1, 1, 1, 1, 1, 1, 1, 1, 1, 1, 1, 1, 1, 1, 1, 1, 1, 1, 1, 1, 1, 1, 1, 1, 1, 1, 1, 1, 1, 1, 1, 1, 1, 1, 1, 1, 1, 1, 1, 1, 1, 1, 1, 1, 1, 1, 1, 1, 1, 1, 1, 1, 1, 1, 1, 1, 1, 1, 1, 1, 1, 1, 1, 1, 1, 1, 1, 1, 1, 1, 1, 1, 1, 1, 1, 1, 1, 1, 1, 1, 1, 1, 1, 1, 1, 1, 1, 1, 1, 1, 1, 1, 1, 1, 1, 1, 1, 1, 1, 1, 1, 1, 1, 1, 1, 1, 1, 1, 1, 1, 1, 1, 1, 1, 1, 1, 1, 1, 1, 1, 1, 1, 1, 1, 1, 1, 1, 1, 1, 1, 1, 1, 1, 1, 1, 1, 1, 1, 1, 1, 1, 1, 1, 1, 1, 1, 1, 1, 1, 1, 1, 1, 1, 1, 1, 1, 1, 1, 1, 1, 1, 1, 1, 1, 1, 1, 1, 1, 1, 1, 1, 1, 1, 1, 1, 1, 1, 1, 1, 1, 1, 1, 1, 1, 1, 1, 1, 1, 1, 1, 1, 1, 1, 1, 1, 1, 1, 1, 1, 1, 1, 1, 1, 1, 1, 1, 1, 1, 1, 1, 1, 1, 1, 1, 1, 1, 1, 1, 1, 1, 1, 1, 1, 1, 1, 1, 1, 1, 1, 1, 1, 1, 1, 1, 1, 1, 1, 1, 1, 1, 1, 1, 1, 1, 1, 1, 1, 1, 1, 1, 1, 1, 1, 1, 1, 1, 1, 1, 1, 1, 1, 1, 1, 1, 1, 1, 1, 1, 1, 1, 1, 1, 1, 1, 1, 1, 1, 1, 1, 1, 1, 1, 1, 1, 1, 1, 1, 1, 1, 1, 1, 1, 1, 1, 1, 1, 1, 1, 1, 1, 1, 1, 1, 1, 1, 1, 1, 1, 1, 1, 1, 1, 1, 1, 1, 1, 1, 1, 1, 1, 1, 1, 1, 1, 1, 1, 1, 1, 1, 1, 1, 1, 1, 1, 1, 1, 1, 1, 1, 1, 1, 1, 1, 4 ),
 ( 0.000000000000000000, 0.002599878613971510263, 0.005208762566300055921, 0.007813076245110234588, 0.01041697056762492211, 0.01302017924898362516, 0.01562522799165661294, 0.01822895742955179393, 0.02083332403451576206, 0.02343772221867868391, 0.02604143078293654281, 0.02864626161639613477, 0.03124961764961396021, 0.03385452714844047750, 0.03645799780571232912, 0.03906266225314121432, 0.04166671052383312535, 0.04427076094224517699, 0.04687542278318937439, 0.04947889361195772356, 0.05208380280015859759, 0.05468715921365963767, 0.05729198803509916865, 0.05989568673917144287, 0.06250009379223495087, 0.06510449848632135494, 0.06770819839843210397, 0.07031302545632363288, 0.07291638160390327694, 0.07552129054917994244, 0.07812475961953217751, 0.08072942239586503033, 0.08333346963797970408, 0.08593751866472883194, 0.08854217935802578821, 0.09114564884740632145, 0.09375055680876714925, 0.09635391199924973893, 0.09895873945611717570, 0.1015624370353711836, 0.1041668426700886191, 0.1067712463110160465, 0.1093749448896196713, 0.1119797708301935452, 0.1145831257515418783, 0.1171880334468678037, 0.1197915013940491491, 0.1223961628153678316, 0.1250002090321265524, 0.1276042567216372492, 0.1302089163955687523, 0.1328123846563000476, 0.1354172914881497103, 0.1380206455552074885, 0.1406254717515977581, 0.1432291683081768907, 0.1458335726268597532, 0.1484379753169847160, 0.1510416726638619811, 0.1536464975900906083, 0.1562498513865758776, 0.1588547579349887939, 0.1614582248604825021, 0.1640628850295551278, 0.1666669303230295940, 0.1692709767774011609, 0.1718756355346959253, 0.1744791026682601387, 0.1770840084736199360, 0.1796873615186004858, 0.1822921865574477218, 0.1848958821930496710, 0.1875002852981585977, 0.1901046871399069693, 0.1927083833567690418, 0.1953132073715553307, 0.1979165601445126987, 0.2005214656490191816, 0.2031249316542690642, 0.2057295906738217384, 0.2083336351460475244, 0.2109376804673406547, 0.2135423384106908962, 0.2161458045185324639, 0.2187507094003866837, 0.2213540615246011867, 0.2239588855088016361, 0.2265625803250888304, 0.2291669823190463362, 0.2317713834148095453, 0.2343750786033309830, 0.2369799018095430365, 0.2395832536602726381, 0.2421881582238437913, 0.2447916234102597566, 0.2473962813829825302, 0.2500003251359625422, 0.2526043694262022354, 0.2552090266582678346, 0.2578124918417971090, 0.2604173959030967600, 0.2630207472078238129, 0.2656255702402394725, 0.2682292643388430320, 0.2708336653240377978, 0.2734380657761767419, 0.2760417600379992398, 0.2786465825384744077, 0.2812499335682448476, 0.2838548372938197173, 0.2864583017627815864, 0.2890629587913320364, 0.2916670019270400371, 0.2942710452882197347, 0.2968757019116316509, 0.2994791662722288139, 0.3020840696158954564, 0.3046874202023847622, 0.3072922423858477359, 0.3098959358683710530, 0.3125003359471613118, 0.3151047358580104651, 0.3177084292947467969, 0.3203132511922952008, 0.3229166015023476888, 0.3255215044928377321, 0.3281249683456989308, 0.3307296245327063788, 0.3333336671530912065, 0.3359377096871765112, 0.3385423658045411677, 0.3411458294435600336, 0.3437507321724898035, 0.3463540821419661686, 0.3489589035792820537, 0.3515625965473047621, 0.3541669958220223235, 0.3567713952938928457, 0.3593750880071304721, 0.3619799094045394461, 0.3645832590960911834, 0.3671881614543835437, 0.3697916247924753486, 0.3723962802405443862, 0.3750003224475334518, 0.3776043642564660408, 0.3802090199703688222, 0.3828124829891406122, 0.3854173852062082184, 0.3880207346598750218, 0.3906255554538268782, 0.3932292480089087938, 0.3958336465818629857, 0.3984380457170473289, 0.4010417378083525053, 0.4036465588083897882, 0.4062499079826380477, 0.4088548098116001062, 0.4114582727362346981, 0.4140629275479489335, 0.4166669694434522730, 0.4192710106291533956, 0.4218756660421624782, 0.4244791285419997062, 0.4270840303500617607, 0.4296873793891050619, 0.4322921996424575197, 0.4348958918861421385, 0.4375002898596233591, 0.4401046887603987101, 0.4427083803313200949, 0.4453132010367379379, 0.4479165497948640051, 0.4505214511973463787, 0.4531249138098211726, 0.4557295680877478938, 0.4583336097736617210, 0.4609376504380365280, 0.4635423056527069874, 0.4661457677349071238, 0.4687506692368063055, 0.4713540179623986193, 0.4739588377779012651, 0.4765625298117197040, 0.4791669272880037522, 0.4817713260566358624, 0.4843750172087082362, 0.4869798377222476216, 0.4895831861654201811, 0.4921880872442612742, 0.4947915496458628049, 0.4973962034925555886, 0.5000002450707665691, 0.5026042853157074441, 0.5052089404345847523, 0.5078124022004342208, 0.5104173034990032720, 0.5130206520123070657, 0.5156254714926987726, 0.5182291634181735995, 0.5208335604995248946, 0.5234379592382720769, 0.5260416500730202838, 0.5286464704974140894, 0.5312498187267931105, 0.5338547195848227789, 0.5364581818768299204, 0.5390628353948335727, 0.5416668769672219330, 0.5442709168946127107, 0.5468755720202369552, 0.5494790335710144635, 0.5520839347690799093, 0.5546872831712518215, 0.5572921024192640793, 0.5598957943379132551, 0.5625001911265891108, 0.5651045899377058479, 0.5677082805566486812, 0.5703131009946261765, 0.5729164491113668545, 0.5755213498514099024, 0.5781248121350983649, 0.5807294654269519185, 0.5833335070953961088, 0.5859375468071157389, 0.5885422020420250089, 0.5911456634790059894, 0.5937505646793920233, 0.5963539130715860281, 0.5989587321899475514, 0.6015624242032879820, 0.6041668208015419372, 0.6067712197872831004, 0.6093749102919370220, 0.6119797308462270324, 0.6145830789514836745, 0.6171879796763642956, 0.6197914420530098445, 0.6223960952212510556, 0.6250001370876311357, 0.6276041766855571247, 0.6302088321322918407, 0.6328122935567517260, 0.6354171948622837629, 0.6380205433456558328, 0.6406253624370956690, 0.6432290546466469250, 0.6458334511567334069, 0.6484378504193577530, 0.6510415409112403351, 0.6536463616845760161, 0.6562497098795055939, 0.6588546106920506462, 0.6614580732629331550, 0.6640627264101022220, 0.6666667685763031370, 0.6692708081623160998, 0.6718754639234225667, 0.6744789254366408970, 0.6770838269501499029, 0.6796871756258610064, 0.6822919947931124218, 0.6848956873004010681, 0.6875000838245786117, 0.6901044834663523364, 0.6927081740469867022, 0.6953129951421085364, 0.6979163435278744609, 0.7005212445309179081, 0.7031247073973251327, 0.7057293606259679164, 0.7083334031938842701, 0.7109374428698714832, 0.7135420990479055536, 0.7161455607511696408, 0.7187504625754957965, 0.7213538115447158949, 0.7239586308905210377, 0.7265623237970838533, 0.7291667204376187650, 0.7317711205608201652, 0.7343748113317387638, 0.7369796328513985584, 0.7395829815291747877, 0.7421878828255610294, 0.7447913460887924941, 0.7473959995014650692, 0.7500000425730045661, 0.7526040824408628538, 0.7552087391383944803, 0.7578122011330034047, 0.7604171033709996586, 0.7630204527349119248, 0.7656252723620247114, 0.7682289657694127971, 0.7708333626285834850, 0.7734377633355060677, 0.7760414543982535607, 0.7786462764452187768, 0.7812496255161931469, 0.7838545272087811266, 0.7864579909701516769, 0.7890626446694239959, 0.7916666883465109938, 0.7942707285081521684, 0.7968753858277685120, 0.7994788482150362308, 0.8020837509695725176, 0.8046871008293766669, 0.8072919208405671121, 0.8098956148503495545, 0.8125000120304503026, 0.8151044134234068927, 0.8177081048795449281, 0.8203129275566022338, 0.8229162771219805661, 0.8255211793136476572, 0.8281246436744912343, 0.8307292977629509023, 0.8333333421475307423, 0.8359373827048843797, 0.8385420407491936956, 0.8411455036304537058, 0.8437504070044209437, 0.8463537574613370085, 0.8489585779593948889, 0.8515622726731627568, 0.8541666702765071673, 0.8567710724578335713, 0.8593747644089445581, 0.8619795878189033811, 0.8645829379799131464, 0.8671878407735589267, 0.8697913058352330085, 0.8723959604154888359, 0.8750000056095312839, 0.8776040466645483873, 0.8802087055361843548, 0.8828121690127931354, 0.8854170731091063340, 0.8880204242643787715, 0.8906252453521178447, 0.8932289408714879642, 0.8958333390004131758, 0.8984377420724726226, 0.9010414346201626179, 0.9036462588658594752, 0.9062496097237539017, 0.9088545132223035949, 0.9114579790861923048, 0.9140626342608790811, 0.9166666803663815477, 0.9192707220210388774, 0.9218753818226663732, 0.9244788459960084914, 0.9270837509176034219, 0.9296871028724987829, 0.9322919246527909820, 0.9348956210794385768, 0.9375000198362011261, 0.9401044239011964176, 0.9427081171475072408, 0.9453129423329229564, 0.9479162939871883520, 0.9505211982878988275, 0.9531246650646376661, 0.9557293209618126228, 0.9583333680330715643, 0.9609374102905526849, 0.9635420713365114853, 0.9661455366701111602, 0.9687504417289087844, 0.9713537931426093897, 0.9739586182492501187, 0.9765623229037746489, 0.9791667147516245340, 0.9817710778420317697, 0.9843748014325267581, 0.9869798465897002826, 0.9895830499482988207, 0.9921869381715581193, 0.9947912477285243416, 0.9974001254724073062, 1.000000000000000000 ),
 .UNSPECIFIED. ) ;
#179274 = CARTESIAN_POINT ( 'NONE',  ( 2.226796682701466246, -0.001291377463900899485, 1.725068445404242201 ) ) ;
#179275 = CARTESIAN_POINT ( 'NONE',  ( 4.411198876399872404, 6.239761003923544713, -1.599625672291273171 ) ) ;
#179277 = CARTESIAN_POINT ( 'NONE',  ( 5.182959862174088883, 9.268813282503625572, 0.7998128361456331437 ) ) ;
#179276 = CARTESIAN_POINT ( 'NONE',  ( 5.666945020832160118, 9.555260257705446847, 0.7216878364870438212 ) ) ;
#179278 = CARTESIAN_POINT ( 'NONE',  ( -11.52521982855896354, 8.148448055807163470, -3.186923921493055811 ) ) ;
#179279 = CARTESIAN_POINT ( 'NONE',  ( 0.3152201331171593512, -1.737291786998166332, 0.3363950369540784080 ) ) ;
#179280 = CARTESIAN_POINT ( 'NONE',  ( 0.3463400477153228407, 1.033117966650568986, -1.727632672016335080 ) ) ;
#179281 = LINE ( 'NONE', #211749, #67884 ) ;
#179282 = CARTESIAN_POINT ( 'NONE',  ( 2.819571115601596123, -0.2173934082839618642, 2.196046946737562511 ) ) ;
#179283 = AXIS2_PLACEMENT_3D ( 'NONE', #158049, #73573, #8569 ) ;
#179284 = CARTESIAN_POINT ( 'NONE',  ( 5.032167298026094748, 1.244454833084396306, 1.778855100471810280 ) ) ;
#179285 = VERTEX_POINT ( 'NONE', #172511 ) ;
#179286 = CARTESIAN_POINT ( 'NONE',  ( 3.088225128862704949, 6.824956093640315302, 0.7998128361456281477 ) ) ;
#179287 = CARTESIAN_POINT ( 'NONE',  ( 9.747949258101261449, 11.43532422494874368, -1.082531754730537088 ) ) ;
#179289 = CARTESIAN_POINT ( 'NONE',  ( 1.651970485933237143, 1.039013645561959853, 1.727991324714774013 ) ) ;
#179288 = CARTESIAN_POINT ( 'NONE',  ( 3.334745777049468618, 1.343786929377327466, -1.640352557257473309 ) ) ;
#179291 = VERTEX_POINT ( 'NONE', #186604 ) ;
#179290 = CARTESIAN_POINT ( 'NONE',  ( 2.566445574732978407, 0.6140501124722294035, 1.704450811836472734 ) ) ;
#179292 = CARTESIAN_POINT ( 'NONE',  ( 6.875920180786008196, 8.050936961452347163, -1.199719254218452047 ) ) ;
#179293 = CARTESIAN_POINT ( 'NONE',  ( 6.582647274634798151, 7.638508894284114170, 1.199719254218462483 ) ) ;
#179294 = B_SPLINE_CURVE_WITH_KNOTS ( 'NONE', 3,
 ( #212435, #98712, #14225, #96, #164771, #130220 ),
 .UNSPECIFIED., .F., .F.,
 ( 4, 2, 4 ),
 ( 0.000000000000000000, 0.0003157158648874033901, 0.0006314317297748067801 ),
 .UNSPECIFIED. ) ;
#179296 = CARTESIAN_POINT ( 'NONE',  ( 0.8838324889288513564, -1.915903395820263366, 0.003361870754229472590 ) ) ;
#179295 = CARTESIAN_POINT ( 'NONE',  ( -5.091250377131585125, 5.898545847196970726, 1.199719254218450271 ) ) ;
#179298 = VECTOR ( 'NONE', #122043, 1000.000000000000000 ) ;
#179297 = AXIS2_PLACEMENT_3D ( 'NONE', #106152, #200376, #37901 ) ;
#179299 = CARTESIAN_POINT ( 'NONE',  ( -2.680963302752292332, 0.4787599428022954462, -0.1016242801182818956 ) ) ;
#179300 = CARTESIAN_POINT ( 'NONE',  ( 9.586610838029415049, -7.161464053357574855, -0.003376046620562692113 ) ) ;
#179301 = CARTESIAN_POINT ( 'NONE',  ( 4.650083499362864359, 7.408552601689905259, 1.082531754730558626 ) ) ;
#179302 = CARTESIAN_POINT ( 'NONE',  ( 1.364683531249986537, -0.03229166632525094088, -0.7879004041258309554 ) ) ;
#179303 = CARTESIAN_POINT ( 'NONE',  ( -4.218316008240990271E-13, -9.350066838357692589, -9.500000000000001776 ) ) ;
#179304 = CARTESIAN_POINT ( 'NONE',  ( -10.15913717534155047, 10.74674821418697057, 0.7998128361456462443 ) ) ;
#179305 = CARTESIAN_POINT ( 'NONE',  ( 5.418883921851007202, 1.995750516393671514, 0.8311057252617033431 ) ) ;
#179306 = CARTESIAN_POINT ( 'NONE',  ( -4.611181642423629157, 7.433443445252599702, 1.082531754730549967 ) ) ;
#179307 = CARTESIAN_POINT ( 'NONE',  ( 5.885648082108200896, 6.039213315313952002, 0.7216878364870328300 ) ) ;
#179308 = CARTESIAN_POINT ( 'NONE',  ( 2.443736651115399283, -1.977012053918187906, 0.7674769708189137507 ) ) ;
#179310 = CARTESIAN_POINT ( 'NONE',  ( -11.80098439192703097, 4.809115636342174760, 4.927210371565812430 ) ) ;
#179309 = CARTESIAN_POINT ( 'NONE',  ( -4.902494178016985060, 4.880919686651536082, 0.5424932267784847717 ) ) ;
#179311 = CARTESIAN_POINT ( 'NONE',  ( 3.813711686511447763, -1.942732367404787830, 0.3338136033803756342 ) ) ;
#179312 = CARTESIAN_POINT ( 'NONE',  ( 5.291234991620994421, -0.05314252713351996088, -1.911838368980276925 ) ) ;
#179313 = ORIENTED_EDGE ( 'NONE', *, *, #185632, .F. ) ;
#179314 = CARTESIAN_POINT ( 'NONE',  ( -1.499999999999990896, 4.629166666666689522, -0.8660254037844429265 ) ) ;
#179315 = CARTESIAN_POINT ( 'NONE',  ( 6.848121164528643945, -0.8440317545377834518, 1.778091661420333702 ) ) ;
#179316 = CARTESIAN_POINT ( 'NONE',  ( 1.499837725185527049, -0.6986378101729547874, -1.812093905146118233 ) ) ;
#179317 = ORIENTED_EDGE ( 'NONE', *, *, #54983, .F. ) ;
#179318 = CARTESIAN_POINT ( 'NONE',  ( -5.000000000000000888, 3.300000000000025135, -0.7749999999999935829 ) ) ;
#179320 = CARTESIAN_POINT ( 'NONE',  ( 7.849244587668864348, 8.122149871893999062, 0.7998128361456291469 ) ) ;
#179319 = CARTESIAN_POINT ( 'NONE',  ( -7.268579750702160780, 8.613002809641560731, -1.082531754730549967 ) ) ;
#179322 = CARTESIAN_POINT ( 'NONE',  ( 6.830610463186557624, 6.863467050006115677, 1.040834085586084257E-14 ) ) ;
#179321 = CARTESIAN_POINT ( 'NONE',  ( 2.888710413438722924, 1.792813287458893790, -1.075199139784080771 ) ) ;
#179324 = ADVANCED_FACE ( 'NONE', ( #38231 ), #107564, .T. ) ;
#179323 = CARTESIAN_POINT ( 'NONE',  ( 6.021229617800532452, 6.197391773621639288, 0.000000000000000000 ) ) ;
#179326 = ORIENTED_EDGE ( 'NONE', *, *, #103372, .F. ) ;
#179325 = CARTESIAN_POINT ( 'NONE',  ( 5.654919265238161685, 0.3773621422162172223, 1.874504418562010999 ) ) ;
#179327 = CARTESIAN_POINT ( 'NONE',  ( 4.582781371344160526, -2.140174514510746029, -0.5380331057033281850 ) ) ;
#179328 = CARTESIAN_POINT ( 'NONE',  ( 3.592985822966657583, -0.4282699184722462693, -2.164648485658649868 ) ) ;
#179329 = CARTESIAN_POINT ( 'NONE',  ( 7.690499447449630210, 9.995335326823163058, 1.599625672291281386 ) ) ;
#179330 = CARTESIAN_POINT ( 'NONE',  ( -11.84668730067608600, 12.69999999999998153, 1.399999999999998357 ) ) ;
#179331 = CARTESIAN_POINT ( 'NONE',  ( 1.928230879603441750, -0.9027140558476205445, -1.685813393195116694 ) ) ;
#179332 = CARTESIAN_POINT ( 'NONE',  ( 0.000000000000000000, 5.999999999999998224, 0.000000000000000000 ) ) ;
#179333 = CARTESIAN_POINT ( 'NONE',  ( 9.103410076571945453, 12.70806329172093818, 1.199719254218450271 ) ) ;
#179334 = CARTESIAN_POINT ( 'NONE',  ( 4.404779037558821386, 0.5491149005726041477, 1.996164414091922135 ) ) ;
#179336 = CARTESIAN_POINT ( 'NONE',  ( 1.745224485312408813, -1.826185749030174499, 1.156423465944363294 ) ) ;
#179335 = CARTESIAN_POINT ( 'NONE',  ( -2.252626078164912560, 5.779814191167667481, 0.7998128361456341429 ) ) ;
#179337 = CARTESIAN_POINT ( 'NONE',  ( 3.316156725143477146, 1.388770557483296697, -1.695381604771596606 ) ) ;
#179338 = CARTESIAN_POINT ( 'NONE',  ( 8.387690588348714726, 12.93738945304888333, 1.040834085586084257E-14 ) ) ;
#179339 = PRESENTATION_STYLE_ASSIGNMENT (( #180389 ) ) ;
#179340 = CARTESIAN_POINT ( 'NONE',  ( -0.4599077567408665357, 8.047644787141420508, 1.947158400785508947 ) ) ;
#179341 = CARTESIAN_POINT ( 'NONE',  ( 5.143339171537801846, 7.093924681584509173, 1.599625672291269396 ) ) ;
#179342 = CARTESIAN_POINT ( 'NONE',  ( 1.364683531249997417, 14.79687500034139447, 2.602085213965210642E-15 ) ) ;
#179343 = CARTESIAN_POINT ( 'NONE',  ( -3.481411583659053566, 7.283673624236017830, 0.000000000000000000 ) ) ;
#179344 = CARTESIAN_POINT ( 'NONE',  ( 0.0006249722829775038483, -1.976948959267275541, 0.3961041280396286890 ) ) ;
#179345 = CARTESIAN_POINT ( 'NONE',  ( -10.30383355670593737, 11.12348669235284504, -0.7216878364870267237 ) ) ;
#179346 = CARTESIAN_POINT ( 'NONE',  ( 5.137584473783054051, 1.933663220787355419, -0.7400441640052906056 ) ) ;
#179347 = CARTESIAN_POINT ( 'NONE',  ( 2.895051130818243834, 1.652057846050537515, -0.9908002393040680200 ) ) ;
#179348 = CARTESIAN_POINT ( 'NONE',  ( 6.257425474675967436, 2.026018168931587482, -0.6146651352928398371 ) ) ;
#179349 = CARTESIAN_POINT ( 'NONE',  ( 4.852928918687680948, 7.749168607522574526, 1.199719254218462483 ) ) ;
#179350 = CARTESIAN_POINT ( 'NONE',  ( -1.201851678989727383E-14, 5.696875000341416140, -1.575800808251660134 ) ) ;
#179351 = CARTESIAN_POINT ( 'NONE',  ( 4.100420354389649802, 1.959567862165834562, 0.1972540966053982214 ) ) ;
#179352 = CARTESIAN_POINT ( 'NONE',  ( 6.333931935734662844, 2.266371222927834772, 0.3428166536569366984 ) ) ;
#179353 = CARTESIAN_POINT ( 'NONE',  ( 4.125493313500066428, -1.746467973620144720, 0.5319596651164605339 ) ) ;
#179354 = CARTESIAN_POINT ( 'NONE',  ( 7.078765600110826561, 8.391552967285011988, -1.082531754730548412 ) ) ;
#179355 = CARTESIAN_POINT ( 'NONE',  ( 4.812781342726866640, 5.677628323678546529, 1.082531754730560403 ) ) ;
#179356 = CARTESIAN_POINT ( 'NONE',  ( -4.945692173934974178, 8.992000979557944973, 0.000000000000000000 ) ) ;
#179357 = CARTESIAN_POINT ( 'NONE',  ( 5.180097208873055692, 8.201141289397330780, -1.199719254218450271 ) ) ;
#179358 = ORIENTED_EDGE ( 'NONE', *, *, #72583, .F. ) ;
#179360 = CARTESIAN_POINT ( 'NONE',  ( 5.537363252524067470, -0.04518311473342268708, 2.012845415592057208 ) ) ;
#179359 = CARTESIAN_POINT ( 'NONE',  ( 1.083273795380396143, -0.8277460070302902206, 1.644747122058511035 ) ) ;
#179361 = CARTESIAN_POINT ( 'NONE',  ( 6.363951117287210302, -0.1083456013219602776, -2.296273276487709847 ) ) ;
#179362 = CARTESIAN_POINT ( 'NONE',  ( 5.963715375765575644, -0.4800653121489819042, 1.901962685674676301 ) ) ;
#179363 = CARTESIAN_POINT ( 'NONE',  ( -5.533699252672048985, 9.607732894759390518, -0.7998128361456231517 ) ) ;
#179364 = CARTESIAN_POINT ( 'NONE',  ( -4.249591082879585535, 7.045274465746411252, 1.199719254218464037 ) ) ;
#179365 = DIRECTION ( 'NONE',  ( 0.000000000000000000, -1.000000000000000000, 0.000000000000000000 ) ) ;
#179366 = CARTESIAN_POINT ( 'NONE',  ( -5.098748287191073203, 8.106234214101666780, 1.199719254218452935 ) ) ;
#179368 = CARTESIAN_POINT ( 'NONE',  ( 0.2154177506630133854, -1.835460468737951878, 0.3602540799089171131 ) ) ;
#179367 = CARTESIAN_POINT ( 'NONE',  ( 1.312182373965790072, 1.401635355298202379, -1.551525349546636123 ) ) ;
#179369 = CARTESIAN_POINT ( 'NONE',  ( 0.000000000000000000, 12.22000000000000064, 0.000000000000000000 ) ) ;
#179370 = CARTESIAN_POINT ( 'NONE',  ( 5.578056150152780113, -1.895089194937165100, -0.4233685073328739557 ) ) ;
#179371 = CARTESIAN_POINT ( 'NONE',  ( -0.2102771530458225069, 7.629137130509110243, -2.803678522703976661 ) ) ;
#179372 = CARTESIAN_POINT ( 'NONE',  ( 0.7139227764019463462, 1.607345104371117772, 0.6680024673673248259 ) ) ;
#179373 = AXIS2_PLACEMENT_3D ( 'NONE', #33234, #131850, #67830 ) ;
#179374 = CARTESIAN_POINT ( 'NONE',  ( 5.126954644262057492, 9.133197518281081173, 0.7998128361456462443 ) ) ;
#179375 = CARTESIAN_POINT ( 'NONE',  ( 0.000000000000000000, 13.49999999999999822, 0.000000000000000000 ) ) ;
#179376 = CARTESIAN_POINT ( 'NONE',  ( 1.875234852168044641, 1.651158054356154148, -0.4988350824523117844 ) ) ;
#179377 = CARTESIAN_POINT ( 'NONE',  ( 1.909981697816802049, -1.036543071415759298, -1.930953618257096993 ) ) ;
#179378 = CARTESIAN_POINT ( 'NONE',  ( 6.884150274805287850, -0.1404709382532287054, 1.702994612897957394 ) ) ;
#179379 = CARTESIAN_POINT ( 'NONE',  ( 3.844505992619148937, 2.196175933995975438, 0.2170506636963928093 ) ) ;
#179380 = CARTESIAN_POINT ( 'NONE',  ( -10.32224513571693869, 3.007486591634276341, -7.366906358548013678 ) ) ;
#179381 = CARTESIAN_POINT ( 'NONE',  ( 1.235490768065301337, -0.05108008202716606688, -2.170608684345101125 ) ) ;
#179382 = CARTESIAN_POINT ( 'NONE',  ( 0.09986456629675066754, -1.825204794925545881, -0.04862044751281074939 ) ) ;
#179383 = CARTESIAN_POINT ( 'NONE',  ( 2.026704517097451586, 0.4691240347775883501, 2.064561701657470660 ) ) ;
#179384 = CARTESIAN_POINT ( 'NONE',  ( 6.539320575229250032, 4.701774335136183147, 2.359470009949143243 ) ) ;
#179385 = VERTEX_POINT ( 'NONE', #173599 ) ;
#179386 = AXIS2_PLACEMENT_3D ( 'NONE', #183757, #49497, #16968 ) ;
#179388 = CARTESIAN_POINT ( 'NONE',  ( -1.364683531250014514, 0.5510416670080878765, -0.7879004041258289570 ) ) ;
#179387 = CARTESIAN_POINT ( 'NONE',  ( 2.613130667218881431, -0.2215951064345271782, 2.281621536969838271 ) ) ;
#179389 = CARTESIAN_POINT ( 'NONE',  ( 1.124100812432970948E-16, 3.400000000000000355, -2.025000000000006573 ) ) ;
#179390 = CARTESIAN_POINT ( 'NONE',  ( 3.818592820543298405, 7.606775390609172405, -0.7998128361456221525 ) ) ;
#179391 = CARTESIAN_POINT ( 'NONE',  ( 4.670683837814712192, 0.8496151569591952057, 2.052583376702998397 ) ) ;
#179392 = CARTESIAN_POINT ( 'NONE',  ( -5.233084105194862445, 9.049089189461916760, 0.7216878364870458196 ) ) ;
#179393 = EDGE_CURVE ( 'NONE', #162523, #174147, #25171, .T. ) ;
#179394 = CARTESIAN_POINT ( 'NONE',  ( 5.097502569058200983, 6.970172302033127210, -1.443375672974051449 ) ) ;
#179395 = CARTESIAN_POINT ( 'NONE',  ( -8.487040972030346353, 9.003895343564625620, 1.040834085586084257E-14 ) ) ;
#179396 = CARTESIAN_POINT ( 'NONE',  ( 4.367134877377630175, 7.148722219365612141, -1.082531754730548412 ) ) ;
#179397 = ORIENTED_EDGE ( 'NONE', *, *, #132097, .T. ) ;
#179398 = CARTESIAN_POINT ( 'NONE',  ( 2.479138880926802901, -2.011204309026824344, -0.1455328587063598189 ) ) ;
#179400 = CARTESIAN_POINT ( 'NONE',  ( 2.377848133335142222, -2.001750602163259174, 0.4968105773679451498 ) ) ;
#179399 = CARTESIAN_POINT ( 'NONE',  ( 8.098297826064319693, 8.342435640030188893, 0.7998128361456481317 ) ) ;
#179401 = DIRECTION ( 'NONE',  ( 0.000000000000000000, -0.08676576675288254215, 0.9962287396576070542 ) ) ;
#179402 = CARTESIAN_POINT ( 'NONE',  ( 5.275531169048895741, 7.248148678680751189, -1.443375672974078761 ) ) ;
#179403 = CARTESIAN_POINT ( 'NONE',  ( 1.499999999999996891, 8.677083334016133520, -0.8660254037844378194 ) ) ;
#179404 = CARTESIAN_POINT ( 'NONE',  ( 0.6823417656249899377, 5.176041667008086655, -1.181850606188754593 ) ) ;
#179405 = CARTESIAN_POINT ( 'NONE',  ( 4.628971764384363752, -2.004251508290517680, 0.8866568735110615940 ) ) ;
#179406 = CARTESIAN_POINT ( 'NONE',  ( 2.461564753630896440, -1.930417925741171103, -0.5826551686555282439 ) ) ;
#179407 = CARTESIAN_POINT ( 'NONE',  ( 2.313779677144182312, 1.201330555204615180, -1.395457044143719072 ) ) ;
#179408 = CARTESIAN_POINT ( 'NONE',  ( 7.633404179693907388, 8.864391950186421454, -1.199719254218441611 ) ) ;
#179409 = SURFACE_SIDE_STYLE ('',( #159950 ) ) ;
#179410 = CARTESIAN_POINT ( 'NONE',  ( 5.104447739783800841, -0.6163660037172628003, -1.718524672285254740 ) ) ;
#179411 = CARTESIAN_POINT ( 'NONE',  ( 5.537732479266092689, -1.587839044716709669, 1.242724925242834066 ) ) ;
#179412 = CARTESIAN_POINT ( 'NONE',  ( -8.311311860377216476, 9.655284244316948872, -1.199719254218446718 ) ) ;
#179414 = CARTESIAN_POINT ( 'NONE',  ( -6.805266759416629618, 6.904175738932996964, 0.000000000000000000 ) ) ;
#179413 = CARTESIAN_POINT ( 'NONE',  ( 6.174757231500850096, -2.146110616029934803, -0.7165941539545512828 ) ) ;
#179415 = CARTESIAN_POINT ( 'NONE',  ( 1.067171494879548987, -1.904794536548588546, -0.8987870243707897222 ) ) ;
#179416 = CARTESIAN_POINT ( 'NONE',  ( -5.752402313948099533, 9.933162809573264695, -0.7998128361456362523 ) ) ;
#179417 = CARTESIAN_POINT ( 'NONE',  ( 8.055515824813896941, 12.54985222892493368, 0.7998128361456462443 ) ) ;
#179418 = SURFACE_SIDE_STYLE ('',( #163166 ) ) ;
#179419 = DIRECTION ( 'NONE',  ( 0.7205630238414714173, 0.000000000000000000, 0.6933894494960498589 ) ) ;
#179420 = CARTESIAN_POINT ( 'NONE',  ( -8.850775351622791831, 9.220326086515070685, -0.7998128361456291469 ) ) ;
#179421 = UNCERTAINTY_MEASURE_WITH_UNIT (LENGTH_MEASURE( 1.000000000000000082E-05 ), #83581, 'distance_accuracy_value', 'NONE');
#179422 = CARTESIAN_POINT ( 'NONE',  ( 1.686272053095002589E-16, -4.517653975874099892, 1.376945625684933061 ) ) ;
#179423 = CARTESIAN_POINT ( 'NONE',  ( 6.003228155800906407, 10.22579295840155744, 0.000000000000000000 ) ) ;
#179424 = CARTESIAN_POINT ( 'NONE',  ( 5.622931663646434153, 6.144404617744410046, -0.8283694935172694063 ) ) ;
#179425 = CARTESIAN_POINT ( 'NONE',  ( -9.246297574839990929, 11.81043314211192019, 1.443375672974076540 ) ) ;
#179426 = CARTESIAN_POINT ( 'NONE',  ( 3.287547529179511319, 0.05108950329585186523, -2.220969887641692342 ) ) ;
#179427 = DIRECTION ( 'NONE',  ( 0.000000000000000000, 0.000000000000000000, 1.000000000000000000 ) ) ;
#179428 = CARTESIAN_POINT ( 'NONE',  ( -4.762657100150483380, 8.778460060142702304, 0.000000000000000000 ) ) ;
#179429 = CARTESIAN_POINT ( 'NONE',  ( 6.419949431270806528, 7.448694743692793274, 1.199719254218462483 ) ) ;
#179430 = CARTESIAN_POINT ( 'NONE',  ( 2.787496613063783713, -1.831585881375777713, 0.7034878451678548972 ) ) ;
#179431 = CARTESIAN_POINT ( 'NONE',  ( 4.690231075323689325, 7.559354456931247412, 1.199719254218462483 ) ) ;
#179432 = CARTESIAN_POINT ( 'NONE',  ( -4.217650912117239415, 7.357101779856191293, 0.8466403022913439047 ) ) ;
#179433 = CARTESIAN_POINT ( 'NONE',  ( 5.007038802148489509, 4.735966778795008381, 0.7998128361456341429 ) ) ;
#179434 = CARTESIAN_POINT ( 'NONE',  ( -5.994113311017573054, 6.165756082374834079, 0.7216878364870257245 ) ) ;
#179435 = CARTESIAN_POINT ( 'NONE',  ( -6.887178846062123938, 8.097758744236356776, -1.082531754730544860 ) ) ;
#179437 = CARTESIAN_POINT ( 'NONE',  ( 1.898838059644195386, -2.080654286433290867, -0.4088066060855889972 ) ) ;
#179436 = COLOUR_RGB ( '', 0.31764706, 0.68627451, 0.89019608) ;
#179438 = CARTESIAN_POINT ( 'NONE',  ( -5.285699784481336927, 7.260012063351913625, 1.599625672291263179 ) ) ;
#179439 = CARTESIAN_POINT ( 'NONE',  ( 3.889662759143839299, 1.564074849111227516, 1.492423382767386730 ) ) ;
#179440 = CARTESIAN_POINT ( 'NONE',  ( 2.559893532628489954, -1.268187297466142338, 1.335118840784771166 ) ) ;
#179441 = CARTESIAN_POINT ( 'NONE',  ( -5.386593377506219582, 6.333579893170925068, 1.078181536478119762 ) ) ;
#179442 = CARTESIAN_POINT ( 'NONE',  ( -1.402160292154681736E-14, -0.1156249996585793222, 1.575800808251672791 ) ) ;
#179443 = CARTESIAN_POINT ( 'NONE',  ( 5.349435159262297290, 1.738085940734758639, -0.09086515553361101949 ) ) ;
#179444 = CARTESIAN_POINT ( 'NONE',  ( -5.790741006368233634, 5.928488393617254992, 0.7216878364870203955 ) ) ;
#179445 = CARTESIAN_POINT ( 'NONE',  ( 4.148431816101584957, 6.823292304551739740, -1.082531754730548412 ) ) ;
#179446 = CARTESIAN_POINT ( 'NONE',  ( 3.133815226704575796, -1.450665623810345473, -1.602838778681405785 ) ) ;
#179447 = CARTESIAN_POINT ( 'NONE',  ( 4.358749857130030492, -0.7741967591250037417, 1.861731939633674893 ) ) ;
#179448 = CARTESIAN_POINT ( 'NONE',  ( -8.297226821439000588, 12.62392235841345389, 1.040834085586084257E-14 ) ) ;
#179449 = AXIS2_PLACEMENT_3D ( 'NONE', #52693, #135037, #136093 ) ;
#179450 = CARTESIAN_POINT ( 'NONE',  ( 2.254944280175336324, -1.671361177491991201, 1.370965666894090385 ) ) ;
#179451 = CARTESIAN_POINT ( 'NONE',  ( 2.987526725409937800, 1.391544230491305933, 1.396620715705886084 ) ) ;
#179452 = CARTESIAN_POINT ( 'NONE',  ( 6.509000000000012776, 0.5843741663743782233, 2.053293374786519188 ) ) ;
#179453 = CARTESIAN_POINT ( 'NONE',  ( 4.528815305949091652, -1.774144813887452266, 0.7903587577767021699 ) ) ;
#179455 = ORIENTED_EDGE ( 'NONE', *, *, #134540, .T. ) ;
#179454 = CARTESIAN_POINT ( 'NONE',  ( -9.775065565328612038, 10.50659070241261794, -0.7216878364870267237 ) ) ;
#179456 = CARTESIAN_POINT ( 'NONE',  ( -6.149505192250180663, 9.332117270003974951, -1.199719254218452047 ) ) ;
#179457 = DIRECTION ( 'NONE',  ( -1.000000000000000000, 0.000000000000000000, 0.000000000000000000 ) ) ;
#179458 = EDGE_CURVE ( 'NONE', #201902, #188755, #157329, .T. ) ;
#179460 = VERTEX_POINT ( 'NONE', #28378 ) ;
#179459 = CARTESIAN_POINT ( 'NONE',  ( -7.130662446144611977, 7.283804040115648526, 0.000000000000000000 ) ) ;
#179461 = CARTESIAN_POINT ( 'NONE',  ( -7.904040366642703930, 10.24446639921506552, 1.443375672974090751 ) ) ;
#179462 = CARTESIAN_POINT ( 'NONE',  ( 1.202499378025536636, -2.206952907257493823, 0.001246274542086866404 ) ) ;
#179463 = CARTESIAN_POINT ( 'NONE',  ( -3.285556943750000070, -2.209374999522041527, 0.000000000000000000 ) ) ;
#179464 = CARTESIAN_POINT ( 'NONE',  ( 4.698074428120575519, 0.8425069249109422564, -1.771795133841248981 ) ) ;
#179465 = CARTESIAN_POINT ( 'NONE',  ( 0.6823417656249899377, 5.738541667008087543, -1.181850606188754593 ) ) ;
#179466 = CARTESIAN_POINT ( 'NONE',  ( -0.7499999999999972244, 3.389583334016149863, -1.299038105676652011 ) ) ;
#179467 = CARTESIAN_POINT ( 'NONE',  ( 5.854153468347242040, 6.181931306435468620, -0.8879621099797951889 ) ) ;
#179469 = CARTESIAN_POINT ( 'NONE',  ( -5.229694566569281555, 7.124396299129368337, 1.599625672291267398 ) ) ;
#179468 = CARTESIAN_POINT ( 'NONE',  ( 0.07479286986305545837, 0.7422478802248284602, -1.939684878352589070 ) ) ;
#179470 = CARTESIAN_POINT ( 'NONE',  ( 3.732213890823964597, 0.2717154217161937280, 1.820854149191558635 ) ) ;
#179471 = VERTEX_POINT ( 'NONE', #127036 ) ;
#179472 = CARTESIAN_POINT ( 'NONE',  ( -1.360316468750024876, -0.5885416663252728275, 0.7853790794158701516 ) ) ;
#179473 = CARTESIAN_POINT ( 'NONE',  ( -8.290974629956718189, 9.631557475493025322, -1.199719254218446718 ) ) ;
#179474 = CARTESIAN_POINT ( 'NONE',  ( -0.3221776901982874031, -8.373013763170321601E-15, 1.292830470765887307 ) ) ;
#179475 = CARTESIAN_POINT ( 'NONE',  ( 5.396778611113259849, -2.069399493756381769, -0.4625044129713885011 ) ) ;
#179476 = CARTESIAN_POINT ( 'NONE',  ( 10.88587197153689701, 8.292399138164135763, 4.942068264615757656 ) ) ;
#179477 = CARTESIAN_POINT ( 'NONE',  ( 4.462605117192430804, 8.358123070033169455, 1.040834085586084257E-14 ) ) ;
#179478 = ORIENTED_EDGE ( 'NONE', *, *, #25456, .F. ) ;
#179479 = CARTESIAN_POINT ( 'NONE',  ( 6.397740692956204178, -0.6987371234766488470, 1.938827229339795455 ) ) ;
#179480 = TOROIDAL_SURFACE ( 'NONE', #41101, 10.92000000000000171, 0.08000000000000000167 ) ;
#179483 = CARTESIAN_POINT ( 'NONE',  ( 3.280630368989821743, 1.663260157205956880, -0.7901080472864712156 ) ) ;
#179482 = CARTESIAN_POINT ( 'NONE',  ( 1.504125588540955683, 1.858726126767410669, 0.09586466133617438379 ) ) ;
#179481 = DIRECTION ( 'NONE',  ( -0.8271092603138155974, 0.5620411653100980676, 1.333541550007727027E-12 ) ) ;
#179484 = CARTESIAN_POINT ( 'NONE',  ( 7.609150525767641504, 9.900428251527500834, -1.599625672291262513 ) ) ;
#179485 = FILL_AREA_STYLE ('',( #112408 ) ) ;
#179486 = CARTESIAN_POINT ( 'NONE',  ( -7.795011973214244883, 8.058878488363559356, 0.7998128361456341429 ) ) ;
#179487 = CYLINDRICAL_SURFACE ( 'NONE', #14784, 0.08000000000000041800 ) ;
#179488 = CARTESIAN_POINT ( 'NONE',  ( 2.860232119962682784, 2.196193069775736362, -0.2169517147150926140 ) ) ;
#179489 = CARTESIAN_POINT ( 'NONE',  ( 6.204402397823557180, -0.8056473179405240215, -2.114295379420629839 ) ) ;
#179490 = CARTESIAN_POINT ( 'NONE',  ( -6.399085315970142851, 8.488685506763726352, -1.443375672974059665 ) ) ;
#179491 = CARTESIAN_POINT ( 'NONE',  ( 6.381129877538572970, -1.660329982341423705, -0.7251259014357125388 ) ) ;
#179492 = CARTESIAN_POINT ( 'NONE',  ( 5.137857799264941683, 1.913235287650059790, -0.1005462703686579862 ) ) ;
#179493 = CARTESIAN_POINT ( 'NONE',  ( 1.364683531249988535, 5.217708333674750065, -0.7879004041258300672 ) ) ;
#179494 = CARTESIAN_POINT ( 'NONE',  ( 6.420764531294745225, 1.746252128813120086, 0.6712297951826234899 ) ) ;
#179495 = CIRCLE ( 'NONE', #16950, 0.1000000000000000333 ) ;
#179496 = CARTESIAN_POINT ( 'NONE',  ( 5.723074792265875566, -1.682715607417185399, -0.7953119777529999990 ) ) ;
#179497 = FACE_OUTER_BOUND ( 'NONE', #4771, .T. ) ;
#179498 = CARTESIAN_POINT ( 'NONE',  ( 6.719637426148988624, -1.715392417075599196, 0.4352852820774539833 ) ) ;
#179499 = CARTESIAN_POINT ( 'NONE',  ( 1.411342602523330214, -1.897109289313268166, 0.6839406069230756779 ) ) ;
#179501 = CARTESIAN_POINT ( 'NONE',  ( 2.947987317136715468, 0.7576180897185936791, -1.965265766029665295 ) ) ;
#179500 = CARTESIAN_POINT ( 'NONE',  ( -9.775592450653132204, 11.36361159963886891, -1.199719254218441611 ) ) ;
#179502 = EDGE_CURVE ( 'NONE', #140029, #149611, #195153, .T. ) ;
#179503 = CARTESIAN_POINT ( 'NONE',  ( 7.910292558569346433, 11.31609285405122556, -1.199719254218446718 ) ) ;
#179505 = CARTESIAN_POINT ( 'NONE',  ( -7.479294296233107708, 11.87759377891399204, 0.7998128361456481317 ) ) ;
#179504 = CARTESIAN_POINT ( 'NONE',  ( 1.436715752608449748, 7.421775496532144523, -4.237684949271973700 ) ) ;
#179506 = DIRECTION ( 'NONE',  ( -1.000000000000000000, 7.771561172376097755E-16, 4.440892098500627148E-16 ) ) ;
#179507 = CARTESIAN_POINT ( 'NONE',  ( 2.883074275722704360, -1.867829236092366951, -0.7691044946091238899 ) ) ;
#179508 = CARTESIAN_POINT ( 'NONE',  ( -1.201851678989727383E-14, 4.071875000341425022, 1.575800808251672791 ) ) ;
#179509 = EDGE_CURVE ( 'NONE', #184190, #62256, #35685, .T. ) ;
#179510 = CARTESIAN_POINT ( 'NONE',  ( 4.532503425670185493, 4.182342172903648070, 1.214306433183764966E-14 ) ) ;
#179511 = CARTESIAN_POINT ( 'NONE',  ( 3.181113218772323226, -0.1555236193923059951, -2.156033859764289407 ) ) ;
#179512 = CARTESIAN_POINT ( 'NONE',  ( 8.188198428010544205, 8.517596018959260107, 0.000000000000000000 ) ) ;
#179514 = LINE ( 'NONE', #97209, #62263 ) ;
#179513 = CARTESIAN_POINT ( 'NONE',  ( 6.047819040147648373, 9.213483425884394507, 1.199719254218452047 ) ) ;
#179515 = CARTESIAN_POINT ( 'NONE',  ( 8.066738210006668908, 12.35501897840907581, 0.7216878364870438212 ) ) ;
#179517 = CARTESIAN_POINT ( 'NONE',  ( 8.952720908857106252, 14.54244786625251962, -7.923410800768315276 ) ) ;
#179516 = CARTESIAN_POINT ( 'NONE',  ( 0.6608746330511162670, -0.7316962540516893654, -2.044312434917434640 ) ) ;
#179518 =( BOUNDED_CURVE ( )  B_SPLINE_CURVE ( 2, ( #31109, #80910, #100348, #35335, #84097, #150184, #97181, #214057, #13758 ),
 .UNSPECIFIED., .F., .T. ) 
 B_SPLINE_CURVE_WITH_KNOTS ( ( 3, 2, 2, 2, 3 ),
 ( 0.1406250000000001943, 0.1458333333333333426, 0.1562500000000000000, 0.1666666666666666574, 0.1718749999999998335 ),
 .UNSPECIFIED. ) 
 CURVE ( )  GEOMETRIC_REPRESENTATION_ITEM ( )  RATIONAL_B_SPLINE_CURVE ( ( 0.9330127018922194093, 0.9330127018922218518, 1.000000000000000000, 0.8660254037844387076, 1.000000000000000000, 0.8660254037844387076, 1.000000000000000000, 0.9330127018922215187, 0.9330127018922194093 ) ) 
 REPRESENTATION_ITEM ( '' )  );
#179519 = CARTESIAN_POINT ( 'NONE',  ( -6.209271165378811297, 10.18797409300986878, 0.7216878364870458196 ) ) ;
#179520 = CARTESIAN_POINT ( 'NONE',  ( -1.364683531250014514, 1.238541667008091096, -0.7879004041258289570 ) ) ;
#179521 = CARTESIAN_POINT ( 'NONE',  ( 1.769323484426460480, 2.095969018468134770, -0.6401429536977767398 ) ) ;
#179522 = CARTESIAN_POINT ( 'NONE',  ( 2.395744609331447172, 1.748901261223069437, 1.435362524944477025 ) ) ;
#179523 = CARTESIAN_POINT ( 'NONE',  ( -7.426115451983156923, 9.686887332112256388, -1.599625672291263179 ) ) ;
#179524 = CARTESIAN_POINT ( 'NONE',  ( -3.090895833791289071, 6.549869539491048442, 1.040834085586084257E-14 ) ) ;
#179526 = AXIS2_PLACEMENT_3D ( 'NONE', #99005, #134722, #184490 ) ;
#179525 = CARTESIAN_POINT ( 'NONE',  ( -1.364683531249997417, 3.821875000341416584, 1.214306433183764966E-14 ) ) ;
#179527 = CARTESIAN_POINT ( 'NONE',  ( 6.198956711081595294, 6.941498593865138567, 0.8670033951987624610 ) ) ;
#179528 = CARTESIAN_POINT ( 'NONE',  ( -0.7500000000000006661, 11.45833333333333393, -1.299038105676657340 ) ) ;
#179529 = CARTESIAN_POINT ( 'NONE',  ( 4.146814880933355596, 5.931313009212638931, 1.599625672291261402 ) ) ;
#179530 =( BOUNDED_SURFACE ( )  B_SPLINE_SURFACE ( 3, 2, ( 
 ( #72714, #175575, #27166 ),
 ( #93271, #159304, #105248 ),
 ( #10902, #60733, #138810 ),
 ( #204829, #188604, #40236 ),
 ( #126897, #78053, #11979 ),
 ( #14093, #211237, #179829 ),
 ( #97527, #110630, #47715 ),
 ( #16221, #129029, #112760 ) ),
 .UNSPECIFIED., .F., .F., .F. ) 
 B_SPLINE_SURFACE_WITH_KNOTS ( ( 4, 2, 2, 4 ),
 ( 3, 3 ),
 ( 0.000000000000000000, 0.0002575597274893397974, 0.0005151194549786795949, 0.001030238909957359190 ),
 ( 0.000000000000000000, 1.000000000000000000 ),
 .UNSPECIFIED. ) 
 GEOMETRIC_REPRESENTATION_ITEM ( )  RATIONAL_B_SPLINE_SURFACE ( (
 ( 1.000000000000000000, 0.9238795325112797441, 1.000000000000000000),
 ( 1.000000000000000000, 0.9228594682462623044, 1.000000000000000000),
 ( 1.000000000000000000, 0.9150875845229113903, 1.000000000000000000),
 ( 1.000000000000000000, 0.8905471774190711898, 1.000000000000000000),
 ( 1.000000000000000000, 0.8740340839248519345, 1.000000000000000000),
 ( 1.000000000000000000, 0.8160099319846257915, 1.000000000000000000),
 ( 1.000000000000000000, 0.7673743911479106172, 1.000000000000000000),
 ( 1.000000000000000000, 0.7100530722070661493, 1.000000000000000000) ) ) 
 REPRESENTATION_ITEM ( '' )  SURFACE ( )  );
#179531 = CARTESIAN_POINT ( 'NONE',  ( 2.653260118625869080, 0.4764888685691510140, -1.704286641089979959 ) ) ;
#179532 = CARTESIAN_POINT ( 'NONE',  ( 6.598651186688741177, -0.5821561243712966016, -2.128545807824663960 ) ) ;
#179533 = CARTESIAN_POINT ( 'NONE',  ( -1.364683531250014514, 8.838541667008069425, -0.7879004041258335089 ) ) ;
#179534 = CARTESIAN_POINT ( 'NONE',  ( -4.773352600463090845, 7.726605912919016106, 1.199719254218452935 ) ) ;
#179535 = CARTESIAN_POINT ( 'NONE',  ( 4.692982559244565088, 1.755779632255444422, 0.9913831279167032440 ) ) ;
#179536 = ORIENTED_EDGE ( 'NONE', *, *, #23138, .F. ) ;
#179537 = CARTESIAN_POINT ( 'NONE',  ( 3.819104250046548632, -0.1383300533824398659, 1.865606469731183825 ) ) ;
#179538 = CARTESIAN_POINT ( 'NONE',  ( 3.748938768049938197, -0.3990674421511587466, -2.031259957477090428 ) ) ;
#179539 = CARTESIAN_POINT ( 'NONE',  ( -6.238160075619175515, 10.29195416494877513, 0.000000000000000000 ) ) ;
#179540 = CARTESIAN_POINT ( 'NONE',  ( -0.5723599497803579794, 3.454715670812215311, -0.3124809264750456061 ) ) ;
#179541 = CARTESIAN_POINT ( 'NONE',  ( -10.41986968326957808, 5.020773655391575829, -5.279272669861445166 ) ) ;
#179542 = CARTESIAN_POINT ( 'NONE',  ( -0.6823417656250212460, 4.613541667008086655, 1.181850606188767472 ) ) ;
#179543 = CARTESIAN_POINT ( 'NONE',  ( 1.195406425308798148, 1.765864799226088744, -0.7346160280939582066 ) ) ;
#179544 = CARTESIAN_POINT ( 'NONE',  ( 2.435929278166943490, 1.204617592564939166, 1.548422000036096202 ) ) ;
#179545 = CARTESIAN_POINT ( 'NONE',  ( 1.352888501574830205, -0.9090079681693465918, 1.799646022210943386 ) ) ;
#179546 = CARTESIAN_POINT ( 'NONE',  ( -5.632486471834530661, 5.535932070087196344, -0.7998128361456362523 ) ) ;
#179548 = CARTESIAN_POINT ( 'NONE',  ( -11.33772463945037146, 12.69999999999998153, 3.599999999999999201 ) ) ;
#179547 = CARTESIAN_POINT ( 'NONE',  ( 9.271078113646423091, 9.710679308875986848, 1.040834085586084257E-14 ) ) ;
#179549 = CARTESIAN_POINT ( 'NONE',  ( 6.362572844203587152, -1.395794784517788045, 1.392370165595870679 ) ) ;
#179550 = CARTESIAN_POINT ( 'NONE',  ( -1.364683531250012516, 2.488541667008088876, -0.7879004041258289570 ) ) ;
#179551 = CARTESIAN_POINT ( 'NONE',  ( 2.390887483786011014, -1.927808053674067823, -0.5802275739894193762 ) ) ;
#179553 = CARTESIAN_POINT ( 'NONE',  ( 2.372804174479496986, -0.3651721903723912921, -2.085361659519912259 ) ) ;
#179552 = CARTESIAN_POINT ( 'NONE',  ( -7.565086526745425033, 7.928281824065535055, 0.7216878364870317197 ) ) ;
#179554 = CARTESIAN_POINT ( 'NONE',  ( 1.499999999999823475, 7.361490936993391188, 4.203511340218978987 ) ) ;
#179555 = CARTESIAN_POINT ( 'NONE',  ( 3.420434311836465291, 0.9283866757503267397, 1.850595421526677775 ) ) ;
#179556 = CARTESIAN_POINT ( 'NONE',  ( 4.329849954717849947, 6.144853928627882489, 1.599625672291262513 ) ) ;
#179558 = CARTESIAN_POINT ( 'NONE',  ( 2.354312230267378236, 5.898448035287240820, -0.7998128361456281477 ) ) ;
#179557 = CARTESIAN_POINT ( 'NONE',  ( 6.228480176075449570, 0.2035102421588113053, 2.080708833908810451 ) ) ;
#179560 = EDGE_LOOP ( 'NONE', ( #182197, #192600, #195646, #198965 ) ) ;
#179559 = CARTESIAN_POINT ( 'NONE',  ( 4.014527796464135712, 1.291161025869846712, -1.290856679043244970 ) ) ;
#179561 = CARTESIAN_POINT ( 'NONE',  ( 8.055515824813896941, 12.54985222892493368, 0.7998128361456462443 ) ) ;
#179562 = SURFACE_SIDE_STYLE ('',( #114621 ) ) ;
#179563 = CARTESIAN_POINT ( 'NONE',  ( 11.59565239942670800, 8.772708109194649495, 2.738260425586001912 ) ) ;
#179564 = CARTESIAN_POINT ( 'NONE',  ( 6.211994372536747022, -2.190858219723303524, 0.2640275128017176565 ) ) ;
#179565 = CARTESIAN_POINT ( 'NONE',  ( -1.364683531250014514, 10.15104166700806587, -0.7879004041258335089 ) ) ;
#179566 = EDGE_LOOP ( 'NONE', ( #184978, #97254, #55259, #30581, #47171 ) ) ;
#179567 = CARTESIAN_POINT ( 'NONE',  ( 5.356085673312771966, 0.7711821229579116643, -1.750063228584404440 ) ) ;
#179568 = CARTESIAN_POINT ( 'NONE',  ( -10.15913717534155047, 10.74674821418697057, 0.7998128361456462443 ) ) ;
#179569 =( BOUNDED_CURVE ( )  B_SPLINE_CURVE ( 2, ( #141174, #22002, #186664, #203960, #170413, #71829, #56681, #42589, #121763 ),
 .UNSPECIFIED., .F., .T. ) 
 B_SPLINE_CURVE_WITH_KNOTS ( ( 3, 2, 2, 2, 3 ),
 ( 0.9732142857142856984, 0.9761904761904761640, 0.9821428571428570953, 0.9880952380952381375, 0.9910714285714286031 ),
 .UNSPECIFIED. ) 
 CURVE ( )  GEOMETRIC_REPRESENTATION_ITEM ( )  RATIONAL_B_SPLINE_CURVE ( ( 0.9330127018922194093, 0.9330127018922194093, 1.000000000000000000, 0.8660254037844387076, 1.000000000000000000, 0.8660254037844387076, 1.000000000000000000, 0.9330127018922194093, 0.9330127018922194093 ) ) 
 REPRESENTATION_ITEM ( '' )  );
#179570 = MECHANICAL_DESIGN_GEOMETRIC_PRESENTATION_REPRESENTATION (  '', ( #138146 ), #30853 ) ;
#179571 = CARTESIAN_POINT ( 'NONE',  ( 6.286176778230493589, 10.48562334124426698, 0.7998128361456462443 ) ) ;
#179572 = CARTESIAN_POINT ( 'NONE',  ( -1.360316468750036645, 2.151041667008108060, -0.7853790794159302147 ) ) ;
#179573 = CARTESIAN_POINT ( 'NONE',  ( 0.7500000000000006661, 9.916666666666671404, -1.299038105676657340 ) ) ;
#179574 = CARTESIAN_POINT ( 'NONE',  ( 8.140346590616603706, 14.24105188827307167, -8.817491472814088738 ) ) ;
#179575 = CARTESIAN_POINT ( 'NONE',  ( 0.9426144736941791669, -1.451487892885485742, -1.132780452900377099 ) ) ;
#179576 = ORIENTED_EDGE ( 'NONE', *, *, #157920, .T. ) ;
#179577 = CARTESIAN_POINT ( 'NONE',  ( 4.973830807571049561, 1.075732564348480746, 1.530087412091485799 ) ) ;
#179578 = CARTESIAN_POINT ( 'NONE',  ( -11.04984958223792368, 13.60917513768126597, 1.056557932048282078 ) ) ;
#179579 = CARTESIAN_POINT ( 'NONE',  ( 6.367489420273535039, 7.457767740854454708, -1.199719254218452047 ) ) ;
#179580 = CARTESIAN_POINT ( 'NONE',  ( -0.08058608058608471292, -5.770897281092843834, 10.99970480893081870 ) ) ;
#179581 = CARTESIAN_POINT ( 'NONE',  ( -5.130090819275266334, 7.806487709571898748, 1.156910012491520590 ) ) ;
#179582 = CARTESIAN_POINT ( 'NONE',  ( -5.585596099150191840, 7.539614753807099667, -1.443375672974052559 ) ) ;
#179583 = CARTESIAN_POINT ( 'NONE',  ( 5.606460214450851964, 6.499623990736163037, 1.199719254218462483 ) ) ;
#179584 = CARTESIAN_POINT ( 'NONE',  ( 1.375766793938013821, -1.922594530582939942, 0.4262983161763284623 ) ) ;
#179585 = CARTESIAN_POINT ( 'NONE',  ( 2.038685622454153190, -1.556895902704044765, 1.281378572682637218 ) ) ;
#179586 = CARTESIAN_POINT ( 'NONE',  ( -8.995998617867369873, 10.45408546138876993, 1.199719254218462483 ) ) ;
#179587 = CARTESIAN_POINT ( 'NONE',  ( 5.716698046817569434, 6.698511138489155137, -1.199719254218452047 ) ) ;
#179588 = FACE_OUTER_BOUND ( 'NONE', #141177, .T. ) ;
#179589 = CARTESIAN_POINT ( 'NONE',  ( 2.677880624963273171, -1.125664371729949265, 1.880105217535378959 ) ) ;
#179590 =( NAMED_UNIT ( * ) SI_UNIT ( $, .STERADIAN. ) SOLID_ANGLE_UNIT ( ) );
#179591 = CARTESIAN_POINT ( 'NONE',  ( -8.109748439268576803, 12.61312361245537517, 0.7998128361456481317 ) ) ;
#179592 = PLANE ( 'NONE',  #58774 ) ;
#179593 = CARTESIAN_POINT ( 'NONE',  ( 1.250000000000037526, 8.500000000000000000, 10.97907099895068583 ) ) ;
#179594 = CARTESIAN_POINT ( 'NONE',  ( 4.923019175537949543, 4.916146257648610352, 0.000000000000000000 ) ) ;
#179595 = CARTESIAN_POINT ( 'NONE',  ( 9.921869487102386032, 10.46993591124128997, 0.000000000000000000 ) ) ;
#179596 = CARTESIAN_POINT ( 'NONE',  ( -9.508841981786570585, 14.91423885135806415, 7.212865296072065391 ) ) ;
#179597 = CARTESIAN_POINT ( 'NONE',  ( 5.506019780925567986, 8.477421273504887722, -1.082531754730548412 ) ) ;
#179598 = ORIENTED_EDGE ( 'NONE', *, *, #188352, .T. ) ;
#179600 = CARTESIAN_POINT ( 'NONE',  ( 2.315091943819780340, 1.615584347832084600, -1.200805960377361981 ) ) ;
#179599 = CARTESIAN_POINT ( 'NONE',  ( 4.440845869443198701, -1.426288408191313639, -1.164454570719307469 ) ) ;
#179601 = CARTESIAN_POINT ( 'NONE',  ( 2.900137762625193183, 0.2794712830477152354, 2.281260185934708140 ) ) ;
#179603 = CARTESIAN_POINT ( 'NONE',  ( 1.815070623055618615, -1.592837743320011601, -0.9620759905232498799 ) ) ;
#179602 = CARTESIAN_POINT ( 'NONE',  ( 2.449293598294706414E-16, 9.999999999999998224, 2.000000000000000000 ) ) ;
#179604 = CARTESIAN_POINT ( 'NONE',  ( 1.642778471875001811, -1.742708332855374298, 2.845375778867859751 ) ) ;
#179605 =( NAMED_UNIT ( * ) SI_UNIT ( $, .STERADIAN. ) SOLID_ANGLE_UNIT ( ) );
#179606 = CARTESIAN_POINT ( 'NONE',  ( 5.220932206144772714, 1.444093599275039885, -1.253800916539760113 ) ) ;
#179607 = CARTESIAN_POINT ( 'NONE',  ( -8.670602931139386627, 10.07445716020612103, 1.199719254218462483 ) ) ;
#179608 = CARTESIAN_POINT ( 'NONE',  ( -4.326460416536637155, 8.061637896019123062, 0.000000000000000000 ) ) ;
#179610 = CARTESIAN_POINT ( 'NONE',  ( 3.379631771358857950, 1.185797501207178861, 1.446808710765794315 ) ) ;
#179609 = CARTESIAN_POINT ( 'NONE',  ( 4.862875367868015886, 0.2033134212856284595, -2.080814050062954390 ) ) ;
#179611 = CARTESIAN_POINT ( 'NONE',  ( 7.212574532790092974, 9.437756259720353924, -1.443375672974057666 ) ) ;
#179612 = CARTESIAN_POINT ( 'NONE',  ( 5.724118993814841794, 1.776208094789998304, 0.4848738846057951135 ) ) ;
#179613 = AXIS2_PLACEMENT_3D ( 'NONE', #22253, #186909, #204197 ) ;
#179614 = CARTESIAN_POINT ( 'NONE',  ( 3.708318708537623021, 4.285125567170706695, -1.199719254218446718 ) ) ;
#179616 = CARTESIAN_POINT ( 'NONE',  ( 3.493197133815315603, 7.227147089426516402, -0.7998128361456291469 ) ) ;
#179615 = CARTESIAN_POINT ( 'NONE',  ( 4.245111494854632461, 7.966730820723463502, 0.000000000000000000 ) ) ;
#179617 = CARTESIAN_POINT ( 'NONE',  ( 4.881344157179084320, 1.607756147011094150, -0.6252594192169037557 ) ) ;
#179618 = CARTESIAN_POINT ( 'NONE',  ( -7.413611068574208041, 7.543634422958360730, 0.7998128361456341429 ) ) ;
#179619 = CARTESIAN_POINT ( 'NONE',  ( -10.89999999999920277, -2.102183477038263480E-15, -0.2598076211376263434 ) ) ;
#179620 = CARTESIAN_POINT ( 'NONE',  ( 0.3585786437626907741, 3.975028841772316301, -0.9637995837462947080 ) ) ;
#179621 = CARTESIAN_POINT ( 'NONE',  ( -1.500000000000058398, 7.360382131182438670, -4.205521753552950770 ) ) ;
#179622 = CARTESIAN_POINT ( 'NONE',  ( 4.276368498475341617, -1.111101898244113872, -1.865058090000100366 ) ) ;
#179623 = CARTESIAN_POINT ( 'NONE',  ( 3.721172816245840842, -0.1328194893376876962, 1.820914920514608459 ) ) ;
#179624 = CARTESIAN_POINT ( 'NONE',  ( 1.358172466202983042, -1.961936380284023063, -0.005482119489134959674 ) ) ;
#179625 = CARTESIAN_POINT ( 'NONE',  ( 5.700440484604645697, 1.420036636931173657, -1.570746850784213056 ) ) ;
#179626 = EDGE_CURVE ( 'NONE', #80292, #130319, #70299, .T. ) ;
#179628 = CARTESIAN_POINT ( 'NONE',  ( -1.364683531250010295, 4.092708333674751842, 0.7879004041258379498 ) ) ;
#179627 = CARTESIAN_POINT ( 'NONE',  ( 6.181209693220585777, 1.577568176048673720, 1.663411239723869173 ) ) ;
#179629 = LINE ( 'NONE', #147138, #5502 ) ;
#179630 = CARTESIAN_POINT ( 'NONE',  ( 9.413438726589914651, 9.876766690643398405, 0.000000000000000000 ) ) ;
#179631 = CARTESIAN_POINT ( 'NONE',  ( 2.069135417989849568, -1.637292086295978111, 1.347470637625711731 ) ) ;
#179632 = CARTESIAN_POINT ( 'NONE',  ( -4.622967192579922724, 4.495809267539077503, 1.214306433183764966E-14 ) ) ;
#179634 = EDGE_CURVE ( 'NONE', #62251, #110706, #178080, .T. ) ;
#179633 = PRESENTATION_LAYER_ASSIGNMENT (  '', '', ( #158924 ) ) ;
#179635 = CARTESIAN_POINT ( 'NONE',  ( 0.000000000000000000, 6.499999999999999112, 0.000000000000000000 ) ) ;
#179636 = CARTESIAN_POINT ( 'NONE',  ( -5.897433631820158340, 5.982686779986042147, 0.7216878364870317197 ) ) ;
#179637 = CARTESIAN_POINT ( 'NONE',  ( 6.104372708633159839, 2.168188666507598228, 0.1146961476086311021 ) ) ;
#179639 = CARTESIAN_POINT ( 'NONE',  ( -0.7500000000000179856, 14.32291666734946567, 1.299038105676658228 ) ) ;
#179638 = CARTESIAN_POINT ( 'NONE',  ( 6.883263157960349155, 7.052567563008111051, 2.551962282169925711 ) ) ;
#179641 = ORIENTED_EDGE ( 'NONE', *, *, #143420, .T. ) ;
#179640 = CARTESIAN_POINT ( 'NONE',  ( 2.579030809547431247, -1.529751724882743247, 1.610829425214066246 ) ) ;
#179642 = CARTESIAN_POINT ( 'NONE',  ( 0.5636314131802122596, -1.270468259257762966, 1.915555708879124852 ) ) ;
#179644 = CARTESIAN_POINT ( 'NONE',  ( 5.559457797297955750, 1.683061182826322666, 1.192002683324727252 ) ) ;
#179643 = CARTESIAN_POINT ( 'NONE',  ( 9.490344339885973923, 12.09515436799890331, -1.443375672974057666 ) ) ;
#179646 = CARTESIAN_POINT ( 'NONE',  ( 3.475000000000000533, -1.195833333333332194, -2.006292185433951047 ) ) ;
#179645 = CARTESIAN_POINT ( 'NONE',  ( 5.987861119090863049, 7.014868056141362551, 1.199719254218452047 ) ) ;
#179647 = CARTESIAN_POINT ( 'NONE',  ( 4.538947565524982686, 8.517465603079630299, 0.000000000000000000 ) ) ;
#179648 = CARTESIAN_POINT ( 'NONE',  ( 0.000000000000000000, -4.134374999522041350, -3.793834371823813001 ) ) ;
#179649 = DIRECTION ( 'NONE',  ( 0.000000000000000000, 0.000000000000000000, -1.000000000000000000 ) ) ;
#179650 = CARTESIAN_POINT ( 'NONE',  ( 5.794452930745782382, 1.501506822132542718, -1.065412412061928160 ) ) ;
#179651 = CARTESIAN_POINT ( 'NONE',  ( 4.157546660884947620, 8.002221537674429896, 1.040834085586084257E-14 ) ) ;
#179652 =( NAMED_UNIT ( * ) PLANE_ANGLE_UNIT ( ) SI_UNIT ( $, .RADIAN. ) );
#179653 = CARTESIAN_POINT ( 'NONE',  ( 1.535739282219195978, 0.8544175402723229729, -1.498188246372294863 ) ) ;
#179654 = CARTESIAN_POINT ( 'NONE',  ( 1.551970632248239612, 1.040795554343958429, 1.727062486439542965 ) ) ;
#179655 = CARTESIAN_POINT ( 'NONE',  ( 1.547921954348607354, -1.621480451111120047, 1.629585861659810009 ) ) ;
#179656 = CARTESIAN_POINT ( 'NONE',  ( 1.364683531249988535, 3.467708333674749621, -0.7879004041258239610 ) ) ;
#179657 = CARTESIAN_POINT ( 'NONE',  ( 2.284789498180723744, -2.218439058979736700, -0.4430748376489759832 ) ) ;
#179658 = CARTESIAN_POINT ( 'NONE',  ( 4.600280035732231987, -2.105589688358105782, -0.05227242994678206467 ) ) ;
#179659 = CARTESIAN_POINT ( 'NONE',  ( -3.363304624641834106, 6.081549941127532222, -1.199719254218452047 ) ) ;
#179660 = CARTESIAN_POINT ( 'NONE',  ( 2.108344674345350445, 1.315072395666099236, -1.184512757523252358 ) ) ;
#179661 = CARTESIAN_POINT ( 'NONE',  ( 5.113396490648394632, 9.117379672398465473, 1.040834085586084257E-14 ) ) ;
#179662 = CARTESIAN_POINT ( 'NONE',  ( 5.248414861821569133, 6.256143772614186638, -1.082531754730548412 ) ) ;
#179663 = CARTESIAN_POINT ( 'NONE',  ( -5.005985031943793295, 6.863401842066301661, -1.599625672291256295 ) ) ;
#179664 = PRESENTATION_LAYER_ASSIGNMENT (  '', '', ( #82712 ) ) ;
#179665 = CARTESIAN_POINT ( 'NONE',  ( 1.499999999999989120, 2.025000000000019895, 1.214306433183764966E-14 ) ) ;
#179666 = CARTESIAN_POINT ( 'NONE',  ( 5.924141181918635368, -2.204746212865996480, 0.2713366554644781603 ) ) ;
#179667 = CARTESIAN_POINT ( 'NONE',  ( 3.714928722721734911, -0.1615716889580356697, 2.185543052782303874 ) ) ;
#179668 = CARTESIAN_POINT ( 'NONE',  ( -4.948889764188092677, 5.732458465429559169, 1.199719254218462483 ) ) ;
#179669 = DIRECTION ( 'NONE',  ( 5.551115123125764213E-17, 0.000000000000000000, -1.000000000000000000 ) ) ;
#179670 = CARTESIAN_POINT ( 'NONE',  ( 6.498696114369957755, -2.079444522786470184, -0.4142970760486197612 ) ) ;
#179671 = CARTESIAN_POINT ( 'NONE',  ( 1.364683531249990311, 2.634375000341422801, 1.214306433183764966E-14 ) ) ;
#179672 = CARTESIAN_POINT ( 'NONE',  ( -1.364683531250014514, 8.838541667008069425, -0.7879004041258335089 ) ) ;
#179673 = CARTESIAN_POINT ( 'NONE',  ( -2.955314298098991266, 6.391691081183366485, 0.7216878364870317197 ) ) ;
#179674 = CARTESIAN_POINT ( 'NONE',  ( 6.029554895997981667, -0.2579198037528374066, 2.104758538420265168 ) ) ;
#179675 = CARTESIAN_POINT ( 'NONE',  ( -6.794044374223859428, 7.099008989448849505, 0.000000000000000000 ) ) ;
#179676 = ORIENTED_EDGE ( 'NONE', *, *, #146727, .F. ) ;
#179677 = CARTESIAN_POINT ( 'NONE',  ( -4.163762573172648196, 7.871823745427799501, 0.000000000000000000 ) ) ;
#179678 = CARTESIAN_POINT ( 'NONE',  ( 6.017121246366603060, 5.914396297049491658, 1.040834085586084257E-14 ) ) ;
#179679 = CARTESIAN_POINT ( 'NONE',  ( 5.847170753249844033, 0.5281823367668266878, -1.763884204139199330 ) ) ;
#179680 = FACE_OUTER_BOUND ( 'NONE', #83595, .T. ) ;
#179681 = AXIS2_PLACEMENT_3D ( 'NONE', #192742, #10794, #207933 ) ;
#179682 = CARTESIAN_POINT ( 'NONE',  ( 2.889872605471108802, 6.605953636083950364, -2.420000000000002149 ) ) ;
#179683 = CARTESIAN_POINT ( 'NONE',  ( -1.364683531250012516, 3.801041667008087099, -0.7879004041258300672 ) ) ;
#179684 = CARTESIAN_POINT ( 'NONE',  ( 2.190578792945916842, 1.345991196328416573, 1.103389618610579381 ) ) ;
#179685 = CARTESIAN_POINT ( 'NONE',  ( -5.807688785661975217, 6.901678836137074668, -1.092232961817845904 ) ) ;
#179686 = FACE_OUTER_BOUND ( 'NONE', #90243, .T. ) ;
#179687 = CARTESIAN_POINT ( 'NONE',  ( -0.6823417656250246877, -0.1364583329919108468, 1.181850606188755259 ) ) ;
#179688 = CARTESIAN_POINT ( 'NONE',  ( -4.303094902415906198, 7.389312076987425648, -1.073240500945132236 ) ) ;
#179689 = CIRCLE ( 'NONE', #37896, 0.07999999999999934941 ) ;
#179690 = CARTESIAN_POINT ( 'NONE',  ( 6.807524309086420367, -0.4794501827766698421, 2.115671360755105646 ) ) ;
#179691 = CARTESIAN_POINT ( 'NONE',  ( -2.137381772448751605, 5.645362501165475777, -0.7998128361456281477 ) ) ;
#179692 = CARTESIAN_POINT ( 'NONE',  ( -6.277061933002790362, 8.346324893301817482, 1.443375672974078761 ) ) ;
#179693 = B_SPLINE_CURVE_WITH_KNOTS ( 'NONE', 3,
 ( #138754, #22825, #119352, #5498, #118285, #38044 ),
 .UNSPECIFIED., .F., .F.,
 ( 4, 2, 4 ),
 ( 0.0001064780297606581909, 0.0003688581118774151668, 0.0006312381939941720749 ),
 .UNSPECIFIED. ) ;
#179694 = CARTESIAN_POINT ( 'NONE',  ( 6.034075718726629844, 1.069613854859407631, -1.878468107683453514 ) ) ;
#179696 = VERTEX_POINT ( 'NONE', #212440 ) ;
#179695 = CARTESIAN_POINT ( 'NONE',  ( 0.000000000000000000, -0.5000000000000005551, 0.000000000000000000 ) ) ;
#179697 = CARTESIAN_POINT ( 'NONE',  ( -1.364683531249997417, 4.259375000341424133, 1.214306433183764966E-14 ) ) ;
#179699 = CARTESIAN_POINT ( 'NONE',  ( 5.905538618093676639, -0.4813517389176332206, 1.911553968036589390 ) ) ;
#179698 = B_SPLINE_CURVE_WITH_KNOTS ( 'NONE', 3,
 ( #81107, #180738, #61662, #113683, #29163, #148257 ),
 .UNSPECIFIED., .F., .F.,
 ( 4, 2, 4 ),
 ( 0.000000000000000000, 0.0003168911866439334617, 0.0006337823732878669234 ),
 .UNSPECIFIED. ) ;
#179700 = CARTESIAN_POINT ( 'NONE',  ( 4.850818353276647343, -0.8162368348260983231, 1.529697846671844941 ) ) ;
#179702 = CARTESIAN_POINT ( 'NONE',  ( 2.349409277133751139, 0.5813161652389825518, -2.113004480973964760 ) ) ;
#179701 = CARTESIAN_POINT ( 'NONE',  ( -5.157946788997579689E-14, -0.2968749996585513529, 1.570758158831766060 ) ) ;
#179703 = CARTESIAN_POINT ( 'NONE',  ( 3.470030448073280205, 2.251904571161921442, -0.5032320387977330389 ) ) ;
#179704 = CARTESIAN_POINT ( 'NONE',  ( 5.430957059787441032, 0.1471976826952873518, 2.055563341089384988 ) ) ;
#179705 = CARTESIAN_POINT ( 'NONE',  ( 0.9197484630441244979, 1.157134895311136669, -1.559417598425276719 ) ) ;
#179706 = CARTESIAN_POINT ( 'NONE',  ( -6.249945625775490399, 7.354319987235250267, 1.082531754730549967 ) ) ;
#179707 = CARTESIAN_POINT ( 'NONE',  ( -4.736594563127865420, 6.619389305106191834, -1.599625672291271394 ) ) ;
#179708 = CARTESIAN_POINT ( 'NONE',  ( 11.84668730067608600, 19.00000000000000000, 1.319999999999998286 ) ) ;
#179709 = EDGE_CURVE ( 'NONE', #55695, #132514, #128109, .T. ) ;
#179710 = CARTESIAN_POINT ( 'NONE',  ( 3.498385214435925317, -1.041973313016024472, 1.846846941210858351 ) ) ;
#179711 = CARTESIAN_POINT ( 'NONE',  ( 1.934220422044398813, -1.621183349045727473, -1.198859219795316955 ) ) ;
#179712 = CARTESIAN_POINT ( 'NONE',  ( -6.846504384776774366, 7.089935991768773427, -0.7216878364870267237 ) ) ;
#179713 = CARTESIAN_POINT ( 'NONE',  ( 4.928867898441261275, 2.110505041808665716, 0.6446608841527908806 ) ) ;
#179714 = CARTESIAN_POINT ( 'NONE',  ( 0.000000000000000000, -0.6343749995220417937, -3.793834371823813001 ) ) ;
#179715 = CARTESIAN_POINT ( 'NONE',  ( 0.3914079065635684973, 3.043201908700336578, -0.4248930002255459359 ) ) ;
#179716 = CARTESIAN_POINT ( 'NONE',  ( 0.09986456629675066754, -1.825204794925545881, -0.04862044751281074939 ) ) ;
#179717 = CARTESIAN_POINT ( 'NONE',  ( -6.668631453075260396, 8.873432343378178544, -1.599625672291271394 ) ) ;
#179719 = CARTESIAN_POINT ( 'NONE',  ( -10.96964784646768365, -7.712340523144905369, 0.6288774950739232095 ) ) ;
#179718 = CARTESIAN_POINT ( 'NONE',  ( -5.840188366348757931, 7.302172906674928576, 1.289283945506283890 ) ) ;
#179720 = CARTESIAN_POINT ( 'NONE',  ( -9.828980619278564011E-14, 7.054063922337708625, 3.955400951015630273 ) ) ;
#179721 = ORIENTED_EDGE ( 'NONE', *, *, #130414, .T. ) ;
#179722 = CARTESIAN_POINT ( 'NONE',  ( 4.768464766973178115, -1.347833537202504317, 1.559116658007191347 ) ) ;
#179723 = CARTESIAN_POINT ( 'NONE',  ( -7.146556367734805626, 9.431011410480991231, 1.443375672974064550 ) ) ;
#179724 = CARTESIAN_POINT ( 'NONE',  ( 6.620655732516624425, 7.629137130509072051, 2.773739711112707784 ) ) ;
#179725 = CARTESIAN_POINT ( 'NONE',  ( -4.497554271431319250, 6.270232621468402989, -1.599625672291256295 ) ) ;
#179726 = CARTESIAN_POINT ( 'NONE',  ( -3.494969737272722643, 7.299491470118629088, -0.7998128361456481317 ) ) ;
#179727 = CARTESIAN_POINT ( 'NONE',  ( 3.721357204503534355, 1.733397938510993885, 1.036269837853747378 ) ) ;
#179728 = CARTESIAN_POINT ( 'NONE',  ( -1.402160292154681736E-14, 0.5875000000000220046, -1.732050807568863648 ) ) ;
#179729 = CARTESIAN_POINT ( 'NONE',  ( 9.490344339885973923, 12.09515436799890331, -1.443375672974057666 ) ) ;
#179730 = CARTESIAN_POINT ( 'NONE',  ( 6.446011968293428041, 9.607765498729298415, -1.199719254218440723 ) ) ;
#179731 = CARTESIAN_POINT ( 'NONE',  ( 3.063408159219972227, 0.3037436250956357386, -2.038260327603860222 ) ) ;
#179732 = EDGE_CURVE ( 'NONE', #18531, #37868, #136652, .T. ) ;
#179733 = DIRECTION ( 'NONE',  ( -0.000000000000000000, -1.000000000000000000, -0.000000000000000000 ) ) ;
#179734 = CARTESIAN_POINT ( 'NONE',  ( 3.845709127770629010, 7.638411082374393146, 0.7998128361456321445 ) ) ;
#179735 = COLOUR_RGB ( '', 0.72549020, 0.75294118, 0.79215686) ;
#179736 = CARTESIAN_POINT ( 'NONE',  ( -0.2411972340275969906, 1.382285239182699854, -2.157708601731861187 ) ) ;
#179737 = CARTESIAN_POINT ( 'NONE',  ( 1.446930991382020748, 0.5358794165791405106, -1.761430032344503349 ) ) ;
#179738 = CARTESIAN_POINT ( 'NONE',  ( 6.287735281038357549, 1.518688880046001444, 1.601449620450722700 ) ) ;
#179739 = CARTESIAN_POINT ( 'NONE',  ( 4.929271367020211514, 7.908511140569038922, 1.199719254218452047 ) ) ;
#179740 = CARTESIAN_POINT ( 'NONE',  ( 2.354944161360218224, -1.672559397656541824, 1.369352967626968898 ) ) ;
#179741 = CARTESIAN_POINT ( 'NONE',  ( -2.982430605326321427, 6.423326772948587227, -0.7216878364870267237 ) ) ;
#179742 = CARTESIAN_POINT ( 'NONE',  ( 1.727750297885573882, 0.7672897036171549834, -1.865047645237365215 ) ) ;
#179743 = CARTESIAN_POINT ( 'NONE',  ( 4.226925616482860804, 3.500738074553328527, -2.444828727306142202 ) ) ;
#179744 = CARTESIAN_POINT ( 'NONE',  ( 0.3209005354254980680, -0.09642172165634513292, 1.868300368337752815 ) ) ;
#179745 = CARTESIAN_POINT ( 'NONE',  ( 5.014510501881845883, 1.360076575639699081, -1.427402630902480762 ) ) ;
#179746 = CARTESIAN_POINT ( 'NONE',  ( 4.733611406029458735, 0.6279933214467496860, -1.916352419866963697 ) ) ;
#179748 = CARTESIAN_POINT ( 'NONE',  ( 10.35806617071623315, 11.18675807536486566, 0.000000000000000000 ) ) ;
#179747 = CARTESIAN_POINT ( 'NONE',  ( -1.201851678989727383E-14, 3.571875000341422357, 1.575800808251672791 ) ) ;
#179750 = CARTESIAN_POINT ( 'NONE',  ( 6.393207918867057415, 1.833407501889987357, -1.036277073347695588 ) ) ;
#179749 = CARTESIAN_POINT ( 'NONE',  ( -5.865874016206865882, 9.995270118883347266, 0.000000000000000000 ) ) ;
#179751 = EDGE_CURVE ( 'NONE', #150697, #83956, #177843, .T. ) ;
#179752 = CARTESIAN_POINT ( 'NONE',  ( 6.162566008723842081, -0.7415158119226210598, -1.933206815039355320 ) ) ;
#179753 = CARTESIAN_POINT ( 'NONE',  ( 6.518772930072240790, 6.499656594706071822, -0.7998128361456281477 ) ) ;
#179754 = CARTESIAN_POINT ( 'NONE',  ( -6.632963465583701534, 8.761543347979550589, -1.599625672291263179 ) ) ;
#179755 = CARTESIAN_POINT ( 'NONE',  ( -1.491528662501878655, 8.751894132169937279, 2.513572095680582041 ) ) ;
#179756 = CARTESIAN_POINT ( 'NONE',  ( 4.065273027966066266, 0.2426392691956253123, -1.956424757721614949 ) ) ;
#179757 = CARTESIAN_POINT ( 'NONE',  ( 6.222917004181202749, 1.493787235515126044, -1.359621011941100743 ) ) ;
#179758 = CARTESIAN_POINT ( 'NONE',  ( -1.500000000000013101, 0.4520833340161533598, 0.8660254037844403729 ) ) ;
#179759 = CARTESIAN_POINT ( 'NONE',  ( 4.969473931871945638, 0.2302171888925855225, -2.296178194122914018 ) ) ;
#179760 = ADVANCED_FACE ( 'NONE', ( #43587 ), #194067, .F. ) ;
#179761 = CARTESIAN_POINT ( 'NONE',  ( 1.885666897375902096, -1.943580278752204515, 0.6908589954031388869 ) ) ;
#179762 = CARTESIAN_POINT ( 'NONE',  ( 6.751597309925441159, 9.860318714012938912, -1.082531754730537088 ) ) ;
#179763 = CARTESIAN_POINT ( 'NONE',  ( 5.234329823327693809, 8.264412672927770487, 1.199719254218451159 ) ) ;
#179764 = CARTESIAN_POINT ( 'NONE',  ( 5.734172623936983904, 5.654565914206774124, 0.7998128361456352531 ) ) ;
#179765 = CARTESIAN_POINT ( 'NONE',  ( -0.6823417656250246877, 0.1135416670080893753, 1.181850606188755259 ) ) ;
#179766 = CARTESIAN_POINT ( 'NONE',  ( 4.903208829997618423, 5.749440385532527564, -1.199719254218450271 ) ) ;
#179767 = CARTESIAN_POINT ( 'NONE',  ( 7.592202833528386208, 7.959917515312338487, 1.040834085586084257E-14 ) ) ;
#179768 = CARTESIAN_POINT ( 'NONE',  ( 3.947858391199970285, 1.570127341852745273, 1.499791163327832466 ) ) ;
#179770 = CARTESIAN_POINT ( 'NONE',  ( 2.665370095338463585, 0.9869154847663293983, 1.554228294351194473 ) ) ;
#179769 = CARTESIAN_POINT ( 'NONE',  ( -3.253593677599670109, 5.779314476299451719, 1.082531754730560403 ) ) ;
#179771 = CARTESIAN_POINT ( 'NONE',  ( 0.6823417656249917140, 4.592708333674755394, 1.181850606188765695 ) ) ;
#179772 = CARTESIAN_POINT ( 'NONE',  ( 5.636325218313963603, 0.4264374063192889475, 2.149501299143250055 ) ) ;
#179773 = CARTESIAN_POINT ( 'NONE',  ( 1.500000000000007105, 10.64264068711930733, 1.214306433183764966E-14 ) ) ;
#179774 = CARTESIAN_POINT ( 'NONE',  ( 6.438354578037611908, 2.236760482230481184, 0.3397759937929164531 ) ) ;
#179775 = CARTESIAN_POINT ( 'NONE',  ( -5.057943438340505082, 6.748278329294532085, -1.445135742742007068 ) ) ;
#179776 = CARTESIAN_POINT ( 'NONE',  ( 5.371503168974233411, 7.687194297833679357, 1.321221623412481394 ) ) ;
#179777 = CARTESIAN_POINT ( 'NONE',  ( -5.438229012412899799, 7.437962829272074750, -1.443375672974066548 ) ) ;
#179778 = CARTESIAN_POINT ( 'NONE',  ( 0.08049558579637566824, -0.1306036352819762714, -1.740669940395103366 ) ) ;
#179779 = CARTESIAN_POINT ( 'NONE',  ( -1.364683531250014514, 12.58854166700806054, -0.7879004041258335089 ) ) ;
#179780 = CARTESIAN_POINT ( 'NONE',  ( 4.547525146836687959, -1.839596654198237369, 0.8179813495266550216 ) ) ;
#179781 = CARTESIAN_POINT ( 'NONE',  ( 7.630541526392844887, 7.796719957080126662, 0.7998128361456341429 ) ) ;
#179782 = CARTESIAN_POINT ( 'NONE',  ( 3.030406611367501224, 1.171151514522270398, -1.750062178063223506 ) ) ;
#179783 = CARTESIAN_POINT ( 'NONE',  ( 2.618635445852790511, 0.2369565241663183774, 1.900835938982778472 ) ) ;
#179784 = CARTESIAN_POINT ( 'NONE',  ( 5.020596955762157698, 4.751784624677624080, 1.040834085586084257E-14 ) ) ;
#179785 = CARTESIAN_POINT ( 'NONE',  ( 2.611712457634679296, 0.5281755657932221126, -1.897318813625125777 ) ) ;
#179786 = CARTESIAN_POINT ( 'NONE',  ( 1.481098450213329976, 1.729700800547562478, -0.7128637423776186255 ) ) ;
#179787 = CARTESIAN_POINT ( 'NONE',  ( 1.574581288703358339, 1.320057194528483135, -1.451483715152704246 ) ) ;
#179790 = ORIENTED_EDGE ( 'NONE', *, *, #164554, .T. ) ;
#179789 = CARTESIAN_POINT ( 'NONE',  ( -0.1405747822309927342, -1.479430311965252542, -1.211566217618691210 ) ) ;
#179788 = CARTESIAN_POINT ( 'NONE',  ( 4.494587217144647262, -0.3816326207147257010, -1.681953545215847168 ) ) ;
#179792 = CARTESIAN_POINT ( 'NONE',  ( 5.260200412422194383, 7.159986452624450770, -1.443375672974051449 ) ) ;
#179791 = CARTESIAN_POINT ( 'NONE',  ( 0.9267433102794273569, 1.311770220233858586, -1.774563083084364834 ) ) ;
#179793 = CARTESIAN_POINT ( 'NONE',  ( -1.364683531250014514, 1.301041667008083325, -0.7879004041258289570 ) ) ;
#179794 = CIRCLE ( 'NONE', #207452, 0.08000000000000020983 ) ;
#179795 = CARTESIAN_POINT ( 'NONE',  ( 6.578970801323708706, -0.09418725797194843485, -1.868394071727994321 ) ) ;
#179796 = CARTESIAN_POINT ( 'NONE',  ( -8.773304256324728101, 3.742896273583257383, -7.826845210040933587 ) ) ;
#179797 = CARTESIAN_POINT ( 'NONE',  ( 6.818239719371234742, -6.631671897294228124, -6.594971851908891125 ) ) ;
#179798 = CARTESIAN_POINT ( 'NONE',  ( 6.596543124887806364, 2.046857425119428697, 0.3097440254393943881 ) ) ;
#179799 = CARTESIAN_POINT ( 'NONE',  ( 0.6958625912084138720, -1.462932864358768459, -1.465259690088885014 ) ) ;
#179800 = CARTESIAN_POINT ( 'NONE',  ( -1.500000000000001332, 1.400000000000019229, 0.000000000000000000 ) ) ;
#179801 = CARTESIAN_POINT ( 'NONE',  ( 7.610204295972345712, 7.772993188256215547, 0.7998128361456341429 ) ) ;
#179802 = CARTESIAN_POINT ( 'NONE',  ( -8.715193815486133033, 9.062147627688959872, 0.7998128361456462443 ) ) ;
#179803 = CARTESIAN_POINT ( 'NONE',  ( 5.825163275726873202, 6.825053905550038991, 1.199719254218452047 ) ) ;
#179804 = CARTESIAN_POINT ( 'NONE',  ( 5.725269513181780567, 1.870077439114096629, 0.9995941271150191598 ) ) ;
#179805 =( NAMED_UNIT ( * ) SI_UNIT ( $, .STERADIAN. ) SOLID_ANGLE_UNIT ( ) );
#179806 = CARTESIAN_POINT ( 'NONE',  ( 1.364683531249988757, 1.634375000341421691, 0.000000000000000000 ) ) ;
#179807 = ORIENTED_EDGE ( 'NONE', *, *, #191370, .F. ) ;
#179808 = CARTESIAN_POINT ( 'NONE',  ( -1.500000000000013101, 2.879166666666688634, -0.8660254037844313801 ) ) ;
#179810 = CARTESIAN_POINT ( 'NONE',  ( 3.171717870593107058, 5.787755718078879674, -1.199719254218446718 ) ) ;
#179809 = CARTESIAN_POINT ( 'NONE',  ( 6.672321430365630412, -0.9237476215336395402, -1.730755693189582667 ) ) ;
#179811 = CARTESIAN_POINT ( 'NONE',  ( 4.288435361214689046, -1.930121902525683053, 0.5825675424541224556 ) ) ;
#179812 = CARTESIAN_POINT ( 'NONE',  ( 3.766719225569253204, -0.1932013629946625344, -1.905979854919868988 ) ) ;
#179813 = DIRECTION ( 'NONE',  ( 1.224646799147349509E-16, 0.000000000000000000, -1.000000000000000000 ) ) ;
#179814 = CARTESIAN_POINT ( 'NONE',  ( 1.628746693258641853, 0.2190750365392846177, 2.180598679842937759 ) ) ;
#179815 = CARTESIAN_POINT ( 'NONE',  ( -1.898923903056559004, 3.739065552179622554, 0.3999999999999835909 ) ) ;
#179816 = CARTESIAN_POINT ( 'NONE',  ( 2.864352374448192240, -1.292745417840788003, 1.352161534859085412 ) ) ;
#179817 = CARTESIAN_POINT ( 'NONE',  ( 0.7499999999999885647, 1.097916667349485564, -1.299038105676652899 ) ) ;
#179818 = CARTESIAN_POINT ( 'NONE',  ( -6.612626235163205024, 8.737816579155630592, -1.599625672291263179 ) ) ;
#179820 = CARTESIAN_POINT ( 'NONE',  ( 5.343409318383084639, 0.4121200312635669993, -2.076573192147526115 ) ) ;
#179819 = CARTESIAN_POINT ( 'NONE',  ( -4.039966587192274083, 5.736380323189513852, 1.443375672974064550 ) ) ;
#179821 = CARTESIAN_POINT ( 'NONE',  ( -0.6823417656250039265, 8.880208333674733723, -1.181850606188755259 ) ) ;
#179823 = LINE ( 'NONE', #15160, #59877 ) ;
#179822 = CARTESIAN_POINT ( 'NONE',  ( 2.823863332701610940, 1.159264052448713889, -1.739707760033171180 ) ) ;
#179825 = VERTEX_POINT ( 'NONE', #175709 ) ;
#179824 = CARTESIAN_POINT ( 'NONE',  ( 0.5688600258280833710, 0.1761389027815796759, -1.715759018540372827 ) ) ;
#179826 = CARTESIAN_POINT ( 'NONE',  ( 5.615048174354031474, 9.702639970055050966, 0.7998128361456462443 ) ) ;
#179827 =( LENGTH_UNIT ( ) NAMED_UNIT ( * ) SI_UNIT ( .MILLI., .METRE. ) );
#179828 = CARTESIAN_POINT ( 'NONE',  ( 0.000000000000000000, -9.900000000000005684, 9.579665964948883783 ) ) ;
#179829 = CARTESIAN_POINT ( 'NONE',  ( 6.689804758640306659, -7.818797203689485720, -6.745710774231028495 ) ) ;
#179831 = CARTESIAN_POINT ( 'NONE',  ( 9.205623113554624481, 10.80261038964432707, 1.082531754730549967 ) ) ;
#179830 = CARTESIAN_POINT ( 'NONE',  ( 5.445571254183207088, 9.504916896522420444, -0.7998128361456281477 ) ) ;
#179832 = ORIENTED_EDGE ( 'NONE', *, *, #139632, .F. ) ;
#179833 = CARTESIAN_POINT ( 'NONE',  ( -1.882262909678046769, 3.299172163371774325, 0.4004916885352270417 ) ) ;
#179835 = CARTESIAN_POINT ( 'NONE',  ( 1.523755425131537278, -1.797796875034236797, 0.2216367714752715545 ) ) ;
#179834 = CARTESIAN_POINT ( 'NONE',  ( 5.342795052237045539, 8.390955439988655229, -1.199719254218450271 ) ) ;
#179836 = CARTESIAN_POINT ( 'NONE',  ( -6.181627972826976958, 9.299317504018391745, 1.199719254218452047 ) ) ;
#179837 = CARTESIAN_POINT ( 'NONE',  ( 3.818592820543298405, 7.606775390609172405, -0.7998128361456221525 ) ) ;
#179838 = CARTESIAN_POINT ( 'NONE',  ( 4.376249722160992839, 8.327651452488305850, 0.000000000000000000 ) ) ;
#179839 = CARTESIAN_POINT ( 'NONE',  ( 6.639320575229252341, 0.005161017367553630275, 1.896863882003448021 ) ) ;
#179840 = CARTESIAN_POINT ( 'NONE',  ( 4.324073113486339714, 7.195437805949965515, 1.011975886212188813 ) ) ;
#179841 = CARTESIAN_POINT ( 'NONE',  ( 8.378575743565351175, 11.75846021992619406, -1.082531754730543083 ) ) ;
#179842 = VERTEX_POINT ( 'NONE', #27299 ) ;
#179843 = AXIS2_PLACEMENT_3D ( 'NONE', #185697, #196894, #132999 ) ;
#179844 = CARTESIAN_POINT ( 'NONE',  ( 2.998338655031260735, 1.846661096025622228, 0.2305314943511579950 ) ) ;
#179845 = CARTESIAN_POINT ( 'NONE',  ( 0.8607750341611281053, -0.04820650858186093651, -1.915179348411770954 ) ) ;
#179846 = CARTESIAN_POINT ( 'NONE',  ( 6.563506682682211490, 0.3285509523427312950, -1.898022546839329472 ) ) ;
#179847 = CARTESIAN_POINT ( 'NONE',  ( -11.94655611907590220, 13.65200944546904083, 1.134828163062136852 ) ) ;
#179848 = CARTESIAN_POINT ( 'NONE',  ( -1.499999999999997780, 3.681250000682819046, 1.214306433183764966E-14 ) ) ;
#179849 = CARTESIAN_POINT ( 'NONE',  ( 4.700249516990034238, 8.244041944096728969, -0.6212051699984559860 ) ) ;
#179850 = SURFACE_SIDE_STYLE ('',( #111716 ) ) ;
#179851 = CARTESIAN_POINT ( 'NONE',  ( -2.318081078256692518, 5.648252324700675508, 1.040834085586084257E-14 ) ) ;
#179852 = CARTESIAN_POINT ( 'NONE',  ( 8.161645285746708112, 9.584636257201740506, -1.082531754730543083 ) ) ;
#179853 = CARTESIAN_POINT ( 'NONE',  ( 4.909022984592102290, -1.584153972474154459, 1.169931220002416339 ) ) ;
#179854 = CARTESIAN_POINT ( 'NONE',  ( 1.682450335255514240, 1.092831414372618326, 1.817064408815848964 ) ) ;
#179855 = CARTESIAN_POINT ( 'NONE',  ( -6.403528624356093601, 6.365204904703887223, 1.040834085586084257E-14 ) ) ;
#179856 = DIRECTION ( 'NONE',  ( 1.000000000000000000, 0.000000000000000000, 0.000000000000000000 ) ) ;
#179857 = CARTESIAN_POINT ( 'NONE',  ( 6.246043798300164873, 0.6838514278588082584, 2.082077653496945402 ) ) ;
#179858 = CARTESIAN_POINT ( 'NONE',  ( -0.4019237886466871523, 9.979914550367427140, -1.499999999999998668 ) ) ;
#179859 = CARTESIAN_POINT ( 'NONE',  ( 4.770489386553291133, -1.258480429039417592, 1.458564191902473661 ) ) ;
#179860 = CARTESIAN_POINT ( 'NONE',  ( -6.449928391799210736, 8.548002428564306143, -1.599625672291263179 ) ) ;
#179861 = CARTESIAN_POINT ( 'NONE',  ( 0.2350025537052654601, -1.671451849548213797, 0.7345932495873632728 ) ) ;
#179862 = CARTESIAN_POINT ( 'NONE',  ( 1.172829962703396456, -1.397616723802884708, 1.707921395779465890 ) ) ;
#179863 = CARTESIAN_POINT ( 'NONE',  ( -5.992450215256712731, 7.101132044915781982, 1.073800501374306382 ) ) ;
#179864 = CARTESIAN_POINT ( 'NONE',  ( -15.75000000000000000, 10.19999999999998153, 1.399999999999998579 ) ) ;
#179865 = VERTEX_POINT ( 'NONE', #64082 ) ;
#179866 = CARTESIAN_POINT ( 'NONE',  ( 2.957086901556340575, 6.464035461875470290, 0.7216878364870257245 ) ) ;
#179867 = VERTEX_POINT ( 'NONE', #45720 ) ;
#179868 = CARTESIAN_POINT ( 'NONE',  ( 6.473500209388782345, -0.2444377345085078923, 1.954170833970412913 ) ) ;
#179869 = CARTESIAN_POINT ( 'NONE',  ( 1.962350597898457671, -1.776395552165145997, -0.7852436748517297449 ) ) ;
#179870 = CARTESIAN_POINT ( 'NONE',  ( 6.556073970538053075, 2.004588421764907036, -1.124284452974108950 ) ) ;
#179872 = CARTESIAN_POINT ( 'NONE',  ( 5.910971410920907942, -1.467885462018687415, 1.143791174867914373 ) ) ;
#179871 = CARTESIAN_POINT ( 'NONE',  ( -6.363572996767778100, 8.517530811019446091, -1.599625672291271394 ) ) ;
#179873 = CARTESIAN_POINT ( 'NONE',  ( 6.900173834712277632, 7.014900660111269559, -0.7998128361456341429 ) ) ;
#179874 = CARTESIAN_POINT ( 'NONE',  ( 0.4019237886466884846, 11.42633545031536535, -1.499999999999994449 ) ) ;
#179875 = CARTESIAN_POINT ( 'NONE',  ( 3.761726504036865926, 7.402781664769409353, 0.2506311418687352521 ) ) ;
#179876 = CARTESIAN_POINT ( 'NONE',  ( -6.905180308061733996, 6.950465202360470052, 0.7998128361456341429 ) ) ;
#179877 = CARTESIAN_POINT ( 'NONE',  ( -7.774674742793745708, 8.035151719539642912, 0.7998128361456341429 ) ) ;
#179878 = CARTESIAN_POINT ( 'NONE',  ( 1.962683346935737205, -2.005255389829229351, -0.8846387633431598285 ) ) ;
#179879 = CARTESIAN_POINT ( 'NONE',  ( 5.355107487717867265, 5.349972945200037522, 1.040834085586084257E-14 ) ) ;
#179880 = ORIENTED_EDGE ( 'NONE', *, *, #158684, .T. ) ;
#179881 = CARTESIAN_POINT ( 'NONE',  ( 3.701970883082871921, 7.364863713882360052, 2.499999999999999556 ) ) ;
#179882 = CYLINDRICAL_SURFACE ( 'NONE', #51246, 1.250000000000000000 ) ;
#179883 = CARTESIAN_POINT ( 'NONE',  ( 1.541335573940459058, -1.321205422867760548, -1.260230113935792318 ) ) ;
#179884 = CARTESIAN_POINT ( 'NONE',  ( -3.541704441667874903, 5.155074486744371853, -1.599625672291256295 ) ) ;
#179885 = CARTESIAN_POINT ( 'NONE',  ( -0.3551009713840111437, 2.785693601408736342, -1.969347843778241458 ) ) ;
#179886 = LINE ( 'NONE', #31510, #181446 ) ;
#179887 = CARTESIAN_POINT ( 'NONE',  ( 9.565441069641300587, 11.11843498845840905, -1.199719254218440723 ) ) ;
#179888 = CARTESIAN_POINT ( 'NONE',  ( 0.3285744372712772199, 1.843197283691574873, 0.5604049541020996728 ) ) ;
#179889 = CARTESIAN_POINT ( 'NONE',  ( 4.030091663008243508, 1.086175826233202857, 1.633415718976807263 ) ) ;
#179890 = ADVANCED_FACE ( 'NONE', ( #29456 ), #125394, .T. ) ;
#179891 = CARTESIAN_POINT ( 'NONE',  ( -7.018317073368468328, 11.33978701890523233, -0.7998128361456291469 ) ) ;
#179892 = CARTESIAN_POINT ( 'NONE',  ( 6.810273232766058449, 6.839740281182199233, 1.040834085586084257E-14 ) ) ;
#179893 = CARTESIAN_POINT ( 'NONE',  ( 4.019203527901527018, -2.096847714747759106, 0.6372333828079318474 ) ) ;
#179894 = EDGE_CURVE ( 'NONE', #93819, #133393, #88100, .T. ) ;
#179895 = CARTESIAN_POINT ( 'NONE',  ( 6.609000000000037289, 1.265604115953523401, 2.115306440354140172 ) ) ;
#179896 = CARTESIAN_POINT ( 'NONE',  ( 4.276279003695676373, -1.059865903354087813, -1.778221194881628220 ) ) ;
#179898 = CARTESIAN_POINT ( 'NONE',  ( 0.6823417656249882723, 1.988541667008083991, -1.181850606188749264 ) ) ;
#179897 = DIRECTION ( 'NONE',  ( -0.000000000000000000, -1.000000000000000000, -0.000000000000000000 ) ) ;
#179899 = ORIENTED_EDGE ( 'NONE', *, *, #117958, .F. ) ;
#179900 = CARTESIAN_POINT ( 'NONE',  ( 3.832918613053246659, 0.7734572015929435107, -2.164792806810557746 ) ) ;
#179901 = CARTESIAN_POINT ( 'NONE',  ( 7.673551755654734130, 9.015193805427763607, -1.082531754730537976 ) ) ;
#179903 = CARTESIAN_POINT ( 'NONE',  ( -4.528060117284247177, 6.305822774963486310, 1.443375672974064550 ) ) ;
#179902 = CARTESIAN_POINT ( 'NONE',  ( 5.668717624289557833, 8.667235424096215723, -1.082531754730548412 ) ) ;
#179904 = CARTESIAN_POINT ( 'NONE',  ( -0.7500000000000179856, 8.322916667349467446, 1.299038105676658228 ) ) ;
#179905 = DIRECTION ( 'NONE',  ( 1.000000000000000000, -0.000000000000000000, -0.000000000000000000 ) ) ;
#179906 = CARTESIAN_POINT ( 'NONE',  ( 3.732312008210575627, 0.2860496425412931143, 1.920654750396868726 ) ) ;
#179907 = ORIENTED_EDGE ( 'NONE', *, *, #72198, .T. ) ;
#179908 = CARTESIAN_POINT ( 'NONE',  ( 8.541273586484978253, 12.90864358430044589, 0.000000000000000000 ) ) ;
#179909 = EDGE_CURVE ( 'NONE', #36225, #76712, #46507, .T. ) ;
#179910 = CARTESIAN_POINT ( 'NONE',  ( 4.412309042748480792, -1.912102599942141268, -0.04143165621695726192 ) ) ;
#179911 =( NAMED_UNIT ( * ) SI_UNIT ( $, .STERADIAN. ) SOLID_ANGLE_UNIT ( ) );
#179912 = CARTESIAN_POINT ( 'NONE',  ( 5.051616488536272875, 0.5384910649316194675, -1.638604462054549238 ) ) ;
#179913 = CARTESIAN_POINT ( 'NONE',  ( 4.012907874177486178, 0.1037781579101039742, 2.014008197856680393 ) ) ;
#179914 = CARTESIAN_POINT ( 'NONE',  ( 4.623847096394516853, 0.3921523929481546267, 2.264879156731691712 ) ) ;
#179915 = CARTESIAN_POINT ( 'NONE',  ( -4.559605246071217088, 3.300000000000025135, 0.7750000000000135669 ) ) ;
#179916 = CARTESIAN_POINT ( 'NONE',  ( 0.3642759247451561322, 2.182245240920151375, -0.3280614795862640820 ) ) ;
#179918 = CARTESIAN_POINT ( 'NONE',  ( -5.478903473698260029, 6.525047153136981137, -1.082531754730549967 ) ) ;
#179917 = CARTESIAN_POINT ( 'NONE',  ( -10.10098813738111545, 11.74323990082152491, -1.199719254218441611 ) ) ;
#179919 = CARTESIAN_POINT ( 'NONE',  ( 6.309784262603465699, -1.756040378898944043, 0.2188775834443684731 ) ) ;
#179921 = CARTESIAN_POINT ( 'NONE',  ( 1.887097267728707894, 1.992918150068530014, -1.132464722766779675 ) ) ;
#179920 = CARTESIAN_POINT ( 'NONE',  ( 6.561219994370630637, 6.619454513046008515, 0.000000000000000000 ) ) ;
#179922 = CARTESIAN_POINT ( 'NONE',  ( 1.007268549873532981, -0.7791258169532075950, -1.556267712415648763 ) ) ;
#179923 = DIRECTION ( 'NONE',  ( 1.000000000000000000, 0.000000000000000000, 0.000000000000000000 ) ) ;
#179924 = CARTESIAN_POINT ( 'NONE',  ( 0.6843859445029027988, -0.9204285295532282918, -1.469136994349945047 ) ) ;
#179925 = CARTESIAN_POINT ( 'NONE',  ( 1.360316468750004448, 0.2968750003413955785, -6.938893903907228378E-15 ) ) ;
#179926 = CARTESIAN_POINT ( 'NONE',  ( -11.55950211276791428, 12.21999999999998288, 3.221476510067112109 ) ) ;
#179927 = CARTESIAN_POINT ( 'NONE',  ( 1.785821596895339702, -2.044763721651895239, 0.7304308730638265912 ) ) ;
#179928 = CARTESIAN_POINT ( 'NONE',  ( 2.255092540634635156, 0.09411513195021348199, -2.014433103604281960 ) ) ;
#179929 = CARTESIAN_POINT ( 'NONE',  ( 0.7499999999999885647, 0.3479166673494848983, -1.299038105676652899 ) ) ;
#179930 = CARTESIAN_POINT ( 'NONE',  ( 0.07700591528353968596, 0.003617085621422307627, -1.910863332519038282 ) ) ;
#179931 = CARTESIAN_POINT ( 'NONE',  ( 1.364683531249996529, 13.21354166700806410, 0.7879004041258405033 ) ) ;
#179932 = CARTESIAN_POINT ( 'NONE',  ( 1.775925898354186572, 0.3739997881802308299, -2.189552662180799913 ) ) ;
#179933 = VERTEX_POINT ( 'NONE', #142078 ) ;
#179934 = CARTESIAN_POINT ( 'NONE',  ( -1.886825320689270225, 2.480000000000016858, 2.459652456995881753 ) ) ;
#179935 = CARTESIAN_POINT ( 'NONE',  ( 1.499999999999987566, -0.7249999999999825473, 0.000000000000000000 ) ) ;
#179936 = CARTESIAN_POINT ( 'NONE',  ( 6.889514614038635187, 11.18951748302043114, -0.7998128361456291469 ) ) ;
#179937 = DIRECTION ( 'NONE',  ( 0.000000000000000000, 0.000000000000000000, -1.000000000000000000 ) ) ;
#179938 = CARTESIAN_POINT ( 'NONE',  ( 1.364683531249986537, -1.136458332991912235, 0.7879004041258500513 ) ) ;
#179939 = CARTESIAN_POINT ( 'NONE',  ( 5.372502291033079302, -0.05049805449116586548, -1.739898325138872215 ) ) ;
#179940 = CARTESIAN_POINT ( 'NONE',  ( 3.156644782993088150, -0.5669402238272451822, -1.878178299617596192 ) ) ;
#179942 = CARTESIAN_POINT ( 'NONE',  ( -5.748293942514169252, 9.650167333001109071, -0.7216878364870207285 ) ) ;
#179941 = CARTESIAN_POINT ( 'NONE',  ( 4.220665892555866883, 3.818531717603609987, -0.7998128361456211532 ) ) ;
#179943 = CIRCLE ( 'NONE', #20809, 11.92000000000000171 ) ;
#179944 = CARTESIAN_POINT ( 'NONE',  ( -1.500389033793473770, 4.450847250840007874, 0.07878897303668215557 ) ) ;
#179945 = CARTESIAN_POINT ( 'NONE',  ( 5.167352989974902222, 0.2290589858122368538, -2.250810084452478765 ) ) ;
#179946 = CARTESIAN_POINT ( 'NONE',  ( 1.223174996406689585, -1.863865272486511460, -0.8838528460363299644 ) ) ;
#179947 = CARTESIAN_POINT ( 'NONE',  ( -6.989391883044787868, 8.113044270762433285, -1.199719254218446718 ) ) ;
#179948 = CARTESIAN_POINT ( 'NONE',  ( 1.973834762636607509, 2.164947816325224039, -0.6572921511966890451 ) ) ;
#179949 = ORIENTED_EDGE ( 'NONE', *, *, #54753, .T. ) ;
#179950 = CARTESIAN_POINT ( 'NONE',  ( -1.500000000000001332, 0.6812500006828161592, 0.000000000000000000 ) ) ;
#179951 = CARTESIAN_POINT ( 'NONE',  ( 2.354581831802166736, -1.448805955455864769, 1.183207591018392568 ) ) ;
#179952 = CARTESIAN_POINT ( 'NONE',  ( 1.599856272741075447, -0.2119130288822292651, 1.721036989116639493 ) ) ;
#179953 = B_SPLINE_CURVE_WITH_KNOTS ( 'NONE', 3,
 ( #168580, #152338, #39652, #102517, #202113, #117772, #22301 ),
 .UNSPECIFIED., .F., .F.,
 ( 4, 3, 4 ),
 ( 3.314949680323801069E-05, 0.0009000000012044577329, 0.001928999666871128449 ),
 .UNSPECIFIED. ) ;
#179954 = CARTESIAN_POINT ( 'NONE',  ( 5.355090213057959403, 0.4282289882464126451, -2.149144931432686256 ) ) ;
#179955 = CARTESIAN_POINT ( 'NONE',  ( 0.4642757356001780966, 2.182421439735841684, -0.3260586787675948117 ) ) ;
#179956 = CARTESIAN_POINT ( 'NONE',  ( 4.030267251519312310, 1.158562084521784108, -1.824840551714689507 ) ) ;
#179957 = CARTESIAN_POINT ( 'NONE',  ( 4.576081071864527061, -1.884036987645235417, -0.4702585519323047025 ) ) ;
#179958 = CARTESIAN_POINT ( 'NONE',  ( -4.256897044566581911, 4.068727428190179296, 1.214306433183764966E-14 ) ) ;
#179959 = CARTESIAN_POINT ( 'NONE',  ( -0.3870735955438814879, 1.000000000000000888, 11.88799243440809050 ) ) ;
#179960 = CARTESIAN_POINT ( 'NONE',  ( 2.031250000000000888, -0.7852924748300881275, -1.895863743164043491 ) ) ;
#179961 = CARTESIAN_POINT ( 'NONE',  ( 4.799922300691145338, 6.743925459469453543, 1.247687964948118733 ) ) ;
#179962 = CARTESIAN_POINT ( 'NONE',  ( -3.719872605471121751, 6.605953636083950364, 2.420000000000000373 ) ) ;
#179963 = EDGE_CURVE ( 'NONE', #205873, #94313, #191824, .T. ) ;
#179964 = CARTESIAN_POINT ( 'NONE',  ( 10.39230484541318589, 3.499999999999989342, -6.000000000000107470 ) ) ;
#179965 = CARTESIAN_POINT ( 'NONE',  ( -2.954552044183079750E-14, 2.578125000341414008, -1.570758158831808249 ) ) ;
#179966 = CARTESIAN_POINT ( 'NONE',  ( 5.414685466650038137, -1.281359335986744341, -1.556910257834144051 ) ) ;
#179967 = CARTESIAN_POINT ( 'NONE',  ( -8.631737353394710155, 13.22211067893587533, 1.040834085586084257E-14 ) ) ;
#179968 = CARTESIAN_POINT ( 'NONE',  ( 9.094822116668764167, 9.505047312402055582, 0.7998128361456462443 ) ) ;
#179969 = CARTESIAN_POINT ( 'NONE',  ( 2.679728069698092074, -0.4610709815545778190, -0.1059060488087510826 ) ) ;
#179971 =( LENGTH_UNIT ( ) NAMED_UNIT ( * ) SI_UNIT ( .MILLI., .METRE. ) );
#179970 = CARTESIAN_POINT ( 'NONE',  ( 3.088313589057069208, -1.798746773638896457, -0.3115406389907551810 ) ) ;
#179972 = DIRECTION ( 'NONE',  ( -0.000000000000000000, 1.000000000000000000, -0.000000000000000000 ) ) ;
#179973 = ORIENTED_EDGE ( 'NONE', *, *, #87967, .F. ) ;
#179974 = CARTESIAN_POINT ( 'NONE',  ( -5.492461626867567226, 6.540864998501174199, 1.082531754730549078 ) ) ;
#179975 = CARTESIAN_POINT ( 'NONE',  ( 1.642778471875001811, -3.580208332855376430, 2.845375778867859751 ) ) ;
#179976 = CARTESIAN_POINT ( 'NONE',  ( -7.974166903131914452, 12.45494515362926435, -0.7998128361456281477 ) ) ;
#179977 = CARTESIAN_POINT ( 'NONE',  ( 6.445964431295706731, -1.320945465521980555, -1.527872228271543342 ) ) ;
#179978 = CARTESIAN_POINT ( 'NONE',  ( 1.225412164737609055, 1.871785320780447792, 0.9964087003688710809 ) ) ;
#179979 = ORIENTED_EDGE ( 'NONE', *, *, #28302, .T. ) ;
#179980 = CARTESIAN_POINT ( 'NONE',  ( -5.960744811863571968, 6.983232364376142698, 1.199719254218452935 ) ) ;
#179981 = CARTESIAN_POINT ( 'NONE',  ( 5.190073875932979419, 4.949507698210251938, 0.7998128361456341429 ) ) ;
#179982 = CARTESIAN_POINT ( 'NONE',  ( 6.737187473210400235, -1.842164534206979676, 0.9240717516781959961 ) ) ;
#179983 = CARTESIAN_POINT ( 'NONE',  ( 6.557263107265463020, -1.238491779027944162, 1.591905563659588907 ) ) ;
#179984 = ORIENTED_EDGE ( 'NONE', *, *, #161695, .T. ) ;
#179985 = VERTEX_POINT ( 'NONE', #208093 ) ;
#179986 = CARTESIAN_POINT ( 'NONE',  ( -9.297140650669053485, 11.86975006391249643, 1.599625672291281386 ) ) ;
#179987 = CARTESIAN_POINT ( 'NONE',  ( 6.994027139803230320, 9.253060644560830994, -1.599625672291267398 ) ) ;
#179990 = ORIENTED_EDGE ( 'NONE', *, *, #30406, .F. ) ;
#179989 = CARTESIAN_POINT ( 'NONE',  ( 7.960204194457795477E-16, -0.4330127018922214077, 6.500000000000000000 ) ) ;
#179988 = CARTESIAN_POINT ( 'NONE',  ( -5.818384198920079520, 6.817144982608731141, 1.199719254218452935 ) ) ;
#179991 = CARTESIAN_POINT ( 'NONE',  ( 6.509182584184366682, 6.829728176725765820, 0.5468608461018635847 ) ) ;
#179992 = CARTESIAN_POINT ( 'NONE',  ( 5.729842239849809893, -1.821464125411855761, -0.8645900286049985617 ) ) ;
#179993 = CARTESIAN_POINT ( 'NONE',  ( 4.927609005033061429, 0.9437523325564222132, -1.580719041474540010 ) ) ;
#179994 = CARTESIAN_POINT ( 'NONE',  ( -0.02319159430947542733, 0.7471999394491578572, -1.895068635927643630 ) ) ;
#179995 = CARTESIAN_POINT ( 'NONE',  ( 2.948224681477436881, 0.8299853515197992415, -2.153443412361542020 ) ) ;
#179996 = CARTESIAN_POINT ( 'NONE',  ( 4.830447868218803897, 8.857549289555754157, -0.7998128361456481317 ) ) ;
#179997 = CARTESIAN_POINT ( 'NONE',  ( 5.958325562381369345, 0.8699925256120243366, 1.978967057501494820 ) ) ;
#179998 = CARTESIAN_POINT ( 'NONE',  ( 7.579171565239241737, 8.801120566655981747, 1.199719254218462483 ) ) ;
#179999 = CARTESIAN_POINT ( 'NONE',  ( 1.171315778946733888, 1.157996810922466313, 1.558895349155087873 ) ) ;
#180000 = CARTESIAN_POINT ( 'NONE',  ( -3.598799709423620374, 6.286017863381107240, 1.199719254218464037 ) ) ;
#180001 = VERTEX_POINT ( 'NONE', #210222 ) ;
#180002 = STYLED_ITEM ( 'NONE', ( #139110 ), #162075 ) ;
#180003 = CARTESIAN_POINT ( 'NONE',  ( 4.446792056507931079, 1.496784378905056334, 1.744297655265887537 ) ) ;
#180004 = CARTESIAN_POINT ( 'NONE',  ( 3.469446951953614189E-15, 6.400000000000023448, 1.214306433183764966E-14 ) ) ;
#180005 = CARTESIAN_POINT ( 'NONE',  ( -3.817502770699643388, 6.611447778194983194, 1.199719254218452935 ) ) ;
#180006 = CARTESIAN_POINT ( 'NONE',  ( 4.258574955689950592, -1.386304660245713860, 1.256184814050688603 ) ) ;
#180009 = CARTESIAN_POINT ( 'NONE',  ( -6.936931872047518155, 8.122117267924091166, 1.199719254218452047 ) ) ;
#180008 = CARTESIAN_POINT ( 'NONE',  ( -0.7500000000000006661, -0.1104166659838465292, -1.299038105676652011 ) ) ;
#180007 = CARTESIAN_POINT ( 'NONE',  ( 1.230557176020010912, 1.282188879665364656, -1.419081615486268433 ) ) ;
#180010 = CARTESIAN_POINT ( 'NONE',  ( 2.262606014870732096, 0.9450075053254001212, 1.994452002680577429 ) ) ;
#180011 = ADVANCED_FACE ( 'NONE', ( #211291 ), #62916, .T. ) ;
#180012 = CARTESIAN_POINT ( 'NONE',  ( 0.1405533004714107914, -0.003749010675423137661, -2.279853246149381896 ) ) ;
#180013 = CARTESIAN_POINT ( 'NONE',  ( 3.192055101013606233, 5.811482486902795230, -1.199719254218446718 ) ) ;
#180014 = CARTESIAN_POINT ( 'NONE',  ( 5.492461626867537916, 9.421972641405202964, -0.7216878364870458196 ) ) ;
#180015 = CARTESIAN_POINT ( 'NONE',  ( -2.774614992291035698, 6.388801257648172971, 1.040834085586084257E-14 ) ) ;
#180016 = CARTESIAN_POINT ( 'NONE',  ( -6.522881301506166629, 9.663759714182251770, 1.082531754730549967 ) ) ;
#180017 = CARTESIAN_POINT ( 'NONE',  ( 1.704304553464238703, -0.7057161435466070554, -1.840894384558971808 ) ) ;
#180018 = CARTESIAN_POINT ( 'NONE',  ( 0.6577796130948220243, -1.951556776833747620, -1.231164357708439017 ) ) ;
#180019 = CARTESIAN_POINT ( 'NONE',  ( 1.855835942623608181, -0.6640040153468586004, 1.846199708051485811 ) ) ;
#180020 = CARTESIAN_POINT ( 'NONE',  ( 5.278211761479340680, -1.098870959053561469, -1.745292714083917174 ) ) ;
#180021 = CARTESIAN_POINT ( 'NONE',  ( 3.877268743828266029, 6.506935386899531437, 1.082531754730558626 ) ) ;
#180022 = CARTESIAN_POINT ( 'NONE',  ( 5.529746549527311039, 7.544733289238903851, -1.599625672291281386 ) ) ;
#180023 = ORIENTED_EDGE ( 'NONE', *, *, #100231, .T. ) ;
#180024 = CARTESIAN_POINT ( 'NONE',  ( -9.001723924469462901, 12.58942944760136484, -1.199719254218446718 ) ) ;
#180025 = CARTESIAN_POINT ( 'NONE',  ( -4.940331642637891818, 4.884205503302849749, 0.5202640082965306334 ) ) ;
#180026 = CARTESIAN_POINT ( 'NONE',  ( 3.009546912109283934, 6.454962464195385330, 0.000000000000000000 ) ) ;
#180027 = CARTESIAN_POINT ( 'NONE',  ( 1.411231479646192222, -1.713112901771263630, 1.333658509791965097 ) ) ;
#180029 = DIRECTION ( 'NONE',  ( 0.000000000000000000, 1.000000000000000000, 0.000000000000000000 ) ) ;
#180028 = PLANE ( 'NONE',  #118601 ) ;
#180030 = ADVANCED_FACE ( 'NONE', ( #59720 ), #36734, .T. ) ;
#180031 = CARTESIAN_POINT ( 'NONE',  ( -3.475000000000000533, -1.779166666666666785, -2.006292185433948827 ) ) ;
#180032 = CARTESIAN_POINT ( 'NONE',  ( 1.844777716111935861, -1.582881869529973562, 0.9963996312925410548 ) ) ;
#180033 = CARTESIAN_POINT ( 'NONE',  ( 5.501312752317830679, 1.763641270444433307, 1.249554385337700024 ) ) ;
#180034 = CARTESIAN_POINT ( 'NONE',  ( -5.460715490240072079, 6.444878312648672392, 1.304320558087665782 ) ) ;
#180035 = CARTESIAN_POINT ( 'NONE',  ( 0.07735805125223117751, 5.721077998510399887, -2.682987299736539377 ) ) ;
#180036 = CARTESIAN_POINT ( 'NONE',  ( -0.6823417656250003738, -0.03229166632524871350, -1.181850606188749264 ) ) ;
#180037 = CARTESIAN_POINT ( 'NONE',  ( 1.910667195161031007, -0.5113573046386342691, -1.842555643073694238 ) ) ;
#180038 = STYLED_ITEM ( 'NONE', ( #13178 ), #171430 ) ;
#180039 = CARTESIAN_POINT ( 'NONE',  ( 3.537761123354207893, 0.7962651652904990662, -1.580685414113996545 ) ) ;
#180040 = CARTESIAN_POINT ( 'NONE',  ( 0.9438406676962156627, -1.213610516764839664, -1.477797202995428938 ) ) ;
#180042 = CARTESIAN_POINT ( 'NONE',  ( 5.677321882007140275, 1.453744714618950606, 1.247594701790984306 ) ) ;
#180041 = CARTESIAN_POINT ( 'NONE',  ( 7.834948825496934610, -6.307829212974246147, 7.720982897393585453 ) ) ;
#180043 = CARTESIAN_POINT ( 'NONE',  ( 6.777801591175982132, -1.910752814866881089, 0.4773036857264860156 ) ) ;
#180044 = CARTESIAN_POINT ( 'NONE',  ( 1.499999999999990896, 5.025000000000022560, 1.214306433183764966E-14 ) ) ;
#180045 = CARTESIAN_POINT ( 'NONE',  ( 0.6859744409541921328, 2.042103856186634925, -0.5713114342573709648 ) ) ;
#180046 = FACE_OUTER_BOUND ( 'NONE', #47351, .T. ) ;
#180047 = CARTESIAN_POINT ( 'NONE',  ( 4.557402362779487959, 0.4096945884842878582, -1.825068887194372991 ) ) ;
#180049 = ORIENTED_EDGE ( 'NONE', *, *, #168717, .T. ) ;
#180048 = CARTESIAN_POINT ( 'NONE',  ( 0.8205984872286451459, 1.685833220154912881, 0.7012733028506010768 ) ) ;
#180051 = CARTESIAN_POINT ( 'NONE',  ( 4.759808938472720463, 8.174556087920027636, -0.7576060450402433144 ) ) ;
#180050 = CARTESIAN_POINT ( 'NONE',  ( 4.406973378220558679, 1.706932345810768359, -1.398813476408675260 ) ) ;
#180052 = CARTESIAN_POINT ( 'NONE',  ( -0.6823417656250246877, -0.9489583329919115684, 1.181850606188755259 ) ) ;
#180053 = CARTESIAN_POINT ( 'NONE',  ( 1.522013433763437895, 2.032506561856410876, -0.3506121680386958261 ) ) ;
#180054 = CARTESIAN_POINT ( 'NONE',  ( 7.298366762858032430, 7.409182732956175244, 1.040834085586084257E-14 ) ) ;
#180055 = CARTESIAN_POINT ( 'NONE',  ( -8.688077508258798431, 9.030511935923748013, -0.7998128361456291469 ) ) ;
#180056 = CARTESIAN_POINT ( 'NONE',  ( -2.923191517300036679, 6.424490846909734820, 0.000000000000000000 ) ) ;
#180057 = CARTESIAN_POINT ( 'NONE',  ( -3.424509409375499747, -0.02075852630553524925, -0.4189850677842354432 ) ) ;
#180058 = ADVANCED_FACE ( 'NONE', ( #200357 ), #8023, .T. ) ;
#180059 = CARTESIAN_POINT ( 'NONE',  ( 0.1753634416057497647, 4.084635187426246539, -2.698744815386323381 ) ) ;
#180060 = ORIENTED_EDGE ( 'NONE', *, *, #55029, .F. ) ;
#180061 = CARTESIAN_POINT ( 'NONE',  ( 3.736834853878097107, -1.994506513866915576, -0.5549897870569252545 ) ) ;
#180062 = CARTESIAN_POINT ( 'NONE',  ( -0.6823417656250246877, -0.6364583329919113464, 1.181850606188755259 ) ) ;
#180063 = CARTESIAN_POINT ( 'NONE',  ( 2.038557401052975671, 2.137775048120754029, 0.3193135401893046899 ) ) ;
#180064 = CARTESIAN_POINT ( 'NONE',  ( -5.779986827147332029, 7.257483166437310729, -1.191988747605486010 ) ) ;
#180065 = CARTESIAN_POINT ( 'NONE',  ( 2.086587641237521495, -1.240871089896943280, 1.593450946908819832 ) ) ;
#180066 = DIRECTION ( 'NONE',  ( 0.000000000000000000, 0.000000000000000000, 1.000000000000000000 ) ) ;
#180067 = ORIENTED_EDGE ( 'NONE', *, *, #173168, .T. ) ;
#180069 = CARTESIAN_POINT ( 'NONE',  ( 7.619319141200063150, 9.912291636198670375, 1.443375672974076540 ) ) ;
#180068 = CARTESIAN_POINT ( 'NONE',  ( 3.475000000000000533, -3.325000000000001510, 0.000000000000000000 ) ) ;
#180070 = CARTESIAN_POINT ( 'NONE',  ( 0.03257979115088038835, 14.52968454062227188, 11.98509113246684699 ) ) ;
#180071 = CARTESIAN_POINT ( 'NONE',  ( -5.167065940139584868, 6.161236697318522637, 1.082531754730549078 ) ) ;
#180072 = CARTESIAN_POINT ( 'NONE',  ( -0.01248194115436446205, -0.5331630387654020531, 1.944732228473695868 ) ) ;
#180073 = CARTESIAN_POINT ( 'NONE',  ( 4.950807510372833065, -1.851323926424643274, -1.172527737679923465 ) ) ;
#180074 = CARTESIAN_POINT ( 'NONE',  ( 1.499999999999989120, 4.827083334016149863, -0.8660254037844323793 ) ) ;
#180075 = CARTESIAN_POINT ( 'NONE',  ( 4.693567934957057375, 1.782326746607498791, -0.6936623114904352239 ) ) ;
#180076 = CARTESIAN_POINT ( 'NONE',  ( -5.251085567194491155, 5.020688004682002159, -0.7998128361456221525 ) ) ;
#180077 = CARTESIAN_POINT ( 'NONE',  ( 5.572037945092146671, 8.484166121707415797, -1.082531754730543971 ) ) ;
#180079 = CARTESIAN_POINT ( 'NONE',  ( 2.636342400811112707, 0.6820146075395253638, 1.897692325672148073 ) ) ;
#180078 = CARTESIAN_POINT ( 'NONE',  ( -11.78331023100045627, 9.799999999999998934, -1.800000000000001155 ) ) ;
#180080 = CARTESIAN_POINT ( 'NONE',  ( -1.364683531250010295, 12.19270833367473195, 0.7879004041258445001 ) ) ;
#180082 = CARTESIAN_POINT ( 'NONE',  ( -3.142457743317409680, 6.888227477170756785, 0.7998128361456352531 ) ) ;
#180081 = CARTESIAN_POINT ( 'NONE',  ( 0.7148891103036036920, 2.120809155261915713, 0.8706237914077943341 ) ) ;
#180083 = CARTESIAN_POINT ( 'NONE',  ( 4.700069144524660736, -1.724479993061514449, -0.04023236952926077803 ) ) ;
#180084 = CARTESIAN_POINT ( 'NONE',  ( -0.1394461523060987751, 0.6550469493228279205, -2.357635998629922902 ) ) ;
#180085 = CARTESIAN_POINT ( 'NONE',  ( 4.521807925357579805, 5.234196320127330715, -1.199719254218452047 ) ) ;
#180086 = DIRECTION ( 'NONE',  ( 0.000000000000000000, 1.000000000000000000, 0.000000000000000000 ) ) ;
#180087 = ORIENTED_EDGE ( 'NONE', *, *, #23742, .T. ) ;
#180088 = CARTESIAN_POINT ( 'NONE',  ( 0.07680821025394038437, 7.629137130509076492, -2.410791881123967695 ) ) ;
#180089 = ORIENTED_EDGE ( 'NONE', *, *, #201840, .T. ) ;
#180090 = CARTESIAN_POINT ( 'NONE',  ( 5.496671973222438723, -1.768653292081886708, -0.3907654940887676509 ) ) ;
#180091 = ORIENTED_EDGE ( 'NONE', *, *, #30664, .F. ) ;
#180092 = CARTESIAN_POINT ( 'NONE',  ( 7.730120138085914583, 12.17022392774227768, 0.7998128361456462443 ) ) ;
#180093 = CARTESIAN_POINT ( 'NONE',  ( 6.391743074199808916, 6.421731439513382433, -0.7998128361456481317 ) ) ;
#180094 = DIRECTION ( 'NONE',  ( -0.000000000000000000, -1.000000000000000000, -0.000000000000000000 ) ) ;
#180095 = CARTESIAN_POINT ( 'NONE',  ( 6.463521484642490655, -1.459484751789320134, -1.072804587801470921 ) ) ;
#180096 = CARTESIAN_POINT ( 'NONE',  ( 6.821160681006788629, 8.091013894996997635, 1.082531754730549967 ) ) ;
#180097 = CARTESIAN_POINT ( 'NONE',  ( -11.84668729035104384, 10.09481419982587802, -1.400000000000001688 ) ) ;
#180098 = CARTESIAN_POINT ( 'NONE',  ( 2.695491272475036837, -0.6865090956127660737, 2.081212476921667776 ) ) ;
#180099 = ORIENTED_EDGE ( 'NONE', *, *, #140054, .F. ) ;
#180101 = CARTESIAN_POINT ( 'NONE',  ( 9.348510611822643313, 10.86534945433664134, 1.199719254218453823 ) ) ;
#180100 = CARTESIAN_POINT ( 'NONE',  ( 6.760206150924522817, -1.860609546209352372, 0.04724569877399482920 ) ) ;
#180102 = CARTESIAN_POINT ( 'NONE',  ( 3.585460515032745210, -0.5529844701629010872, 1.834067302312661241 ) ) ;
#180103 = DIRECTION ( 'NONE',  ( 0.000000000000000000, 0.000000000000000000, 1.000000000000000000 ) ) ;
#180105 = CIRCLE ( 'NONE', #197401, 12.00000000000000178 ) ;
#180104 =( BOUNDED_SURFACE ( )  B_SPLINE_SURFACE ( 3, 3, ( 
 ( #153797, #204647, #58429, #8597, #75742, #23778, #72527, #38979, #22695, #141854, #154867, #139704, #74679, #24846, #123525, #206796, #125643, #140782, #71449, #88809, #6449, #138622, #56297, #190543, #122457, #188416, #40052, #106162, #89883, #155935, #193745, #209981, #14977, #109385, #161263, #142916, #113645, #76795, #43266, #159124, #145047, #146103, #143989, #110445, #175391, #162332, #46452, #81073, #179650, #195895, #208916, #211049, #30192, #26977, #12850, #94152, #112574, #93082, #60550, #61622, #31270, #45392, #97345, #126708, #192670, #63751, #213184, #163402, #147159, #44323, #78924, #176447, #129910, #96282, #178584, #62675, #212114, #64814, #128834, #191604, #10725, #28059, #160192, #11792, #194816, #77866, #127791, #111508, #13917, #79998, #177514, #29127, #95214, #47532, #48590, #100522, #82127, #52838, #16044, #196950, #98393, #84271, #85340, #83190, #49637, #114706, #101590, #200138, #168723, #118974, #135183, #148221, #150357, #183901, #180701, #166596, #33382, #51791, #32325, #214222, #853, #184952, #133059, #36579, #65851, #132000, #2995, #152479, #102665, #20326, #198009, #18185, #115761, #69063, #149273, #86412, #181751, #201198, #4059, #130960, #99463, #164457, #35512, #19258, #34447, #165520, #167658, #50706, #17113, #151422, #66918, #199060, #116830, #182832, #1927, #67986, #134129, #117908, #74436, #70129, #39800, #186023, #5121, #203329, #56049, #188167, #202263, #187098, #25663, #58177, #21377, #136242, #170858, #122205, #105907, #124337, #106988, #72268, #88560, #53913, #22448, #120049, #155685, #154620, #139446, #87485, #173013, #71197, #24594, #37660, #6199, #90701, #40883, #140536, #171932, #104813, #137313, #54982, #206548, #38732, #23526, #156763, #138376, #121135, #8351, #91772, #190295, #205481, #41953, #108065, #153551, #204394, #103737, #89633, #7267, #169788, #157829, #174091, #73344, #57113, #123282, #189243, #97103, #59233, #26735, #47287, #75495, #78681, #93907, #194568, #129665, #111264, #159947, #94966, #113399, #46214, #161014, #193511, #109136, #28883, #13680, #79751, #143744, #12609, #92837, #9425, #179407, #175149, #192425, #158881, #141607, #144808, #207615, #11551, #178344, #210814, #145867, #77621, #10477, #61382, #76552, #209738, #208672, #211874, #60303, #142662, #126461, #63513, #125391, #44079, #62439, #127539, #112330, #128602, #110198, #191357, #176208, #27809, #29953, #195652, #45152, #177267, #96038, #162090, #31027, #43022, #180459, #32076, #98164, #116570, #101321, #197755, #133872, #67721, #164211, #80831, #114459, #81884, #16859, #34187, #99215, #167403, #199879, #1665, #33135, #17918, #85075, #183640, #165264, #51522, #49394, #35246, #117647, #18993, #15798, #212938, #118705, #147969, #213981, #151160, #82940, #48348, #2729, #166328, #68802, #132801, #100261, #65601, #134922, #131750, #115513, #149013, #84004, #589, #200928, #52576, #184693, #66655, #150094, #36313, #163155, #198804, #14739, #181506, #146920, #64575, #130717, #50452, #196708, #182564, #169527, #185757, #106720, #38466, #201987, #172747, #105627, #6997, #72001, #39529, #4852, #56849, #123021, #70931, #153275, #188972, #57911, #40616, #171656, #24322, #8086, #119777, #54710, #135971, #87211, #186834, #3787, #190040, #73075, #20057, #102392, #53644, #121932, #168459, #152218, #37390, #140267 ),
 ( #138112, #103465, #187899, #90428, #156497, #22172, #23253, #21107, #86147, #124076, #137040, #203067, #120861, #69862, #89366, #104542, #170587, #74175, #155414, #206287, #88287, #154351, #5929, #204123, #55775, #139176, #205207, #92584, #58982, #108871, #178079, #173828, #158626, #44895, #175950, #144550, #94711, #26474, #25405, #10223, #42764, #177006, #29697, #43824, #208413, #76297, #142405, #128349, #109941, #125138, #191095, #174894, #209474, #194316, #60047, #12348, #160753, #126202, #91507, #77364, #145617, #79498, #13423, #157568, #192164, #193248, #107803, #95779, #27546, #111001, #28623, #93641, #159684, #11285, #211613, #9161, #143478, #207362, #161835, #141347, #75237, #61116, #127276, #210557, #78428, #62193, #45957, #112078, #63249, #129410, #41692, #199626, #212680, #148769, #33942, #179145, #165011, #97905, #50204, #47023, #146666, #65353, #117396, #197504, #101070, #130465, #196455, #67478, #2479, #183393, #167157, #48098, #16606, #114210, #133624, #147712, #34998, #64321, #51272, #150917, #18744, #180208, #30768, #100017, #83755, #98960, #31830, #166081, #115263, #96848, #17669, #149847, #163966, #162895, #15542, #66411, #1416, #68555, #81627, #84829, #195393, #82687, #14478, #213730, #131500, #181256, #338, #113138, #49147, #80567, #32883, #132556, #198555, #116322, #182313, #120614, #188730, #171415, #136796, #153035, #52336, #20867, #200685, #5675, #86966, #203889, #151976, #23003, #69620, #89121, #134682, #4609, #155175, #105376, #138937, #186591, #169281, #135730, #201752, #204958, #37140, #21925, #39281, #55533, #88034, #6759, #122770, #137869, #3550, #118464, #90188, #19815, #103221, #53393, #184450, #71753, #36068, #70683, #72834, #154106, #56606, #202821, #119530, #38219, #185516, #104292, #54470, #40368, #170340, #121688, #187655, #106470, #102150, #172497, #24083, #156251, #7829, #168216, #85902, #57673, #193780, #74988, #212150, #64848, #78963, #29161, #61659, #45427, #163436, #145085, #91257, #157317, #8908, #30231, #15016, #111543, #47569, #195931, #141096, #206039, #25156, #210017, #211088, #162371, #12886, #81105, #113680, #129944, #161301, #146137, #213218, #97379, #62711, #179684, #177552, #147193, #31304, #130994, #127827, #123831, #32363, #95252, #128872, #196984, #194855, #173586, #48623, #80034, #114738, #46487, #13951, #112610, #180736, #98427, #178621, #96316, #164492, #73921, #140014, #63786, #189793, #41444, #107552, #182866, #49673, #888, #100556, #132034, #103774, #201233, #148254, #16078, #115798, #35547, #82161, #65886, #33420, #53948, #214255, #85375, #166627, #52874, #136277, #117942, #18219, #101625, #120087, #119010, #167692, #200170, #181786, #19293, #20362, #86446, #150390, #99498, #151457, #152511, #4096, #1959, #3029, #165555, #198044, #186062, #17148, #199092, #83224, #149307, #69097, #66955, #84305, #184988, #135221, #70166, #68022, #133094, #134161, #50738, #51824, #116864, #202297, #34482, #183935, #36614, #37698, #102701, #168758, #173045, #89668, #58214, #8385, #154652, #153587, #72306, #170892, #90735, #157867, #171969, #122243, #6234, #138411, #41991, #23560, #187136, #38765, #104846, #123312, #108099, #204432, #140572, #74467, #22484, #87522, #121167, #88595, #155719, #40915, #105945, #174128, #206585, #124372, #39838, #24628, #91809, #190330, #7304, #25701 ),
 ( #55018, #9460, #156798, #75532, #139486, #107021, #56085, #141643, #207652, #188201, #73380, #59273, #125429, #191394, #43059, #169826, #21412, #205514, #57146, #203366, #189276, #5157, #71233, #137348, #79788, #26772, #109172, #142701, #128640, #196746, #158919, #126498, #146957, #175185, #178379, #193546, #145902, #14776, #210851, #45188, #194605, #212972, #211911, #46249, #78719, #143780, #112367, #92873, #97139, #176244, #29988, #96074, #95005, #111303, #127578, #64613, #10515, #144845, #60338, #31064, #208710, #76590, #192462, #62477, #63548, #61415, #27846, #44115, #129704, #162127, #130752, #163193, #113436, #110236, #13715, #195686, #93944, #47323, #11586, #179443, #159984, #77658, #177306, #80867, #28920, #209775, #161051, #12647, #134963, #69905, #184730, #20100, #115550, #84049, #181546, #200971, #631, #102433, #65641, #118747, #3831, #86188, #131790, #98199, #167444, #151201, #166370, #197795, #101365, #182608, #164247, #19037, #85115, #214019, #15835, #33174, #133914, #2772, #136015, #99255, #52619, #48387, #17962, #81921, #49430, #165303, #34231, #150137, #180497, #16898, #114500, #36356, #82979, #32114, #149052, #67763, #66696, #132842, #100304, #198846, #1709, #50493, #168501, #116614, #199920, #51567, #152257, #148008, #117692, #183684, #35290, #68843, #40661, #186876, #185800, #104586, #203109, #123065, #190083, #204164, #154394, #38508, #170631, #74217, #55819, #4895, #70973, #137083, #155458, #140312, #22217, #172791, #106762, #187940, #121976, #5972, #25446, #119820, #171699, #153320, #124120, #87256, #53688, #169569, #7041, #156541, #72043, #120903, #37432, #24363, #56890, #91553, #41735, #206330, #54754, #73117, #90475, #103510, #23298, #88330, #189019, #21150, #138156, #39570, #107844, #105672, #173873, #89408, #139218, #57955, #9206, #157610, #75278, #205248, #8131, #202028, #79542, #93687, #195437, #158667, #211656, #96890, #113183, #10265, #191140, #46001, #29738, #44936, #76340, #194358, #61159, #42806, #112120, #178123, #92625, #108914, #208455, #12392, #95820, #14520, #60087, #145660, #141393, #111044, #174936, #142447, #126247, #127321, #177051, #59022, #43869, #162939, #129454, #192207, #26517, #78471, #161879, #193291, #47066, #13466, #143523, #159729, #125178, #27589, #207403, #144590, #11328, #210604, #109985, #63294, #175995, #179187, #77406, #209519, #30810, #28668, #94753, #160801, #62233, #128391, #81667, #84864, #197541, #182350, #199661, #149885, #33979, #35031, #68589, #116360, #184483, #118501, #52372, #212723, #115305, #17703, #146707, #134714, #147753, #1450, #83790, #31871, #165053, #2516, #82729, #200721, #15580, #213771, #167191, #102185, #36100, #168252, #65392, #100054, #131539, #18778, #32922, #80614, #97950, #150952, #64362, #130508, #164004, #196495, #51307, #183430, #198593, #49186, #133660, #375, #48137, #117432, #101105, #181295, #114251, #98998, #166118, #180247, #16645, #148806, #66449, #132591, #50240, #67515, #169317, #153070, #5712, #137904, #152010, #136830, #189829, #7868, #185552, #135765, #105414, #40404, #154144, #73956, #56641, #21963, #38254, #3582, #120648, #85938, #171452, #186627, #89157, #37181, #122805, #20901, #188764, #19851, #104328, #106506, #204997, #24117, #71789, #54504, #86997, #4647, #90220, #202856, #121725, #138974, #155210, #187690, #172533 ),
 ( #23041, #170376, #156284, #140048, #72868, #88071, #6791, #206073, #57707, #203923, #123864, #55571, #41478, #107588, #69657, #70717, #201788, #53428, #39319, #103256, #119565, #109727, #58769, #29479, #176789, #78215, #143267, #110787, #76085, #128131, #193023, #46811, #8944, #190885, #211404, #25193, #28404, #43609, #144338, #79286, #60902, #175734, #44675, #63034, #210338, #94498, #209257, #124923, #160536, #177867, #95570, #93429, #12142, #42551, #173621, #129201, #108654, #142186, #174682, #91297, #61977, #157355, #27327, #75024, #59834, #194094, #125987, #26255, #11067, #92372, #159468, #158409, #161620, #10009, #208201, #191944, #13213, #141136, #77146, #45744, #127061, #111862, #145404, #195178, #207146, #15328, #113998, #33725, #100856, #115049, #65143, #97691, #81418, #199408, #181047, #130251, #196242, #47885, #66194, #51053, #147499, #83538, #17454, #179993, #30552, #64109, #31616, #32663, #198345, #48930, #117176, #149620, #165868, #197290, #182094, #34782, #133403, #98742, #1202, #213520, #183178, #67264, #166941, #163749, #162685, #68338, #131299, #164800, #18534, #16392, #212465, #84611, #116103, #150700, #82471, #49985, #148561, #2262, #134470, #127, #132339, #200473, #112925, #178938, #99803, #96631, #14259, #80350, #146450, #85676, #36919, #136581, #167998, #139791, #22783, #184230, #52120, #151764, #53181, #187439, #40138, #54254, #4393, #103002, #20655, #138716, #120391, #69403, #135510, #201533, #5459, #204733, #86745, #88900, #171193, #119309, #35854, #3333, #185295, #186366, #137649, #202601, #56383, #154954, #105153, #38001, #121469, #188507, #72617, #104073, #6539, #152815, #122546, #106251, #172275, #169058, #101932, #7609, #70464, #170120, #23862, #21706, #87818, #89969, #55318, #156021, #153890, #203669, #71539, #73693, #118248, #39067, #19604, #11881, #161357, #160279, #60639, #77957, #111597, #8686, #158163, #24933, #190627, #75830, #107327, #79019, #176533, #123611, #205818, #91037, #10809, #57450, #41222, #74768, #29218, #189574, #126801, #141937, #28145, #177606, #93173, #207950, #76884, #95308, #94240, #143004, #175479, #157097, #209002, #210074, #61713, #125730, #192757, #140871, #173352, #12940, #206883, #174423, #58515, #124670, #44414, #42287, #59572, #108399, #92108, #110533, #9754, #25999, #43351, #191691, #109471, #27066, #127881, #159208, #144078, #193831, #45481, #62764, #47619, #148303, #64897, #33467, #198092, #129996, #128926, #113731, #194905, #96371, #63838, #213268, #16126, #81156, #83269, #49719, #115847, #15066, #214302, #67004, #165605, #147241, #99542, #179737, #17195, #149357, #938, #212202, #46542, #100601, #195986, #14000, #133141, #131044, #30286, #199141, #65933, #181833, #114786, #82210, #31354, #50785, #116914, #97429, #163483, #182914, #166677, #34530, #132082, #18268, #145136, #162423, #197034, #178671, #48669, #180785, #112663, #211142, #80084, #146187, #32409, #98475, #164540, #157639, #134205, #186911, #173905, #84351, #40691, #187977, #90506, #107879, #73149, #39603, #56924, #25481, #156571, #123097, #7076, #120940, #205286, #57988, #124151, #23332, #189054, #38543, #150440, #2003, #104620, #55854, #22255, #200214, #106794, #54792, #105707, #170668, #122010, #172822, #171735, #88365, #139254, #6009, #155493, #138190, #190112, #204200, #154431, #72079, #41766 ),
 ( #91587, #89441, #24394, #8165, #74249, #68068, #140343, #206361, #146886, #212906, #19770, #4562, #98128, #37093, #185471, #64539, #164179, #135682, #80796, #169233, #130683, #20823, #63474, #15764, #86920, #103171, #70637, #52288, #81849, #196672, #48312, #136748, #180423, #168171, #152988, #201707, #85852, #202775, #54426, #102101, #170292, #104246, #38174, #195614, #150869, #3502, #129628, #120567, #114423, #53350, #69572, #118417, #68508, #2433, #21880, #47251, #36023, #14702, #186544, #163120, #113365, #30992, #151928, #87986, #134635, #32041, #179370, #154062, #119484, #97067, #200640, #184403, #22958, #173533, #58687, #203840, #189742, #122720, #74939, #71708, #171364, #90137, #142107, #7780, #125908, #155130, #6712, #92290, #27239, #208120, #191865, #72788, #41394, #138889, #158334, #172447, #59748, #89073, #76002, #175652, #43526, #204908, #55486, #124835, #108570, #123783, #56561, #190801, #139966, #121640, #42461, #174597, #188683, #187608, #40318, #91208, #26174, #93346, #106424, #9928, #5627, #107505, #39235, #24034, #156204, #205989, #25106, #137821, #73872, #105327, #109649, #57625, #157270, #8860, #141050, #207056, #213436, #196157, #161533, #177778, #77055, #45654, #10981, #30463, #212377, #79198, #209176, #130165, #64017, #110703, #60815, #12058, #96548, #47798, #32579, #78126, #163662, #159382, #129111, #126976, #94412, #144256, #145315, #62942, #143185, #61887, #114956, #147410, #176703, #192935, #162595, #179906, #211318, #65059, #113911, #13119, #29393, #44589, #111771, #28316, #14170, #95487, #80264, #160451, #31529, #210249, #97604, #128050, #195086, #15244, #81331, #131215, #46723, #194005, #112836, #178852, #197203, #146363, #48842, #180957, #93811, #42927, #109037, #175056, #193417, #178250, #60209, #210725, #144713, #26643, #157736, #191262, #158788, #159852, #111172, #176117, #29863, #62351, #78593, #110106, #94873, #162001, #46123, #27717, #128512, #126370, #112240, #194480, #95946, #92744, #75405, #195559, #10385, #76461, #13590, #11455, #125303, #79664, #28790, #145779, #209644, #177173, #142569, #211782, #63420, #208576, #192329, #129572, #47195, #113310, #160926, #25572, #91683, #43988, #77528, #59145, #143649, #61285, #141518, #9333, #207526, #127446, #45061, #12520, #198717, #52490, #14647, #196619, #2641, #30937, #34104, #49310, #98072, #165175, #82853, #97013, #81796, #134836, #167315, #130627, #80741, #50363, #199790, #99126, #18902, #1574, #181418, #197666, #163066, #65518, #146829, #116486, #131663, #100175, #48258, #67635, #114372, #133782, #179316, #115427, #51435, #150004, #183549, #16769, #213895, #180367, #31991, #35156, #64485, #33048, #212848, #15711, #132712, #117555, #84986, #502, #68714, #200839, #151077, #164127, #148929, #182475, #147879, #66570, #166240, #17830, #83913, #101233, #120771, #136957, #156406, #36224, #88195, #69778, #40527, #3702, #184607, #86057, #71914, #72990, #70841, #37304, #102303, #89281, #187814, #7993, #106631, #122929, #135886, #138023, #171568, #168376, #154269, #21025, #39440, #19973, #201905, #202983, #172660, #186751, #24235, #53557, #119690, #205120, #140176, #90337, #74085, #185675, #5843, #103378, #56763, #54624, #206198, #169440, #188886, #118620, #152134, #87122, #153192, #23165, #6913, #22084, #4764, #155329, #38373, #104454, #139093 ),
 ( #170501, #204038, #55687, #121843, #105534, #111992, #75151, #128264, #13339, #29607, #141261, #107716, #176918, #160668, #175867, #207269, #110912, #192074, #173743, #28533, #94625, #9077, #25320, #125053, #143388, #12263, #145531, #191008, #62105, #57826, #27455, #91421, #58900, #42675, #43740, #93553, #189955, #174809, #79414, #45870, #108783, #157482, #209386, #78340, #109853, #177994, #144463, #59959, #76208, #41605, #158536, #123988, #61030, #10133, #127191, #26385, #210467, #92497, #194226, #142318, #208328, #95693, #161748, #126114, #159597, #11195, #77276, #193158, #44808, #96763, #15458, #84742, #48011, #164927, #165996, #199541, #32800, #100981, #34909, #183302, #129330, #31745, #148687, #63164, #51183, #64237, #66327, #256, #197418, #213646, #81545, #167070, #195306, #181175, #162814, #133534, #14391, #46937, #179061, #16519, #17581, #163883, #130381, #113055, #182229, #132472, #18662, #117306, #1332, #80482, #82602, #50119, #30680, #98874, #114128, #198474, #146582, #212599, #147628, #211529, #65272, #196371, #180120, #97819, #83664, #131418, #49060, #115180, #116240, #33853, #99934, #149755, #67393, #54385, #68471, #53311, #106382, #138846, #102065, #52246, #21837, #171320, #70594, #204863, #187567, #152945, #169191, #134598, #37050, #2392, #87945, #103133, #5585, #168130, #39193, #85811, #105284, #150830, #20783, #22915, #121595, #155086, #136709, #185430, #151890, #3464, #6672, #35984, #86878, #23993, #201663, #104205, #89031, #56518, #186502, #40271, #188641, #122678, #200599, #4521, #154019, #118374, #172405, #69534, #71665, #137779, #202734, #120523, #38133, #184362, #19732, #170252, #135641, #72749, #119443, #203797, #55443, #43489, #44550, #42425, #8824, #73829, #60777, #159343, #128014, #12017, #94372, #107466, #109608, #143144, #139925, #59707, #207017, #10940, #156161, #41356, #174560, #78090, #92248, #210211, #25068, #91170, #176666, #111731, #144215, #61847, #157229, #125867, #74900, #28278, #108530, #193967, #173492, #160412, #45615, #177738, #141009, #205952, #209138, #192894, #208080, #58648, #126936, #9887, #57584, #110665, #90096, #124802, #123742, #190761, #175614, #7742, #189703, #26136, #158296, #75963, #191826, #142066, #27201, #93308, #77015, #82346, #113874, #98616, #165742, #49857, #179869, #132212, #63979, #115984, #198221, #181972, #96511, #79157, #199282, #162561, #112799, #33602, #31494, #129073, #99673, #32541, #148437, #213401, #180920, #146324, #17329, #83410, #212339, #80225, #149492, #50924, #1075, #164677, #67140, #133274, #46681, #196121, #62903, #14133, #97569, #145273, #117050, #5, #161497, #29353, #195044, #48804, #95448, #211280, #178811, #13077, #30426, #16261, #163626, #66070, #130133, #131178, #15207, #114921, #47760, #81298, #147375, #65023, #197168, #202470, #187310, #38937, #102871, #186235, #200345, #183047, #138581, #68208, #151635, #51994, #34662, #120259, #166811, #53044, #100732, #69270, #54123, #135384, #118120, #20533, #35725, #168930, #167870, #105020, #19468, #184105, #101801, #171059, #18405, #85544, #37869, #86615, #71405, #21575, #3201, #84481, #201405, #119177, #103947, #22655, #185163, #36787, #152683, #204604, #4265, #70335, #136452, #169989, #87681, #153754, #121334, #5325, #137517, #203534, #55187, #150571, #134340, #88766, #154823, #6408, #72480 ),
 ( #56255, #2133, #106120, #93039, #191560, #160149, #44279, #126662, #139661, #75698, #175351, #172143, #91976, #24800, #43224, #188371, #73560, #206753, #110400, #124540, #28010, #57318, #123483, #208872, #143942, #176404, #94108, #189446, #158034, #41088, #60502, #74635, #11746, #205682, #192627, #77821, #209938, #107196, #23735, #26931, #10678, #25866, #173221, #159081, #42155, #89841, #76749, #142870, #90902, #155890, #156965, #207815, #122412, #40009, #8556, #7478, #140742, #9621, #58384, #190497, #108270, #174291, #141812, #59443, #125600, #109341, #49587, #12804, #177470, #147111, #82078, #195845, #115711, #98344, #63705, #79950, #193701, #162284, #127744, #213137, #13872, #130909, #78877, #164409, #211005, #15993, #61576, #146053, #148171, #32278, #65800, #47486, #96234, #62628, #128788, #131947, #161217, #212067, #149220, #112522, #14928, #214173, #181701, #97294, #165467, #99413, #33331, #45345, #129862, #64767, #111464, #17063, #194769, #196901, #48540, #197958, #83142, #29084, #95168, #46406, #163353, #178535, #145000, #113596, #30145, #179599, #31220, #81023, #114659, #180653, #50653, #119996, #103687, #118923, #84218, #53863, #135129, #116779, #185973, #37606, #166541, #182776, #67932, #86357, #169736, #88508, #134077, #5070, #795, #184903, #34394, #150306, #200085, #201146, #36527, #133008, #117857, #170808, #203282, #18129, #100466, #152428, #21325, #52784, #54929, #87432, #2940, #19206, #199008, #101539, #66863, #4007, #167608, #70077, #1872, #153500, #51734, #71145, #183849, #85285, #137262, #121081, #187048, #102614, #35461, #151371, #69012, #38680, #168669, #20273, #136191, #202209, #104759, #22399, #142614, #190247, #44031, #192376, #126413, #72216, #189194, #91727, #6146, #208622, #7217, #9376, #157778, #140487, #156711, #172963, #110149, #138323, #124288, #105852, #76503, #39747, #204339, #122148, #108016, #109085, #106940, #73291, #55997, #125344, #75447, #176162, #60256, #158834, #171879, #174042, #207568, #188116, #41905, #57065, #141560, #23476, #89583, #24542, #27762, #8302, #154570, #155632, #139394, #205427, #25615, #92789, #40831, #191307, #59189, #123229, #90650, #74386, #206498, #58129, #42975, #175100, #10431, #26687, #149788, #178298, #166029, #18693, #117341, #29905, #199573, #128555, #183338, #51217, #34943, #160970, #143697, #52281, #12560, #177220, #101015, #95990, #193463, #167106, #97056, #1362, #63463, #30981, #210770, #84775, #150862, #62390, #144759, #2424, #118408, #68501, #17614, #134629, #200633, #111217, #46168, #127492, #78634, #162043, #209689, #184394, #67424, #11503, #93858, #45107, #113354, #159896, #61333, #28833, #77574, #94921, #83700, #13633, #133567, #194520, #195604, #79706, #179359, #112282, #145821, #211826, #129617, #47239, #55476, #40307, #106415, #170283, #39226, #53341, #36014, #205980, #135673, #4554, #119475, #102093, #187599, #19761, #120556, #168163, #136739, #121630, #202765, #185463, #87977, #103162, #21871, #20815, #172438, #86911, #37083, #169223, #24025, #85843, #152979, #105317, #154051, #138879, #89063, #70628, #151920, #54415, #186535, #171355, #90127, #38164, #104237, #5618, #57615, #71700, #137812, #203831, #22949, #156194, #3493, #155121, #69563, #6703, #72780, #204897, #56550, #201698, #122711, #123773, #7770, #188674, #73861, #139955, #210238 ) ),
 .UNSPECIFIED., .T., .F., .T. ) 
 B_SPLINE_SURFACE_WITH_KNOTS ( ( 4, 3, 4 ),
 ( 4, 1, 1, 1, 1, 1, 1, 1, 1, 1, 1, 1, 1, 1, 1, 1, 1, 1, 1, 1, 1, 1, 1, 1, 1, 1, 1, 1, 1, 1, 1, 1, 1, 1, 1, 1, 1, 1, 1, 1, 1, 1, 1, 1, 1, 1, 1, 1, 1, 1, 1, 1, 1, 1, 1, 1, 1, 1, 1, 1, 1, 1, 1, 1, 1, 1, 1, 1, 1, 1, 1, 1, 1, 1, 1, 1, 1, 1, 1, 1, 1, 1, 1, 1, 1, 1, 1, 1, 1, 1, 1, 1, 1, 1, 1, 1, 1, 1, 1, 1, 1, 1, 1, 1, 1, 1, 1, 1, 1, 1, 1, 1, 1, 1, 1, 1, 1, 1, 1, 1, 1, 1, 1, 1, 1, 1, 1, 1, 1, 1, 1, 1, 1, 1, 1, 1, 1, 1, 1, 1, 1, 1, 1, 1, 1, 1, 1, 1, 1, 1, 1, 1, 1, 1, 1, 1, 1, 1, 1, 1, 1, 1, 1, 1, 1, 1, 1, 1, 1, 1, 1, 1, 1, 1, 1, 1, 1, 1, 1, 1, 1, 1, 1, 1, 1, 1, 1, 1, 1, 1, 1, 1, 1, 1, 1, 1, 1, 1, 1, 1, 1, 1, 1, 1, 1, 1, 1, 1, 1, 1, 1, 1, 1, 1, 1, 1, 1, 1, 1, 1, 1, 1, 1, 1, 1, 1, 1, 1, 1, 1, 1, 1, 1, 1, 1, 1, 1, 1, 1, 1, 1, 1, 1, 1, 1, 1, 1, 1, 1, 1, 1, 1, 1, 1, 1, 1, 1, 1, 1, 1, 1, 1, 1, 1, 1, 1, 1, 1, 1, 1, 1, 1, 1, 1, 1, 1, 1, 1, 1, 1, 1, 1, 1, 1, 1, 1, 1, 1, 1, 1, 1, 1, 1, 1, 1, 1, 1, 1, 1, 1, 1, 1, 1, 1, 1, 1, 1, 1, 1, 1, 1, 1, 1, 1, 1, 1, 1, 1, 1, 1, 1, 1, 1, 1, 1, 1, 1, 1, 1, 1, 1, 1, 1, 1, 1, 1, 1, 1, 1, 1, 1, 1, 1, 1, 1, 1, 1, 1, 1, 1, 1, 1, 1, 1, 1, 1, 1, 1, 1, 1, 1, 1, 1, 1, 1, 1, 1, 1, 1, 1, 1, 1, 1, 1, 1, 1, 1, 1, 1, 1, 1, 1, 1, 1, 4 ),
 ( 0.000000000000000000, 0.5000000000000000000, 1.000000000000000000 ),
 ( 0.000000000000000000, 0.002600209826155936224, 0.005208878553436857226, 0.007813350965615119270, 0.01041570154746907992, 0.01302155883015148306, 0.01562460066207539862, 0.01822947720112986364, 0.02083337797298438765, 0.02343721533725894035, 0.02604213897589890969, 0.02864525980212044229, 0.03125073504456635232, 0.03385369766904555017, 0.03645898980682723417, 0.03906240375024701977, 0.04166680464497042602, 0.04427120869897264999, 0.04687461886132015393, 0.04947991130494613921, 0.05208287402783655373, 0.05468834688957619622, 0.05729146186993632622, 0.05989639238693608009, 0.06250023923939096449, 0.06510408216679804128, 0.06770901469741306966, 0.07031212675311915294, 0.07291759917081726272, 0.07552056149378454097, 0.07812585104223603027, 0.08072926279340975064, 0.08333366149866272554, 0.08593806365491549193, 0.08854147146176674643, 0.09114676191340240208, 0.09374972248801059782, 0.09635519323906190092, 0.09895830628708340848, 0.1015632345865536273, 0.1041670796237980645, 0.1067709202568039306, 0.1093758509056654005, 0.1119789607794838548, 0.1145844312107493490, 0.1171873915655986947, 0.1197926790194954738, 0.1223960889855860712, 0.1250004854864837645, 0.1276048858798866925, 0.1302082914968497596, 0.1328135800830011481, 0.1354165386474412147, 0.1380220074263333041, 0.1406251186789811980, 0.1432300448973659046, 0.1458338882574615747, 0.1484377267335943440, 0.1510426556371624596, 0.1536457634674935069, 0.1562512320483212536, 0.1588541905735017246, 0.1614594760690261366, 0.1640628843880489185, 0.1666672788216651824, 0.1692716775892487424, 0.1718750811543677814, 0.1744803680111783883, 0.1770833247038955116, 0.1796887916465979840, 0.1822919012421508056, 0.1848968255159594287, 0.1875006673364670307, 0.1901045037933276616, 0.1927094310880738681, 0.1953125370132051675, 0.1979180038795354257, 0.2005209607134520455, 0.2031262443867272172, 0.2057296511966431873, 0.2083340436999963075, 0.2109384409787386505, 0.2135418426300015604, 0.2161471278935624962, 0.2187500828529475860, 0.2213555480953768861, 0.2239586561720615654, 0.2265635786377499516, 0.2291674190561798496, 0.2317712536313151217, 0.2343761794536610432, 0.2369792836118274071, 0.2395847488995502261, 0.2421877041805577391, 0.2447929861676560459, 0.2473963916063780244, 0.2500007823164346887, 0.2526051782432667259, 0.2552085781186103075, 0.2578138619249652486, 0.2604168152893601151, 0.2630222789673848927, 0.2656253856633817301, 0.2682303064573571261, 0.2708341456111751366, 0.2734379784420828963, 0.2760429029284052760, 0.2786460054577940548, 0.2812514693027542978, 0.2838544231691620401, 0.2864597036061101165, 0.2890631078115080133, 0.2916674968651886135, 0.2942718915769991783, 0.2968752898143142138, 0.2994805722994643427, 0.3020835242071668869, 0.3046889864566129091, 0.3072920919100609050, 0.3098970111686871198, 0.3125008491953192857, 0.3151046804194536644, 0.3177096037060897493, 0.3203127047448455222, 0.3229181672828482230, 0.3255211198729257016, 0.3281263988957095479, 0.3307298020056156362, 0.3333341895397992083, 0.3359385831734401084, 0.3385419799105768290, 0.3411472612104861635, 0.3437502117997557338, 0.3463556727564109927, 0.3489587771054129539, 0.3515636949650152721, 0.3541675320018531359, 0.3567713617566292128, 0.3593762839798815834, 0.3619793836661120978, 0.3645848450329270407, 0.3671877964849088460, 0.3697930742294792128, 0.3723964763816929868, 0.3750008625332226786, 0.3776052552255140804, 0.3802086506002868016, 0.3828139308508870520, 0.3854168802599494681, 0.3880223400595693151, 0.3906254434421968513, 0.3932303600390676390, 0.3958341962234732669, 0.3984380246462727593, 0.4010429459424146859, 0.4036460444141952153, 0.4062515047455624306, 0.4088544551976535102, 0.4114597317999305615, 0.4140631331322238151, 0.4166675180379114662, 0.4192719099256467796, 0.4218753040758395079, 0.4244805834130354061, 0.4270835317800880659, 0.4296889905584002634, 0.4322920931126992272, 0.4348970085831024290, 0.4375008440524135733, 0.4401046712805898320, 0.4427095917858701601, 0.4453126891812490551, 0.4479181486128839262, 0.4505210982032648026, 0.4531263737991432228, 0.4557297744492659897, 0.4583341582458977381, 0.4609385494658484461, 0.4635419425292200413, 0.4661472210888942258, 0.4687501685521111572, 0.4713556264448209299, 0.4739587283088163017, 0.4765636427889929916, 0.4791674776805284197, 0.4817713038514113699, 0.4843762237020596273, 0.4869793201590638665, 0.4895847788266616818, 0.4921877276934932821, 0.4947930024188478271, 0.4973964025245324327, 0.5000007853488734888, 0.5026051760377950872, 0.5052085681520839255, 0.5078138460701020485, 0.5104167927676396266, 0.5130222499104345468, 0.5156253512221359303, 0.5182302648483090302, 0.5208340992993732987, 0.5234379245502747136, 0.5260428438825063280, 0.5286459395391455152, 0.5312513975783873521, 0.5338543458598166147, 0.5364596198505067193, 0.5390630195494738874, 0.5416674015382738627, 0.5442717918329101900, 0.5468751831358398263, 0.5494804605480556603, 0.5520834066180569932, 0.5546888631466128095, 0.5572919640440190392, 0.5598968769523987588, 0.5625007111002878757, 0.5651045355685063720, 0.5677094545185276120, 0.5703125495128006373, 0.5729180070593572482, 0.5755209548935220631, 0.5781262282853970591, 0.5807296277153600750, 0.5833340090053582561, 0.5859383990424469335, 0.5885417896717308750, 0.5911470667139914204, 0.5937500122945923442, 0.5963554683445766447, 0.5989585689656815592, 0.6015634812924701702, 0.6041673152744758690, 0.6067711390973024033, 0.6093760578013157625, 0.6119791522712144660, 0.6145846094607528842, 0.6171875569857874222, 0.6197928299146914233, 0.6223962292133623508, 0.6250006099412922511, 0.6276049998575695676, 0.6302083899509167697, 0.6328136667590675835, 0.6354166119884008257, 0.6380220676954796444, 0.6406251681782773044, 0.6432300800596744139, 0.6458339140130902045, 0.6484377373278128465, 0.6510426559220214848, 0.6536457500055372627, 0.6562512069737248543, 0.6588541543277639523, 0.6614594269295416273, 0.6640628262346358612, 0.6666672065372305500, 0.6692715964694370134, 0.6718749861645568755, 0.6744802628744462902, 0.6770832078906477980, 0.6796886633904898334, 0.6822917638729786294, 0.6848966754451861760, 0.6875005095073121186, 0.6901043324512210475, 0.6927092510718347862, 0.6953123449069624762, 0.6979178017894718256, 0.7005207491106575368, 0.7031260215211581066, 0.7057294209703992571, 0.7083338009843969107, 0.7109381910692819107, 0.7135415805038890502, 0.7161468572513741693, 0.7187498021925872171, 0.7213552576208688283, 0.7239583582410578089, 0.7265632696402853918, 0.7291671039484327599, 0.7317709266588259265, 0.7343758454420658000, 0.7369789391668094547, 0.7395843960993241373, 0.7421873435258099505, 0.7447926158808931829, 0.7473960156120186271, 0.7500003954741673029, 0.7526047858484943287, 0.7552081751603144655, 0.7578134520812660480, 0.7604163970856469001, 0.7630218525780576577, 0.7656249534739711926, 0.7682298648364407345, 0.7708336995279378989, 0.7734375221421257995, 0.7760424412242287184, 0.7786455349766069345, 0.7812509920948264019, 0.7838539397647821261, 0.7864592122003229990, 0.7890626123510894319, 0.7916669921981516200, 0.7942713829987035901, 0.7968747723254782089, 0.7994800495557851105, 0.8020829947615083499, 0.8046884504537559213, 0.8072915517634385862, 0.8098964632253897733, 0.8125002984375870874, 0.8151041210928977598, 0.8177090406101226172, 0.8203121345281733090, 0.8229175919678175521, 0.8255205400194353116, 0.8281258126713292311, 0.8307292133795166622, 0.8333335933482756142, 0.8359379847118599827, 0.8385413741913512187, 0.8411466518669262760, 0.8437495974121898001, 0.8463550534400045011, 0.8489581553015269622, 0.8515630669992224622, 0.8541669028694969246, 0.8567707257032814994, 0.8593756457919137226, 0.8619787400136992295, 0.8645841979105142183, 0.8671871464820134490, 0.8697924194861808012, 0.8723958208895988831, 0.8750002011168627192, 0.8776045931803160283, 0.8802079829503125508, 0.8828132612070975771, 0.8854162072301272612, 0.8880216637292678294, 0.8906247662807315058, 0.8932296783504612980, 0.8958335150162225480, 0.8984373381658604663, 0.9010422589622166800, 0.9036453536258294283, 0.9062508121155921081, 0.9088537613452241093, 0.9114590348376164775, 0.9140624370741091687, 0.9166668176967164294, 0.9192712105969091940, 0.9218746007952320909, 0.9244798797692056480, 0.9270828264082496828, 0.9296882835145078294, 0.9322913868941045124, 0.9348962994721256026, 0.9375001370706889103, 0.9401039606740361210, 0.9427088823143441321, 0.9453119775565693717, 0.9479174367776000976, 0.9505203868030935865, 0.9531256609099927335, 0.9557290641454977420, 0.9583334452981105978, 0.9609378390199675435, 0.9635412300619400350, 0.9661465102466426647, 0.9687494557931184413, 0.9713549143510965544, 0.9739580252604012056, 0.9765629275426017664, 0.9791667581373608709, 0.9817706348486141543, 0.9843755007711335603, 0.9869785191422796311, 0.9895843624858681187, 0.9921867025132995455, 0.9947911529560371502, 0.9973998138561904758, 1.000000000000000000 ),
 .UNSPECIFIED. ) 
 GEOMETRIC_REPRESENTATION_ITEM ( )  RATIONAL_B_SPLINE_SURFACE ( (
 ( 1.000000000000000222, 1.000000000000000222, 0.9999999999999997780, 1.000000000000000222, 1.000000000000000000, 1.000000000000000000, 0.9999999999999997780, 1.000000000000000000, 1.000000000000000000, 1.000000000000000000, 1.000000000000000000, 1.000000000000000222, 1.000000000000000000, 1.000000000000000000, 1.000000000000000222, 0.9999999999999994449, 1.000000000000000222, 1.000000000000000000, 0.9999999999999997780, 1.000000000000000444, 1.000000000000000000, 1.000000000000000222, 1.000000000000000000, 1.000000000000000000, 0.9999999999999996669, 1.000000000000000000, 1.000000000000000222, 0.9999999999999996669, 1.000000000000000222, 1.000000000000000000, 1.000000000000000222, 1.000000000000000000, 1.000000000000000222, 0.9999999999999997780, 1.000000000000000444, 1.000000000000000000, 1.000000000000000222, 0.9999999999999997780, 1.000000000000000222, 1.000000000000000000, 1.000000000000000000, 0.9999999999999997780, 1.000000000000000000, 0.9999999999999997780, 1.000000000000000000, 0.9999999999999997780, 1.000000000000000000, 1.000000000000000000, 0.9999999999999997780, 1.000000000000000000, 1.000000000000000222, 0.9999999999999996669, 1.000000000000000000, 1.000000000000000000, 1.000000000000000222, 0.9999999999999997780, 1.000000000000000444, 1.000000000000000000, 0.9999999999999997780, 1.000000000000000000, 1.000000000000000000, 1.000000000000000000, 1.000000000000000222, 1.000000000000000000, 1.000000000000000000, 1.000000000000000222, 1.000000000000000000, 1.000000000000000000, 0.9999999999999997780, 1.000000000000000222, 1.000000000000000000, 0.9999999999999997780, 1.000000000000000000, 1.000000000000000000, 1.000000000000000000, 1.000000000000000000, 1.000000000000000222, 0.9999999999999996669, 1.000000000000000444, 0.9999999999999996669, 1.000000000000000000, 0.9999999999999996669, 1.000000000000000444, 1.000000000000000000, 1.000000000000000000, 1.000000000000000222, 1.000000000000000000, 1.000000000000000000, 1.000000000000000222, 0.9999999999999997780, 1.000000000000000000, 1.000000000000000444, 0.9999999999999997780, 1.000000000000000444, 0.9999999999999997780, 1.000000000000000000, 1.000000000000000222, 1.000000000000000000, 0.9999999999999997780, 1.000000000000000222, 1.000000000000000222, 0.9999999999999997780, 1.000000000000000000, 1.000000000000000222, 0.9999999999999997780, 1.000000000000000444, 0.9999999999999997780, 1.000000000000000444, 0.9999999999999997780, 1.000000000000000000, 1.000000000000000222, 0.9999999999999996669, 1.000000000000000000, 1.000000000000000000, 1.000000000000000444, 1.000000000000000222, 0.9999999999999997780, 1.000000000000000222, 1.000000000000000222, 1.000000000000000000, 1.000000000000000222, 0.9999999999999997780, 1.000000000000000000, 1.000000000000000222, 0.9999999999999996669, 1.000000000000000000, 1.000000000000000000, 1.000000000000000000, 1.000000000000000000, 1.000000000000000000, 1.000000000000000000, 1.000000000000000000, 0.9999999999999997780, 1.000000000000000222, 0.9999999999999997780, 1.000000000000000000, 0.9999999999999997780, 1.000000000000000222, 1.000000000000000000, 1.000000000000000000, 1.000000000000000000, 1.000000000000000222, 0.9999999999999997780, 0.9999999999999997780, 1.000000000000000222, 1.000000000000000222, 1.000000000000000000, 1.000000000000000444, 0.9999999999999996669, 1.000000000000000444, 0.9999999999999997780, 1.000000000000000222, 1.000000000000000000, 1.000000000000000000, 1.000000000000000000, 1.000000000000000222, 0.9999999999999997780, 0.9999999999999997780, 1.000000000000000444, 1.000000000000000444, 0.9999999999999997780, 1.000000000000000000, 1.000000000000000000, 1.000000000000000000, 1.000000000000000222, 1.000000000000000000, 1.000000000000000000, 1.000000000000000222, 1.000000000000000222, 1.000000000000000000, 1.000000000000000444, 1.000000000000000000, 1.000000000000000222, 1.000000000000000000, 1.000000000000000000, 1.000000000000000444, 1.000000000000000000, 1.000000000000000222, 1.000000000000000000, 1.000000000000000222, 0.9999999999999997780, 1.000000000000000222, 1.000000000000000222, 1.000000000000000000, 0.9999999999999996669, 1.000000000000000222, 1.000000000000000000, 1.000000000000000000, 1.000000000000000222, 1.000000000000000222, 1.000000000000000222, 0.9999999999999997780, 1.000000000000000000, 1.000000000000000222, 1.000000000000000000, 1.000000000000000000, 1.000000000000000000, 0.9999999999999996669, 1.000000000000000444, 1.000000000000000222, 0.9999999999999996669, 1.000000000000000444, 1.000000000000000000, 1.000000000000000000, 1.000000000000000222, 0.9999999999999997780, 1.000000000000000444, 0.9999999999999997780, 0.9999999999999997780, 1.000000000000000444, 0.9999999999999997780, 1.000000000000000222, 1.000000000000000000, 1.000000000000000000, 1.000000000000000000, 0.9999999999999997780, 1.000000000000000000, 1.000000000000000222, 0.9999999999999996669, 1.000000000000000222, 1.000000000000000000, 1.000000000000000222, 0.9999999999999996669, 0.9999999999999997780, 1.000000000000000444, 0.9999999999999997780, 0.9999999999999997780, 1.000000000000000000, 1.000000000000000222, 1.000000000000000000, 1.000000000000000000, 0.9999999999999996669, 1.000000000000000222, 1.000000000000000000, 0.9999999999999997780, 1.000000000000000000, 1.000000000000000000, 0.9999999999999997780, 1.000000000000000444, 0.9999999999999996669, 1.000000000000000444, 0.9999999999999997780, 1.000000000000000000, 1.000000000000000222, 0.9999999999999997780, 1.000000000000000222, 1.000000000000000222, 0.9999999999999997780, 1.000000000000000000, 1.000000000000000000, 1.000000000000000000, 1.000000000000000222, 1.000000000000000000, 1.000000000000000000, 1.000000000000000222, 1.000000000000000222, 1.000000000000000000, 1.000000000000000000, 1.000000000000000222, 0.9999999999999997780, 1.000000000000000000, 1.000000000000000222, 1.000000000000000000, 1.000000000000000222, 0.9999999999999997780, 1.000000000000000222, 0.9999999999999997780, 1.000000000000000222, 0.9999999999999997780, 1.000000000000000222, 1.000000000000000000, 1.000000000000000000, 1.000000000000000444, 0.9999999999999996669, 1.000000000000000222, 0.9999999999999997780, 1.000000000000000000, 1.000000000000000222, 1.000000000000000000, 1.000000000000000222, 0.9999999999999997780, 0.9999999999999997780, 1.000000000000000000, 0.9999999999999997780, 1.000000000000000000, 1.000000000000000000, 1.000000000000000222, 1.000000000000000000, 1.000000000000000000, 1.000000000000000222, 1.000000000000000000, 1.000000000000000000, 1.000000000000000000, 1.000000000000000000, 0.9999999999999997780, 1.000000000000000222, 1.000000000000000222, 0.9999999999999997780, 1.000000000000000444, 1.000000000000000444, 0.9999999999999997780, 1.000000000000000000, 0.9999999999999997780, 1.000000000000000000, 1.000000000000000000, 1.000000000000000000, 1.000000000000000000, 0.9999999999999997780, 1.000000000000000222, 1.000000000000000000, 0.9999999999999997780, 1.000000000000000222, 1.000000000000000000, 1.000000000000000000, 1.000000000000000000, 1.000000000000000444, 1.000000000000000000, 0.9999999999999997780, 0.9999999999999997780, 0.9999999999999997780, 1.000000000000000222, 1.000000000000000222, 0.9999999999999996669, 1.000000000000000222, 0.9999999999999997780, 1.000000000000000222, 1.000000000000000000, 1.000000000000000000, 0.9999999999999996669, 1.000000000000000222, 1.000000000000000222, 1.000000000000000000, 1.000000000000000000, 1.000000000000000222, 0.9999999999999997780, 1.000000000000000000, 1.000000000000000222, 0.9999999999999994449, 1.000000000000000222, 1.000000000000000000, 1.000000000000000222, 0.9999999999999997780, 1.000000000000000000, 1.000000000000000000, 0.9999999999999997780, 1.000000000000000000, 1.000000000000000222, 0.9999999999999997780, 1.000000000000000000, 1.000000000000000000, 1.000000000000000000, 1.000000000000000000, 1.000000000000000222, 1.000000000000000000, 0.9999999999999996669, 0.9999999999999996669, 1.000000000000000222, 0.9999999999999997780, 1.000000000000000222, 1.000000000000000000, 0.9999999999999997780, 1.000000000000000222, 0.9999999999999997780, 1.000000000000000444, 1.000000000000000222, 1.000000000000000000, 1.000000000000000222, 1.000000000000000222, 1.000000000000000000, 1.000000000000000000, 1.000000000000000000, 1.000000000000000000, 1.000000000000000000, 1.000000000000000000, 1.000000000000000000, 0.9999999999999997780, 1.000000000000000000, 0.9999999999999996669, 1.000000000000000444, 0.9999999999999996669, 1.000000000000000000, 1.000000000000000000, 0.9999999999999997780, 1.000000000000000444, 1.000000000000000000, 1.000000000000000000, 1.000000000000000000),
 ( 0.3333333333333334259, 0.3333333333333334259, 0.3333333333333333703, 0.3333333333333333703, 0.3333333333333334259, 0.3333333333333333703, 0.3333333333333333703, 0.3333333333333334259, 0.3333333333333333148, 0.3333333333333334814, 0.3333333333333332593, 0.3333333333333335369, 0.3333333333333333148, 0.3333333333333333703, 0.3333333333333334259, 0.3333333333333332593, 0.3333333333333333703, 0.3333333333333333703, 0.3333333333333334259, 0.3333333333333334814, 0.3333333333333333148, 0.3333333333333334259, 0.3333333333333333703, 0.3333333333333333703, 0.3333333333333333148, 0.3333333333333333703, 0.3333333333333334259, 0.3333333333333332038, 0.3333333333333334259, 0.3333333333333333703, 0.3333333333333334259, 0.3333333333333333703, 0.3333333333333333148, 0.3333333333333334259, 0.3333333333333334259, 0.3333333333333333703, 0.3333333333333334814, 0.3333333333333332593, 0.3333333333333334259, 0.3333333333333334259, 0.3333333333333333148, 0.3333333333333333703, 0.3333333333333333148, 0.3333333333333333703, 0.3333333333333333148, 0.3333333333333333703, 0.3333333333333333703, 0.3333333333333333703, 0.3333333333333333148, 0.3333333333333333148, 0.3333333333333334259, 0.3333333333333332593, 0.3333333333333333703, 0.3333333333333333703, 0.3333333333333333703, 0.3333333333333332593, 0.3333333333333334259, 0.3333333333333333148, 0.3333333333333333148, 0.3333333333333333703, 0.3333333333333333703, 0.3333333333333333703, 0.3333333333333334259, 0.3333333333333333148, 0.3333333333333334259, 0.3333333333333334259, 0.3333333333333333703, 0.3333333333333333703, 0.3333333333333333148, 0.3333333333333333703, 0.3333333333333333703, 0.3333333333333333148, 0.3333333333333333703, 0.3333333333333332593, 0.3333333333333334814, 0.3333333333333333148, 0.3333333333333333703, 0.3333333333333332593, 0.3333333333333335369, 0.3333333333333333703, 0.3333333333333333703, 0.3333333333333333703, 0.3333333333333334259, 0.3333333333333334259, 0.3333333333333333148, 0.3333333333333334259, 0.3333333333333333148, 0.3333333333333333703, 0.3333333333333335369, 0.3333333333333333148, 0.3333333333333334259, 0.3333333333333334814, 0.3333333333333333148, 0.3333333333333335369, 0.3333333333333332593, 0.3333333333333333703, 0.3333333333333333148, 0.3333333333333334259, 0.3333333333333333148, 0.3333333333333334814, 0.3333333333333333703, 0.3333333333333333148, 0.3333333333333333703, 0.3333333333333334259, 0.3333333333333333703, 0.3333333333333334259, 0.3333333333333332593, 0.3333333333333335924, 0.3333333333333333148, 0.3333333333333333148, 0.3333333333333334259, 0.3333333333333332593, 0.3333333333333333703, 0.3333333333333333148, 0.3333333333333335369, 0.3333333333333333703, 0.3333333333333333703, 0.3333333333333334259, 0.3333333333333334259, 0.3333333333333333703, 0.3333333333333333703, 0.3333333333333333703, 0.3333333333333333703, 0.3333333333333334259, 0.3333333333333333703, 0.3333333333333333703, 0.3333333333333333703, 0.3333333333333334259, 0.3333333333333333148, 0.3333333333333333703, 0.3333333333333333703, 0.3333333333333334259, 0.3333333333333333148, 0.3333333333333333703, 0.3333333333333333703, 0.3333333333333333703, 0.3333333333333333148, 0.3333333333333334259, 0.3333333333333333148, 0.3333333333333333703, 0.3333333333333334259, 0.3333333333333333703, 0.3333333333333333703, 0.3333333333333333703, 0.3333333333333333703, 0.3333333333333334259, 0.3333333333333334259, 0.3333333333333334259, 0.3333333333333333148, 0.3333333333333334259, 0.3333333333333333148, 0.3333333333333334259, 0.3333333333333334259, 0.3333333333333333703, 0.3333333333333333148, 0.3333333333333333703, 0.3333333333333333703, 0.3333333333333333148, 0.3333333333333334259, 0.3333333333333335369, 0.3333333333333333148, 0.3333333333333332593, 0.3333333333333334814, 0.3333333333333332593, 0.3333333333333333703, 0.3333333333333333703, 0.3333333333333333703, 0.3333333333333334259, 0.3333333333333334259, 0.3333333333333334259, 0.3333333333333335369, 0.3333333333333333703, 0.3333333333333333703, 0.3333333333333333703, 0.3333333333333334259, 0.3333333333333333703, 0.3333333333333333703, 0.3333333333333334259, 0.3333333333333333703, 0.3333333333333334259, 0.3333333333333332593, 0.3333333333333334259, 0.3333333333333334259, 0.3333333333333333148, 0.3333333333333333703, 0.3333333333333333703, 0.3333333333333333703, 0.3333333333333333703, 0.3333333333333334259, 0.3333333333333334259, 0.3333333333333334259, 0.3333333333333333148, 0.3333333333333333703, 0.3333333333333334259, 0.3333333333333332593, 0.3333333333333334814, 0.3333333333333333148, 0.3333333333333332593, 0.3333333333333335369, 0.3333333333333333148, 0.3333333333333333703, 0.3333333333333334259, 0.3333333333333333148, 0.3333333333333333703, 0.3333333333333334259, 0.3333333333333333148, 0.3333333333333335369, 0.3333333333333332593, 0.3333333333333333703, 0.3333333333333334259, 0.3333333333333333148, 0.3333333333333334259, 0.3333333333333333148, 0.3333333333333333703, 0.3333333333333333703, 0.3333333333333333703, 0.3333333333333333703, 0.3333333333333334259, 0.3333333333333332593, 0.3333333333333334259, 0.3333333333333334259, 0.3333333333333333703, 0.3333333333333333703, 0.3333333333333333148, 0.3333333333333334814, 0.3333333333333333703, 0.3333333333333332593, 0.3333333333333334259, 0.3333333333333334259, 0.3333333333333334259, 0.3333333333333333703, 0.3333333333333332038, 0.3333333333333335369, 0.3333333333333333148, 0.3333333333333333148, 0.3333333333333333703, 0.3333333333333333703, 0.3333333333333333703, 0.3333333333333334259, 0.3333333333333333148, 0.3333333333333334814, 0.3333333333333333148, 0.3333333333333333703, 0.3333333333333334259, 0.3333333333333333148, 0.3333333333333334259, 0.3333333333333333148, 0.3333333333333334259, 0.3333333333333333148, 0.3333333333333333703, 0.3333333333333333703, 0.3333333333333334259, 0.3333333333333333703, 0.3333333333333333148, 0.3333333333333334814, 0.3333333333333334259, 0.3333333333333333703, 0.3333333333333333148, 0.3333333333333334259, 0.3333333333333333703, 0.3333333333333333703, 0.3333333333333334259, 0.3333333333333333703, 0.3333333333333334814, 0.3333333333333333148, 0.3333333333333334259, 0.3333333333333333703, 0.3333333333333334259, 0.3333333333333333148, 0.3333333333333333703, 0.3333333333333334259, 0.3333333333333333703, 0.3333333333333334259, 0.3333333333333332593, 0.3333333333333333703, 0.3333333333333332593, 0.3333333333333334259, 0.3333333333333333703, 0.3333333333333334259, 0.3333333333333334259, 0.3333333333333333148, 0.3333333333333333148, 0.3333333333333334259, 0.3333333333333333148, 0.3333333333333333148, 0.3333333333333333703, 0.3333333333333333703, 0.3333333333333334259, 0.3333333333333333703, 0.3333333333333334814, 0.3333333333333332593, 0.3333333333333334259, 0.3333333333333333703, 0.3333333333333333703, 0.3333333333333334259, 0.3333333333333333703, 0.3333333333333333703, 0.3333333333333334259, 0.3333333333333334259, 0.3333333333333334814, 0.3333333333333333148, 0.3333333333333333148, 0.3333333333333333703, 0.3333333333333333148, 0.3333333333333334259, 0.3333333333333333703, 0.3333333333333333148, 0.3333333333333332593, 0.3333333333333334259, 0.3333333333333334259, 0.3333333333333333148, 0.3333333333333333703, 0.3333333333333334259, 0.3333333333333333148, 0.3333333333333334259, 0.3333333333333334259, 0.3333333333333334814, 0.3333333333333333148, 0.3333333333333333703, 0.3333333333333332593, 0.3333333333333334814, 0.3333333333333333703, 0.3333333333333332593, 0.3333333333333334814, 0.3333333333333332593, 0.3333333333333334259, 0.3333333333333333703, 0.3333333333333333148, 0.3333333333333333148, 0.3333333333333334259, 0.3333333333333333703, 0.3333333333333333703, 0.3333333333333333703, 0.3333333333333333703, 0.3333333333333334259, 0.3333333333333333148, 0.3333333333333334259, 0.3333333333333332038, 0.3333333333333334259, 0.3333333333333333148, 0.3333333333333334814, 0.3333333333333333703, 0.3333333333333333703, 0.3333333333333334259, 0.3333333333333333148, 0.3333333333333333703, 0.3333333333333333703, 0.3333333333333333703, 0.3333333333333333703, 0.3333333333333333703, 0.3333333333333334259, 0.3333333333333333148, 0.3333333333333334814, 0.3333333333333334259, 0.3333333333333332593, 0.3333333333333333703, 0.3333333333333333703, 0.3333333333333333703, 0.3333333333333333703, 0.3333333333333333703, 0.3333333333333334259, 0.3333333333333333148, 0.3333333333333333703, 0.3333333333333334259, 0.3333333333333335369, 0.3333333333333333148, 0.3333333333333333703, 0.3333333333333334259, 0.3333333333333333703, 0.3333333333333333703, 0.3333333333333333703, 0.3333333333333333703, 0.3333333333333333703, 0.3333333333333333703, 0.3333333333333333703, 0.3333333333333333703, 0.3333333333333334259, 0.3333333333333332593, 0.3333333333333334814, 0.3333333333333332593, 0.3333333333333334259, 0.3333333333333333703, 0.3333333333333333703, 0.3333333333333334814, 0.3333333333333333148, 0.3333333333333333703, 0.3333333333333333703),
 ( 0.3333333333333334259, 0.3333333333333334259, 0.3333333333333333703, 0.3333333333333333703, 0.3333333333333334259, 0.3333333333333333703, 0.3333333333333333703, 0.3333333333333334259, 0.3333333333333333148, 0.3333333333333334814, 0.3333333333333332593, 0.3333333333333335369, 0.3333333333333333148, 0.3333333333333333703, 0.3333333333333334259, 0.3333333333333332593, 0.3333333333333333703, 0.3333333333333333703, 0.3333333333333334259, 0.3333333333333334814, 0.3333333333333333148, 0.3333333333333334259, 0.3333333333333333703, 0.3333333333333333703, 0.3333333333333333148, 0.3333333333333333703, 0.3333333333333334259, 0.3333333333333332038, 0.3333333333333334259, 0.3333333333333333703, 0.3333333333333334259, 0.3333333333333333703, 0.3333333333333333148, 0.3333333333333334259, 0.3333333333333334259, 0.3333333333333333703, 0.3333333333333334814, 0.3333333333333332593, 0.3333333333333334259, 0.3333333333333334259, 0.3333333333333333148, 0.3333333333333333703, 0.3333333333333333148, 0.3333333333333333703, 0.3333333333333333148, 0.3333333333333333703, 0.3333333333333333703, 0.3333333333333333703, 0.3333333333333333148, 0.3333333333333333148, 0.3333333333333334259, 0.3333333333333332593, 0.3333333333333333703, 0.3333333333333333703, 0.3333333333333333703, 0.3333333333333332593, 0.3333333333333334259, 0.3333333333333333148, 0.3333333333333333148, 0.3333333333333333703, 0.3333333333333333703, 0.3333333333333333703, 0.3333333333333334259, 0.3333333333333333148, 0.3333333333333334259, 0.3333333333333334259, 0.3333333333333333703, 0.3333333333333333703, 0.3333333333333333148, 0.3333333333333333703, 0.3333333333333333703, 0.3333333333333333148, 0.3333333333333333703, 0.3333333333333332593, 0.3333333333333334814, 0.3333333333333333148, 0.3333333333333333703, 0.3333333333333332593, 0.3333333333333335369, 0.3333333333333333703, 0.3333333333333333703, 0.3333333333333333703, 0.3333333333333334259, 0.3333333333333334259, 0.3333333333333333148, 0.3333333333333334259, 0.3333333333333333148, 0.3333333333333333703, 0.3333333333333335369, 0.3333333333333333148, 0.3333333333333334259, 0.3333333333333334814, 0.3333333333333333148, 0.3333333333333335369, 0.3333333333333332593, 0.3333333333333333703, 0.3333333333333333148, 0.3333333333333334259, 0.3333333333333333148, 0.3333333333333334814, 0.3333333333333333703, 0.3333333333333333148, 0.3333333333333333703, 0.3333333333333334259, 0.3333333333333333703, 0.3333333333333334259, 0.3333333333333332593, 0.3333333333333335924, 0.3333333333333333148, 0.3333333333333333148, 0.3333333333333334259, 0.3333333333333332593, 0.3333333333333333703, 0.3333333333333333148, 0.3333333333333335369, 0.3333333333333333703, 0.3333333333333333703, 0.3333333333333334259, 0.3333333333333334259, 0.3333333333333333703, 0.3333333333333333703, 0.3333333333333333703, 0.3333333333333333703, 0.3333333333333334259, 0.3333333333333333703, 0.3333333333333333703, 0.3333333333333333703, 0.3333333333333334259, 0.3333333333333333148, 0.3333333333333333703, 0.3333333333333333703, 0.3333333333333334259, 0.3333333333333333148, 0.3333333333333333703, 0.3333333333333333703, 0.3333333333333333703, 0.3333333333333333148, 0.3333333333333334259, 0.3333333333333333148, 0.3333333333333333703, 0.3333333333333334259, 0.3333333333333333703, 0.3333333333333333703, 0.3333333333333333703, 0.3333333333333333703, 0.3333333333333334259, 0.3333333333333334259, 0.3333333333333334259, 0.3333333333333333148, 0.3333333333333334259, 0.3333333333333333148, 0.3333333333333334259, 0.3333333333333334259, 0.3333333333333333703, 0.3333333333333333148, 0.3333333333333333703, 0.3333333333333333703, 0.3333333333333333148, 0.3333333333333334259, 0.3333333333333335369, 0.3333333333333333148, 0.3333333333333332593, 0.3333333333333334814, 0.3333333333333332593, 0.3333333333333333703, 0.3333333333333333703, 0.3333333333333333703, 0.3333333333333334259, 0.3333333333333334259, 0.3333333333333334259, 0.3333333333333335369, 0.3333333333333333703, 0.3333333333333333703, 0.3333333333333333703, 0.3333333333333334259, 0.3333333333333333703, 0.3333333333333333703, 0.3333333333333334259, 0.3333333333333333703, 0.3333333333333334259, 0.3333333333333332593, 0.3333333333333334259, 0.3333333333333334259, 0.3333333333333333148, 0.3333333333333333703, 0.3333333333333333703, 0.3333333333333333703, 0.3333333333333333703, 0.3333333333333334259, 0.3333333333333334259, 0.3333333333333334259, 0.3333333333333333148, 0.3333333333333333703, 0.3333333333333334259, 0.3333333333333332593, 0.3333333333333334814, 0.3333333333333333148, 0.3333333333333332593, 0.3333333333333335369, 0.3333333333333333148, 0.3333333333333333703, 0.3333333333333334259, 0.3333333333333333148, 0.3333333333333333703, 0.3333333333333334259, 0.3333333333333333148, 0.3333333333333335369, 0.3333333333333332593, 0.3333333333333333703, 0.3333333333333334259, 0.3333333333333333148, 0.3333333333333334259, 0.3333333333333333148, 0.3333333333333333703, 0.3333333333333333703, 0.3333333333333333703, 0.3333333333333333703, 0.3333333333333334259, 0.3333333333333332593, 0.3333333333333334259, 0.3333333333333334259, 0.3333333333333333703, 0.3333333333333333703, 0.3333333333333333148, 0.3333333333333334814, 0.3333333333333333703, 0.3333333333333332593, 0.3333333333333334259, 0.3333333333333334259, 0.3333333333333334259, 0.3333333333333333703, 0.3333333333333332038, 0.3333333333333335369, 0.3333333333333333148, 0.3333333333333333148, 0.3333333333333333703, 0.3333333333333333703, 0.3333333333333333703, 0.3333333333333334259, 0.3333333333333333148, 0.3333333333333334814, 0.3333333333333333148, 0.3333333333333333703, 0.3333333333333334259, 0.3333333333333333148, 0.3333333333333334259, 0.3333333333333333148, 0.3333333333333334259, 0.3333333333333333148, 0.3333333333333333703, 0.3333333333333333703, 0.3333333333333334259, 0.3333333333333333703, 0.3333333333333333148, 0.3333333333333334814, 0.3333333333333334259, 0.3333333333333333703, 0.3333333333333333148, 0.3333333333333334259, 0.3333333333333333703, 0.3333333333333333703, 0.3333333333333334259, 0.3333333333333333703, 0.3333333333333334814, 0.3333333333333333148, 0.3333333333333334259, 0.3333333333333333703, 0.3333333333333334259, 0.3333333333333333148, 0.3333333333333333703, 0.3333333333333334259, 0.3333333333333333703, 0.3333333333333334259, 0.3333333333333332593, 0.3333333333333333703, 0.3333333333333332593, 0.3333333333333334259, 0.3333333333333333703, 0.3333333333333334259, 0.3333333333333334259, 0.3333333333333333148, 0.3333333333333333148, 0.3333333333333334259, 0.3333333333333333148, 0.3333333333333333148, 0.3333333333333333703, 0.3333333333333333703, 0.3333333333333334259, 0.3333333333333333703, 0.3333333333333334814, 0.3333333333333332593, 0.3333333333333334259, 0.3333333333333333703, 0.3333333333333333703, 0.3333333333333334259, 0.3333333333333333703, 0.3333333333333333703, 0.3333333333333334259, 0.3333333333333334259, 0.3333333333333334814, 0.3333333333333333148, 0.3333333333333333148, 0.3333333333333333703, 0.3333333333333333148, 0.3333333333333334259, 0.3333333333333333703, 0.3333333333333333148, 0.3333333333333332593, 0.3333333333333334259, 0.3333333333333334259, 0.3333333333333333148, 0.3333333333333333703, 0.3333333333333334259, 0.3333333333333333148, 0.3333333333333334259, 0.3333333333333334259, 0.3333333333333334814, 0.3333333333333333148, 0.3333333333333333703, 0.3333333333333332593, 0.3333333333333334814, 0.3333333333333333703, 0.3333333333333332593, 0.3333333333333334814, 0.3333333333333332593, 0.3333333333333334259, 0.3333333333333333703, 0.3333333333333333148, 0.3333333333333333148, 0.3333333333333334259, 0.3333333333333333703, 0.3333333333333333703, 0.3333333333333333703, 0.3333333333333333703, 0.3333333333333334259, 0.3333333333333333148, 0.3333333333333334259, 0.3333333333333332038, 0.3333333333333334259, 0.3333333333333333148, 0.3333333333333334814, 0.3333333333333333703, 0.3333333333333333703, 0.3333333333333334259, 0.3333333333333333148, 0.3333333333333333703, 0.3333333333333333703, 0.3333333333333333703, 0.3333333333333333703, 0.3333333333333333703, 0.3333333333333334259, 0.3333333333333333148, 0.3333333333333334814, 0.3333333333333334259, 0.3333333333333332593, 0.3333333333333333703, 0.3333333333333333703, 0.3333333333333333703, 0.3333333333333333703, 0.3333333333333333703, 0.3333333333333334259, 0.3333333333333333148, 0.3333333333333333703, 0.3333333333333334259, 0.3333333333333335369, 0.3333333333333333148, 0.3333333333333333703, 0.3333333333333334259, 0.3333333333333333703, 0.3333333333333333703, 0.3333333333333333703, 0.3333333333333333703, 0.3333333333333333703, 0.3333333333333333703, 0.3333333333333333703, 0.3333333333333333703, 0.3333333333333334259, 0.3333333333333332593, 0.3333333333333334814, 0.3333333333333332593, 0.3333333333333334259, 0.3333333333333333703, 0.3333333333333333703, 0.3333333333333334814, 0.3333333333333333148, 0.3333333333333333703, 0.3333333333333333703),
 ( 1.000000000000000222, 1.000000000000000222, 0.9999999999999997780, 1.000000000000000222, 1.000000000000000000, 1.000000000000000000, 0.9999999999999997780, 1.000000000000000000, 1.000000000000000000, 1.000000000000000000, 1.000000000000000000, 1.000000000000000222, 1.000000000000000000, 1.000000000000000000, 1.000000000000000222, 0.9999999999999994449, 1.000000000000000222, 1.000000000000000000, 0.9999999999999997780, 1.000000000000000444, 1.000000000000000000, 1.000000000000000222, 1.000000000000000000, 1.000000000000000000, 0.9999999999999996669, 1.000000000000000000, 1.000000000000000222, 0.9999999999999996669, 1.000000000000000222, 1.000000000000000000, 1.000000000000000222, 1.000000000000000000, 1.000000000000000222, 0.9999999999999997780, 1.000000000000000444, 1.000000000000000000, 1.000000000000000222, 0.9999999999999997780, 1.000000000000000222, 1.000000000000000000, 1.000000000000000000, 0.9999999999999997780, 1.000000000000000000, 0.9999999999999997780, 1.000000000000000000, 0.9999999999999997780, 1.000000000000000000, 1.000000000000000000, 0.9999999999999997780, 1.000000000000000000, 1.000000000000000222, 0.9999999999999996669, 1.000000000000000000, 1.000000000000000000, 1.000000000000000222, 0.9999999999999997780, 1.000000000000000444, 1.000000000000000000, 0.9999999999999997780, 1.000000000000000000, 1.000000000000000000, 1.000000000000000000, 1.000000000000000222, 1.000000000000000000, 1.000000000000000000, 1.000000000000000222, 1.000000000000000000, 1.000000000000000000, 0.9999999999999997780, 1.000000000000000222, 1.000000000000000000, 0.9999999999999997780, 1.000000000000000000, 1.000000000000000000, 1.000000000000000000, 1.000000000000000000, 1.000000000000000222, 0.9999999999999996669, 1.000000000000000444, 0.9999999999999996669, 1.000000000000000000, 0.9999999999999996669, 1.000000000000000444, 1.000000000000000000, 1.000000000000000000, 1.000000000000000222, 1.000000000000000000, 1.000000000000000000, 1.000000000000000222, 0.9999999999999997780, 1.000000000000000000, 1.000000000000000444, 0.9999999999999997780, 1.000000000000000444, 0.9999999999999997780, 1.000000000000000000, 1.000000000000000222, 1.000000000000000000, 0.9999999999999997780, 1.000000000000000222, 1.000000000000000222, 0.9999999999999997780, 1.000000000000000000, 1.000000000000000222, 0.9999999999999997780, 1.000000000000000444, 0.9999999999999997780, 1.000000000000000444, 0.9999999999999997780, 1.000000000000000000, 1.000000000000000222, 0.9999999999999996669, 1.000000000000000000, 1.000000000000000000, 1.000000000000000444, 1.000000000000000222, 0.9999999999999997780, 1.000000000000000222, 1.000000000000000222, 1.000000000000000000, 1.000000000000000222, 0.9999999999999997780, 1.000000000000000000, 1.000000000000000222, 0.9999999999999996669, 1.000000000000000000, 1.000000000000000000, 1.000000000000000000, 1.000000000000000000, 1.000000000000000000, 1.000000000000000000, 1.000000000000000000, 0.9999999999999997780, 1.000000000000000222, 0.9999999999999997780, 1.000000000000000000, 0.9999999999999997780, 1.000000000000000222, 1.000000000000000000, 1.000000000000000000, 1.000000000000000000, 1.000000000000000222, 0.9999999999999997780, 0.9999999999999997780, 1.000000000000000222, 1.000000000000000222, 1.000000000000000000, 1.000000000000000444, 0.9999999999999996669, 1.000000000000000444, 0.9999999999999997780, 1.000000000000000222, 1.000000000000000000, 1.000000000000000000, 1.000000000000000000, 1.000000000000000222, 0.9999999999999997780, 0.9999999999999997780, 1.000000000000000444, 1.000000000000000444, 0.9999999999999997780, 1.000000000000000000, 1.000000000000000000, 1.000000000000000000, 1.000000000000000222, 1.000000000000000000, 1.000000000000000000, 1.000000000000000222, 1.000000000000000222, 1.000000000000000000, 1.000000000000000444, 1.000000000000000000, 1.000000000000000222, 1.000000000000000000, 1.000000000000000000, 1.000000000000000444, 1.000000000000000000, 1.000000000000000222, 1.000000000000000000, 1.000000000000000222, 0.9999999999999997780, 1.000000000000000222, 1.000000000000000222, 1.000000000000000000, 0.9999999999999996669, 1.000000000000000222, 1.000000000000000000, 1.000000000000000000, 1.000000000000000222, 1.000000000000000222, 1.000000000000000222, 0.9999999999999997780, 1.000000000000000000, 1.000000000000000222, 1.000000000000000000, 1.000000000000000000, 1.000000000000000000, 0.9999999999999996669, 1.000000000000000444, 1.000000000000000222, 0.9999999999999996669, 1.000000000000000444, 1.000000000000000000, 1.000000000000000000, 1.000000000000000222, 0.9999999999999997780, 1.000000000000000444, 0.9999999999999997780, 0.9999999999999997780, 1.000000000000000444, 0.9999999999999997780, 1.000000000000000222, 1.000000000000000000, 1.000000000000000000, 1.000000000000000000, 0.9999999999999997780, 1.000000000000000000, 1.000000000000000222, 0.9999999999999996669, 1.000000000000000222, 1.000000000000000000, 1.000000000000000222, 0.9999999999999996669, 0.9999999999999997780, 1.000000000000000444, 0.9999999999999997780, 0.9999999999999997780, 1.000000000000000000, 1.000000000000000222, 1.000000000000000000, 1.000000000000000000, 0.9999999999999996669, 1.000000000000000222, 1.000000000000000000, 0.9999999999999997780, 1.000000000000000000, 1.000000000000000000, 0.9999999999999997780, 1.000000000000000444, 0.9999999999999996669, 1.000000000000000444, 0.9999999999999997780, 1.000000000000000000, 1.000000000000000222, 0.9999999999999997780, 1.000000000000000222, 1.000000000000000222, 0.9999999999999997780, 1.000000000000000000, 1.000000000000000000, 1.000000000000000000, 1.000000000000000222, 1.000000000000000000, 1.000000000000000000, 1.000000000000000222, 1.000000000000000222, 1.000000000000000000, 1.000000000000000000, 1.000000000000000222, 0.9999999999999997780, 1.000000000000000000, 1.000000000000000222, 1.000000000000000000, 1.000000000000000222, 0.9999999999999997780, 1.000000000000000222, 0.9999999999999997780, 1.000000000000000222, 0.9999999999999997780, 1.000000000000000222, 1.000000000000000000, 1.000000000000000000, 1.000000000000000444, 0.9999999999999996669, 1.000000000000000222, 0.9999999999999997780, 1.000000000000000000, 1.000000000000000222, 1.000000000000000000, 1.000000000000000222, 0.9999999999999997780, 0.9999999999999997780, 1.000000000000000000, 0.9999999999999997780, 1.000000000000000000, 1.000000000000000000, 1.000000000000000222, 1.000000000000000000, 1.000000000000000000, 1.000000000000000222, 1.000000000000000000, 1.000000000000000000, 1.000000000000000000, 1.000000000000000000, 0.9999999999999997780, 1.000000000000000222, 1.000000000000000222, 0.9999999999999997780, 1.000000000000000444, 1.000000000000000444, 0.9999999999999997780, 1.000000000000000000, 0.9999999999999997780, 1.000000000000000000, 1.000000000000000000, 1.000000000000000000, 1.000000000000000000, 0.9999999999999997780, 1.000000000000000222, 1.000000000000000000, 0.9999999999999997780, 1.000000000000000222, 1.000000000000000000, 1.000000000000000000, 1.000000000000000000, 1.000000000000000444, 1.000000000000000000, 0.9999999999999997780, 0.9999999999999997780, 0.9999999999999997780, 1.000000000000000222, 1.000000000000000222, 0.9999999999999996669, 1.000000000000000222, 0.9999999999999997780, 1.000000000000000222, 1.000000000000000000, 1.000000000000000000, 0.9999999999999996669, 1.000000000000000222, 1.000000000000000222, 1.000000000000000000, 1.000000000000000000, 1.000000000000000222, 0.9999999999999997780, 1.000000000000000000, 1.000000000000000222, 0.9999999999999994449, 1.000000000000000222, 1.000000000000000000, 1.000000000000000222, 0.9999999999999997780, 1.000000000000000000, 1.000000000000000000, 0.9999999999999997780, 1.000000000000000000, 1.000000000000000222, 0.9999999999999997780, 1.000000000000000000, 1.000000000000000000, 1.000000000000000000, 1.000000000000000000, 1.000000000000000222, 1.000000000000000000, 0.9999999999999996669, 0.9999999999999996669, 1.000000000000000222, 0.9999999999999997780, 1.000000000000000222, 1.000000000000000000, 0.9999999999999997780, 1.000000000000000222, 0.9999999999999997780, 1.000000000000000444, 1.000000000000000222, 1.000000000000000000, 1.000000000000000222, 1.000000000000000222, 1.000000000000000000, 1.000000000000000000, 1.000000000000000000, 1.000000000000000000, 1.000000000000000000, 1.000000000000000000, 1.000000000000000000, 0.9999999999999997780, 1.000000000000000000, 0.9999999999999996669, 1.000000000000000444, 0.9999999999999996669, 1.000000000000000000, 1.000000000000000000, 0.9999999999999997780, 1.000000000000000444, 1.000000000000000000, 1.000000000000000000, 1.000000000000000000),
 ( 0.3333333333333334259, 0.3333333333333334259, 0.3333333333333333703, 0.3333333333333333703, 0.3333333333333334259, 0.3333333333333333703, 0.3333333333333333703, 0.3333333333333334259, 0.3333333333333333148, 0.3333333333333334814, 0.3333333333333332593, 0.3333333333333335369, 0.3333333333333333148, 0.3333333333333333703, 0.3333333333333334259, 0.3333333333333332593, 0.3333333333333333703, 0.3333333333333333703, 0.3333333333333334259, 0.3333333333333334814, 0.3333333333333333148, 0.3333333333333334259, 0.3333333333333333703, 0.3333333333333333703, 0.3333333333333333148, 0.3333333333333333703, 0.3333333333333334259, 0.3333333333333332038, 0.3333333333333334259, 0.3333333333333333703, 0.3333333333333334259, 0.3333333333333333703, 0.3333333333333333148, 0.3333333333333334259, 0.3333333333333334259, 0.3333333333333333703, 0.3333333333333334814, 0.3333333333333332593, 0.3333333333333334259, 0.3333333333333334259, 0.3333333333333333148, 0.3333333333333333703, 0.3333333333333333148, 0.3333333333333333703, 0.3333333333333333148, 0.3333333333333333703, 0.3333333333333333703, 0.3333333333333333703, 0.3333333333333333148, 0.3333333333333333148, 0.3333333333333334259, 0.3333333333333332593, 0.3333333333333333703, 0.3333333333333333703, 0.3333333333333333703, 0.3333333333333332593, 0.3333333333333334259, 0.3333333333333333148, 0.3333333333333333148, 0.3333333333333333703, 0.3333333333333333703, 0.3333333333333333703, 0.3333333333333334259, 0.3333333333333333148, 0.3333333333333334259, 0.3333333333333334259, 0.3333333333333333703, 0.3333333333333333703, 0.3333333333333333148, 0.3333333333333333703, 0.3333333333333333703, 0.3333333333333333148, 0.3333333333333333703, 0.3333333333333332593, 0.3333333333333334814, 0.3333333333333333148, 0.3333333333333333703, 0.3333333333333332593, 0.3333333333333335369, 0.3333333333333333703, 0.3333333333333333703, 0.3333333333333333703, 0.3333333333333334259, 0.3333333333333334259, 0.3333333333333333148, 0.3333333333333334259, 0.3333333333333333148, 0.3333333333333333703, 0.3333333333333335369, 0.3333333333333333148, 0.3333333333333334259, 0.3333333333333334814, 0.3333333333333333148, 0.3333333333333335369, 0.3333333333333332593, 0.3333333333333333703, 0.3333333333333333148, 0.3333333333333334259, 0.3333333333333333148, 0.3333333333333334814, 0.3333333333333333703, 0.3333333333333333148, 0.3333333333333333703, 0.3333333333333334259, 0.3333333333333333703, 0.3333333333333334259, 0.3333333333333332593, 0.3333333333333335924, 0.3333333333333333148, 0.3333333333333333148, 0.3333333333333334259, 0.3333333333333332593, 0.3333333333333333703, 0.3333333333333333148, 0.3333333333333335369, 0.3333333333333333703, 0.3333333333333333703, 0.3333333333333334259, 0.3333333333333334259, 0.3333333333333333703, 0.3333333333333333703, 0.3333333333333333703, 0.3333333333333333703, 0.3333333333333334259, 0.3333333333333333703, 0.3333333333333333703, 0.3333333333333333703, 0.3333333333333334259, 0.3333333333333333148, 0.3333333333333333703, 0.3333333333333333703, 0.3333333333333334259, 0.3333333333333333148, 0.3333333333333333703, 0.3333333333333333703, 0.3333333333333333703, 0.3333333333333333148, 0.3333333333333334259, 0.3333333333333333148, 0.3333333333333333703, 0.3333333333333334259, 0.3333333333333333703, 0.3333333333333333703, 0.3333333333333333703, 0.3333333333333333703, 0.3333333333333334259, 0.3333333333333334259, 0.3333333333333334259, 0.3333333333333333148, 0.3333333333333334259, 0.3333333333333333148, 0.3333333333333334259, 0.3333333333333334259, 0.3333333333333333703, 0.3333333333333333148, 0.3333333333333333703, 0.3333333333333333703, 0.3333333333333333148, 0.3333333333333334259, 0.3333333333333335369, 0.3333333333333333148, 0.3333333333333332593, 0.3333333333333334814, 0.3333333333333332593, 0.3333333333333333703, 0.3333333333333333703, 0.3333333333333333703, 0.3333333333333334259, 0.3333333333333334259, 0.3333333333333334259, 0.3333333333333335369, 0.3333333333333333703, 0.3333333333333333703, 0.3333333333333333703, 0.3333333333333334259, 0.3333333333333333703, 0.3333333333333333703, 0.3333333333333334259, 0.3333333333333333703, 0.3333333333333334259, 0.3333333333333332593, 0.3333333333333334259, 0.3333333333333334259, 0.3333333333333333148, 0.3333333333333333703, 0.3333333333333333703, 0.3333333333333333703, 0.3333333333333333703, 0.3333333333333334259, 0.3333333333333334259, 0.3333333333333334259, 0.3333333333333333148, 0.3333333333333333703, 0.3333333333333334259, 0.3333333333333332593, 0.3333333333333334814, 0.3333333333333333148, 0.3333333333333332593, 0.3333333333333335369, 0.3333333333333333148, 0.3333333333333333703, 0.3333333333333334259, 0.3333333333333333148, 0.3333333333333333703, 0.3333333333333334259, 0.3333333333333333148, 0.3333333333333335369, 0.3333333333333332593, 0.3333333333333333703, 0.3333333333333334259, 0.3333333333333333148, 0.3333333333333334259, 0.3333333333333333148, 0.3333333333333333703, 0.3333333333333333703, 0.3333333333333333703, 0.3333333333333333703, 0.3333333333333334259, 0.3333333333333332593, 0.3333333333333334259, 0.3333333333333334259, 0.3333333333333333703, 0.3333333333333333703, 0.3333333333333333148, 0.3333333333333334814, 0.3333333333333333703, 0.3333333333333332593, 0.3333333333333334259, 0.3333333333333334259, 0.3333333333333334259, 0.3333333333333333703, 0.3333333333333332038, 0.3333333333333335369, 0.3333333333333333148, 0.3333333333333333148, 0.3333333333333333703, 0.3333333333333333703, 0.3333333333333333703, 0.3333333333333334259, 0.3333333333333333148, 0.3333333333333334814, 0.3333333333333333148, 0.3333333333333333703, 0.3333333333333334259, 0.3333333333333333148, 0.3333333333333334259, 0.3333333333333333148, 0.3333333333333334259, 0.3333333333333333148, 0.3333333333333333703, 0.3333333333333333703, 0.3333333333333334259, 0.3333333333333333703, 0.3333333333333333148, 0.3333333333333334814, 0.3333333333333334259, 0.3333333333333333703, 0.3333333333333333148, 0.3333333333333334259, 0.3333333333333333703, 0.3333333333333333703, 0.3333333333333334259, 0.3333333333333333703, 0.3333333333333334814, 0.3333333333333333148, 0.3333333333333334259, 0.3333333333333333703, 0.3333333333333334259, 0.3333333333333333148, 0.3333333333333333703, 0.3333333333333334259, 0.3333333333333333703, 0.3333333333333334259, 0.3333333333333332593, 0.3333333333333333703, 0.3333333333333332593, 0.3333333333333334259, 0.3333333333333333703, 0.3333333333333334259, 0.3333333333333334259, 0.3333333333333333148, 0.3333333333333333148, 0.3333333333333334259, 0.3333333333333333148, 0.3333333333333333148, 0.3333333333333333703, 0.3333333333333333703, 0.3333333333333334259, 0.3333333333333333703, 0.3333333333333334814, 0.3333333333333332593, 0.3333333333333334259, 0.3333333333333333703, 0.3333333333333333703, 0.3333333333333334259, 0.3333333333333333703, 0.3333333333333333703, 0.3333333333333334259, 0.3333333333333334259, 0.3333333333333334814, 0.3333333333333333148, 0.3333333333333333148, 0.3333333333333333703, 0.3333333333333333148, 0.3333333333333334259, 0.3333333333333333703, 0.3333333333333333148, 0.3333333333333332593, 0.3333333333333334259, 0.3333333333333334259, 0.3333333333333333148, 0.3333333333333333703, 0.3333333333333334259, 0.3333333333333333148, 0.3333333333333334259, 0.3333333333333334259, 0.3333333333333334814, 0.3333333333333333148, 0.3333333333333333703, 0.3333333333333332593, 0.3333333333333334814, 0.3333333333333333703, 0.3333333333333332593, 0.3333333333333334814, 0.3333333333333332593, 0.3333333333333334259, 0.3333333333333333703, 0.3333333333333333148, 0.3333333333333333148, 0.3333333333333334259, 0.3333333333333333703, 0.3333333333333333703, 0.3333333333333333703, 0.3333333333333333703, 0.3333333333333334259, 0.3333333333333333148, 0.3333333333333334259, 0.3333333333333332038, 0.3333333333333334259, 0.3333333333333333148, 0.3333333333333334814, 0.3333333333333333703, 0.3333333333333333703, 0.3333333333333334259, 0.3333333333333333148, 0.3333333333333333703, 0.3333333333333333703, 0.3333333333333333703, 0.3333333333333333703, 0.3333333333333333703, 0.3333333333333334259, 0.3333333333333333148, 0.3333333333333334814, 0.3333333333333334259, 0.3333333333333332593, 0.3333333333333333703, 0.3333333333333333703, 0.3333333333333333703, 0.3333333333333333703, 0.3333333333333333703, 0.3333333333333334259, 0.3333333333333333148, 0.3333333333333333703, 0.3333333333333334259, 0.3333333333333335369, 0.3333333333333333148, 0.3333333333333333703, 0.3333333333333334259, 0.3333333333333333703, 0.3333333333333333703, 0.3333333333333333703, 0.3333333333333333703, 0.3333333333333333703, 0.3333333333333333703, 0.3333333333333333703, 0.3333333333333333703, 0.3333333333333334259, 0.3333333333333332593, 0.3333333333333334814, 0.3333333333333332593, 0.3333333333333334259, 0.3333333333333333703, 0.3333333333333333703, 0.3333333333333334814, 0.3333333333333333148, 0.3333333333333333703, 0.3333333333333333703),
 ( 0.3333333333333334259, 0.3333333333333334259, 0.3333333333333333703, 0.3333333333333333703, 0.3333333333333334259, 0.3333333333333333703, 0.3333333333333333703, 0.3333333333333334259, 0.3333333333333333148, 0.3333333333333334814, 0.3333333333333332593, 0.3333333333333335369, 0.3333333333333333148, 0.3333333333333333703, 0.3333333333333334259, 0.3333333333333332593, 0.3333333333333333703, 0.3333333333333333703, 0.3333333333333334259, 0.3333333333333334814, 0.3333333333333333148, 0.3333333333333334259, 0.3333333333333333703, 0.3333333333333333703, 0.3333333333333333148, 0.3333333333333333703, 0.3333333333333334259, 0.3333333333333332038, 0.3333333333333334259, 0.3333333333333333703, 0.3333333333333334259, 0.3333333333333333703, 0.3333333333333333148, 0.3333333333333334259, 0.3333333333333334259, 0.3333333333333333703, 0.3333333333333334814, 0.3333333333333332593, 0.3333333333333334259, 0.3333333333333334259, 0.3333333333333333148, 0.3333333333333333703, 0.3333333333333333148, 0.3333333333333333703, 0.3333333333333333148, 0.3333333333333333703, 0.3333333333333333703, 0.3333333333333333703, 0.3333333333333333148, 0.3333333333333333148, 0.3333333333333334259, 0.3333333333333332593, 0.3333333333333333703, 0.3333333333333333703, 0.3333333333333333703, 0.3333333333333332593, 0.3333333333333334259, 0.3333333333333333148, 0.3333333333333333148, 0.3333333333333333703, 0.3333333333333333703, 0.3333333333333333703, 0.3333333333333334259, 0.3333333333333333148, 0.3333333333333334259, 0.3333333333333334259, 0.3333333333333333703, 0.3333333333333333703, 0.3333333333333333148, 0.3333333333333333703, 0.3333333333333333703, 0.3333333333333333148, 0.3333333333333333703, 0.3333333333333332593, 0.3333333333333334814, 0.3333333333333333148, 0.3333333333333333703, 0.3333333333333332593, 0.3333333333333335369, 0.3333333333333333703, 0.3333333333333333703, 0.3333333333333333703, 0.3333333333333334259, 0.3333333333333334259, 0.3333333333333333148, 0.3333333333333334259, 0.3333333333333333148, 0.3333333333333333703, 0.3333333333333335369, 0.3333333333333333148, 0.3333333333333334259, 0.3333333333333334814, 0.3333333333333333148, 0.3333333333333335369, 0.3333333333333332593, 0.3333333333333333703, 0.3333333333333333148, 0.3333333333333334259, 0.3333333333333333148, 0.3333333333333334814, 0.3333333333333333703, 0.3333333333333333148, 0.3333333333333333703, 0.3333333333333334259, 0.3333333333333333703, 0.3333333333333334259, 0.3333333333333332593, 0.3333333333333335924, 0.3333333333333333148, 0.3333333333333333148, 0.3333333333333334259, 0.3333333333333332593, 0.3333333333333333703, 0.3333333333333333148, 0.3333333333333335369, 0.3333333333333333703, 0.3333333333333333703, 0.3333333333333334259, 0.3333333333333334259, 0.3333333333333333703, 0.3333333333333333703, 0.3333333333333333703, 0.3333333333333333703, 0.3333333333333334259, 0.3333333333333333703, 0.3333333333333333703, 0.3333333333333333703, 0.3333333333333334259, 0.3333333333333333148, 0.3333333333333333703, 0.3333333333333333703, 0.3333333333333334259, 0.3333333333333333148, 0.3333333333333333703, 0.3333333333333333703, 0.3333333333333333703, 0.3333333333333333148, 0.3333333333333334259, 0.3333333333333333148, 0.3333333333333333703, 0.3333333333333334259, 0.3333333333333333703, 0.3333333333333333703, 0.3333333333333333703, 0.3333333333333333703, 0.3333333333333334259, 0.3333333333333334259, 0.3333333333333334259, 0.3333333333333333148, 0.3333333333333334259, 0.3333333333333333148, 0.3333333333333334259, 0.3333333333333334259, 0.3333333333333333703, 0.3333333333333333148, 0.3333333333333333703, 0.3333333333333333703, 0.3333333333333333148, 0.3333333333333334259, 0.3333333333333335369, 0.3333333333333333148, 0.3333333333333332593, 0.3333333333333334814, 0.3333333333333332593, 0.3333333333333333703, 0.3333333333333333703, 0.3333333333333333703, 0.3333333333333334259, 0.3333333333333334259, 0.3333333333333334259, 0.3333333333333335369, 0.3333333333333333703, 0.3333333333333333703, 0.3333333333333333703, 0.3333333333333334259, 0.3333333333333333703, 0.3333333333333333703, 0.3333333333333334259, 0.3333333333333333703, 0.3333333333333334259, 0.3333333333333332593, 0.3333333333333334259, 0.3333333333333334259, 0.3333333333333333148, 0.3333333333333333703, 0.3333333333333333703, 0.3333333333333333703, 0.3333333333333333703, 0.3333333333333334259, 0.3333333333333334259, 0.3333333333333334259, 0.3333333333333333148, 0.3333333333333333703, 0.3333333333333334259, 0.3333333333333332593, 0.3333333333333334814, 0.3333333333333333148, 0.3333333333333332593, 0.3333333333333335369, 0.3333333333333333148, 0.3333333333333333703, 0.3333333333333334259, 0.3333333333333333148, 0.3333333333333333703, 0.3333333333333334259, 0.3333333333333333148, 0.3333333333333335369, 0.3333333333333332593, 0.3333333333333333703, 0.3333333333333334259, 0.3333333333333333148, 0.3333333333333334259, 0.3333333333333333148, 0.3333333333333333703, 0.3333333333333333703, 0.3333333333333333703, 0.3333333333333333703, 0.3333333333333334259, 0.3333333333333332593, 0.3333333333333334259, 0.3333333333333334259, 0.3333333333333333703, 0.3333333333333333703, 0.3333333333333333148, 0.3333333333333334814, 0.3333333333333333703, 0.3333333333333332593, 0.3333333333333334259, 0.3333333333333334259, 0.3333333333333334259, 0.3333333333333333703, 0.3333333333333332038, 0.3333333333333335369, 0.3333333333333333148, 0.3333333333333333148, 0.3333333333333333703, 0.3333333333333333703, 0.3333333333333333703, 0.3333333333333334259, 0.3333333333333333148, 0.3333333333333334814, 0.3333333333333333148, 0.3333333333333333703, 0.3333333333333334259, 0.3333333333333333148, 0.3333333333333334259, 0.3333333333333333148, 0.3333333333333334259, 0.3333333333333333148, 0.3333333333333333703, 0.3333333333333333703, 0.3333333333333334259, 0.3333333333333333703, 0.3333333333333333148, 0.3333333333333334814, 0.3333333333333334259, 0.3333333333333333703, 0.3333333333333333148, 0.3333333333333334259, 0.3333333333333333703, 0.3333333333333333703, 0.3333333333333334259, 0.3333333333333333703, 0.3333333333333334814, 0.3333333333333333148, 0.3333333333333334259, 0.3333333333333333703, 0.3333333333333334259, 0.3333333333333333148, 0.3333333333333333703, 0.3333333333333334259, 0.3333333333333333703, 0.3333333333333334259, 0.3333333333333332593, 0.3333333333333333703, 0.3333333333333332593, 0.3333333333333334259, 0.3333333333333333703, 0.3333333333333334259, 0.3333333333333334259, 0.3333333333333333148, 0.3333333333333333148, 0.3333333333333334259, 0.3333333333333333148, 0.3333333333333333148, 0.3333333333333333703, 0.3333333333333333703, 0.3333333333333334259, 0.3333333333333333703, 0.3333333333333334814, 0.3333333333333332593, 0.3333333333333334259, 0.3333333333333333703, 0.3333333333333333703, 0.3333333333333334259, 0.3333333333333333703, 0.3333333333333333703, 0.3333333333333334259, 0.3333333333333334259, 0.3333333333333334814, 0.3333333333333333148, 0.3333333333333333148, 0.3333333333333333703, 0.3333333333333333148, 0.3333333333333334259, 0.3333333333333333703, 0.3333333333333333148, 0.3333333333333332593, 0.3333333333333334259, 0.3333333333333334259, 0.3333333333333333148, 0.3333333333333333703, 0.3333333333333334259, 0.3333333333333333148, 0.3333333333333334259, 0.3333333333333334259, 0.3333333333333334814, 0.3333333333333333148, 0.3333333333333333703, 0.3333333333333332593, 0.3333333333333334814, 0.3333333333333333703, 0.3333333333333332593, 0.3333333333333334814, 0.3333333333333332593, 0.3333333333333334259, 0.3333333333333333703, 0.3333333333333333148, 0.3333333333333333148, 0.3333333333333334259, 0.3333333333333333703, 0.3333333333333333703, 0.3333333333333333703, 0.3333333333333333703, 0.3333333333333334259, 0.3333333333333333148, 0.3333333333333334259, 0.3333333333333332038, 0.3333333333333334259, 0.3333333333333333148, 0.3333333333333334814, 0.3333333333333333703, 0.3333333333333333703, 0.3333333333333334259, 0.3333333333333333148, 0.3333333333333333703, 0.3333333333333333703, 0.3333333333333333703, 0.3333333333333333703, 0.3333333333333333703, 0.3333333333333334259, 0.3333333333333333148, 0.3333333333333334814, 0.3333333333333334259, 0.3333333333333332593, 0.3333333333333333703, 0.3333333333333333703, 0.3333333333333333703, 0.3333333333333333703, 0.3333333333333333703, 0.3333333333333334259, 0.3333333333333333148, 0.3333333333333333703, 0.3333333333333334259, 0.3333333333333335369, 0.3333333333333333148, 0.3333333333333333703, 0.3333333333333334259, 0.3333333333333333703, 0.3333333333333333703, 0.3333333333333333703, 0.3333333333333333703, 0.3333333333333333703, 0.3333333333333333703, 0.3333333333333333703, 0.3333333333333333703, 0.3333333333333334259, 0.3333333333333332593, 0.3333333333333334814, 0.3333333333333332593, 0.3333333333333334259, 0.3333333333333333703, 0.3333333333333333703, 0.3333333333333334814, 0.3333333333333333148, 0.3333333333333333703, 0.3333333333333333703),
 ( 1.000000000000000222, 1.000000000000000222, 0.9999999999999997780, 1.000000000000000222, 1.000000000000000000, 1.000000000000000000, 0.9999999999999997780, 1.000000000000000000, 1.000000000000000000, 1.000000000000000000, 1.000000000000000000, 1.000000000000000222, 1.000000000000000000, 1.000000000000000000, 1.000000000000000222, 0.9999999999999994449, 1.000000000000000222, 1.000000000000000000, 0.9999999999999997780, 1.000000000000000444, 1.000000000000000000, 1.000000000000000222, 1.000000000000000000, 1.000000000000000000, 0.9999999999999996669, 1.000000000000000000, 1.000000000000000222, 0.9999999999999996669, 1.000000000000000222, 1.000000000000000000, 1.000000000000000222, 1.000000000000000000, 1.000000000000000222, 0.9999999999999997780, 1.000000000000000444, 1.000000000000000000, 1.000000000000000222, 0.9999999999999997780, 1.000000000000000222, 1.000000000000000000, 1.000000000000000000, 0.9999999999999997780, 1.000000000000000000, 0.9999999999999997780, 1.000000000000000000, 0.9999999999999997780, 1.000000000000000000, 1.000000000000000000, 0.9999999999999997780, 1.000000000000000000, 1.000000000000000222, 0.9999999999999996669, 1.000000000000000000, 1.000000000000000000, 1.000000000000000222, 0.9999999999999997780, 1.000000000000000444, 1.000000000000000000, 0.9999999999999997780, 1.000000000000000000, 1.000000000000000000, 1.000000000000000000, 1.000000000000000222, 1.000000000000000000, 1.000000000000000000, 1.000000000000000222, 1.000000000000000000, 1.000000000000000000, 0.9999999999999997780, 1.000000000000000222, 1.000000000000000000, 0.9999999999999997780, 1.000000000000000000, 1.000000000000000000, 1.000000000000000000, 1.000000000000000000, 1.000000000000000222, 0.9999999999999996669, 1.000000000000000444, 0.9999999999999996669, 1.000000000000000000, 0.9999999999999996669, 1.000000000000000444, 1.000000000000000000, 1.000000000000000000, 1.000000000000000222, 1.000000000000000000, 1.000000000000000000, 1.000000000000000222, 0.9999999999999997780, 1.000000000000000000, 1.000000000000000444, 0.9999999999999997780, 1.000000000000000444, 0.9999999999999997780, 1.000000000000000000, 1.000000000000000222, 1.000000000000000000, 0.9999999999999997780, 1.000000000000000222, 1.000000000000000222, 0.9999999999999997780, 1.000000000000000000, 1.000000000000000222, 0.9999999999999997780, 1.000000000000000444, 0.9999999999999997780, 1.000000000000000444, 0.9999999999999997780, 1.000000000000000000, 1.000000000000000222, 0.9999999999999996669, 1.000000000000000000, 1.000000000000000000, 1.000000000000000444, 1.000000000000000222, 0.9999999999999997780, 1.000000000000000222, 1.000000000000000222, 1.000000000000000000, 1.000000000000000222, 0.9999999999999997780, 1.000000000000000000, 1.000000000000000222, 0.9999999999999996669, 1.000000000000000000, 1.000000000000000000, 1.000000000000000000, 1.000000000000000000, 1.000000000000000000, 1.000000000000000000, 1.000000000000000000, 0.9999999999999997780, 1.000000000000000222, 0.9999999999999997780, 1.000000000000000000, 0.9999999999999997780, 1.000000000000000222, 1.000000000000000000, 1.000000000000000000, 1.000000000000000000, 1.000000000000000222, 0.9999999999999997780, 0.9999999999999997780, 1.000000000000000222, 1.000000000000000222, 1.000000000000000000, 1.000000000000000444, 0.9999999999999996669, 1.000000000000000444, 0.9999999999999997780, 1.000000000000000222, 1.000000000000000000, 1.000000000000000000, 1.000000000000000000, 1.000000000000000222, 0.9999999999999997780, 0.9999999999999997780, 1.000000000000000444, 1.000000000000000444, 0.9999999999999997780, 1.000000000000000000, 1.000000000000000000, 1.000000000000000000, 1.000000000000000222, 1.000000000000000000, 1.000000000000000000, 1.000000000000000222, 1.000000000000000222, 1.000000000000000000, 1.000000000000000444, 1.000000000000000000, 1.000000000000000222, 1.000000000000000000, 1.000000000000000000, 1.000000000000000444, 1.000000000000000000, 1.000000000000000222, 1.000000000000000000, 1.000000000000000222, 0.9999999999999997780, 1.000000000000000222, 1.000000000000000222, 1.000000000000000000, 0.9999999999999996669, 1.000000000000000222, 1.000000000000000000, 1.000000000000000000, 1.000000000000000222, 1.000000000000000222, 1.000000000000000222, 0.9999999999999997780, 1.000000000000000000, 1.000000000000000222, 1.000000000000000000, 1.000000000000000000, 1.000000000000000000, 0.9999999999999996669, 1.000000000000000444, 1.000000000000000222, 0.9999999999999996669, 1.000000000000000444, 1.000000000000000000, 1.000000000000000000, 1.000000000000000222, 0.9999999999999997780, 1.000000000000000444, 0.9999999999999997780, 0.9999999999999997780, 1.000000000000000444, 0.9999999999999997780, 1.000000000000000222, 1.000000000000000000, 1.000000000000000000, 1.000000000000000000, 0.9999999999999997780, 1.000000000000000000, 1.000000000000000222, 0.9999999999999996669, 1.000000000000000222, 1.000000000000000000, 1.000000000000000222, 0.9999999999999996669, 0.9999999999999997780, 1.000000000000000444, 0.9999999999999997780, 0.9999999999999997780, 1.000000000000000000, 1.000000000000000222, 1.000000000000000000, 1.000000000000000000, 0.9999999999999996669, 1.000000000000000222, 1.000000000000000000, 0.9999999999999997780, 1.000000000000000000, 1.000000000000000000, 0.9999999999999997780, 1.000000000000000444, 0.9999999999999996669, 1.000000000000000444, 0.9999999999999997780, 1.000000000000000000, 1.000000000000000222, 0.9999999999999997780, 1.000000000000000222, 1.000000000000000222, 0.9999999999999997780, 1.000000000000000000, 1.000000000000000000, 1.000000000000000000, 1.000000000000000222, 1.000000000000000000, 1.000000000000000000, 1.000000000000000222, 1.000000000000000222, 1.000000000000000000, 1.000000000000000000, 1.000000000000000222, 0.9999999999999997780, 1.000000000000000000, 1.000000000000000222, 1.000000000000000000, 1.000000000000000222, 0.9999999999999997780, 1.000000000000000222, 0.9999999999999997780, 1.000000000000000222, 0.9999999999999997780, 1.000000000000000222, 1.000000000000000000, 1.000000000000000000, 1.000000000000000444, 0.9999999999999996669, 1.000000000000000222, 0.9999999999999997780, 1.000000000000000000, 1.000000000000000222, 1.000000000000000000, 1.000000000000000222, 0.9999999999999997780, 0.9999999999999997780, 1.000000000000000000, 0.9999999999999997780, 1.000000000000000000, 1.000000000000000000, 1.000000000000000222, 1.000000000000000000, 1.000000000000000000, 1.000000000000000222, 1.000000000000000000, 1.000000000000000000, 1.000000000000000000, 1.000000000000000000, 0.9999999999999997780, 1.000000000000000222, 1.000000000000000222, 0.9999999999999997780, 1.000000000000000444, 1.000000000000000444, 0.9999999999999997780, 1.000000000000000000, 0.9999999999999997780, 1.000000000000000000, 1.000000000000000000, 1.000000000000000000, 1.000000000000000000, 0.9999999999999997780, 1.000000000000000222, 1.000000000000000000, 0.9999999999999997780, 1.000000000000000222, 1.000000000000000000, 1.000000000000000000, 1.000000000000000000, 1.000000000000000444, 1.000000000000000000, 0.9999999999999997780, 0.9999999999999997780, 0.9999999999999997780, 1.000000000000000222, 1.000000000000000222, 0.9999999999999996669, 1.000000000000000222, 0.9999999999999997780, 1.000000000000000222, 1.000000000000000000, 1.000000000000000000, 0.9999999999999996669, 1.000000000000000222, 1.000000000000000222, 1.000000000000000000, 1.000000000000000000, 1.000000000000000222, 0.9999999999999997780, 1.000000000000000000, 1.000000000000000222, 0.9999999999999994449, 1.000000000000000222, 1.000000000000000000, 1.000000000000000222, 0.9999999999999997780, 1.000000000000000000, 1.000000000000000000, 0.9999999999999997780, 1.000000000000000000, 1.000000000000000222, 0.9999999999999997780, 1.000000000000000000, 1.000000000000000000, 1.000000000000000000, 1.000000000000000000, 1.000000000000000222, 1.000000000000000000, 0.9999999999999996669, 0.9999999999999996669, 1.000000000000000222, 0.9999999999999997780, 1.000000000000000222, 1.000000000000000000, 0.9999999999999997780, 1.000000000000000222, 0.9999999999999997780, 1.000000000000000444, 1.000000000000000222, 1.000000000000000000, 1.000000000000000222, 1.000000000000000222, 1.000000000000000000, 1.000000000000000000, 1.000000000000000000, 1.000000000000000000, 1.000000000000000000, 1.000000000000000000, 1.000000000000000000, 0.9999999999999997780, 1.000000000000000000, 0.9999999999999996669, 1.000000000000000444, 0.9999999999999996669, 1.000000000000000000, 1.000000000000000000, 0.9999999999999997780, 1.000000000000000444, 1.000000000000000000, 1.000000000000000000, 1.000000000000000000) ) ) 
 REPRESENTATION_ITEM ( '' )  SURFACE ( )  );
#180106 = CARTESIAN_POINT ( 'NONE',  ( 6.670655732516626912, 7.629137130509076492, 2.426260288887295502 ) ) ;
#180107 = CARTESIAN_POINT ( 'NONE',  ( -0.6823417656250003738, -0.03229166632524871350, -1.181850606188749264 ) ) ;
#180108 = CARTESIAN_POINT ( 'NONE',  ( 5.992340707560160240, 7.053780915984068756, 1.082531754730558626 ) ) ;
#180109 = CARTESIAN_POINT ( 'NONE',  ( -8.351459436338030784, 11.72682452816096976, -1.082531754730543971 ) ) ;
#180110 = CARTESIAN_POINT ( 'NONE',  ( 0.2862814217290919894, -1.017545141758866789, 1.907252267444502269 ) ) ;
#180111 = CARTESIAN_POINT ( 'NONE',  ( -4.773352600463090845, 7.726605912919016106, 1.199719254218452935 ) ) ;
#180112 = CARTESIAN_POINT ( 'NONE',  ( 3.770049233051776749, 6.556085317605844232, 1.199719254218451159 ) ) ;
#180113 = CARTESIAN_POINT ( 'NONE',  ( 2.168725436055967570, -1.667931858681595880, -0.7425449061374129744 ) ) ;
#180114 = CARTESIAN_POINT ( 'NONE',  ( -2.578021764892882040, 6.159442492350315490, 0.7998128361456341429 ) ) ;
#180115 = CARTESIAN_POINT ( 'NONE',  ( 3.768406797884563453, -1.226484811506942219, 1.352366043108323979 ) ) ;
#180116 = CARTESIAN_POINT ( 'NONE',  ( 9.259438961641526689, 13.05523824266862398, 8.991576184352215506 ) ) ;
#180117 = ORIENTED_EDGE ( 'NONE', *, *, #129667, .T. ) ;
#180118 = CARTESIAN_POINT ( 'NONE',  ( 3.279706249791583872, -1.898816934168370496, 0.5228806403664593150 ) ) ;
#180119 = VERTEX_POINT ( 'NONE', #82358 ) ;
#180120 = CARTESIAN_POINT ( 'NONE',  ( 4.493657767381210810, -1.941711754461509232, -0.04422589797668275563 ) ) ;
#180121 = VERTEX_POINT ( 'NONE', #181983 ) ;
#180122 = CARTESIAN_POINT ( 'NONE',  ( -5.101610940492132151, 9.173906207207963348, -0.7998128361456362523 ) ) ;
#180124 = CARTESIAN_POINT ( 'NONE',  ( 5.414351406770180120, -2.120778210838507150, 0.002142078463891750485 ) ) ;
#180123 = CARTESIAN_POINT ( 'NONE',  ( 6.964048179274811012, 8.153752959689313684, 1.199719254218452047 ) ) ;
#180125 = CARTESIAN_POINT ( 'NONE',  ( 11.00592740523952173, 9.989797575316798017, 1.444008943503716225 ) ) ;
#180126 = CARTESIAN_POINT ( 'NONE',  ( 2.578645926699867363, -1.317302948579327504, 1.386430337501590282 ) ) ;
#180127 = CARTESIAN_POINT ( 'NONE',  ( 5.490304984925487908, 6.429369728800919503, -1.257259817782523381 ) ) ;
#180128 = CARTESIAN_POINT ( 'NONE',  ( -9.496663239506002441, -6.863887327018314721, -0.01979922387980589255 ) ) ;
#180129 = ORIENTED_EDGE ( 'NONE', *, *, #126913, .F. ) ;
#180130 = CARTESIAN_POINT ( 'NONE',  ( 4.041212305325117882, 6.872442235258051646, -1.199719254218448494 ) ) ;
#180131 = CARTESIAN_POINT ( 'NONE',  ( 4.494793336055456834, -1.953237823851183164, -0.4868166104980836684 ) ) ;
#180132 = CARTESIAN_POINT ( 'NONE',  ( -11.88168329227127096, 11.37999999999998302, 1.685799833707126050 ) ) ;
#180133 = CARTESIAN_POINT ( 'NONE',  ( 5.566980414702134894, -1.652319403193935887, -0.7768266693391965294 ) ) ;
#180134 = CARTESIAN_POINT ( 'NONE',  ( 0.4849360239999983002, 1.980737741294085419, 0.6024896509310637693 ) ) ;
#180135 = CARTESIAN_POINT ( 'NONE',  ( -7.022760382198764084, 11.13704484596649635, 0.7216878364870458196 ) ) ;
#180136 = CARTESIAN_POINT ( 'NONE',  ( -6.615421019548638704, 6.757903343899189785, 0.08170615477586136433 ) ) ;
#180137 = FACE_BOUND ( 'NONE', #113872, .T. ) ;
#180138 = CARTESIAN_POINT ( 'NONE',  ( 5.313307075269409374, -0.2735208697075517947, 1.850433306854900817 ) ) ;
#180139 = CARTESIAN_POINT ( 'NONE',  ( 7.786460292950004636, 7.978625184730144149, 1.040834085586084257E-14 ) ) ;
#180140 = CARTESIAN_POINT ( 'NONE',  ( -3.924195396151603177, 6.665646164563756138, 1.199719254218464037 ) ) ;
#180142 = EDGE_CURVE ( 'NONE', #33049, #138365, #43139, .T. ) ;
#180141 = STYLED_ITEM ( 'NONE', ( #6723 ), #163490 ) ;
#180143 = CARTESIAN_POINT ( 'NONE',  ( 0.6823417656249969321, 10.08854166700806587, -1.181850606188757036 ) ) ;
#180144 = CARTESIAN_POINT ( 'NONE',  ( -5.599681137644054729, 6.491715067794862293, 1.199719254218450271 ) ) ;
#180146 = CARTESIAN_POINT ( 'NONE',  ( -8.106849506328558164, 8.422688943663599659, 0.000000000000000000 ) ) ;
#180145 = CARTESIAN_POINT ( 'NONE',  ( 3.816783937446950770, 4.411668334231586996, 1.199719254218464037 ) ) ;
#180147 = CARTESIAN_POINT ( 'NONE',  ( -5.289089322662584358, 5.343228095960675716, 0.000000000000000000 ) ) ;
#180148 = CARTESIAN_POINT ( 'NONE',  ( -4.934277840369690971, 7.844075682818238526, -1.199719254218452047 ) ) ;
#180149 = CARTESIAN_POINT ( 'NONE',  ( 0.8661811918178536907, -2.060611401584189650, 0.1992402130865863485 ) ) ;
#180150 = CARTESIAN_POINT ( 'NONE',  ( 2.812237032231167611, 1.173781612916646289, -1.761886306039317285 ) ) ;
#180151 = CARTESIAN_POINT ( 'NONE',  ( 9.348510611822643313, 10.86534945433664134, 1.199719254218453823 ) ) ;
#180152 = DIRECTION ( 'NONE',  ( -5.551115123125758667E-17, 0.000000000000000000, 1.000000000000000000 ) ) ;
#180153 = CARTESIAN_POINT ( 'NONE',  ( 6.983263157960365675, -0.006178392973848687020, 2.053544886540019210 ) ) ;
#180154 = CARTESIAN_POINT ( 'NONE',  ( 4.388746605030885206, 7.362284722717403085, 1.177686187499202619 ) ) ;
#180155 = CARTESIAN_POINT ( 'NONE',  ( 5.504247177468186258, 6.484338464210099851, 1.082531754730558626 ) ) ;
#180157 = DIRECTION ( 'NONE',  ( -7.387867266669436732E-31, -1.000000000000000000, 8.546850786086437571E-32 ) ) ;
#180156 = CARTESIAN_POINT ( 'NONE',  ( 1.001543065824772753E-15, -3.062499999999998668, 4.012584370867899430 ) ) ;
#180158 = CARTESIAN_POINT ( 'NONE',  ( 2.291363848578463980, 1.773334254936178356, 1.452501744581054632 ) ) ;
#180159 = CARTESIAN_POINT ( 'NONE',  ( 0.02954982209854747910, -1.120125052174587577, -1.442194003765177035 ) ) ;
#180160 = CARTESIAN_POINT ( 'NONE',  ( 1.916128293556786044, -1.911906470838855343, 0.05044092668918254141 ) ) ;
#180161 = ORIENTED_EDGE ( 'NONE', *, *, #183755, .T. ) ;
#180162 = CARTESIAN_POINT ( 'NONE',  ( 6.439759776366758892, 10.45687747249582955, 0.7216878364870438212 ) ) ;
#180163 = EDGE_CURVE ( 'NONE', #193155, #166389, #195257, .T. ) ;
#180164 = CARTESIAN_POINT ( 'NONE',  ( 1.213140692357208117, 1.643459361250454442, -1.162501220127802437 ) ) ;
#180165 = CARTESIAN_POINT ( 'NONE',  ( 1.024179675629211861, 0.9620134025654383247, 1.709582039726687652 ) ) ;
#180166 = CARTESIAN_POINT ( 'NONE',  ( -8.272446282632566650, 12.80293776304669962, 0.7998128361456481317 ) ) ;
#180167 = CARTESIAN_POINT ( 'NONE',  ( -8.064402442030170093, 8.302891025323665630, 0.7998128361456602331 ) ) ;
#180168 = CARTESIAN_POINT ( 'NONE',  ( -11.91807834161487634, 8.018667342336753379, 1.063137970766440121 ) ) ;
#180170 = CARTESIAN_POINT ( 'NONE',  ( 1.973191454406374890, 1.694654629526294087, -0.5103889506637182549 ) ) ;
#180169 = CARTESIAN_POINT ( 'NONE',  ( 4.171883282844288665, -1.203828960760118694, 1.709054251895093746 ) ) ;
#180171 = CARTESIAN_POINT ( 'NONE',  ( 0.7500000000000006661, 12.08333333333333570, 1.299038105676657340 ) ) ;
#180173 = CARTESIAN_POINT ( 'NONE',  ( 5.085981902069889315, -2.274473487728204013, -0.2844877896996683142 ) ) ;
#180172 = CARTESIAN_POINT ( 'NONE',  ( -11.95753012856830644, 7.932397174992964928, -1.041636101723666163 ) ) ;
#180174 = CARTESIAN_POINT ( 'NONE',  ( 4.909954989264024405, 1.196826376938535219, -1.263709391550037031 ) ) ;
#180175 = CARTESIAN_POINT ( 'NONE',  ( 7.404724451357931336, 11.79059562655963056, 0.7998128361456462443 ) ) ;
#180176 = CARTESIAN_POINT ( 'NONE',  ( -7.100579091573050228, -6.583980363594990948, 6.484567079770452658 ) ) ;
#180177 = CARTESIAN_POINT ( 'NONE',  ( 4.094866968876837987, 0.9280426781237434142, -1.464329598137555477 ) ) ;
#180178 = B_SPLINE_CURVE_WITH_KNOTS ( 'NONE', 3,
 ( #126111, #31480, #131164, #16248, #17318, #198209 ),
 .UNSPECIFIED., .F., .F.,
 ( 4, 2, 4 ),
 ( 0.000000000000000000, 0.0002835903134653046712, 0.0005671806269306093424 ),
 .UNSPECIFIED. ) ;
#180179 =( BOUNDED_SURFACE ( )  B_SPLINE_SURFACE ( 3, 2, ( 
 ( #206659, #87592, #107103 ),
 ( #6313, #187212, #153664 ),
 ( #7382, #72387, #90809 ),
 ( #188277, #104924, #203439 ),
 ( #207729, #59352, #190407 ),
 ( #156873, #74547, #125508 ),
 ( #38841, #157943, #139563 ),
 ( #8459, #172048, #103846 ) ),
 .UNSPECIFIED., .F., .F., .T. ) 
 B_SPLINE_SURFACE_WITH_KNOTS ( ( 4, 2, 2, 4 ),
 ( 3, 3 ),
 ( 0.000000000000000000, 0.0004924884914732687849, 0.0007387327372099031231, 0.0009849769829465375697 ),
 ( 0.000000000000000000, 1.000000000000000000 ),
 .UNSPECIFIED. ) 
 GEOMETRIC_REPRESENTATION_ITEM ( )  RATIONAL_B_SPLINE_SURFACE ( (
 ( 1.000000000000000000, 0.7045118851637611757, 1.000000000000000000),
 ( 1.000000000000000000, 0.7593505504064838041, 1.000000000000000000),
 ( 1.000000000000000000, 0.8104906253032566621, 1.000000000000000000),
 ( 1.000000000000000000, 0.8722646935501406906, 1.000000000000000000),
 ( 1.000000000000000000, 0.8905178607896868659, 1.000000000000000000),
 ( 1.000000000000000000, 0.9170530604351515569, 1.000000000000000000),
 ( 1.000000000000000000, 0.9248184710078943827, 1.000000000000000000),
 ( 1.000000000000000000, 0.9238795325112871826, 1.000000000000000000) ) ) 
 REPRESENTATION_ITEM ( '' )  SURFACE ( )  );
#180180 = AXIS2_PLACEMENT_3D ( 'NONE', #94980, #211886, #126472 ) ;
#180181 = CARTESIAN_POINT ( 'NONE',  ( 4.932167329841075976, 1.246153044254302289, 1.777787927081382779 ) ) ;
#180182 = CARTESIAN_POINT ( 'NONE',  ( 4.518945272056516416, 4.166524327021037699, 0.7998128361456341429 ) ) ;
#180183 = CARTESIAN_POINT ( 'NONE',  ( 5.981657729715996297, -0.6748525008196132324, 1.900413905137773529 ) ) ;
#180184 = CARTESIAN_POINT ( 'NONE',  ( 0.4062500000042400528, 1.895863743059760909, -0.7852924748300097457 ) ) ;
#180185 = AXIS2_PLACEMENT_3D ( 'NONE', #193826, #162420, #212198 ) ;
#180186 = CARTESIAN_POINT ( 'NONE',  ( -1.500000000000011324, 5.660416667349481123, -0.8660254037844313801 ) ) ;
#180187 = CARTESIAN_POINT ( 'NONE',  ( 3.434515876041916105, 1.879162883219337665, 0.4232601004234298747 ) ) ;
#180188 = CARTESIAN_POINT ( 'NONE',  ( 0.7500000000000006661, 10.36458333401613174, 1.299038105676657340 ) ) ;
#180189 = CARTESIAN_POINT ( 'NONE',  ( 5.836230100724939085, -1.233609159639902142, -1.847210489216906781 ) ) ;
#180190 = VERTEX_POINT ( 'NONE', #17 ) ;
#180192 = STYLED_ITEM ( 'NONE', ( #182945 ), #57047 ) ;
#180191 = CARTESIAN_POINT ( 'NONE',  ( 6.983263157960335477, 6.035714437257905018, 2.641087593604172667 ) ) ;
#180193 = CARTESIAN_POINT ( 'NONE',  ( 1.499999999999987121, 3.295833333333354709, -0.8660254037844262731 ) ) ;
#180194 = CARTESIAN_POINT ( 'NONE',  ( 5.392392409933256303, 7.314210449720692786, 1.599625672291267398 ) ) ;
#180195 = CARTESIAN_POINT ( 'NONE',  ( 1.260717678522350838, 2.218966152042425755, 0.1042569218142989779 ) ) ;
#180196 = CARTESIAN_POINT ( 'NONE',  ( 6.830524215763060347, -1.208013408316032322, 1.546442907991877558 ) ) ;
#180197 = CARTESIAN_POINT ( 'NONE',  ( 7.076992996653421741, 10.23994701519558781, -1.082531754730537976 ) ) ;
#180198 = CARTESIAN_POINT ( 'NONE',  ( -9.991996023147281747, 11.72004545083573568, 1.082531754730558626 ) ) ;
#180199 = CARTESIAN_POINT ( 'NONE',  ( 7.838022202476093270, 8.316983122409855156, 0.7216878364870267237 ) ) ;
#180200 = CARTESIAN_POINT ( 'NONE',  ( -4.828112100242303306, 4.805421336470338645, -0.7216878364870338292 ) ) ;
#180202 = CARTESIAN_POINT ( 'NONE',  ( 4.105966297347532823, 0.6976637339557908435, -1.941222516249243579 ) ) ;
#180201 = CARTESIAN_POINT ( 'NONE',  ( 8.041957671200231417, 12.53403438304231976, 1.040834085586084257E-14 ) ) ;
#180203 = CARTESIAN_POINT ( 'NONE',  ( -2.605138072120212200, 6.191078184115536232, -0.7998128361456281477 ) ) ;
#180204 = CARTESIAN_POINT ( 'NONE',  ( -0.7499999999999972244, 4.639583334016150751, -1.299038105676652899 ) ) ;
#180205 = CARTESIAN_POINT ( 'NONE',  ( -1.364683531250014514, -0.7197916663252461600, 0.7879004041258379498 ) ) ;
#180206 = CARTESIAN_POINT ( 'NONE',  ( 6.468025801952650866, 0.9617254617904011926, 1.604207369834034669 ) ) ;
#180207 = CARTESIAN_POINT ( 'NONE',  ( 6.205661552121055635, 1.621658882679182456, 0.6149916719311411262 ) ) ;
#180208 = CARTESIAN_POINT ( 'NONE',  ( 4.511116409865087995, -1.705632679577104849, 0.3454082310308664305 ) ) ;
#180209 = CARTESIAN_POINT ( 'NONE',  ( 5.359550796103802028, 5.147230771742885125, -0.7998128361456231517 ) ) ;
#180210 = CARTESIAN_POINT ( 'NONE',  ( 2.736170862265740578, 2.275407485025813692, 0.2777600125268233633 ) ) ;
#180211 = CARTESIAN_POINT ( 'NONE',  ( -1.364683531249997417, 4.821875000341417916, 1.214306433183764966E-14 ) ) ;
#180212 = CARTESIAN_POINT ( 'NONE',  ( 0.9898993202219902310, -0.4452471680344311511, -1.786356756097874587 ) ) ;
#180213 = CARTESIAN_POINT ( 'NONE',  ( 10.18233705906309972, 11.83814697611718714, 1.199719254218450271 ) ) ;
#180214 = CARTESIAN_POINT ( 'NONE',  ( 2.437500000000002220, 1.451031289061020857, -1.451031289061217366 ) ) ;
#180215 = CARTESIAN_POINT ( 'NONE',  ( 1.518276268637512194, 1.228937244518006011, -1.350148523839814096 ) ) ;
#180216 = CARTESIAN_POINT ( 'NONE',  ( 2.531875153343257523, -1.674887184936912909, 1.122499117612890673 ) ) ;
#180217 = CARTESIAN_POINT ( 'NONE',  ( 1.763894328224338448, 1.128481436294457740, 1.878420861880884862 ) ) ;
#180218 = CARTESIAN_POINT ( 'NONE',  ( 8.771385051288104862, 13.55262984818672045, -7.723180138624951674 ) ) ;
#180219 = CARTESIAN_POINT ( 'NONE',  ( 4.612399560509667928, -0.8980232107528103302, -1.905027153144087437 ) ) ;
#180220 = CARTESIAN_POINT ( 'NONE',  ( -7.711890448074853133, 7.891627032375787998, -0.7998128361456291469 ) ) ;
#180221 = CARTESIAN_POINT ( 'NONE',  ( 1.627480586986803868, 0.1543294891723171747, -2.064685722993148342 ) ) ;
#180222 = CARTESIAN_POINT ( 'NONE',  ( 6.193377243344257543, 6.120028293523423812, -0.7998128361456281477 ) ) ;
#180223 = CARTESIAN_POINT ( 'NONE',  ( -1.360316468750013108, -0.3281249996585910989, -3.469446951953614189E-14 ) ) ;
#180224 = CARTESIAN_POINT ( 'NONE',  ( 3.422626747576805961, -0.8610355553571764631, -1.937992358232228041 ) ) ;
#180225 = CARTESIAN_POINT ( 'NONE',  ( -0.6823417656250003738, 0.2177083336747515085, -1.181850606188749264 ) ) ;
#180226 = CARTESIAN_POINT ( 'NONE',  ( -0.01707793031917748464, -0.1336475082493841504, -1.895772241332476682 ) ) ;
#180227 = ORIENTED_EDGE ( 'NONE', *, *, #117565, .T. ) ;
#180228 = CARTESIAN_POINT ( 'NONE',  ( -5.119085517611572378, 8.129960982925583224, 1.199719254218452935 ) ) ;
#180229 = CARTESIAN_POINT ( 'NONE',  ( 8.401248741962376698, 12.95320729893149370, 0.7998128361456462443 ) ) ;
#180230 = CARTESIAN_POINT ( 'NONE',  ( 7.336370518326124746, 7.731722824234849689, -0.7216878364870317197 ) ) ;
#180231 = CARTESIAN_POINT ( 'NONE',  ( -3.475000000000000533, -3.106249999044085275, 0.000000000000000000 ) ) ;
#180232 = CARTESIAN_POINT ( 'NONE',  ( -7.230575994789712801, 7.330093503543126054, 0.7998128361456341429 ) ) ;
#180233 = CARTESIAN_POINT ( 'NONE',  ( 3.709244008563481465, 1.704072514596865817, -1.083995235011512515 ) ) ;
#180234 = CARTESIAN_POINT ( 'NONE',  ( 0.6925746140923200178, -2.090094003047581861, -0.2575201054717362048 ) ) ;
#180235 = CARTESIAN_POINT ( 'NONE',  ( -6.143779885648060102, 7.196773283791382703, 1.199719254218452047 ) ) ;
#180236 = CARTESIAN_POINT ( 'NONE',  ( 8.565000355531088516, 11.01558638625153286, -1.599625672291257406 ) ) ;
#180237 = CARTESIAN_POINT ( 'NONE',  ( 5.629708122894265365, 1.793948666107824774, -0.4946651665681394139 ) ) ;
#180238 = CARTESIAN_POINT ( 'NONE',  ( 6.740374924288304648, 11.01552117831172062, 1.040834085586084257E-14 ) ) ;
#180239 = CARTESIAN_POINT ( 'NONE',  ( -0.6500564563262781759, 4.350073393241474129, -0.06808518787147278817 ) ) ;
#180240 = CARTESIAN_POINT ( 'NONE',  ( -8.012505595996376684, 12.29174759539704986, 0.000000000000000000 ) ) ;
#180241 = CARTESIAN_POINT ( 'NONE',  ( -7.542413527904030524, 7.693903958843159252, 1.040834085586084257E-14 ) ) ;
#180242 = CARTESIAN_POINT ( 'NONE',  ( 6.297740734744428970, -0.6968897171561654336, 1.939616516419547132 ) ) ;
#180244 = CARTESIAN_POINT ( 'NONE',  ( -4.022959435666734862, 7.784601250164370434, 0.4788606935734913694 ) ) ;
#180243 = CARTESIAN_POINT ( 'NONE',  ( -4.762657100150483380, 8.778460060142702304, 0.000000000000000000 ) ) ;
#180245 = CARTESIAN_POINT ( 'NONE',  ( 0.6823417656249882723, 0.1760416670080894308, -1.181850606188749264 ) ) ;
#180246 = CARTESIAN_POINT ( 'NONE',  ( 2.372030889105484430, -0.3844106184479143540, 1.690481094739235912 ) ) ;
#180247 = CARTESIAN_POINT ( 'NONE',  ( 0.8139225777531241546, 1.606474054549825503, 0.6698172574813018310 ) ) ;
#180249 = CARTESIAN_POINT ( 'NONE',  ( 6.887178846062110615, 9.058127958537705027, -1.443375672974057666 ) ) ;
#180248 = CARTESIAN_POINT ( 'NONE',  ( 0.2183775786483640735, -2.262126603235939282, 0.4550015798871313577 ) ) ;
#180250 = CARTESIAN_POINT ( 'NONE',  ( -11.01567899581106325, 5.044704703271206903, 4.264317011375222677 ) ) ;
#180251 = CARTESIAN_POINT ( 'NONE',  ( 2.934896792925650644, 0.2487164785463981398, 2.045624280402899231 ) ) ;
#180252 = CARTESIAN_POINT ( 'NONE',  ( 4.924636110261782385, 6.768494766770632332, 1.599625672291267398 ) ) ;
#180253 = CARTESIAN_POINT ( 'NONE',  ( 1.616564310028177243, 0.5879328921069119085, -1.928455639302439462 ) ) ;
#180254 = DIRECTION ( 'NONE',  ( 0.000000000000000000, 0.000000000000000000, -1.000000000000000000 ) ) ;
#180255 = CARTESIAN_POINT ( 'NONE',  ( -4.773352600463090845, 7.726605912919016106, 1.199719254218452935 ) ) ;
#180256 = AXIS2_PLACEMENT_3D ( 'NONE', #40378, #173595, #104300 ) ;
#180257 = CARTESIAN_POINT ( 'NONE',  ( 0.9011734813738042638, 1.610450750236171125, 1.136898926478569383 ) ) ;
#180259 = CARTESIAN_POINT ( 'NONE',  ( -7.932929277771797238, 8.427708043588125975, 0.000000000000000000 ) ) ;
#180258 = CARTESIAN_POINT ( 'NONE',  ( 4.851772015791367743, -1.356534033432246211, -1.348250844427544282 ) ) ;
#180260 = CARTESIAN_POINT ( 'NONE',  ( 6.199877634063251541, -0.7475181258948644381, 2.076568058718592624 ) ) ;
#180261 = CARTESIAN_POINT ( 'NONE',  ( -7.065207446052813367, 8.375735120883982532, -1.082531754730549967 ) ) ;
#180262 = CARTESIAN_POINT ( 'NONE',  ( 7.364013710877980401, 8.620379413226322285, -1.199719254218452047 ) ) ;
#180263 = CARTESIAN_POINT ( 'NONE',  ( -6.420668264523499147, 9.648474187656182366, 1.199719254218452935 ) ) ;
#180264 = CARTESIAN_POINT ( 'NONE',  ( -0.04036499569192492781, -1.562578347245877630, -1.279382211958324689 ) ) ;
#180265 = DIRECTION ( 'NONE',  ( 0.000000000000000000, 1.000000000000000000, 0.000000000000000000 ) ) ;
#180266 = CARTESIAN_POINT ( 'NONE',  ( 4.173124822893734986, -2.151704308474690741, -0.8341741560445140591 ) ) ;
#180267 = CARTESIAN_POINT ( 'NONE',  ( 4.844172697165038066, -0.9265620464425131653, 1.729294158640543699 ) ) ;
#180268 = CARTESIAN_POINT ( 'NONE',  ( 1.446067858876250112, -0.8869304882095051523, 1.749921244195346004 ) ) ;
#180269 = CARTESIAN_POINT ( 'NONE',  ( 0.000000000000000000, 0.2000000000000057288, -8.500000000000000000 ) ) ;
#180270 = CARTESIAN_POINT ( 'NONE',  ( -9.472628840146047224, 14.62787916692008849, 7.367007921869499931 ) ) ;
#180271 = EDGE_LOOP ( 'NONE', ( #117048, #59121, #81699, #99375 ) ) ;
#180272 = CARTESIAN_POINT ( 'NONE',  ( 0.6029268795967283046, 1.958829854606686904, 0.8042956034161384826 ) ) ;
#180274 = CARTESIAN_POINT ( 'NONE',  ( -7.507464373665155399, 9.781794407407920389, 1.599625672291295375 ) ) ;
#180273 = CARTESIAN_POINT ( 'NONE',  ( -4.086893239515592136, 6.855460315155083251, 1.199719254218464037 ) ) ;
#180275 = CARTESIAN_POINT ( 'NONE',  ( 0.6031360380127914755, -1.832534659106283659, 0.1778487281504093076 ) ) ;
#180276 = EDGE_LOOP ( 'NONE', ( #77573, #17393, #167040, #28411 ) ) ;
#180277 = CARTESIAN_POINT ( 'NONE',  ( 3.766621525425926098, -0.8750874339106663458, -1.987059052243181689 ) ) ;
#180278 = CARTESIAN_POINT ( 'NONE',  ( 10.86983561997773684, 9.640297115645962478, 5.096404461738570646 ) ) ;
#180280 = EDGE_CURVE ( 'NONE', #2091, #119510, #30770, .T. ) ;
#180279 = CARTESIAN_POINT ( 'NONE',  ( 1.775790443353560732, 0.3575140072833470906, -2.090081039791711337 ) ) ;
#180281 = CARTESIAN_POINT ( 'NONE',  ( -1.201851678989727383E-14, 2.993750000682821266, 1.732050807568877637 ) ) ;
#180282 = CARTESIAN_POINT ( 'NONE',  ( 7.540305987494599016, 11.94877408538573427, -0.7998128361456291469 ) ) ;
#180283 = CARTESIAN_POINT ( 'NONE',  ( 7.785697387528199762E-15, 0.5624999999999894529, 1.224999999999973443 ) ) ;
#180284 = CARTESIAN_POINT ( 'NONE',  ( 2.811851269462920744, -2.038842655386669644, 0.2989082417928933810 ) ) ;
#180285 = PRESENTATION_LAYER_ASSIGNMENT (  '', '', ( #156011 ) ) ;
#180287 = CARTESIAN_POINT ( 'NONE',  ( -0.05938221139379848412, -1.422385081007140117, -1.168950373246782526 ) ) ;
#180286 = CARTESIAN_POINT ( 'NONE',  ( -7.883176251342026042, 11.28445716228600126, -1.199719254218446718 ) ) ;
#180288 = CARTESIAN_POINT ( 'NONE',  ( 1.364683531249990311, 2.884375000341422801, 1.214306433183764966E-14 ) ) ;
#180289 = CARTESIAN_POINT ( 'NONE',  ( -0.02264175331115856477, 0.2280268304470518537, -2.122276614016995744 ) ) ;
#180290 = CARTESIAN_POINT ( 'NONE',  ( 1.392936117481126113, 4.158586050112920596, -0.5577005436122643989 ) ) ;
#180291 = CARTESIAN_POINT ( 'NONE',  ( 1.499999999999990896, 4.275000000000021672, 1.214306433183764966E-14 ) ) ;
#180292 = CARTESIAN_POINT ( 'NONE',  ( 0.9665587677401198397, 1.115807381107810192, 1.968008997871427468 ) ) ;
#180293 = CARTESIAN_POINT ( 'NONE',  ( -9.002250809794000830, 11.52571191622492464, -1.443375672974059665 ) ) ;
#180294 = CARTESIAN_POINT ( 'NONE',  ( 1.019438801881300316, -0.4388897500222695425, 1.757493349343726585 ) ) ;
#180295 = CARTESIAN_POINT ( 'NONE',  ( 2.483477273924311834, -0.5967159848992757976, 1.820515277383168540 ) ) ;
#180296 = CARTESIAN_POINT ( 'NONE',  ( 3.174344110969638866, -1.018096006688212096, -1.802650257252853772 ) ) ;
#180297 = CARTESIAN_POINT ( 'NONE',  ( -0.6823417656250003738, 1.530208333674752730, -1.181850606188749264 ) ) ;
#180298 = CIRCLE ( 'NONE', #104228, 6.961139734775127152 ) ;
#180299 = CARTESIAN_POINT ( 'NONE',  ( 1.463681139585114588, 1.942636298559533792, -0.3350429378523085977 ) ) ;
#180300 = CARTESIAN_POINT ( 'NONE',  ( 5.391212663409540973, 1.697947877755761947, -0.9101574019480199729 ) ) ;
#180302 = CARTESIAN_POINT ( 'NONE',  ( 6.157602363183391603, 6.969851231138187941, -0.9158007892692658913 ) ) ;
#180301 = CARTESIAN_POINT ( 'NONE',  ( 0.7510979139944070626, 0.6750874020578813139, 2.206752807669599470 ) ) ;
#180303 = CARTESIAN_POINT ( 'NONE',  ( -1.201851678989727383E-14, 3.321875000341421025, 1.575800808251672791 ) ) ;
#180304 = CARTESIAN_POINT ( 'NONE',  ( 5.687952575977194947, -1.305682642493616541, -1.596842856974973301 ) ) ;
#180305 = CARTESIAN_POINT ( 'NONE',  ( -4.388035272317281077, 8.271124917678806199, 0.7998128361456481317 ) ) ;
#180306 = CARTESIAN_POINT ( 'NONE',  ( 6.262976894508937242, 9.394224579314053969, -1.199719254218440723 ) ) ;
#180307 = CARTESIAN_POINT ( 'NONE',  ( -1.350460993223241868, 3.453365176191621089, 0.3113056364347011606 ) ) ;
#180308 = EDGE_CURVE ( 'NONE', #180412, #99270, #41131, .T. ) ;
#180309 = CARTESIAN_POINT ( 'NONE',  ( 6.821333371289608927, -0.1635999628400324479, 2.070553102365073173 ) ) ;
#180310 = CARTESIAN_POINT ( 'NONE',  ( 0.6823417656249882723, 2.988541667008084879, -1.181850606188754593 ) ) ;
#180311 = CARTESIAN_POINT ( 'NONE',  ( 4.534552404040613105, 2.118918870418550870, 0.4265773709258223190 ) ) ;
#180312 = CARTESIAN_POINT ( 'NONE',  ( 4.951822102061871789, -1.429791030739693047, -1.426725901824247078 ) ) ;
#180313 = CARTESIAN_POINT ( 'NONE',  ( -4.284013352238255301, 6.981470763377843447, -1.082531754730549967 ) ) ;
#180314 = CARTESIAN_POINT ( 'NONE',  ( -5.097502569058215194, 6.970172302033127210, -1.443375672974053447 ) ) ;
#180317 = CARTESIAN_POINT ( 'NONE',  ( 5.992340707560163793, 6.093411701682730275, 0.7216878364870317197 ) ) ;
#180316 = CARTESIAN_POINT ( 'NONE',  ( 3.285556943749998737, -2.705208332855374209, -1.896917185911906500 ) ) ;
#180315 = CARTESIAN_POINT ( 'NONE',  ( 6.688968683495743583, 8.897159112202094988, -1.599625672291283607 ) ) ;
#180318 = CARTESIAN_POINT ( 'NONE',  ( -5.679940009482361774, 5.591294530676332641, 0.7998128361456281477 ) ) ;
#180319 = CARTESIAN_POINT ( 'NONE',  ( 3.591030000661588062, 1.731995077137841843, 1.032480907900306111 ) ) ;
#180320 = CARTESIAN_POINT ( 'NONE',  ( -6.855619230004478482, 11.14997286831390788, -0.7998128361456291469 ) ) ;
#180321 = CARTESIAN_POINT ( 'NONE',  ( -2.428882075142555497, 5.985446187641602300, 1.040834085586084257E-14 ) ) ;
#180323 = CARTESIAN_POINT ( 'NONE',  ( 0.6823417656249934904, 9.442708333674735499, 1.181850606188764807 ) ) ;
#180322 = CARTESIAN_POINT ( 'NONE',  ( 5.207972885698374022, -2.151664816535401314, 0.2080130470862306957 ) ) ;
#180324 = FILL_AREA_STYLE ('',( #196574 ) ) ;
#180325 = CARTESIAN_POINT ( 'NONE',  ( -11.99120512803725447, 8.059048065725468390, -0.5291463972175238784 ) ) ;
#180327 = CARTESIAN_POINT ( 'NONE',  ( 5.062125140741547291, -1.117816439015427044, 1.678017345901124058 ) ) ;
#180326 = CARTESIAN_POINT ( 'NONE',  ( -7.836249598574384301, 8.244638741199329601, 1.040834085586084257E-14 ) ) ;
#180328 = CARTESIAN_POINT ( 'NONE',  ( -1.402160292154681736E-14, -0.2406249996585799189, -1.575800808251665908 ) ) ;
#180329 = CARTESIAN_POINT ( 'NONE',  ( 1.312684994149786455, 1.519677550804766852, 0.8159285863849721210 ) ) ;
#180330 = CARTESIAN_POINT ( 'NONE',  ( 3.237364818613055473, 6.998952398349030268, -1.734723475976807094E-15 ) ) ;
#180332 = CARTESIAN_POINT ( 'NONE',  ( 7.180978637093494044, 8.406838493811077839, -1.199719254218452047 ) ) ;
#180331 = CARTESIAN_POINT ( 'NONE',  ( 8.649738815838679429, 10.15407870897571563, -1.082531754730543083 ) ) ;
#180333 = CARTESIAN_POINT ( 'NONE',  ( -11.95117894359873212, 8.932389826126765797, -1.235014725827771720 ) ) ;
#180334 = CARTESIAN_POINT ( 'NONE',  ( 6.432864026670258362, 0.1834693771665257822, 1.861492386831371748 ) ) ;
#180336 = CARTESIAN_POINT ( 'NONE',  ( 0.6627443117090633384, 0.5862905632768620201, 1.925809981296212170 ) ) ;
#180335 = PRODUCT_DEFINITION_FORMATION_WITH_SPECIFIED_SOURCE ( 'ANY', '', #67584, .NOT_KNOWN. ) ;
#180337 = PRESENTATION_STYLE_ASSIGNMENT (( #63387 ) ) ;
#180338 = CARTESIAN_POINT ( 'NONE',  ( 2.731697238759897672, -2.059418846490802313, 0.7933392487004319316 ) ) ;
#180339 = VECTOR ( 'NONE', #135246, 1000.000000000000000 ) ;
#180340 = CARTESIAN_POINT ( 'NONE',  ( -5.085717018457573957, 8.947437264926888290, 0.7216878364870267237 ) ) ;
#180341 = ORIENTED_EDGE ( 'NONE', *, *, #209339, .F. ) ;
#180342 = CARTESIAN_POINT ( 'NONE',  ( 8.798878505144646311, 11.28844422746735532, -1.443375672974052559 ) ) ;
#180344 = CARTESIAN_POINT ( 'NONE',  ( 1.370720498019749378, -0.2986500928384462350, -1.994069080148860973 ) ) ;
#180343 = CARTESIAN_POINT ( 'NONE',  ( 1.910938629679886480, -0.5684797485801665884, -2.042784538176869003 ) ) ;
#180346 = ORIENTED_EDGE ( 'NONE', *, *, #83296, .F. ) ;
#180345 = CARTESIAN_POINT ( 'NONE',  ( 2.320317256442219644, -0.6965147209693119956, -1.672536871252501500 ) ) ;
#180347 = CARTESIAN_POINT ( 'NONE',  ( 6.688968683495743583, 8.897159112202094988, -1.599625672291283607 ) ) ;
#180348 = CARTESIAN_POINT ( 'NONE',  ( 4.950698647284403009, 8.927565521807144577, 1.040834085586084257E-14 ) ) ;
#180350 = CARTESIAN_POINT ( 'NONE',  ( 0.7256311455483875905, 0.7733690622436960593, -1.752846625659326696 ) ) ;
#180349 = CARTESIAN_POINT ( 'NONE',  ( -5.413783410558481002, 5.210502155273325720, -0.7998128361456221525 ) ) ;
#180351 = CARTESIAN_POINT ( 'NONE',  ( -2.651186565980338639, 0.4067314603539678441, -0.1428011528578489453 ) ) ;
#180352 = DIRECTION ( 'NONE',  ( 0.000000000000000000, 1.000000000000000000, 0.000000000000000000 ) ) ;
#180353 = CARTESIAN_POINT ( 'NONE',  ( 6.765155463094761679, 6.995028916473103209, 0.7216878364870317197 ) ) ;
#180354 = CARTESIAN_POINT ( 'NONE',  ( 1.364683531249988757, 0.9468750003414211358, 0.000000000000000000 ) ) ;
#180355 = CARTESIAN_POINT ( 'NONE',  ( 3.834746474454188013E-15, 12.84375000068279782, 1.500000000000001554 ) ) ;
#180356 = CARTESIAN_POINT ( 'NONE',  ( -8.839026081105473054, 12.39961529701003684, -1.199719254218446718 ) ) ;
#180357 = CARTESIAN_POINT ( 'NONE',  ( 5.243122039519461097, -1.856066598825537373, 1.107904190987746063 ) ) ;
#180358 = CARTESIAN_POINT ( 'NONE',  ( -6.970300371201519241, 7.304640985922785212, 0.7216878364870317197 ) ) ;
#180359 = CARTESIAN_POINT ( 'NONE',  ( 4.692530564105613422, 7.528350520548263702, -1.082531754730548412 ) ) ;
#180360 = CARTESIAN_POINT ( 'NONE',  ( 1.652743449602233294, 2.098267697663996234, 0.3060111223712051465 ) ) ;
#180361 = CARTESIAN_POINT ( 'NONE',  ( -0.3282377607281457554, 2.551335450315352915, 1.224999999999984324 ) ) ;
#180362 =( BOUNDED_SURFACE ( )  B_SPLINE_SURFACE ( 1, 2, ( 
 ( #201891, #50351, #100163, #166227, #19958, #169426, #184593, #38359, #18890, #84974, #35143, #103364, #16757, #151065, #101219, #17817, #2628, #153178, #83901, #116471, #3689, #68700, #134822, #490, #51422, #70827, #167303, #34092, #53543, #82840, #67624, #21009, #148916, #182463, #133768, #198706, #200827, #199776, #52478, #36211, #117543, #186737, #66558, #102290, #183537, #168363, #4752, #86043, #119675, #152118, #69766, #135872, #185661, #136944, #37291, #132700, #202970, #54611, #120759, #42659, #104437, #172645, #188873, #105521, #90323, #92480, #39428, #55673, #157466, #156392, #7978, #154254, #205107, #10118, #40513, #187799, #207254, #192059, #23151, #108768, #170486, #121829, #171555, #138010, #74067, #89266, #206183, #123973, #155316, #126099, #22070, #106616, #204025, #6900, #158521, #107701, #189940, #72977, #71901, #88182, #24221, #41589, #140159, #57810, #56749, #139080, #25304, #122915, #76193, #173727, #91406, #9060, #5827, #75136, #141245, #58882, #125037, #190993, #174793, #26369, #59943, #142302, #208313, #30667, #93538, #212586, #177979, #129317, #109837, #62090, #162800, #31732, #130367, #161734, #28518, #96750, #15444, #211515, #95680, #94609, #160652, #110898, #176904, #47998, #61016, #147614, #146568, #97805, #12250, #194212, #128248, #79399, #78327, #144449, #210452, #45857, #143373, #175849, #77259, #111979, #29594, #13325, #145516, #159582, #44792, #63152, #131405, #195292, #46924, #113042, #179048, #14377, #196357, #163867, #27440, #80467, #64225, #114115, #180108, #209372, #11180, #127174, #81533, #213632, #65258, #43722, #193143, #198461, #199527, #70581, #33840, #51171, #150818, #117294, #183291, #69522, #185418, #49046, #18649, #19720, #82588, #132459, #50105, #52235, #201649, #2380, #197405, #34896, #100969, #67380, #135629, #115166, #167058, #133521, #116225, #84729, #37036, #182217, #148675, #35973, #68458, #134587, #32784, #83652, #103120, #200587, #66315, #85799, #181161, #99921, #53299, #98861, #243, #165982, #16506, #118362, #17568, #184351, #102052, #149741, #4509, #164913, #168119, #1319, #151878, #169178, #3453, #119431, #20770, #86866, #152931, #138835, #156149, #72738, #40260, #22903, #171309, #57572, #39184, #42412, #7731, #104193, #105272, #38121, #5574, #41343, #106372, #172395, #90086, #73816, #170241, #92232, #157214, #187555, #123730, #186489, #91158, #56505, #139909, #202722, #155072, #107452, #124788, #8810, #23983, #121584, #189692, #108517, #205940, #188629, #89019, #6661, #203786, #55432, #140996, #154007, #26121, #25056, #190748, #204851, #122667, #173479, #74888, #207004, #58635, #21825, #71654, #174546, #158283, #9873, #136697, #54375, #87934, #120512, #137768, #126921, #62887, #125854, #30412, #210197, #161484, #142051, #94358, #195030, #63960, #162546, #193953, #60761, #129056, #47741, #29338, #127999, #192879, #44534, #143128, #209124, #80207, #93294, #179852, #178796, #130115, #110652, #12002, #160400, #111718, #176653, #28266, #78076, #144201, #175598, #208066, #109593, #61833, #45601, #177726, #95431, #191811, #77002, #13062, #163607, #79141, #145258, #211263, #46664, #112785, #14116, #196105, #59691, #96496, #146308, #27188, #10926, #212322, #113857, #31475, #97550, #75949, #43475, #159330, #99656, #167853, #15189, #83391, #165725, #16243, #1058, #3183, #164661, #180901, #68190, #67123, #133256, #65007, #115966, #135371, #17313, #98600, #118104, #102856, #148421, #19451, #81280, #32524, #82329, #48787, #199262, #93774, #117035, #34646, #66053, #36770, #147356, #149475, #114904, #132197, #69254, #18387, #100716, #198204, #197150, #213383, #50907, #166793, #183030, #84464, #181955, #49839, #150556, #33583, #201389, #2116, #134323, #131159, #85527, #200329, #184089, #51979, #35708, #101785, #151616, #53027, #119160, #185146, #124522, #168912, #137500, #205665, #58368, #187291, #203517, #54106, #42138, #190479, #70319, #20515, #121316, #206737, #154805, #71388, #6391, #171041, #202452, #90887, #155873, #72464, #55171, #156946, #8537, #86600, #153739, #4250, #5307, #21561, #74619, #140724, #37850, #73541, #152666, #120241, #136436, #107178 ),
 ( #103928, #169973, #23718, #173204, #122396, #186219, #22640, #88748, #38918, #24784, #87667, #138564, #105002, #204585, #56236, #188354, #39994, #106102, #7462, #172124, #89825, #139643, #57303, #123466, #189429, #41071, #210985, #195828, #26914, #112506, #108253, #59425, #125583, #141793, #94090, #43208, #209920, #127724, #159064, #129845, #25849, #110383, #207797, #191543, #96217, #111446, #193683, #109324, #75683, #174274, #176388, #45327, #44260, #11728, #208854, #142850, #29065, #10660, #13855, #177451, #175331, #76732, #9606, #93023, #12786, #77804, #162268, #91958, #60485, #158018, #126643, #192608, #79931, #146037, #27993, #78860, #160129, #143925, #61558, #46389, #95148, #161200, #144981, #62613, #128775, #194752, #178518, #30128, #212051, #63691, #17045, #14913, #99397, #135115, #151356, #35444, #181686, #165450, #83124, #98328, #117843, #15977, #82062, #34378, #47466, #163333, #49569, #149204, #18115, #50637, #130891, #48523, #183835, #85270, #132990, #114643, #213119, #33316, #67918, #101523, #147095, #66846, #51721, #167593, #779, #182760, #2925, #198990, #19192, #115693, #197941, #81007, #116763, #180636, #68998, #32260, #100451, #64749, #113581, #134063, #166524, #84202, #179583, #196885, #65781, #31205, #150291, #97279, #1858, #148154, #200072, #164394, #131931, #214155, #90359, #36513, #20258, #189973, #91440, #52769, #59979, #206217, #92517, #106650, #140195, #118905, #24254, #10153, #102599, #8012, #159619, #201131, #172677, #26405, #93574, #74103, #156426, #86342, #77297, #11216, #168654, #184889, #57843, #27476, #41623, #124006, #107737, #173762, #152414, #126133, #191030, #25339, #157501, #192093, #3993, #9096, #75172, #202193, #141282, #43760, #136174, #70062, #42697, #207290, #58916, #53849, #125073, #109873, #108803, #122947, #158556, #188904, #40546, #208348, #174828, #76227, #142338, #175886, #129348, #78360, #30702, #162834, #194246, #164946, #61050, #145551, #28554, #12282, #131436, #146599, #14412, #144481, #110932, #16538, #211548, #80502, #79433, #46957, #29629, #178011, #64257, #45890, #49079, #212617, #176937, #112011, #44827, #210487, #48033, #113074, #179080, #96783, #130400, #94643, #98893, #163902, #95714, #196390, #193178, #97837, #63183, #114147, #209405, #161768, #180139, #197439, #15478, #31767, #128284, #81562, #115199, #147646, #195326, #13359, #213664, #62124, #65289, #181192, #160687, #32819, #143409, #127210, #51204, #18682, #101002, #118393, #117326, #67411, #1349, #199560, #182248, #148705, #116259, #183324, #133552, #34928, #167091, #198492, #83685, #84761, #170272, #150848, #2412, #36000, #68489, #134617, #169211, #70613, #274, #184381, #119461, #33873, #17601, #149774, #151908, #86898, #102081, #82620, #200619, #52266, #168149, #20802, #19749, #85829, #3482, #69549, #50136, #135659, #201682, #66346, #53328, #185449, #37069, #103150, #152965, #4539, #136728, #132490, #202752, #54405, #99951, #120544, #186523, #38153, #104225, #166015, #109629, #90116, #156182, #106401, #174579, #21857, #7760, #172425, #22935, #73849, #9906, #171341, #187587, #74918, #139944, #205970, #71686, #122699, #142085, #24014, #105304, #124816, #87964, #155108, #26155, #154038, #39213, #89051, #55463, #57602, #6693, #123761, #41376, #72768, #43508, #5604, #189722, #121618, #138867, #75982, #25084, #107486, #204885, #203818, #137799, #173511, #91186, #157247, #8840, #188662, #56537, #141029, #40291, #208100, #207036, #58666, #190780, #42443, #108547, #92269, #158315, #59728, #125887, #191845, #209158, #131197, #196139, #12037, #162578, #10960, #130149, #95468, #46702, #27220, #193986, #80246, #163644, #47779, #79178, #160431, #14152, #147391, #129091, #13098, #78108, #144235, #28296, #94392, #179887, #192914, #65041, #63998, #15225, #210229, #111751, #45634, #211299, #61867, #128032, #177757, #29373, #60796, #93326, #126955, #176684, #30445, #31511, #195063, #48822, #161516, #145294, #62923, #113893, #175634, #112818, #178831, #96529, #146344, #81315, #110686, #44570, #212357, #97586, #213418, #77035, #197185, #159362, #143163, #198240, #3223, #202492, #33622, #119198, #114938, #66089 ) ),
 .UNSPECIFIED., .F., .F., .F. ) 
 B_SPLINE_SURFACE_WITH_KNOTS ( ( 2, 2 ),
 ( 3, 2, 2, 2, 2, 2, 2, 2, 2, 2, 2, 2, 2, 2, 2, 2, 2, 2, 2, 2, 2, 2, 2, 2, 2, 2, 2, 2, 2, 2, 2, 2, 2, 2, 2, 2, 2, 2, 2, 2, 2, 2, 2, 2, 2, 2, 2, 2, 2, 2, 2, 2, 2, 2, 2, 2, 2, 2, 2, 2, 2, 2, 2, 2, 2, 2, 2, 2, 2, 2, 2, 2, 2, 2, 2, 2, 2, 2, 2, 2, 2, 2, 2, 2, 2, 2, 2, 2, 2, 2, 2, 2, 2, 2, 2, 2, 2, 2, 2, 2, 2, 2, 2, 2, 2, 2, 2, 2, 2, 2, 2, 2, 2, 2, 2, 2, 2, 2, 2, 2, 2, 2, 2, 2, 2, 2, 2, 2, 2, 2, 2, 2, 2, 2, 2, 2, 2, 2, 2, 2, 2, 2, 2, 2, 2, 2, 2, 2, 2, 2, 2, 2, 2, 2, 2, 2, 2, 2, 2, 2, 2, 2, 2, 2, 2, 2, 2, 2, 2, 2, 2, 2, 2, 2, 2, 2, 2, 2, 2, 2, 2, 2, 2, 2, 2, 2, 2, 2, 2, 2, 2, 2, 2, 2, 2, 2, 2, 2, 2, 2, 2, 2, 2, 2, 2, 2, 2, 2, 2, 2, 2, 2, 2, 2, 2, 2, 2, 2, 2, 2, 2, 2, 2, 2, 2, 2, 2, 2, 2, 2, 2, 2, 2, 2, 2, 2, 2, 2, 2, 2, 3 ),
 ( 0.000000000000000000, 1.000000000000000000 ),
 ( 0.000000000000000000, 0.004166666666666666609, 0.008333333333333333218, 0.01250000000000000069, 0.01666666666666666644, 0.02083333333333333218, 0.02500000000000000139, 0.02916666666666666713, 0.03333333333333333287, 0.03749999999999999861, 0.04166666666666666435, 0.04583333333333333010, 0.05000000000000000278, 0.05416666666666666852, 0.05833333333333333426, 0.06250000000000000000, 0.06666666666666666574, 0.07083333333333333148, 0.07499999999999999722, 0.07916666666666666297, 0.08333333333333332871, 0.08749999999999999445, 0.09166666666666666019, 0.09583333333333333981, 0.1000000000000000056, 0.1041666666666666713, 0.1083333333333333370, 0.1125000000000000028, 0.1166666666666666685, 0.1208333333333333343, 0.1250000000000000000, 0.1291666666666666796, 0.1333333333333333315, 0.1375000000000000111, 0.1416666666666666630, 0.1458333333333333426, 0.1499999999999999944, 0.1541666666666666741, 0.1583333333333333259, 0.1625000000000000056, 0.1666666666666666574, 0.1708333333333333370, 0.1749999999999999889, 0.1791666666666666685, 0.1833333333333333204, 0.1875000000000000000, 0.1916666666666666796, 0.1958333333333333315, 0.2000000000000000111, 0.2041666666666666630, 0.2083333333333333426, 0.2124999999999999944, 0.2166666666666666741, 0.2208333333333333259, 0.2250000000000000056, 0.2291666666666666574, 0.2333333333333333370, 0.2374999999999999889, 0.2416666666666666685, 0.2458333333333333204, 0.2500000000000000000, 0.2541666666666666519, 0.2583333333333333592, 0.2625000000000000111, 0.2666666666666666630, 0.2708333333333333148, 0.2750000000000000222, 0.2791666666666666741, 0.2833333333333333259, 0.2874999999999999778, 0.2916666666666666852, 0.2958333333333333370, 0.2999999999999999889, 0.3041666666666666408, 0.3083333333333333481, 0.3125000000000000000, 0.3166666666666666519, 0.3208333333333333592, 0.3250000000000000111, 0.3291666666666666630, 0.3333333333333333148, 0.3375000000000000222, 0.3416666666666666741, 0.3458333333333333259, 0.3499999999999999778, 0.3541666666666666852, 0.3583333333333333370, 0.3624999999999999889, 0.3666666666666666408, 0.3708333333333333481, 0.3750000000000000000, 0.3791666666666666519, 0.3833333333333333592, 0.3875000000000000111, 0.3916666666666666630, 0.3958333333333333148, 0.4000000000000000222, 0.4041666666666666741, 0.4083333333333333259, 0.4124999999999999778, 0.4166666666666666852, 0.4208333333333333370, 0.4249999999999999889, 0.4291666666666666408, 0.4333333333333333481, 0.4375000000000000000, 0.4416666666666666519, 0.4458333333333333592, 0.4500000000000000111, 0.4541666666666666630, 0.4583333333333333148, 0.4625000000000000222, 0.4666666666666666741, 0.4708333333333333259, 0.4749999999999999778, 0.4791666666666666852, 0.4833333333333333370, 0.4874999999999999889, 0.4916666666666666408, 0.4958333333333333481, 0.5000000000000000000, 0.5041666666666666519, 0.5083333333333333037, 0.5124999999999999556, 0.5166666666666667185, 0.5208333333333333703, 0.5250000000000000222, 0.5291666666666666741, 0.5333333333333333259, 0.5374999999999999778, 0.5416666666666666297, 0.5458333333333332815, 0.5500000000000000444, 0.5541666666666666963, 0.5583333333333333481, 0.5625000000000000000, 0.5666666666666666519, 0.5708333333333333037, 0.5749999999999999556, 0.5791666666666667185, 0.5833333333333333703, 0.5875000000000000222, 0.5916666666666666741, 0.5958333333333333259, 0.5999999999999999778, 0.6041666666666666297, 0.6083333333333332815, 0.6125000000000000444, 0.6166666666666666963, 0.6208333333333333481, 0.6250000000000000000, 0.6291666666666666519, 0.6333333333333333037, 0.6374999999999999556, 0.6416666666666667185, 0.6458333333333333703, 0.6500000000000000222, 0.6541666666666666741, 0.6583333333333333259, 0.6624999999999999778, 0.6666666666666666297, 0.6708333333333332815, 0.6750000000000000444, 0.6791666666666666963, 0.6833333333333333481, 0.6875000000000000000, 0.6916666666666666519, 0.6958333333333333037, 0.6999999999999999556, 0.7041666666666667185, 0.7083333333333333703, 0.7125000000000000222, 0.7166666666666666741, 0.7208333333333333259, 0.7249999999999999778, 0.7291666666666666297, 0.7333333333333332815, 0.7375000000000000444, 0.7416666666666666963, 0.7458333333333333481, 0.7500000000000000000, 0.7541666666666666519, 0.7583333333333333037, 0.7624999999999999556, 0.7666666666666667185, 0.7708333333333333703, 0.7750000000000000222, 0.7791666666666666741, 0.7833333333333333259, 0.7874999999999999778, 0.7916666666666666297, 0.7958333333333332815, 0.8000000000000000444, 0.8041666666666666963, 0.8083333333333333481, 0.8125000000000000000, 0.8166666666666666519, 0.8208333333333333037, 0.8249999999999999556, 0.8291666666666667185, 0.8333333333333333703, 0.8375000000000000222, 0.8416666666666666741, 0.8458333333333333259, 0.8499999999999999778, 0.8541666666666666297, 0.8583333333333332815, 0.8625000000000000444, 0.8666666666666666963, 0.8708333333333333481, 0.8750000000000000000, 0.8791666666666666519, 0.8833333333333333037, 0.8874999999999999556, 0.8916666666666667185, 0.8958333333333333703, 0.9000000000000000222, 0.9041666666666666741, 0.9083333333333333259, 0.9124999999999999778, 0.9166666666666666297, 0.9208333333333332815, 0.9250000000000000444, 0.9291666666666666963, 0.9333333333333333481, 0.9375000000000000000, 0.9416666666666666519, 0.9458333333333333037, 0.9499999999999999556, 0.9541666666666667185, 0.9583333333333333703, 0.9625000000000000222, 0.9666666666666666741, 0.9708333333333333259, 0.9749999999999999778, 0.9791666666666666297, 0.9833333333333332815, 0.9875000000000000444, 0.9916666666666666963, 0.9958333333333333481, 1.000000000000000000 ),
 .UNSPECIFIED. ) 
 GEOMETRIC_REPRESENTATION_ITEM ( )  RATIONAL_B_SPLINE_SURFACE ( (
 ( 1.000000000000000000, 0.8660254037844387076, 1.000000000000000000, 0.8660254037844387076, 1.000000000000000000, 0.8660254037844387076, 1.000000000000000000, 0.8660254037844387076, 1.000000000000000000, 0.8660254037844387076, 1.000000000000000000, 0.8660254037844387076, 1.000000000000000000, 0.8660254037844387076, 1.000000000000000000, 0.8660254037844387076, 1.000000000000000000, 0.8660254037844387076, 1.000000000000000000, 0.8660254037844387076, 1.000000000000000000, 0.8660254037844387076, 1.000000000000000000, 0.8660254037844387076, 1.000000000000000000, 0.8660254037844387076, 1.000000000000000000, 0.8660254037844387076, 1.000000000000000000, 0.8660254037844387076, 1.000000000000000000, 0.8660254037844387076, 1.000000000000000000, 0.8660254037844387076, 1.000000000000000000, 0.8660254037844387076, 1.000000000000000000, 0.8660254037844387076, 1.000000000000000000, 0.8660254037844387076, 1.000000000000000000, 0.8660254037844387076, 1.000000000000000000, 0.8660254037844387076, 1.000000000000000000, 0.8660254037844387076, 1.000000000000000000, 0.8660254037844387076, 1.000000000000000000, 0.8660254037844387076, 1.000000000000000000, 0.8660254037844387076, 1.000000000000000000, 0.8660254037844387076, 1.000000000000000000, 0.8660254037844387076, 1.000000000000000000, 0.8660254037844387076, 1.000000000000000000, 0.8660254037844387076, 1.000000000000000000, 0.8660254037844387076, 1.000000000000000000, 0.8660254037844387076, 1.000000000000000000, 0.8660254037844387076, 1.000000000000000000, 0.8660254037844387076, 1.000000000000000000, 0.8660254037844387076, 1.000000000000000000, 0.8660254037844387076, 1.000000000000000000, 0.8660254037844387076, 1.000000000000000000, 0.8660254037844387076, 1.000000000000000000, 0.8660254037844387076, 1.000000000000000000, 0.8660254037844387076, 1.000000000000000000, 0.8660254037844387076, 1.000000000000000000, 0.8660254037844387076, 1.000000000000000000, 0.8660254037844387076, 1.000000000000000000, 0.8660254037844387076, 1.000000000000000000, 0.8660254037844387076, 1.000000000000000000, 0.8660254037844387076, 1.000000000000000000, 0.8660254037844387076, 1.000000000000000000, 0.8660254037844387076, 1.000000000000000000, 0.8660254037844387076, 1.000000000000000000, 0.8660254037844387076, 1.000000000000000000, 0.8660254037844387076, 1.000000000000000000, 0.8660254037844387076, 1.000000000000000000, 0.8660254037844387076, 1.000000000000000000, 0.8660254037844387076, 1.000000000000000000, 0.8660254037844387076, 1.000000000000000000, 0.8660254037844387076, 1.000000000000000000, 0.8660254037844387076, 1.000000000000000000, 0.8660254037844387076, 1.000000000000000000, 0.8660254037844387076, 1.000000000000000000, 0.8660254037844387076, 1.000000000000000000, 0.8660254037844387076, 1.000000000000000000, 0.8660254037844387076, 1.000000000000000000, 0.8660254037844387076, 1.000000000000000000, 0.8660254037844387076, 1.000000000000000000, 0.8660254037844387076, 1.000000000000000000, 0.8660254037844387076, 1.000000000000000000, 0.8660254037844387076, 1.000000000000000000, 0.8660254037844387076, 1.000000000000000000, 0.8660254037844387076, 1.000000000000000000, 0.8660254037844387076, 1.000000000000000000, 0.8660254037844387076, 1.000000000000000000, 0.8660254037844387076, 1.000000000000000000, 0.8660254037844387076, 1.000000000000000000, 0.8660254037844387076, 1.000000000000000000, 0.8660254037844387076, 1.000000000000000000, 0.8660254037844387076, 1.000000000000000000, 0.8660254037844387076, 1.000000000000000000, 0.8660254037844387076, 1.000000000000000000, 0.8660254037844387076, 1.000000000000000000, 0.8660254037844387076, 1.000000000000000000, 0.8660254037844387076, 1.000000000000000000, 0.8660254037844387076, 1.000000000000000000, 0.8660254037844387076, 1.000000000000000000, 0.8660254037844387076, 1.000000000000000000, 0.8660254037844387076, 1.000000000000000000, 0.8660254037844387076, 1.000000000000000000, 0.8660254037844387076, 1.000000000000000000, 0.8660254037844387076, 1.000000000000000000, 0.8660254037844387076, 1.000000000000000000, 0.8660254037844387076, 1.000000000000000000, 0.8660254037844387076, 1.000000000000000000, 0.8660254037844387076, 1.000000000000000000, 0.8660254037844387076, 1.000000000000000000, 0.8660254037844387076, 1.000000000000000000, 0.8660254037844387076, 1.000000000000000000, 0.8660254037844387076, 1.000000000000000000, 0.8660254037844387076, 1.000000000000000000, 0.8660254037844387076, 1.000000000000000000, 0.8660254037844387076, 1.000000000000000000, 0.8660254037844387076, 1.000000000000000000, 0.8660254037844387076, 1.000000000000000000, 0.8660254037844387076, 1.000000000000000000, 0.8660254037844387076, 1.000000000000000000, 0.8660254037844387076, 1.000000000000000000, 0.8660254037844387076, 1.000000000000000000, 0.8660254037844387076, 1.000000000000000000, 0.8660254037844387076, 1.000000000000000000, 0.8660254037844387076, 1.000000000000000000, 0.8660254037844387076, 1.000000000000000000, 0.8660254037844387076, 1.000000000000000000, 0.8660254037844387076, 1.000000000000000000, 0.8660254037844387076, 1.000000000000000000, 0.8660254037844387076, 1.000000000000000000, 0.8660254037844387076, 1.000000000000000000, 0.8660254037844387076, 1.000000000000000000, 0.8660254037844387076, 1.000000000000000000, 0.8660254037844387076, 1.000000000000000000, 0.8660254037844387076, 1.000000000000000000, 0.8660254037844387076, 1.000000000000000000, 0.8660254037844387076, 1.000000000000000000, 0.8660254037844387076, 1.000000000000000000, 0.8660254037844387076, 1.000000000000000000, 0.8660254037844387076, 1.000000000000000000, 0.8660254037844387076, 1.000000000000000000, 0.8660254037844387076, 1.000000000000000000, 0.8660254037844387076, 1.000000000000000000, 0.8660254037844387076, 1.000000000000000000, 0.8660254037844387076, 1.000000000000000000, 0.8660254037844387076, 1.000000000000000000, 0.8660254037844387076, 1.000000000000000000, 0.8660254037844387076, 1.000000000000000000, 0.8660254037844387076, 1.000000000000000000, 0.8660254037844387076, 1.000000000000000000, 0.8660254037844387076, 1.000000000000000000, 0.8660254037844387076, 1.000000000000000000, 0.8660254037844387076, 1.000000000000000000, 0.8660254037844387076, 1.000000000000000000, 0.8660254037844387076, 1.000000000000000000, 0.8660254037844387076, 1.000000000000000000, 0.8660254037844387076, 1.000000000000000000, 0.8660254037844387076, 1.000000000000000000, 0.8660254037844387076, 1.000000000000000000, 0.8660254037844387076, 1.000000000000000000, 0.8660254037844387076, 1.000000000000000000, 0.8660254037844387076, 1.000000000000000000, 0.8660254037844387076, 1.000000000000000000, 0.8660254037844387076, 1.000000000000000000, 0.8660254037844387076, 1.000000000000000000, 0.8660254037844387076, 1.000000000000000000, 0.8660254037844387076, 1.000000000000000000, 0.8660254037844387076, 1.000000000000000000, 0.8660254037844387076, 1.000000000000000000, 0.8660254037844387076, 1.000000000000000000, 0.8660254037844387076, 1.000000000000000000, 0.8660254037844387076, 1.000000000000000000, 0.8660254037844387076, 1.000000000000000000, 0.8660254037844387076, 1.000000000000000000, 0.8660254037844387076, 1.000000000000000000, 0.8660254037844387076, 1.000000000000000000, 0.8660254037844387076, 1.000000000000000000, 0.8660254037844387076, 1.000000000000000000, 0.8660254037844387076, 1.000000000000000000, 0.8660254037844387076, 1.000000000000000000, 0.8660254037844387076, 1.000000000000000000, 0.8660254037844387076, 1.000000000000000000, 0.8660254037844387076, 1.000000000000000000, 0.8660254037844387076, 1.000000000000000000, 0.8660254037844387076, 1.000000000000000000, 0.8660254037844387076, 1.000000000000000000, 0.8660254037844387076, 1.000000000000000000, 0.8660254037844387076, 1.000000000000000000, 0.8660254037844387076, 1.000000000000000000, 0.8660254037844387076, 1.000000000000000000, 0.8660254037844387076, 1.000000000000000000, 0.8660254037844387076, 1.000000000000000000, 0.8660254037844387076, 1.000000000000000000, 0.8660254037844387076, 1.000000000000000000, 0.8660254037844387076, 1.000000000000000000, 0.8660254037844387076, 1.000000000000000000, 0.8660254037844387076, 1.000000000000000000, 0.8660254037844387076, 1.000000000000000000, 0.8660254037844387076, 1.000000000000000000, 0.8660254037844387076, 1.000000000000000000, 0.8660254037844387076, 1.000000000000000000, 0.8660254037844387076, 1.000000000000000000, 0.8660254037844387076, 1.000000000000000000, 0.8660254037844387076, 1.000000000000000000, 0.8660254037844387076, 1.000000000000000000, 0.8660254037844387076, 1.000000000000000000, 0.8660254037844387076, 1.000000000000000000, 0.8660254037844387076, 1.000000000000000000, 0.8660254037844387076, 1.000000000000000000, 0.8660254037844387076, 1.000000000000000000, 0.8660254037844387076, 1.000000000000000000, 0.8660254037844387076, 1.000000000000000000, 0.8660254037844387076, 1.000000000000000000, 0.8660254037844387076, 1.000000000000000000, 0.8660254037844387076, 1.000000000000000000, 0.8660254037844387076, 1.000000000000000000, 0.8660254037844387076, 1.000000000000000000, 0.8660254037844387076, 1.000000000000000000, 0.8660254037844387076, 1.000000000000000000, 0.8660254037844387076, 1.000000000000000000, 0.8660254037844387076, 1.000000000000000000, 0.8660254037844387076, 1.000000000000000000, 0.8660254037844387076, 1.000000000000000000, 0.8660254037844387076, 1.000000000000000000, 0.8660254037844387076, 1.000000000000000000, 0.8660254037844387076, 1.000000000000000000, 0.8660254037844387076, 1.000000000000000000, 0.8660254037844387076, 1.000000000000000000, 0.8660254037844387076, 1.000000000000000000, 0.8660254037844387076, 1.000000000000000000, 0.8660254037844387076, 1.000000000000000000, 0.8660254037844387076, 1.000000000000000000, 0.8660254037844387076, 1.000000000000000000, 0.8660254037844387076, 1.000000000000000000, 0.8660254037844387076, 1.000000000000000000, 0.8660254037844387076, 1.000000000000000000, 0.8660254037844387076, 1.000000000000000000, 0.8660254037844387076, 1.000000000000000000, 0.8660254037844387076, 1.000000000000000000, 0.8660254037844387076, 1.000000000000000000, 0.8660254037844387076, 1.000000000000000000, 0.8660254037844387076, 1.000000000000000000, 0.8660254037844387076, 1.000000000000000000, 0.8660254037844387076, 1.000000000000000000, 0.8660254037844387076, 1.000000000000000000, 0.8660254037844387076, 1.000000000000000000, 0.8660254037844387076, 1.000000000000000000, 0.8660254037844387076, 1.000000000000000000, 0.8660254037844387076, 1.000000000000000000, 0.8660254037844387076, 1.000000000000000000, 0.8660254037844387076, 1.000000000000000000, 0.8660254037844387076, 1.000000000000000000, 0.8660254037844387076, 1.000000000000000000, 0.8660254037844387076, 1.000000000000000000, 0.8660254037844387076, 1.000000000000000000, 0.8660254037844387076, 1.000000000000000000, 0.8660254037844387076, 1.000000000000000000),
 ( 1.000000000000000000, 0.8660254037844387076, 1.000000000000000000, 0.8660254037844387076, 1.000000000000000000, 0.8660254037844387076, 1.000000000000000000, 0.8660254037844387076, 1.000000000000000000, 0.8660254037844387076, 1.000000000000000000, 0.8660254037844387076, 1.000000000000000000, 0.8660254037844387076, 1.000000000000000000, 0.8660254037844387076, 1.000000000000000000, 0.8660254037844387076, 1.000000000000000000, 0.8660254037844387076, 1.000000000000000000, 0.8660254037844387076, 1.000000000000000000, 0.8660254037844387076, 1.000000000000000000, 0.8660254037844387076, 1.000000000000000000, 0.8660254037844387076, 1.000000000000000000, 0.8660254037844387076, 1.000000000000000000, 0.8660254037844387076, 1.000000000000000000, 0.8660254037844387076, 1.000000000000000000, 0.8660254037844387076, 1.000000000000000000, 0.8660254037844387076, 1.000000000000000000, 0.8660254037844387076, 1.000000000000000000, 0.8660254037844387076, 1.000000000000000000, 0.8660254037844387076, 1.000000000000000000, 0.8660254037844387076, 1.000000000000000000, 0.8660254037844387076, 1.000000000000000000, 0.8660254037844387076, 1.000000000000000000, 0.8660254037844387076, 1.000000000000000000, 0.8660254037844387076, 1.000000000000000000, 0.8660254037844387076, 1.000000000000000000, 0.8660254037844387076, 1.000000000000000000, 0.8660254037844387076, 1.000000000000000000, 0.8660254037844387076, 1.000000000000000000, 0.8660254037844387076, 1.000000000000000000, 0.8660254037844387076, 1.000000000000000000, 0.8660254037844387076, 1.000000000000000000, 0.8660254037844387076, 1.000000000000000000, 0.8660254037844387076, 1.000000000000000000, 0.8660254037844387076, 1.000000000000000000, 0.8660254037844387076, 1.000000000000000000, 0.8660254037844387076, 1.000000000000000000, 0.8660254037844387076, 1.000000000000000000, 0.8660254037844387076, 1.000000000000000000, 0.8660254037844387076, 1.000000000000000000, 0.8660254037844387076, 1.000000000000000000, 0.8660254037844387076, 1.000000000000000000, 0.8660254037844387076, 1.000000000000000000, 0.8660254037844387076, 1.000000000000000000, 0.8660254037844387076, 1.000000000000000000, 0.8660254037844387076, 1.000000000000000000, 0.8660254037844387076, 1.000000000000000000, 0.8660254037844387076, 1.000000000000000000, 0.8660254037844387076, 1.000000000000000000, 0.8660254037844387076, 1.000000000000000000, 0.8660254037844387076, 1.000000000000000000, 0.8660254037844387076, 1.000000000000000000, 0.8660254037844387076, 1.000000000000000000, 0.8660254037844387076, 1.000000000000000000, 0.8660254037844387076, 1.000000000000000000, 0.8660254037844387076, 1.000000000000000000, 0.8660254037844387076, 1.000000000000000000, 0.8660254037844387076, 1.000000000000000000, 0.8660254037844387076, 1.000000000000000000, 0.8660254037844387076, 1.000000000000000000, 0.8660254037844387076, 1.000000000000000000, 0.8660254037844387076, 1.000000000000000000, 0.8660254037844387076, 1.000000000000000000, 0.8660254037844387076, 1.000000000000000000, 0.8660254037844387076, 1.000000000000000000, 0.8660254037844387076, 1.000000000000000000, 0.8660254037844387076, 1.000000000000000000, 0.8660254037844387076, 1.000000000000000000, 0.8660254037844387076, 1.000000000000000000, 0.8660254037844387076, 1.000000000000000000, 0.8660254037844387076, 1.000000000000000000, 0.8660254037844387076, 1.000000000000000000, 0.8660254037844387076, 1.000000000000000000, 0.8660254037844387076, 1.000000000000000000, 0.8660254037844387076, 1.000000000000000000, 0.8660254037844387076, 1.000000000000000000, 0.8660254037844387076, 1.000000000000000000, 0.8660254037844387076, 1.000000000000000000, 0.8660254037844387076, 1.000000000000000000, 0.8660254037844387076, 1.000000000000000000, 0.8660254037844387076, 1.000000000000000000, 0.8660254037844387076, 1.000000000000000000, 0.8660254037844387076, 1.000000000000000000, 0.8660254037844387076, 1.000000000000000000, 0.8660254037844387076, 1.000000000000000000, 0.8660254037844387076, 1.000000000000000000, 0.8660254037844387076, 1.000000000000000000, 0.8660254037844387076, 1.000000000000000000, 0.8660254037844387076, 1.000000000000000000, 0.8660254037844387076, 1.000000000000000000, 0.8660254037844387076, 1.000000000000000000, 0.8660254037844387076, 1.000000000000000000, 0.8660254037844387076, 1.000000000000000000, 0.8660254037844387076, 1.000000000000000000, 0.8660254037844387076, 1.000000000000000000, 0.8660254037844387076, 1.000000000000000000, 0.8660254037844387076, 1.000000000000000000, 0.8660254037844387076, 1.000000000000000000, 0.8660254037844387076, 1.000000000000000000, 0.8660254037844387076, 1.000000000000000000, 0.8660254037844387076, 1.000000000000000000, 0.8660254037844387076, 1.000000000000000000, 0.8660254037844387076, 1.000000000000000000, 0.8660254037844387076, 1.000000000000000000, 0.8660254037844387076, 1.000000000000000000, 0.8660254037844387076, 1.000000000000000000, 0.8660254037844387076, 1.000000000000000000, 0.8660254037844387076, 1.000000000000000000, 0.8660254037844387076, 1.000000000000000000, 0.8660254037844387076, 1.000000000000000000, 0.8660254037844387076, 1.000000000000000000, 0.8660254037844387076, 1.000000000000000000, 0.8660254037844387076, 1.000000000000000000, 0.8660254037844387076, 1.000000000000000000, 0.8660254037844387076, 1.000000000000000000, 0.8660254037844387076, 1.000000000000000000, 0.8660254037844387076, 1.000000000000000000, 0.8660254037844387076, 1.000000000000000000, 0.8660254037844387076, 1.000000000000000000, 0.8660254037844387076, 1.000000000000000000, 0.8660254037844387076, 1.000000000000000000, 0.8660254037844387076, 1.000000000000000000, 0.8660254037844387076, 1.000000000000000000, 0.8660254037844387076, 1.000000000000000000, 0.8660254037844387076, 1.000000000000000000, 0.8660254037844387076, 1.000000000000000000, 0.8660254037844387076, 1.000000000000000000, 0.8660254037844387076, 1.000000000000000000, 0.8660254037844387076, 1.000000000000000000, 0.8660254037844387076, 1.000000000000000000, 0.8660254037844387076, 1.000000000000000000, 0.8660254037844387076, 1.000000000000000000, 0.8660254037844387076, 1.000000000000000000, 0.8660254037844387076, 1.000000000000000000, 0.8660254037844387076, 1.000000000000000000, 0.8660254037844387076, 1.000000000000000000, 0.8660254037844387076, 1.000000000000000000, 0.8660254037844387076, 1.000000000000000000, 0.8660254037844387076, 1.000000000000000000, 0.8660254037844387076, 1.000000000000000000, 0.8660254037844387076, 1.000000000000000000, 0.8660254037844387076, 1.000000000000000000, 0.8660254037844387076, 1.000000000000000000, 0.8660254037844387076, 1.000000000000000000, 0.8660254037844387076, 1.000000000000000000, 0.8660254037844387076, 1.000000000000000000, 0.8660254037844387076, 1.000000000000000000, 0.8660254037844387076, 1.000000000000000000, 0.8660254037844387076, 1.000000000000000000, 0.8660254037844387076, 1.000000000000000000, 0.8660254037844387076, 1.000000000000000000, 0.8660254037844387076, 1.000000000000000000, 0.8660254037844387076, 1.000000000000000000, 0.8660254037844387076, 1.000000000000000000, 0.8660254037844387076, 1.000000000000000000, 0.8660254037844387076, 1.000000000000000000, 0.8660254037844387076, 1.000000000000000000, 0.8660254037844387076, 1.000000000000000000, 0.8660254037844387076, 1.000000000000000000, 0.8660254037844387076, 1.000000000000000000, 0.8660254037844387076, 1.000000000000000000, 0.8660254037844387076, 1.000000000000000000, 0.8660254037844387076, 1.000000000000000000, 0.8660254037844387076, 1.000000000000000000, 0.8660254037844387076, 1.000000000000000000, 0.8660254037844387076, 1.000000000000000000, 0.8660254037844387076, 1.000000000000000000, 0.8660254037844387076, 1.000000000000000000, 0.8660254037844387076, 1.000000000000000000, 0.8660254037844387076, 1.000000000000000000, 0.8660254037844387076, 1.000000000000000000, 0.8660254037844387076, 1.000000000000000000, 0.8660254037844387076, 1.000000000000000000, 0.8660254037844387076, 1.000000000000000000, 0.8660254037844387076, 1.000000000000000000, 0.8660254037844387076, 1.000000000000000000, 0.8660254037844387076, 1.000000000000000000, 0.8660254037844387076, 1.000000000000000000, 0.8660254037844387076, 1.000000000000000000, 0.8660254037844387076, 1.000000000000000000, 0.8660254037844387076, 1.000000000000000000, 0.8660254037844387076, 1.000000000000000000, 0.8660254037844387076, 1.000000000000000000, 0.8660254037844387076, 1.000000000000000000, 0.8660254037844387076, 1.000000000000000000, 0.8660254037844387076, 1.000000000000000000, 0.8660254037844387076, 1.000000000000000000, 0.8660254037844387076, 1.000000000000000000, 0.8660254037844387076, 1.000000000000000000, 0.8660254037844387076, 1.000000000000000000, 0.8660254037844387076, 1.000000000000000000, 0.8660254037844387076, 1.000000000000000000, 0.8660254037844387076, 1.000000000000000000, 0.8660254037844387076, 1.000000000000000000, 0.8660254037844387076, 1.000000000000000000, 0.8660254037844387076, 1.000000000000000000, 0.8660254037844387076, 1.000000000000000000, 0.8660254037844387076, 1.000000000000000000, 0.8660254037844387076, 1.000000000000000000, 0.8660254037844387076, 1.000000000000000000, 0.8660254037844387076, 1.000000000000000000, 0.8660254037844387076, 1.000000000000000000, 0.8660254037844387076, 1.000000000000000000, 0.8660254037844387076, 1.000000000000000000, 0.8660254037844387076, 1.000000000000000000, 0.8660254037844387076, 1.000000000000000000, 0.8660254037844387076, 1.000000000000000000, 0.8660254037844387076, 1.000000000000000000, 0.8660254037844387076, 1.000000000000000000, 0.8660254037844387076, 1.000000000000000000, 0.8660254037844387076, 1.000000000000000000, 0.8660254037844387076, 1.000000000000000000, 0.8660254037844387076, 1.000000000000000000, 0.8660254037844387076, 1.000000000000000000, 0.8660254037844387076, 1.000000000000000000, 0.8660254037844387076, 1.000000000000000000, 0.8660254037844387076, 1.000000000000000000, 0.8660254037844387076, 1.000000000000000000, 0.8660254037844387076, 1.000000000000000000, 0.8660254037844387076, 1.000000000000000000, 0.8660254037844387076, 1.000000000000000000, 0.8660254037844387076, 1.000000000000000000, 0.8660254037844387076, 1.000000000000000000, 0.8660254037844387076, 1.000000000000000000, 0.8660254037844387076, 1.000000000000000000, 0.8660254037844387076, 1.000000000000000000, 0.8660254037844387076, 1.000000000000000000, 0.8660254037844387076, 1.000000000000000000, 0.8660254037844387076, 1.000000000000000000, 0.8660254037844387076, 1.000000000000000000, 0.8660254037844387076, 1.000000000000000000, 0.8660254037844387076, 1.000000000000000000, 0.8660254037844387076, 1.000000000000000000, 0.8660254037844387076, 1.000000000000000000, 0.8660254037844387076, 1.000000000000000000, 0.8660254037844387076, 1.000000000000000000, 0.8660254037844387076, 1.000000000000000000, 0.8660254037844387076, 1.000000000000000000) ) ) 
 REPRESENTATION_ITEM ( '' )  SURFACE ( )  );
#180363 = CARTESIAN_POINT ( 'NONE',  ( 3.426987366535645396, 0.04501397872612270673, 1.970993176858675699 ) ) ;
#180364 = CARTESIAN_POINT ( 'NONE',  ( 5.836178160628028522, -1.067892152678026951, -1.586260290404594597 ) ) ;
#180365 = VERTEX_POINT ( 'NONE', #63991 ) ;
#180366 = CARTESIAN_POINT ( 'NONE',  ( 6.725064210944283971, -1.800211566667491825, -0.7994317546313032263 ) ) ;
#180367 = CARTESIAN_POINT ( 'NONE',  ( 1.376788300709189450, 1.794419955772775355, -0.7429034522522351969 ) ) ;
#180368 = ORIENTED_EDGE ( 'NONE', *, *, #43321, .T. ) ;
#180369 = DIRECTION ( 'NONE',  ( 0.000000000000000000, 0.000000000000000000, 1.000000000000000000 ) ) ;
#180371 = CARTESIAN_POINT ( 'NONE',  ( 6.933015448541703485, 9.181880338089085214, 1.599625672291268286 ) ) ;
#180370 = CARTESIAN_POINT ( 'NONE',  ( -6.292392690518209264, 8.434487120394948079, -1.443375672974066548 ) ) ;
#180373 = CARTESIAN_POINT ( 'NONE',  ( 7.969495366734495434, 8.192166104145387706, 1.040834085586084257E-14 ) ) ;
#180372 = CARTESIAN_POINT ( 'NONE',  ( 2.238330470135694750, 0.4590858415520538416, 2.039436070248427324 ) ) ;
#180375 = CARTESIAN_POINT ( 'NONE',  ( 4.787437638956922648, 6.678706226906775179, -1.443375672974068769 ) ) ;
#180374 = CARTESIAN_POINT ( 'NONE',  ( 7.630541526392844887, 7.796719957080126662, 0.7998128361456341429 ) ) ;
#180377 = ORIENTED_EDGE ( 'NONE', *, *, #22239, .F. ) ;
#180376 = CARTESIAN_POINT ( 'NONE',  ( 5.848291733227988232, 0.9385554955868085081, -1.666026892748099009 ) ) ;
#180378 = CARTESIAN_POINT ( 'NONE',  ( 4.020313978404310262, -1.133593497508533110, -1.893353337301090233 ) ) ;
#180379 = CARTESIAN_POINT ( 'NONE',  ( 1.624349867039249329, -1.226448341774049267, -1.834376716147153363 ) ) ;
#180380 = CARTESIAN_POINT ( 'NONE',  ( -0.04225267894259204793, -6.625438066542577609, -11.00000000000012434 ) ) ;
#180381 = CARTESIAN_POINT ( 'NONE',  ( 0.3461628310420067911, 0.9829124436787042285, -1.640176041098049264 ) ) ;
#180382 = CARTESIAN_POINT ( 'NONE',  ( -5.101945877444165944, 4.846691699973280976, 0.000000000000000000 ) ) ;
#180383 = CARTESIAN_POINT ( 'NONE',  ( 8.550388431712704573, 13.12720360364021133, 0.000000000000000000 ) ) ;
#180384 = CARTESIAN_POINT ( 'NONE',  ( 4.070807014193541740, 1.466255041752505539, -1.461937513464212079 ) ) ;
#180386 = CARTESIAN_POINT ( 'NONE',  ( 1.569428280142046717, 0.1587979871724466974, -2.155937297210829495 ) ) ;
#180385 = CARTESIAN_POINT ( 'NONE',  ( -2.415323921528888196, 5.969628341758991930, 0.7998128361456341429 ) ) ;
#180387 = CARTESIAN_POINT ( 'NONE',  ( 3.790727848299980440, 1.850687065220711469, -1.173560875862532660 ) ) ;
#180388 = CARTESIAN_POINT ( 'NONE',  ( -1.225000000000040057, 0.7708333333333476922, 0.7072540797572656190 ) ) ;
#180389 = SURFACE_STYLE_USAGE ( .BOTH. , #97035 ) ;
#180390 = CARTESIAN_POINT ( 'NONE',  ( -6.732740262479597781, 15.44786667752632248, 9.889642727345355766 ) ) ;
#180391 = EDGE_CURVE ( 'NONE', #107567, #116778, #115995, .T. ) ;
#180392 = CARTESIAN_POINT ( 'NONE',  ( -1.364683531250010295, 14.44270833367473550, 0.7879004041258445001 ) ) ;
#180393 = CARTESIAN_POINT ( 'NONE',  ( -3.494969737272722643, 7.299491470118629088, -0.7998128361456481317 ) ) ;
#180394 = UNCERTAINTY_MEASURE_WITH_UNIT (LENGTH_MEASURE( 1.000000000000000082E-05 ), #122217, 'distance_accuracy_value', 'NONE');
#180395 = CARTESIAN_POINT ( 'NONE',  ( 0.7037502660087076034, 1.864169469917423161, 0.7691187473759173443 ) ) ;
#180396 = AXIS2_PLACEMENT_3D ( 'NONE', #189861, #171480, #159500 ) ;
#180397 = CARTESIAN_POINT ( 'NONE',  ( -10.14113571334194930, 10.93367254176152059, -0.7216878364870267237 ) ) ;
#180398 = CARTESIAN_POINT ( 'NONE',  ( 4.364170320198999420, -2.065056620294950740, 0.1471644388686063065 ) ) ;
#180399 = CARTESIAN_POINT ( 'NONE',  ( 3.633351821168579132, -1.779675539450284560, 0.7381315413402672609 ) ) ;
#180401 = EDGE_CURVE ( 'NONE', #51499, #176259, #46518, .T. ) ;
#180400 = CARTESIAN_POINT ( 'NONE',  ( 5.589508065689547500, -0.5136281568550029597, 2.053882654316901313 ) ) ;
#180402 = CARTESIAN_POINT ( 'NONE',  ( 5.452350330990040739, 9.512825819463730070, 0.7998128361456462443 ) ) ;
#180403 = CARTESIAN_POINT ( 'NONE',  ( 9.601861708076793178, 3.883749503203103526, 7.121442012218603956 ) ) ;
#180404 = CARTESIAN_POINT ( 'NONE',  ( 4.346514977827297344, -1.947402357529237626, -0.2931004117151541633 ) ) ;
#180405 = CARTESIAN_POINT ( 'NONE',  ( 6.509759575370489770, -1.074588918421373940, -2.024802758542126213 ) ) ;
#180406 = CARTESIAN_POINT ( 'NONE',  ( 4.459475772512963232, 0.3974328844052883447, -1.781742007231662983 ) ) ;
#180407 = PRODUCT_DEFINITION_SHAPE ( 'NONE', 'NONE',  #214417 ) ;
#180408 = CARTESIAN_POINT ( 'NONE',  ( 5.076602173674213070, 4.887400388900169368, 0.000000000000000000 ) ) ;
#180409 = CARTESIAN_POINT ( 'NONE',  ( 5.151735183068521629, 5.112705256442466428, 1.040834085586084257E-14 ) ) ;
#180410 = CARTESIAN_POINT ( 'NONE',  ( -5.447343857640614573, 9.577261277214532242, -0.7998128361456362523 ) ) ;
#180411 = CARTESIAN_POINT ( 'NONE',  ( 4.830447868218803897, 8.857549289555754157, -0.7998128361456481317 ) ) ;
#180412 = VERTEX_POINT ( 'NONE', #131191 ) ;
#180413 = CARTESIAN_POINT ( 'NONE',  ( 4.746344407351839045, 1.031357595523854309, -1.728805965807812095 ) ) ;
#180414 = CARTESIAN_POINT ( 'NONE',  ( 6.276074014454348315, 2.002121775873589637, -1.129333029253890341 ) ) ;
#180415 = CARTESIAN_POINT ( 'NONE',  ( 4.170719094083116474, 1.390339895272204362, -1.384257141873693087 ) ) ;
#180416 = CARTESIAN_POINT ( 'NONE',  ( -7.314787569772770226, 8.492672571945082183, -1.199719254218452935 ) ) ;
#180417 = CARTESIAN_POINT ( 'NONE',  ( -3.113568832632681360, 6.784247404713427798, -0.7998128361456281477 ) ) ;
#180418 = CARTESIAN_POINT ( 'NONE',  ( -10.43625799253213060, 3.019799309333130566, -6.025376361320772034 ) ) ;
#180419 = CARTESIAN_POINT ( 'NONE',  ( -7.110325215724114578, 7.260077271291732082, 0.000000000000000000 ) ) ;
#180421 = CARTESIAN_POINT ( 'NONE',  ( 5.998865924308096176, 1.444533723251522073, -1.022291996631684574 ) ) ;
#180420 = CARTESIAN_POINT ( 'NONE',  ( 0.2575178465553956686, 2.067414111102347185, -0.3107122069949171395 ) ) ;
#180422 = DIRECTION ( 'NONE',  ( -1.000000000000000000, 1.014813233446432150E-15, 1.972152263052529514E-31 ) ) ;
#180423 = CARTESIAN_POINT ( 'NONE',  ( 6.175724022258248347, -1.036883830621424307, 1.641789595683869729 ) ) ;
#180424 = CARTESIAN_POINT ( 'NONE',  ( 2.379091696419192381, 2.003018898301941686, -0.8894332929959417600 ) ) ;
#180425 = CARTESIAN_POINT ( 'NONE',  ( 1.083124124047912362, -0.7835505874942759741, 1.554128773191378432 ) ) ;
#180426 = TOROIDAL_SURFACE ( 'NONE', #14357, 3.971937515251341644, 0.08000000000000000167 ) ;
#180427 = CARTESIAN_POINT ( 'NONE',  ( 6.124532705071213279, 8.168374127381657246, -1.599625672291262513 ) ) ;
#180428 = CARTESIAN_POINT ( 'NONE',  ( 2.226796682701466246, -0.001291377463900899485, 1.725068445404242201 ) ) ;
#180429 = CARTESIAN_POINT ( 'NONE',  ( 1.329895901633147748, 1.076045675571284166, -1.909117696414885934 ) ) ;
#180430 = CARTESIAN_POINT ( 'NONE',  ( 4.266400587755204477, 1.039063272370500668, 1.946970035688735390 ) ) ;
#180431 = CARTESIAN_POINT ( 'NONE',  ( 1.868283874303029446, -2.155004017527381244, 0.2628641719419066991 ) ) ;
#180432 = CARTESIAN_POINT ( 'NONE',  ( 0.1350027811974127134, -1.670744041527939094, 0.7364786222084362954 ) ) ;
#180433 = CARTESIAN_POINT ( 'NONE',  ( 2.641944905847165792, 2.106676525318150972, -0.2125944600365035908 ) ) ;
#180434 = CARTESIAN_POINT ( 'NONE',  ( 6.639320575229253230, 6.038193673056963640, 2.491643636677738360 ) ) ;
#180435 = EDGE_CURVE ( 'NONE', #156791, #93013, #196133, .T. ) ;
#180436 = VERTEX_POINT ( 'NONE', #180930 ) ;
#180438 = CARTESIAN_POINT ( 'NONE',  ( -0.6823417656250246877, -0.1364583329919108468, 1.181850606188755259 ) ) ;
#180437 = CARTESIAN_POINT ( 'NONE',  ( 2.999882145774832143, -2.289621049425132338, 0.1149546659729560466 ) ) ;
#180439 = CARTESIAN_POINT ( 'NONE',  ( 2.683624340501134853, 5.218313266304903664, -1.199719254218446718 ) ) ;
#180440 = CARTESIAN_POINT ( 'NONE',  ( 4.222474775652216294, 7.013638773981186958, 1.199719254218462483 ) ) ;
#180441 = CIRCLE ( 'NONE', #35085, 1.220000000000001750 ) ;
#180442 = CARTESIAN_POINT ( 'NONE',  ( 4.653117599668723514, 0.3792583102804178985, 2.188544891856615049 ) ) ;
#180443 = CARTESIAN_POINT ( 'NONE',  ( -7.375272376154096143, 8.667201196010339004, -1.082531754730544860 ) ) ;
#180444 = CARTESIAN_POINT ( 'NONE',  ( 5.566601156340460044, 5.879629814773917218, -0.7777157291131882033 ) ) ;
#180445 = CARTESIAN_POINT ( 'NONE',  ( 4.148431816101584957, 6.823292304551739740, -1.082531754730548412 ) ) ;
#180446 = CARTESIAN_POINT ( 'NONE',  ( -6.846504384776758378, 9.010674420371453053, -1.443375672974058777 ) ) ;
#180447 = CARTESIAN_POINT ( 'NONE',  ( 4.068855497876973537, 7.761098824249525130, -0.7216878364870338292 ) ) ;
#180448 = ORIENTED_EDGE ( 'NONE', *, *, #42311, .F. ) ;
#180449 = CARTESIAN_POINT ( 'NONE',  ( 3.358046224211252095, 0.04667712216412447934, -2.016033814150198999 ) ) ;
#180451 = CARTESIAN_POINT ( 'NONE',  ( 2.729405006034294257, 0.1058063225414084541, -2.059999219628326994 ) ) ;
#180450 = CARTESIAN_POINT ( 'NONE',  ( 7.613066949273408213, 8.840665181362512115, -1.199719254218441611 ) ) ;
#180452 = DIRECTION ( 'NONE',  ( 1.040834085586084257E-15, 1.000000000000000000, -4.622230424712076367E-32 ) ) ;
#180453 = EDGE_CURVE ( 'NONE', #92739, #116046, #29351, .T. ) ;
#180454 = CARTESIAN_POINT ( 'NONE',  ( 3.716343503477301802, 7.349834830783237294, -1.734723475976807094E-15 ) ) ;
#180455 = CARTESIAN_POINT ( 'NONE',  ( -9.612263720970512182, -6.681311647492908179, 0.1963700886236081633 ) ) ;
#180456 = CARTESIAN_POINT ( 'NONE',  ( 1.364683531249988535, 4.155208333674753618, -0.7879004041258239610 ) ) ;
#180457 = CARTESIAN_POINT ( 'NONE',  ( 4.523480939507462217, -1.347072049868164978, -1.728447516733351952 ) ) ;
#180458 = CARTESIAN_POINT ( 'NONE',  ( 2.039685609654022347, -1.556907966322677472, 1.281362143053674130 ) ) ;
#180459 = CARTESIAN_POINT ( 'NONE',  ( 1.610644152589552958, -0.2245515952020246675, 1.827417025815617935 ) ) ;
#180460 = CARTESIAN_POINT ( 'NONE',  ( 6.435316467980822353, 10.65961964595298817, 1.040834085586084257E-14 ) ) ;
#180461 = SURFACE_STYLE_USAGE ( .BOTH. , #161016 ) ;
#180462 = CARTESIAN_POINT ( 'NONE',  ( 5.034128509002383289, 0.9373949799435166153, -1.566401400633938179 ) ) ;
#180463 = CARTESIAN_POINT ( 'NONE',  ( 6.434220164165640021, -1.621181005584397372, -1.198863592720422977 ) ) ;
#180464 = CARTESIAN_POINT ( 'NONE',  ( -6.828502922777144768, 11.11833717654868892, 0.7998128361456481317 ) ) ;
#180466 = CARTESIAN_POINT ( 'NONE',  ( -6.414942957921379474, 7.513130201443591005, -1.199719254218452047 ) ) ;
#180465 = CARTESIAN_POINT ( 'NONE',  ( 4.522535110384587220, 1.395170471642327437, -1.781064426588598426 ) ) ;
#180467 = CARTESIAN_POINT ( 'NONE',  ( 0.9792911203426227784, -0.05348914117170092131, -2.105562491362684252 ) ) ;
#180468 = B_SPLINE_CURVE_WITH_KNOTS ( 'NONE', 3,
 ( #160227, #31305, #47570, #177553, #175425, #111544, #45428, #60586, #97380, #129945, #113681, #179685, #163437, #208950, #15017, #147194, #109420, #27010 ),
 .UNSPECIFIED., .F., .F.,
 ( 4, 2, 2, 2, 2, 2, 2, 2, 4 ),
 ( 0.7103161267730502271, 0.7245945595572033104, 0.7388729923413562828, 0.7531514251255093662, 0.7674298579096623385, 0.7817082906938154219, 0.7959867234779685052, 0.8102651562621214776, 0.8245435890462745609 ),
 .UNSPECIFIED. ) ;
#180469 = CARTESIAN_POINT ( 'NONE',  ( -6.074935347375019390, 9.245119117649618801, 1.199719254218452047 ) ) ;
#180470 = CARTESIAN_POINT ( 'NONE',  ( 5.107906530550561541, 0.6527686194882609261, -1.964817160181751010 ) ) ;
#180471 = CARTESIAN_POINT ( 'NONE',  ( 8.646349277213076334, 11.11049346154719508, 1.599625672291281386 ) ) ;
#180472 = CARTESIAN_POINT ( 'NONE',  ( 4.014051167739200565, 7.807899849707989226, -0.3196577630155780225 ) ) ;
#180473 = CARTESIAN_POINT ( 'NONE',  ( -9.515124878692420296, 9.995400534762978850, 1.040834085586084257E-14 ) ) ;
#180474 = SURFACE_STYLE_USAGE ( .BOTH. , #114475 ) ;
#180475 = CARTESIAN_POINT ( 'NONE',  ( 5.664274315459256748, 9.830346811336296398, -0.7998128361456481317 ) ) ;
#180476 = CARTESIAN_POINT ( 'NONE',  ( 5.365762136054953224, 6.315268812753259020, -1.079746804988683806 ) ) ;
#180477 = CARTESIAN_POINT ( 'NONE',  ( -9.327646496521984076, 11.90534021740758064, -1.443375672974059665 ) ) ;
#180478 = CARTESIAN_POINT ( 'NONE',  ( 2.162617739553638785, 2.221014589654236371, 0.04931172913892957477 ) ) ;
#180479 = CARTESIAN_POINT ( 'NONE',  ( 5.011754246625688580, 8.023990808224052529, -1.135194352273690255 ) ) ;
#180480 = CARTESIAN_POINT ( 'NONE',  ( -5.887983850084758330, 10.09134126839936840, 0.7998128361456291469 ) ) ;
#180481 = CARTESIAN_POINT ( 'NONE',  ( 6.287230548435207567, 8.358188277972981695, -1.599625672291262513 ) ) ;
#180482 = CARTESIAN_POINT ( 'NONE',  ( 3.103904542773823660, 0.7086415210641981988, -1.829580771271981154 ) ) ;
#180483 = CARTESIAN_POINT ( 'NONE',  ( 4.449046963578762615, 8.342305224150557308, -0.7998128361456231517 ) ) ;
#180484 = CARTESIAN_POINT ( 'NONE',  ( -4.124159483505494883, 7.474427186445510962, 0.6511861734826256409 ) ) ;
#180485 = CARTESIAN_POINT ( 'NONE',  ( 3.979481780810941949, 4.601482484822914998, 1.199719254218464037 ) ) ;
#180486 = CARTESIAN_POINT ( 'NONE',  ( -6.482206841109545259, 6.735198534148810090, 0.7216878364870257245 ) ) ;
#180487 = CARTESIAN_POINT ( 'NONE',  ( -7.049876689426106680, 9.247942109129029475, -1.443375672974059665 ) ) ;
#180488 = CARTESIAN_POINT ( 'NONE',  ( 2.250376613284802207, 0.9954810856505689198, -1.872389709364124188 ) ) ;
#180489 = CARTESIAN_POINT ( 'NONE',  ( -5.424143973919053785, 8.485862515284315677, 1.199719254218454489 ) ) ;
#180490 = CARTESIAN_POINT ( 'NONE',  ( 5.248475795274027078, -1.946838731704622072, -0.2419367024937419397 ) ) ;
#180492 = CARTESIAN_POINT ( 'NONE',  ( 3.292016909520224743, -0.8776455207864016783, 1.975710135277891633 ) ) ;
#180491 = B_SPLINE_CURVE_WITH_KNOTS ( 'NONE', 3,
 ( #70864, #69311, #4304, #200385, #34698, #184144, #136492, #135422, #35767, #68248, #198256, #118159 ),
 .UNSPECIFIED., .F., .F.,
 ( 4, 2, 2, 2, 2, 4 ),
 ( 0.000000000000000000, 0.0007653844701297385540, 0.001530768940259477108, 0.001913461175324346819, 0.002296153410389216963, 0.003061537880518958119 ),
 .UNSPECIFIED. ) ;
#180493 = CARTESIAN_POINT ( 'NONE',  ( 2.929072846782492245, -1.238530643895646488, -1.362589426554157157 ) ) ;
#180494 = CONICAL_SURFACE ( 'NONE', #59413, 3.000000000000000000, 0.7853981633974523868 ) ;
#180495 = CARTESIAN_POINT ( 'NONE',  ( -4.014213326890253342, 7.626914324717730231, 0.01912188359321290165 ) ) ;
#180496 = CARTESIAN_POINT ( 'NONE',  ( -0.6823417656250246877, -0.6364583329919113464, 1.181850606188755259 ) ) ;
#180497 = CARTESIAN_POINT ( 'NONE',  ( 4.488070181461626618, -0.3849740463353290010, -1.697036094149968255 ) ) ;
#180498 = CARTESIAN_POINT ( 'NONE',  ( -3.946832114909622380, 7.618738210787626919, 0.7216878364870227269 ) ) ;
#180499 = CARTESIAN_POINT ( 'NONE',  ( 3.823036129373602154, 6.443664003369091731, -1.082531754730548412 ) ) ;
#180500 = CARTESIAN_POINT ( 'NONE',  ( -1.874318606243677236E-12, -8.296536394940149606, 10.41260094160982064 ) ) ;
#180501 = CARTESIAN_POINT ( 'NONE',  ( 2.061604318190731533, 0.3698614785779800185, -2.129673623264888960 ) ) ;
#180502 = CARTESIAN_POINT ( 'NONE',  ( 4.393907559866160994, 0.09612058942952760032, 2.013924333851605297 ) ) ;
#180503 = CARTESIAN_POINT ( 'NONE',  ( -8.256552360598034213, 11.61609960646427986, 1.082531754730549967 ) ) ;
#180504 = CARTESIAN_POINT ( 'NONE',  ( 0.9015118058452382677, 1.767791302423503685, 1.243857928393626633 ) ) ;
#180505 = CARTESIAN_POINT ( 'NONE',  ( 2.389859445797080095, -0.8464594663768022498, 1.780534303499915927 ) ) ;
#180506 = CARTESIAN_POINT ( 'NONE',  ( -6.607915433898670088, 6.755313035342081385, 0.3810012274577500579 ) ) ;
#180507 = CARTESIAN_POINT ( 'NONE',  ( 3.860829347334773232, 0.2347576860389360420, -1.927744540433872888 ) ) ;
#180510 = VERTEX_POINT ( 'NONE', #50937 ) ;
#180509 = DIRECTION ( 'NONE',  ( 0.000000000000000000, 1.000000000000000000, 0.000000000000000000 ) ) ;
#180508 = DIRECTION ( 'NONE',  ( 0.6507913734559627184, 0.7592566023653016805, 0.000000000000000000 ) ) ;
#180511 = CARTESIAN_POINT ( 'NONE',  ( -7.944151662964566540, 8.232874793072271657, 0.000000000000000000 ) ) ;
#180512 = CARTESIAN_POINT ( 'NONE',  ( 3.413620815590684199, 7.204584394822967752, 0.7998128361456281477 ) ) ;
#180514 = ORIENTED_EDGE ( 'NONE', *, *, #181170, .F. ) ;
#180513 = CARTESIAN_POINT ( 'NONE',  ( -4.847922445338252118, 7.813604065273374921, -1.199719254218453823 ) ) ;
#180515 = CARTESIAN_POINT ( 'NONE',  ( -7.334597914868722590, 11.50085530074811935, -0.7216878364870267237 ) ) ;
#180516 = CARTESIAN_POINT ( 'NONE',  ( 1.360703683432495259, 0.8952624662355921359, 2.017188127302282030 ) ) ;
#180517 = CARTESIAN_POINT ( 'NONE',  ( 1.642778471875000035, -1.976041666188709689, -2.845375778867859751 ) ) ;
#180518 = CARTESIAN_POINT ( 'NONE',  ( 5.207842308544940124, 0.6190457291245822224, -1.861560318597937913 ) ) ;
#180519 = CARTESIAN_POINT ( 'NONE',  ( 3.063770578283632862, 1.346675374253442969, 1.633852266970806211 ) ) ;
#180520 = CARTESIAN_POINT ( 'NONE',  ( 0.7499999999999885647, 2.847916667349487341, -1.299038105676658228 ) ) ;
#180521 = CARTESIAN_POINT ( 'NONE',  ( 4.646344025792163990, -1.477054284018078256, 1.098930429567553047 ) ) ;
#180522 = ORIENTED_EDGE ( 'NONE', *, *, #163335, .T. ) ;
#180523 = CARTESIAN_POINT ( 'NONE',  ( -8.193204901359996128, 8.453160561208463264, 1.040834085586084257E-14 ) ) ;
#180525 = EDGE_CURVE ( 'NONE', #77955, #126795, #5012, .T. ) ;
#180524 = CARTESIAN_POINT ( 'NONE',  ( 4.676102344489991403, 2.097148071331572439, -0.3138259731317455392 ) ) ;
#180526 = CARTESIAN_POINT ( 'NONE',  ( -5.546112223000226216, 5.929839062422638918, -0.8878705470019981894 ) ) ;
#180527 = CARTESIAN_POINT ( 'NONE',  ( 6.148786358997489820, 7.132337826040578754, -1.199719254218446718 ) ) ;
#180528 = ORIENTED_EDGE ( 'NONE', *, *, #124029, .F. ) ;
#180529 = CARTESIAN_POINT ( 'NONE',  ( 6.292271403379039896, -2.050439857688883372, -0.2063938634464974886 ) ) ;
#180532 = CARTESIAN_POINT ( 'NONE',  ( 3.544333174469185721, -1.503253232081468216, 1.062929765333266108 ) ) ;
#180531 = CARTESIAN_POINT ( 'NONE',  ( 0.2560159283585193846, -1.860519322180047785, -0.05176575080893807551 ) ) ;
#180530 = DIRECTION ( 'NONE',  ( -0.5620411653101037297, -0.8271092603138117116, 0.000000000000000000 ) ) ;
#180533 = CARTESIAN_POINT ( 'NONE',  ( 8.932124273304774320, 9.315233161810734686, 0.7998128361456462443 ) ) ;
#180534 = CARTESIAN_POINT ( 'NONE',  ( -11.35993080936265187, 3.555461883994699868, 3.691065267805003103 ) ) ;
#180535 = CARTESIAN_POINT ( 'NONE',  ( -6.119526231721793330, 8.232809585132461194, 1.599625672291263179 ) ) ;
#180536 = DIRECTION ( 'NONE',  ( 1.000000000000000000, 0.000000000000000000, 0.000000000000000000 ) ) ;
#180537 = CARTESIAN_POINT ( 'NONE',  ( 3.035963658818414235, -1.482449291622448095, -1.634993338104336891 ) ) ;
#180538 = CARTESIAN_POINT ( 'NONE',  ( 4.850980959722003938, -1.821092479232713446, 1.342276170020906711 ) ) ;
#180539 = CARTESIAN_POINT ( 'NONE',  ( -7.226132686403777150, 7.532835677000276675, 1.040834085586084257E-14 ) ) ;
#180540 = CARTESIAN_POINT ( 'NONE',  ( 5.730666697864316816, 1.210223194361861543, -1.348246716841319692 ) ) ;
#180541 = CARTESIAN_POINT ( 'NONE',  ( 5.647645028696767433, 1.886156043628923529, -0.3343808708002778407 ) ) ;
#180542 = CARTESIAN_POINT ( 'NONE',  ( 0.7499999999999885647, 3.097916667349487341, -1.299038105676658228 ) ) ;
#180543 = CARTESIAN_POINT ( 'NONE',  ( 5.770339134078734666, -1.185559297855027561, 1.446973003893243348 ) ) ;
#180544 = ADVANCED_FACE ( 'NONE', ( #188384 ), #122427, .F. ) ;
#180545 = CARTESIAN_POINT ( 'NONE',  ( 6.109776933011930922, 0.5395433811187456685, -1.781096067677762962 ) ) ;
#180546 = CYLINDRICAL_SURFACE ( 'NONE', #209608, 1.250000000000000000 ) ;
#180547 = CIRCLE ( 'NONE', #170019, 0.2999999999999999334 ) ;
#180548 = CARTESIAN_POINT ( 'NONE',  ( 6.174623306383559829, -1.681873830149778648, -0.5512017132776861894 ) ) ;
#180549 = CARTESIAN_POINT ( 'NONE',  ( 1.094935803221647186, 1.780670018850015079, 0.9462964651613046119 ) ) ;
#180551 = CARTESIAN_POINT ( 'NONE',  ( 3.422586708326117666, 1.336063110485498973, -1.628023012543792447 ) ) ;
#180550 = CARTESIAN_POINT ( 'NONE',  ( -2.779058300676980675, 5.225689869889666106, -1.082531754730543083 ) ) ;
#180552 = CARTESIAN_POINT ( 'NONE',  ( 8.289920859751990889, 11.75899253876431416, 1.199719254218450271 ) ) ;
#180554 = CARTESIAN_POINT ( 'NONE',  ( -9.179033691651859783, 10.66762638080401260, 1.199719254218462483 ) ) ;
#180553 = DIRECTION ( 'NONE',  ( 0.000000000000000000, 0.000000000000000000, 1.000000000000000000 ) ) ;
#180555 = CARTESIAN_POINT ( 'NONE',  ( 2.285421205933793942, 0.09476354472776055138, -2.017669629103500117 ) ) ;
#180556 = CARTESIAN_POINT ( 'NONE',  ( 1.364683531249986537, 2.405208333674752286, -0.7879004041258239610 ) ) ;
#180557 = CARTESIAN_POINT ( 'NONE',  ( 2.822068529938852155, 6.444163718237301275, -0.7998128361456291469 ) ) ;
#180558 = CARTESIAN_POINT ( 'NONE',  ( 3.690839692606663558, -0.4176960054509891163, -2.120685484085436112 ) ) ;
#180559 = CARTESIAN_POINT ( 'NONE',  ( 6.890000000000050306, -0.002781820520068867264, 1.999840353888074240 ) ) ;
#180562 = CARTESIAN_POINT ( 'NONE',  ( -15.75000000000000000, 12.69999999999999929, -1.800000000000001155 ) ) ;
#180561 = CARTESIAN_POINT ( 'NONE',  ( 11.86145016429273191, 10.19999999999999929, -1.100000000000000533 ) ) ;
#180560 = CARTESIAN_POINT ( 'NONE',  ( 5.571474780572990504, 5.464751763615448787, 0.7998128361456352531 ) ) ;
#180563 = CARTESIAN_POINT ( 'NONE',  ( 8.392133896734655707, 11.77427806529038357, 1.082531754730546636 ) ) ;
#180564 = CARTESIAN_POINT ( 'NONE',  ( -11.78331023100045627, 11.37999999999998302, 1.799999999999999600 ) ) ;
#180565 = CARTESIAN_POINT ( 'NONE',  ( -8.188761592974058701, 8.655902734665618325, -0.7216878364870278340 ) ) ;
#180566 = CARTESIAN_POINT ( 'NONE',  ( -1.402160292154681736E-14, 0.3218750003414227456, 1.575800808251672791 ) ) ;
#180567 = CARTESIAN_POINT ( 'NONE',  ( 1.365048776756357940, 0.1565470504056795942, -2.186014887712848243 ) ) ;
#180568 = CARTESIAN_POINT ( 'NONE',  ( 0.3138284133839603918, 8.211984188053584433, 1.978018658440966915 ) ) ;
#180569 = CARTESIAN_POINT ( 'NONE',  ( 3.151526295007577527, -1.848778841746369972, -1.303968314058404854 ) ) ;
#180570 = CARTESIAN_POINT ( 'NONE',  ( -9.020252271793614440, 9.418049160047695878, 0.7998128361456462443 ) ) ;
#180571 = CARTESIAN_POINT ( 'NONE',  ( -4.433153041544240835, 4.274359424664112339, 0.7216878364870317197 ) ) ;
#180572 = CARTESIAN_POINT ( 'NONE',  ( -1.201851678989727383E-14, 3.634375000341422357, 1.575800808251672791 ) ) ;
#180573 = CARTESIAN_POINT ( 'NONE',  ( 4.893454165248502186, 8.027304163657891678, -0.9628252682179049282 ) ) ;
#180574 = CARTESIAN_POINT ( 'NONE',  ( -6.009258394948636914E-15, 10.43750000000000178, -1.732050807568875195 ) ) ;
#180575 = CARTESIAN_POINT ( 'NONE',  ( 7.404161286838808920, 8.771181268467660885, -1.082531754730548412 ) ) ;
#180576 = CARTESIAN_POINT ( 'NONE',  ( 3.268565602506213974, -1.633896335792903054, -0.6804537918285047393 ) ) ;
#180577 = B_SPLINE_CURVE_WITH_KNOTS ( 'NONE', 3,
 ( #117473, #1489, #67554, #66487 ),
 .UNSPECIFIED., .F., .F.,
 ( 4, 4 ),
 ( 0.000000000000000000, 0.0005756945739314307765 ),
 .UNSPECIFIED. ) ;
#180578 = CARTESIAN_POINT ( 'NONE',  ( 3.141273780804701765, 0.05169848057553745602, 2.012594475454997145 ) ) ;
#180579 = CARTESIAN_POINT ( 'NONE',  ( 6.528370574810466564, 1.275976099532463381, -1.800301716031265764 ) ) ;
#180580 = CARTESIAN_POINT ( 'NONE',  ( -0.6823417656250003738, 9.651041667008065872, 1.181850606188754593 ) ) ;
#180581 = ORIENTED_EDGE ( 'NONE', *, *, #169868, .F. ) ;
#180582 = CARTESIAN_POINT ( 'NONE',  ( -6.635789839245807897, 6.706452665400368218, 0.7998128361456341429 ) ) ;
#180583 = CARTESIAN_POINT ( 'NONE',  ( 5.132435489663482286, 0.5880379476735001498, 1.928747580961232444 ) ) ;
#180584 = ORIENTED_EDGE ( 'NONE', *, *, #171517, .F. ) ;
#180585 = CARTESIAN_POINT ( 'NONE',  ( 2.096370420935515178, -0.4963513585865795275, -1.803540123670114736 ) ) ;
#180586 = CARTESIAN_POINT ( 'NONE',  ( 3.502843950909264592, 0.4983820457637299639, 2.009271733256080772 ) ) ;
#180587 = CARTESIAN_POINT ( 'NONE',  ( -5.750066545527201534, 9.722511713174800008, 0.000000000000000000 ) ) ;
#180588 = CARTESIAN_POINT ( 'NONE',  ( 2.039183100597967258, 0.003605121848727563250, 1.912571728241836633 ) ) ;
#180589 = FILL_AREA_STYLE_COLOUR ( '', #202339 ) ;
#180590 = CARTESIAN_POINT ( 'NONE',  ( -9.968662085647130411, 5.546348307810219147, -6.001034872913991514 ) ) ;
#180591 = CARTESIAN_POINT ( 'NONE',  ( -4.001066012398721838, 7.682011088333574378, -6.818990669119789124E-05 ) ) ;
#180592 = CARTESIAN_POINT ( 'NONE',  ( -1.201851678989727383E-14, 4.259375000341417028, -1.575800808251660134 ) ) ;
#180593 = CARTESIAN_POINT ( 'NONE',  ( 1.002048865836258518, -0.8573748960705519506, 1.709468765625526521 ) ) ;
#180594 = CARTESIAN_POINT ( 'NONE',  ( 3.139059813392345077, -0.1416510307416830594, -1.956792864499560691 ) ) ;
#180595 = CARTESIAN_POINT ( 'NONE',  ( 0.7903884775103053872, -1.915307795730587959, 0.6297756287277082032 ) ) ;
#180596 = CARTESIAN_POINT ( 'NONE',  ( -6.120580001926503755, 6.105374521861167914, -0.7998128361456362523 ) ) ;
#180598 = CARTESIAN_POINT ( 'NONE',  ( -11.33772463945037323, 12.59097530385348307, 3.599999999999999201 ) ) ;
#180597 = CARTESIAN_POINT ( 'NONE',  ( 9.257519960032755790, 9.694861462993381807, 0.7998128361456462443 ) ) ;
#180599 = CARTESIAN_POINT ( 'NONE',  ( 6.802032592820894230, -1.970958832386409565, 0.04617810802716794394 ) ) ;
#180600 = CARTESIAN_POINT ( 'NONE',  ( -1.364683531250012516, 2.280208333674751842, 0.7879004041258379498 ) ) ;
#180601 = CARTESIAN_POINT ( 'NONE',  ( 2.144791297303435762, 1.953827510466410455, 0.4849535144586021307 ) ) ;
#180603 = CARTESIAN_POINT ( 'NONE',  ( 1.845463042662376818, 0.3584012047737962781, -2.086523245552903472 ) ) ;
#180602 = CARTESIAN_POINT ( 'NONE',  ( -6.670248388243482651, 9.765411638717282017, 1.082531754730548412 ) ) ;
#180604 = CARTESIAN_POINT ( 'NONE',  ( -15.75000000000000000, 10.19999999999999929, -1.100000000000000311 ) ) ;
#180605 = CARTESIAN_POINT ( 'NONE',  ( 3.684089399883890614, -1.230936008959164996, -1.664559344884769088 ) ) ;
#180606 = CARTESIAN_POINT ( 'NONE',  ( 4.061549535745618833, 6.896169004081968090, -1.199719254218452047 ) ) ;
#180608 = CARTESIAN_POINT ( 'NONE',  ( 5.379888026524302980, 5.170957540566797128, -0.7998128361456211532 ) ) ;
#180607 = CARTESIAN_POINT ( 'NONE',  ( 5.982390446235332782, -0.3055207467456683701, -2.068066053634140200 ) ) ;
#180610 = ORIENTED_EDGE ( 'NONE', *, *, #510, .F. ) ;
#180609 = CARTESIAN_POINT ( 'NONE',  ( 4.577060434696750946, -0.0006114206978560799951, -1.825762228460731551 ) ) ;
#180611 = CARTESIAN_POINT ( 'NONE',  ( 8.890396042259068210, 11.39521468743417998, -1.599625672291257406 ) ) ;
#180612 = CARTESIAN_POINT ( 'NONE',  ( -1.084637062511542016, 2.867628807292011750, -1.105835307554790647 ) ) ;
#180613 = CARTESIAN_POINT ( 'NONE',  ( 8.857939311156123097, 13.09004391473939677, -7.626805567664353802 ) ) ;
#180614 = CARTESIAN_POINT ( 'NONE',  ( 6.335036379411270957, 0.2100110484798515254, 2.196758413611602290 ) ) ;
#180615 = CARTESIAN_POINT ( 'NONE',  ( -1.364683531250000748, 10.67187500034139802, 0.000000000000000000 ) ) ;
#180616 = VERTEX_POINT ( 'NONE', #120272 ) ;
#180617 = CARTESIAN_POINT ( 'NONE',  ( 4.723256143441832755, 1.665581346147155806, 0.9393396248940300008 ) ) ;
#180618 = CARTESIAN_POINT ( 'NONE',  ( -2.286521462199063492, 5.819358805874190743, 1.040834085586084257E-14 ) ) ;
#180619 = CIRCLE ( 'NONE', #139065, 1.359291649810832503 ) ;
#180620 = CARTESIAN_POINT ( 'NONE',  ( 7.983053520348166288, 8.207983950027992748, -0.7998128361456281477 ) ) ;
#180621 = VECTOR ( 'NONE', #135595, 1000.000000000000000 ) ;
#180622 = CARTESIAN_POINT ( 'NONE',  ( -1.360316468750030428, 1.171875000341417117, -4.336808689942017736E-14 ) ) ;
#180623 = CARTESIAN_POINT ( 'NONE',  ( 5.653386866774156694, 5.697965554099049257, -0.7216878364870207285 ) ) ;
#180624 = CARTESIAN_POINT ( 'NONE',  ( 10.98997987423604172, -6.893137084989842123, -0.4694063952341842594 ) ) ;
#180626 = EDGE_CURVE ( 'NONE', #6713, #59141, #72792, .T. ) ;
#180625 = CARTESIAN_POINT ( 'NONE',  ( 2.580963302752299349, 0.4788041664877049075, 0.000000000000000000 ) ) ;
#180627 = CARTESIAN_POINT ( 'NONE',  ( 0.2746299231596514012, 1.718356743839201561, -0.6618312839273902126 ) ) ;
#180628 = ORIENTED_EDGE ( 'NONE', *, *, #200627, .F. ) ;
#180629 = CARTESIAN_POINT ( 'NONE',  ( -6.400331034103001748, 9.624747418832267698, 1.199719254218452935 ) ) ;
#180630 = EDGE_CURVE ( 'NONE', #10241, #21185, #53057, .T. ) ;
#180631 = CARTESIAN_POINT ( 'NONE',  ( 4.762891570102392613, -1.670096840553733752, -0.8426394062573672183 ) ) ;
#180632 = CARTESIAN_POINT ( 'NONE',  ( 0.07661050522434449672, 6.948789054712463553, -2.305832378935098514 ) ) ;
#180633 = CARTESIAN_POINT ( 'NONE',  ( 7.842465510862060896, 8.114240948952696542, 0.000000000000000000 ) ) ;
#180634 = CARTESIAN_POINT ( 'NONE',  ( -0.08058608058608696112, -5.907420853759267843, 10.99970480893081870 ) ) ;
#180635 = CARTESIAN_POINT ( 'NONE',  ( -8.026063749610063525, 8.466088584074293877, -0.7216878364870278340 ) ) ;
#180636 = CARTESIAN_POINT ( 'NONE',  ( 6.010342169559767633, 5.906487374108181143, -0.7998128361456281477 ) ) ;
#180637 = CARTESIAN_POINT ( 'NONE',  ( 0.7077770966438132749, 0.6232387800201264483, -1.868272854783992187 ) ) ;
#180638 = CARTESIAN_POINT ( 'NONE',  ( 2.109000121467627498, 0.002830143620808495131, 2.016598147190066914 ) ) ;
#180639 = CARTESIAN_POINT ( 'NONE',  ( -7.133561379084627063, 11.47423870890741782, 0.7998128361456481317 ) ) ;
#180640 = CARTESIAN_POINT ( 'NONE',  ( 5.662465432362883355, 6.635239754958710989, 1.199719254218451159 ) ) ;
#180641 = CARTESIAN_POINT ( 'NONE',  ( 6.770610912236884715, -7.154544010627095219, 6.663994888585883736 ) ) ;
#180642 = CARTESIAN_POINT ( 'NONE',  ( 2.115410589380119610, -2.125216164159982046, 0.5342070311455533460 ) ) ;
#180643 = CARTESIAN_POINT ( 'NONE',  ( -0.3769810270651957618, 3.049942316455299451, -0.4288785890453079008 ) ) ;
#180644 = CARTESIAN_POINT ( 'NONE',  ( -8.448702279610222021, 13.00856975952063088, 1.040834085586084257E-14 ) ) ;
#180645 = CARTESIAN_POINT ( 'NONE',  ( -1.499999999999997780, 3.400000000000021227, 1.214306433183764966E-14 ) ) ;
#180646 = LINE ( 'NONE', #113590, #205718 ) ;
#180647 = ADVANCED_FACE ( 'NONE', ( #5336 ), #103958, .F. ) ;
#180648 = CARTESIAN_POINT ( 'NONE',  ( -10.19200560444942560, 4.477620260464512114, -5.707107691925500603 ) ) ;
#180649 = CARTESIAN_POINT ( 'NONE',  ( 8.422639742587595180, 10.84949900448412130, -1.599625672291268286 ) ) ;
#180650 = CARTESIAN_POINT ( 'NONE',  ( 6.396834479292349052, -8.176568542494905500, 7.055228938194280985 ) ) ;
#180651 = CARTESIAN_POINT ( 'NONE',  ( 7.539742822975472158, 7.968990512992423447, -0.7216878364870317197 ) ) ;
#180652 = VERTEX_POINT ( 'NONE', #54136 ) ;
#180654 = CARTESIAN_POINT ( 'NONE',  ( 2.033841672972019676, -1.952135521142538854, 0.4911360252713212193 ) ) ;
#180653 = CARTESIAN_POINT ( 'NONE',  ( 4.370544011308346910, -0.004580445953385886559, -1.841430844414258861 ) ) ;
#180655 = CARTESIAN_POINT ( 'NONE',  ( 3.339543098909302898, -1.371423271284638590, 1.844254897846734131 ) ) ;
#180657 = CARTESIAN_POINT ( 'NONE',  ( 0.8130640335680532349, -1.568041438259277554, -1.001899246494031948 ) ) ;
#180656 = CARTESIAN_POINT ( 'NONE',  ( -0.7500000000000006661, 9.958333333333332149, -1.299038105676657340 ) ) ;
#180658 = CARTESIAN_POINT ( 'NONE',  ( -1.642778471875000035, -1.917708332855375897, -2.845375778867859751 ) ) ;
#180659 = SURFACE_SIDE_STYLE ('',( #14934 ) ) ;
#180660 = CARTESIAN_POINT ( 'NONE',  ( 5.502191098127390489, -0.8541586074963626318, 1.711093258865265643 ) ) ;
#180661 = CARTESIAN_POINT ( 'NONE',  ( -7.862839020921525091, 11.26073039346208660, -1.199719254218446718 ) ) ;
#180662 = CARTESIAN_POINT ( 'NONE',  ( -7.282137904315833410, 7.668451441222825515, 0.000000000000000000 ) ) ;
#180664 = CARTESIAN_POINT ( 'NONE',  ( 3.801501934187266230, -0.5436965770258190833, 1.789884385262895616 ) ) ;
#180663 = CARTESIAN_POINT ( 'NONE',  ( 3.544548742447044987, -1.707904676211311479, 1.205638247120393247 ) ) ;
#180665 = CARTESIAN_POINT ( 'NONE',  ( 6.155038550924133212, 10.12470270947942730, 0.7216878364870438212 ) ) ;
#180666 = CARTESIAN_POINT ( 'NONE',  ( 5.618664544990171095, -0.03892770779775727580, 1.841008343696965310 ) ) ;
#180668 = CARTESIAN_POINT ( 'NONE',  ( 5.542585869888291938, 5.360771691158120689, -0.7998128361456211532 ) ) ;
#180667 = CARTESIAN_POINT ( 'NONE',  ( -4.229780737783618072, 6.918199379847403740, 1.082531754730560403 ) ) ;
#180669 = CARTESIAN_POINT ( 'NONE',  ( 5.426277463695272196, 1.022757762066462961, -1.388784613272223689 ) ) ;
#180670 = CARTESIAN_POINT ( 'NONE',  ( -7.576308911938196999, 7.733448573549685179, 0.7998128361456462443 ) ) ;
#180671 = CARTESIAN_POINT ( 'NONE',  ( 0.6153164582703105623, 0.1250789957258427176, 1.729716150945133535 ) ) ;
#180672 = SURFACE_STYLE_FILL_AREA ( #162305 ) ;
#180673 = CARTESIAN_POINT ( 'NONE',  ( 1.911175648939857030, 3.243131119507701943, 0.4542559028653122555 ) ) ;
#180674 = CARTESIAN_POINT ( 'NONE',  ( 9.579417154662843714, -9.998067499250630874, -0.08973735058632786865 ) ) ;
#180675 = CARTESIAN_POINT ( 'NONE',  ( 5.084931552659712750, 2.075598280349931546, 0.6366630897998347693 ) ) ;
#180676 = CARTESIAN_POINT ( 'NONE',  ( 3.158640206316553289, -1.382037546686708973, 1.193037399656725395 ) ) ;
#180677 = CARTESIAN_POINT ( 'NONE',  ( 1.639427129605858902, 1.814645582613241714, -0.7458448512465406521 ) ) ;
#180678 = CARTESIAN_POINT ( 'NONE',  ( 5.893796404173470727, -2.101076160772547219, 0.2616963346634570975 ) ) ;
#180680 = CARTESIAN_POINT ( 'NONE',  ( -1.201851678989727383E-14, 3.759375000341422801, -1.575800808251660134 ) ) ;
#180679 = CARTESIAN_POINT ( 'NONE',  ( 5.689115845898126800, 1.733752489355618875, 1.499825188574270607 ) ) ;
#180681 = CARTESIAN_POINT ( 'NONE',  ( 7.781490099239519509, 11.16582331816642260, 1.199719254218460707 ) ) ;
#180682 = CARTESIAN_POINT ( 'NONE',  ( 1.594549238318817785, -1.131586138893545979, 1.793127659086241499 ) ) ;
#180683 = CARTESIAN_POINT ( 'NONE',  ( -4.284013352238265959, 5.060732334775157604, -1.082531754730544860 ) ) ;
#180684 = CARTESIAN_POINT ( 'NONE',  ( 2.290347054751562528, 1.000000000000000888, -11.71088463649530453 ) ) ;
#180685 = CARTESIAN_POINT ( 'NONE',  ( -5.382223794500852421, 5.381608636446842731, -0.7216878364870197293 ) ) ;
#180686 = VECTOR ( 'NONE', #35988, 1000.000000000000000 ) ;
#180687 = CARTESIAN_POINT ( 'NONE',  ( 6.403213944470495633, -1.838587781526521248, 1.154350301468348272 ) ) ;
#180689 = CARTESIAN_POINT ( 'NONE',  ( -6.009258394948636914E-15, 12.71875000068280137, -1.732050807568875195 ) ) ;
#180688 = CARTESIAN_POINT ( 'NONE',  ( 6.883263157960330503, 2.417872181280413812, 2.534681901920758929 ) ) ;
#180691 = EDGE_LOOP ( 'NONE', ( #153878, #207674 ) ) ;
#180690 = CARTESIAN_POINT ( 'NONE',  ( 2.209928731909744481, 1.719286606775907611, 1.406518386542881638 ) ) ;
#180692 = CARTESIAN_POINT ( 'NONE',  ( 6.029922689959810178, -1.701949372586025744, 1.081063231324945528 ) ) ;
#180694 = CARTESIAN_POINT ( 'NONE',  ( 5.049704294756152123, 1.524832160660544611, 1.389060530156678297 ) ) ;
#180693 = CARTESIAN_POINT ( 'NONE',  ( 4.467575310902914154, 5.170924936596891008, 1.199719254218464037 ) ) ;
#180696 = CARTESIAN_POINT ( 'NONE',  ( -0.2409995289980037536, -0.004801160710915518791, -2.000252362011435192 ) ) ;
#180695 = CARTESIAN_POINT ( 'NONE',  ( 4.681308178468477799, 8.683552984847038303, 0.000000000000000000 ) ) ;
#180697 = ADVANCED_FACE ( 'NONE', ( #204617 ), #117148, .F. ) ;
#180698 = CARTESIAN_POINT ( 'NONE',  ( 6.412080304620304538, 6.445458208337293549, -0.7998128361456481317 ) ) ;
#180699 = CARTESIAN_POINT ( 'NONE',  ( 1.642778471875001811, -3.580208332855376430, 2.845375778867859751 ) ) ;
#180700 = DIRECTION ( 'NONE',  ( 0.6507913734559641616, -0.7592566023653004592, 0.000000000000000000 ) ) ;
#180701 = CARTESIAN_POINT ( 'NONE',  ( 4.634224865634020141, 0.3196297827482602050, 1.813140464320086132 ) ) ;
#180702 = EDGE_CURVE ( 'NONE', #63064, #206426, #77735, .T. ) ;
#180703 = CARTESIAN_POINT ( 'NONE',  ( 6.166260936116925606, 6.088392601758203071, 0.7998128361456341429 ) ) ;
#180704 = CARTESIAN_POINT ( 'NONE',  ( -0.2104748580754183807, 2.005809028216706924, -2.517884123765606663 ) ) ;
#180705 = CARTESIAN_POINT ( 'NONE',  ( 1.359898630301906053, 0.6939498547450100308, 1.579201994853156821 ) ) ;
#180706 = CARTESIAN_POINT ( 'NONE',  ( -0.1706859984542466180, -1.561801110730935971, -1.275320528755889526 ) ) ;
#180707 = CARTESIAN_POINT ( 'NONE',  ( 2.145563594533715257, 0.9871410470321148045, 2.076082784368099787 ) ) ;
#180708 = CARTESIAN_POINT ( 'NONE',  ( 1.364683531249988535, 3.426041667008085323, 0.7879004041258500513 ) ) ;
#180709 = CARTESIAN_POINT ( 'NONE',  ( 1.177466099744011174, -0.05591215127281846942, -2.261859306125458158 ) ) ;
#180710 = CARTESIAN_POINT ( 'NONE',  ( 4.705754021700633949, -0.5625300431781330435, 2.029483779808038957 ) ) ;
#180711 = CARTESIAN_POINT ( 'NONE',  ( -3.851398154733808088, 6.650992392901508232, -1.199719254218450271 ) ) ;
#180712 = CARTESIAN_POINT ( 'NONE',  ( 2.038023431533928509, 1.749628755847471018, 0.2652362932685590757 ) ) ;
#180713 = CARTESIAN_POINT ( 'NONE',  ( 7.623762449586013901, 7.788811034138823253, 1.040834085586084257E-14 ) ) ;
#180714 = CARTESIAN_POINT ( 'NONE',  ( 5.844973620822844218, 6.952128991449046502, 1.082531754730549967 ) ) ;
#180715 = CARTESIAN_POINT ( 'NONE',  ( -6.762819695118240659, 6.784377820593065600, 0.7998128361456341429 ) ) ;
#180716 = CARTESIAN_POINT ( 'NONE',  ( 0.7499999999999885647, 2.316666666666689078, -1.299038105676652899 ) ) ;
#180717 = COLOUR_RGB ( '', 0.66274510, 0.83137255, 0.94901961) ;
#180719 = CARTESIAN_POINT ( 'NONE',  ( 5.572587854402127228, 0.9002147710611071441, 2.031021293335387501 ) ) ;
#180718 = CARTESIAN_POINT ( 'NONE',  ( 2.549219474610735947, 0.2639673528169217964, 2.104066465523121376 ) ) ;
#180720 = CARTESIAN_POINT ( 'NONE',  ( 3.222796723461582413, 0.05406831605479084368, 2.190948157972896659 ) ) ;
#180721 = CARTESIAN_POINT ( 'NONE',  ( -3.574546055497324737, 7.322054164722185732, 0.7998128361456341429 ) ) ;
#180722 = CARTESIAN_POINT ( 'NONE',  ( -11.94980361058168938, 10.19999999999999929, 1.099999999999996980 ) ) ;
#180723 = CARTESIAN_POINT ( 'NONE',  ( 6.375647721065083928, 0.3630326626483972308, -2.089014862189771726 ) ) ;
#180724 = CARTESIAN_POINT ( 'NONE',  ( 0.6823417656249899377, 3.426041667008085323, -1.181850606188754593 ) ) ;
#180725 = CARTESIAN_POINT ( 'NONE',  ( 6.610000000000030518, 1.266345627986571021, 2.115470293623383569 ) ) ;
#180726 = CARTESIAN_POINT ( 'NONE',  ( -5.287316719649550301, 5.270883715786984780, 0.7216878364870317197 ) ) ;
#180727 = CARTESIAN_POINT ( 'NONE',  ( 5.625269520628737752, 1.871107552910089122, 0.9978724776121964402 ) ) ;
#180728 = CARTESIAN_POINT ( 'NONE',  ( -7.282137904315833410, 7.668451441222825515, 0.000000000000000000 ) ) ;
#180729 = ORIENTED_EDGE ( 'NONE', *, *, #151802, .T. ) ;
#180731 = CARTESIAN_POINT ( 'NONE',  ( 1.469576158976824144E-15, 3.481540744127368026, 12.00000000000000178 ) ) ;
#180730 = CARTESIAN_POINT ( 'NONE',  ( -4.150204419558982671, 7.856005899545188242, 0.7216878364870338292 ) ) ;
#180732 = CARTESIAN_POINT ( 'NONE',  ( 5.412729640353754590, 7.337937218544611895, 1.599625672291267398 ) ) ;
#180733 = CARTESIAN_POINT ( 'NONE',  ( 6.093280168761200599, -0.6138376400152152357, 1.736067454429328416 ) ) ;
#180734 = CARTESIAN_POINT ( 'NONE',  ( 0.000000000000000000, 0.4000000000000010214, 0.000000000000000000 ) ) ;
#180735 = CARTESIAN_POINT ( 'NONE',  ( -1.364683531250012516, 4.551041667008082214, -0.7879004041258300672 ) ) ;
#180736 = CARTESIAN_POINT ( 'NONE',  ( 1.856607919947508956, 0.2971036446917668106, -1.714703581143263156 ) ) ;
#180737 = CARTESIAN_POINT ( 'NONE',  ( 4.383363735919856730, 4.008345868194933104, -0.7998128361456211532 ) ) ;
#180738 = CARTESIAN_POINT ( 'NONE',  ( 11.80247861663003484, 12.29999999999998295, 1.695431928471866190 ) ) ;
#180739 = CARTESIAN_POINT ( 'NONE',  ( -1.364683531250014514, 0.09270833367475767028, 0.7879004041258379498 ) ) ;
#180740 = CARTESIAN_POINT ( 'NONE',  ( -0.3999999999999979683, 3.322650755865472760, -0.5865692111442778467 ) ) ;
#180741 = CARTESIAN_POINT ( 'NONE',  ( 6.034075718726629844, 1.069613854859407631, -1.878468107683453514 ) ) ;
#180742 = B_SPLINE_CURVE_WITH_KNOTS ( 'NONE', 3,
 ( #90982, #172222, #191635, #125675, #43299, #171138, #109419 ),
 .UNSPECIFIED., .F., .F.,
 ( 4, 3, 4 ),
 ( 0.000000000000000000, 2.778001202718379905E-05, 5.460790091229219688E-05 ),
 .UNSPECIFIED. ) ;
#180743 = CARTESIAN_POINT ( 'NONE',  ( -3.918470089549458635, 4.530302178351167441, -1.199719254218452047 ) ) ;
#180744 = CARTESIAN_POINT ( 'NONE',  ( -6.521108698048779573, 8.631046119188804155, -1.443375672974058777 ) ) ;
#180745 = CARTESIAN_POINT ( 'NONE',  ( 5.541917325712655717, 0.8799508658935292216, -1.974686638939105343 ) ) ;
#180747 = VERTEX_POINT ( 'NONE', #152696 ) ;
#180746 = DIRECTION ( 'NONE',  ( -0.000000000000000000, 1.000000000000000000, -0.000000000000000000 ) ) ;
#180748 = CARTESIAN_POINT ( 'NONE',  ( -1.201851678989727383E-14, 2.946875000341419248, -1.575800808251660134 ) ) ;
#180749 = CARTESIAN_POINT ( 'NONE',  ( 5.940691962724923059, 0.3820465716247494758, 1.933821394355714096 ) ) ;
#180750 = CARTESIAN_POINT ( 'NONE',  ( 5.061730935934568798, 1.440722419422343803, -0.9642406207952100017 ) ) ;
#180752 = CARTESIAN_POINT ( 'NONE',  ( 2.454835928891830221, -1.908367152989149718, -1.077367144120815023 ) ) ;
#180751 = CARTESIAN_POINT ( 'NONE',  ( -1.360316468750021768, -1.109374999658574446, -3.122502256758252770E-14 ) ) ;
#180753 = CARTESIAN_POINT ( 'NONE',  ( 3.786388324757625323, -1.140120265720317327, 2.006200910446949592 ) ) ;
#180754 = CARTESIAN_POINT ( 'NONE',  ( 4.622373940358720290, 1.271062617260295458, -1.621988140548079826 ) ) ;
#180755 = CARTESIAN_POINT ( 'NONE',  ( 0.7263842893957738189, 0.1423072432159468159, 1.936797167885440096 ) ) ;
#180756 = CARTESIAN_POINT ( 'NONE',  ( -7.090551149822745813, 9.295395646258437949, 1.443375672974078761 ) ) ;
#180757 = CARTESIAN_POINT ( 'NONE',  ( -5.178288325776719603, 5.006034233019745372, 0.000000000000000000 ) ) ;
#180758 = CYLINDRICAL_SURFACE ( 'NONE', #43914, 0.07999999999999998779 ) ;
#180759 = CARTESIAN_POINT ( 'NONE',  ( 4.306960158517386894, -0.4675538901007176285, -2.068242682749166672 ) ) ;
#180760 = CARTESIAN_POINT ( 'NONE',  ( 3.894033820048811823, 8.999999999999998224, -0.7749999999999996891 ) ) ;
#180761 = CARTESIAN_POINT ( 'NONE',  ( 1.758435621656749603, 1.928751379572872571, -0.5880216644931559600 ) ) ;
#180762 = CARTESIAN_POINT ( 'NONE',  ( -6.521108698048783126, 7.670676904887464786, -1.082531754730543083 ) ) ;
#180763 = CARTESIAN_POINT ( 'NONE',  ( 4.208205882762393379, -2.201082536721191474, 0.1591639695062776749 ) ) ;
#180764 = CARTESIAN_POINT ( 'NONE',  ( -3.602337597214539753E-15, 12.81249999999999822, 1.500000000000001554 ) ) ;
#180765 = CARTESIAN_POINT ( 'NONE',  ( -6.587282531393266360, 8.778525268082516320, 1.599625672291269396 ) ) ;
#180767 = CARTESIAN_POINT ( 'NONE',  ( 6.825078400183551608, 4.689370880799383912, 2.706890346843467299 ) ) ;
#180766 = CARTESIAN_POINT ( 'NONE',  ( -5.780704523637806069, 7.347994962087573079, -1.310296981949153006 ) ) ;
#180768 = CARTESIAN_POINT ( 'NONE',  ( 5.094532678321557206, 4.917790403868676385, -0.1305349544365452807 ) ) ;
#180769 = ORIENTED_EDGE ( 'NONE', *, *, #134258, .F. ) ;
#180770 = CARTESIAN_POINT ( 'NONE',  ( 4.399328490915206835, 1.653984737846543540, 1.229246434344443806 ) ) ;
#180771 = CARTESIAN_POINT ( 'NONE',  ( 0.6801582343750004478, 2.057291667008069425, -1.178068619123876282 ) ) ;
#180772 = UNCERTAINTY_MEASURE_WITH_UNIT (LENGTH_MEASURE( 1.000000000000000082E-05 ), #67595, 'distance_accuracy_value', 'NONE');
#180773 = CARTESIAN_POINT ( 'NONE',  ( -0.2106854629475400364, 0.7093903261615883693, -2.078205123749873984 ) ) ;
#180774 = CARTESIAN_POINT ( 'NONE',  ( -4.042302355168801320, 7.867769847672247074, 0.7998128361456341429 ) ) ;
#180775 = CARTESIAN_POINT ( 'NONE',  ( 3.211586479193883292, 1.593432852337670624, 1.240894322269629813 ) ) ;
#180776 = CARTESIAN_POINT ( 'NONE',  ( -0.7500000000000006661, -0.6416666666666446250, -1.299038105676652011 ) ) ;
#180777 = CARTESIAN_POINT ( 'NONE',  ( 9.083599731475976213, 12.58098820582193689, 1.082531754730546636 ) ) ;
#180778 = CARTESIAN_POINT ( 'NONE',  ( 6.272618624616828953, 10.46980549536166016, 1.040834085586084257E-14 ) ) ;
#180779 = CARTESIAN_POINT ( 'NONE',  ( 2.905207415116388248, 1.740275362031361794, 1.103647167516639938 ) ) ;
#180780 =( BOUNDED_SURFACE ( )  B_SPLINE_SURFACE ( 1, 2, ( 
 ( #42665, #41596, #142309, #78334, #123979, #77266, #156398, #177988, #140166, #174799, #26375, #92488, #43728, #62097, #160661, #209378, #109843, #29601, #107707, #158527, #175857, #108774, #25310, #194219, #206189, #91412, #157472, #9067, #27446, #159588, #61022, #146574, #81539, #17575, #162806, #180114, #83659, #95687, #16513, #199534, #80475, #181168, #130374, #14383, #30673, #213640, #116233, #195300, #133527, #114122, #183297, #65266, #82596, #212593, #1326, #148682, #131412, #64231, #63158, #15451, #179054, #129323, #66322, #250, #196364, #161741, #13332, #49053, #165990, #149749, #46930, #197412, #48004, #31738, #182224, #132466, #164920, #147621, #198468, #50113, #67387, #51177, #96756, #33847, #115173, #99928, #145523, #97811, #113048, #32793, #163874, #98868, #117300, #79406, #211522, #19726, #68465, #103127, #171315, #150824, #104200, #34903, #138840, #100975, #53306, #119438, #185425, #136704, #105278, #71660, #170247, #152939, #122672, #2387, #37043, #70589, #169185, #202728, #5580, #20777, #120518, #151885, #167064, #3459, #86873, #54380, #18656, #89026, #4516, #155079, #85805, #137774, #203792, #22910, #186496, #118369, #38127, #21832, #6666, #87940, #72742, #55438, #204856, #154014, #200593, #56511, #102060, #121590, #187562, #168125, #39189, #84736, #134593, #52241, #184357, #69529, #35979, #135636, #201657, #123736, #92240, #209131, #73821, #12010, #207010, #61840, #158290, #175606, #41350, #94365, #27195, #9880, #91164, #156154, #108523, #57577, #7735, #159337, #93301, #74894, #188634, #106376, #142059, #44543, #176660, #139915, #75956, #157220, #58641, #60769, #10933, #43483, #174552, #77009, #143136, #28273, #160407, #189697, #126929, #208073, #192886, #23988, #8818, #205946, #125861, #42418, #59699, #191818, #173485, #90090, #25062, #107459, #26128, #110659, #141002, #109601, #40265, #78084, #172400, #124794, #190755, #144208, #210204, #198213, #164670, #197159, #31484, #1067, #29345, #130125, #163617, #63969, #81289, #98609, #196113, #213392, #30418, #128007, #96503, #47750, #15198, #111724, #181965, #179860, #33593, #178803, #16253, #82338, #49848, #146316, #211271, #212330, #113865, #99665, #65016, #115975, #148430, #165734, #97559, #79148, #17321, #195037, #131169, #32534, #162553, #161490, #66062, #17640, #95440, #129064, #132205, #14124, #83402, #193961, #80216, #147366, #149484, #145264, #13069, #48796, #112791, #45608, #114913, #177732, #180911, #62895, #46671, #171049, #71397, #18396, #135379, #117043, #105009, #36779, #69263, #201398, #169981, #102864, #22647, #54116, #3192, #20525, #153747, #86608, #55179, #85536, #185155, #70328, #21568, #151626, #168921, #202461, #154814, #152675, #101794, #38926, #68200, #183039, #136445, #199273, #187299, #4258, #203525, #121324, #5315, #88757, #133265, #120250, #186227, #67132, #35718, #53035, #50916, #37859, #134332, #103938, #34655, #84473, #166804, #137508, #100725, #200337, #150564, #167863, #87675, #2125, #51988, #118113, #184098, #119170, #19461, #74628, #106111, #72472, #40002, #107187, #10668, #124530, #91967, #25857, #8546, #108261, #191551, #139652, #140733, #94099, #138571, #109332, #28002, #7470, #43215, #75691, #159072, #142860, #126652, #175341, #60493, #44271, #208863, #190488, #158025, #173212, #9614, #23727, #6399, #206745, #90894, #73549, #76739, #205673, #58375, #57310, #26922, #204593, #141801, #93031, #192618, #41079, #42146, #174282, #110392, #176397, #56245, #123475, #122404, #188362, #59434, #207805, #189437, #172132, #125591, #89833, #155881, #24791, #156954, #46397, #160138, #77813, #113588, #15985, #148162, #127734, #129853, #128781, #30137, #32269, #213127, #14921, #79940, #64758, #147103, #214164, #65789, #29074, #130900, #63698, #98336, #209929, #194760, #45336, #97286, #13862, #195836, #179591, #144990, #61568, #210995, #193692, #146045, #82070, #111456, #81015, #11738, #49577, #143934, #178526, #96225, #162276, #47476, #131939, #196893, #48531, #31213, #33324, #177460, #212058, #163342, #114651, #180644, #164402, #197950, #115702, #62620, #95158, #112513, #181694, #161209, #12795, #78869, #151364, #153493 ),
 ( #103681, #50645, #167601, #149212, #137256, #69006, #101532, #19200, #202201, #135123, #203275, #86351, #35453, #52777, #185967, #118915, #87426, #117850, #2934, #102608, #53857, #183842, #201139, #20267, #187041, #184896, #134071, #71138, #100458, #787, #168662, #17053, #5063, #36521, #21319, #54922, #37599, #121073, #165458, #152422, #169730, #99405, #66854, #4001, #67926, #85278, #83133, #70070, #136183, #119990, #132998, #198999, #116772, #182769, #34386, #166533, #18123, #84211, #150299, #200080, #1865, #51728, #109878, #159626, #61055, #23467, #88500, #92522, #72209, #175890, #178015, #154562, #110937, #38673, #145554, #104752, #59984, #126137, #192099, #143414, #112014, #78365, #176943, #11220, #129351, #6139, #43765, #77302, #27481, #209408, #12284, #93581, #127214, #158561, #170801, #10159, #193182, #44831, #22390, #95718, #28558, #161771, #76235, #144485, #210492, #29632, #94647, #122141, #160691, #62127, #13363, #128288, #79437, #194250, #211553, #45893, #204331, #63186, #105844, #138316, #55990, #142344, #188109, #39739, #171871, #208353, #196394, #166020, #163905, #167096, #46961, #31770, #181195, #117331, #48037, #65292, #183329, #195330, #116262, #84767, #180144, #66351, #15481, #114151, #130406, #98897, #1354, #80505, #18685, #213668, #68494, #164950, #182253, #97840, #101007, #33877, #16543, #81566, #162838, #115202, #64261, #14416, #17606, #99955, #147652, #113079, #179083, #131439, #197443, #49084, #82624, #51209, #83690, #50140, #148709, #30705, #96788, #32822, #279, #132495, #198495, #149778, #67415, #133556, #199565, #146602, #34935, #150853, #2417, #212620, #188666, #186527, #40296, #185454, #171346, #89056, #56541, #152971, #3486, #4545, #202756, #106407, #71691, #122703, #22940, #204890, #104230, #85835, #24018, #201688, #137804, #39217, #169216, #168155, #72773, #155113, #36005, #135665, #105308, #103155, #172430, #200624, #37076, #120549, #90120, #53333, #70618, #156187, #134621, #55467, #7764, #119466, #5608, #20807, #86904, #69555, #38157, #6697, #19754, #52273, #136732, #118400, #170276, #121623, #54409, #184386, #187592, #21861, #87969, #102086, #154043, #203823, #151913, #138872, #126959, #174583, #73853, #205974, #27225, #144239, #61870, #41380, #43512, #42448, #158320, #160434, #192919, #143167, #208105, #44575, #60801, #128035, #193989, #157251, #110689, #191850, #12040, #123766, #108552, #173516, #10966, #142090, #109633, #93330, #58671, #189727, #124820, #107490, #59733, #210233, #25090, #209162, #139948, #177760, #57606, #91190, #125891, #8844, #111755, #175639, #75986, #159366, #176687, #77040, #29376, #28300, #9911, #94396, #78111, #45638, #95471, #92273, #161519, #74922, #141034, #207041, #190785, #26159, #100752, #131200, #47783, #199302, #14155, #129095, #16283, #145297, #133296, #164697, #149515, #1101, #165767, #67160, #79182, #98638, #32561, #50947, #196142, #97589, #117072, #82370, #80249, #148459, #13103, #178834, #112821, #17351, #211302, #146348, #183070, #113897, #198243, #62927, #28, #66092, #34683, #15228, #213421, #81318, #30449, #195066, #46706, #179891, #83433, #197188, #132235, #49881, #147394, #114941, #116006, #212360, #65044, #96534, #162581, #181992, #64001, #130152, #33625, #99697, #31514, #163648, #48826, #180941, #6434, #204630, #154850, #136475, #37894, #53069, #103972, #184128, #166834, #20556, #36812, #167893, #171084, #85568, #4289, #151658, #137544, #18430, #21602, #38964, #203562, #201429, #70361, #86640, #121360, #122440, #56281, #3228, #68232, #35751, #200369, #202496, #69295, #187335, #54148, #22680, #170014, #55214, #40034, #188398, #88792, #52017, #119202, #72509, #120285, #87708, #186260, #168953, #153780, #105049, #135406, #152707, #84504, #150593, #138607, #2155, #19493, #134365, #5350, #118143, #101825, #185188, #102894, #71432, #143970, #94135, #75723, #191586, #206777, #43247, #123508, #106146, #174317, #190525, #107224, #110427, #24828, #158061, #90928, #76776, #172170, #175374, #192653, #142898, #140765, #9647, #25891, #60531, #61603, #209963, #156994, #7502, #189473, #139688, #141837, #8581, #126691, #207843, #176431 ) ),
 .UNSPECIFIED., .F., .F., .F. ) 
 B_SPLINE_SURFACE_WITH_KNOTS ( ( 2, 2 ),
 ( 3, 2, 2, 2, 2, 2, 2, 2, 2, 2, 2, 2, 2, 2, 2, 2, 2, 2, 2, 2, 2, 2, 2, 2, 2, 2, 2, 2, 2, 2, 2, 2, 2, 2, 2, 2, 2, 2, 2, 2, 2, 2, 2, 2, 2, 2, 2, 2, 2, 2, 2, 2, 2, 2, 2, 2, 2, 2, 2, 2, 2, 2, 2, 2, 2, 2, 2, 2, 2, 2, 2, 2, 2, 2, 2, 2, 2, 2, 2, 2, 2, 2, 2, 2, 2, 2, 2, 2, 2, 2, 2, 2, 2, 2, 2, 2, 2, 2, 2, 2, 2, 2, 2, 2, 2, 2, 2, 2, 2, 2, 2, 2, 2, 2, 2, 2, 2, 2, 2, 2, 2, 2, 2, 2, 2, 2, 2, 2, 2, 2, 2, 2, 2, 2, 2, 2, 2, 2, 2, 2, 2, 2, 2, 2, 2, 2, 2, 2, 2, 2, 2, 2, 2, 2, 2, 2, 2, 2, 2, 2, 2, 2, 2, 2, 2, 2, 2, 2, 2, 2, 2, 2, 2, 2, 2, 2, 2, 2, 2, 2, 2, 2, 2, 2, 2, 2, 2, 2, 2, 2, 2, 2, 2, 2, 2, 2, 2, 2, 2, 2, 2, 2, 2, 2, 2, 2, 2, 2, 2, 2, 2, 2, 2, 2, 2, 2, 2, 2, 2, 2, 2, 2, 2, 2, 2, 2, 2, 2, 2, 2, 2, 2, 2, 2, 2, 2, 2, 2, 2, 2, 3 ),
 ( 0.000000000000000000, 1.000000000000000000 ),
 ( 0.000000000000000000, 0.004166666666666666609, 0.008333333333333333218, 0.01250000000000000069, 0.01666666666666666644, 0.02083333333333333218, 0.02500000000000000139, 0.02916666666666666713, 0.03333333333333333287, 0.03749999999999999861, 0.04166666666666666435, 0.04583333333333333010, 0.05000000000000000278, 0.05416666666666666852, 0.05833333333333333426, 0.06250000000000000000, 0.06666666666666666574, 0.07083333333333333148, 0.07499999999999999722, 0.07916666666666666297, 0.08333333333333332871, 0.08749999999999999445, 0.09166666666666666019, 0.09583333333333333981, 0.1000000000000000056, 0.1041666666666666713, 0.1083333333333333370, 0.1125000000000000028, 0.1166666666666666685, 0.1208333333333333343, 0.1250000000000000000, 0.1291666666666666796, 0.1333333333333333315, 0.1375000000000000111, 0.1416666666666666630, 0.1458333333333333426, 0.1499999999999999944, 0.1541666666666666741, 0.1583333333333333259, 0.1625000000000000056, 0.1666666666666666574, 0.1708333333333333370, 0.1749999999999999889, 0.1791666666666666685, 0.1833333333333333204, 0.1875000000000000000, 0.1916666666666666796, 0.1958333333333333315, 0.2000000000000000111, 0.2041666666666666630, 0.2083333333333333426, 0.2124999999999999944, 0.2166666666666666741, 0.2208333333333333259, 0.2250000000000000056, 0.2291666666666666574, 0.2333333333333333370, 0.2374999999999999889, 0.2416666666666666685, 0.2458333333333333204, 0.2500000000000000000, 0.2541666666666666519, 0.2583333333333333592, 0.2625000000000000111, 0.2666666666666666630, 0.2708333333333333148, 0.2750000000000000222, 0.2791666666666666741, 0.2833333333333333259, 0.2874999999999999778, 0.2916666666666666852, 0.2958333333333333370, 0.2999999999999999889, 0.3041666666666666408, 0.3083333333333333481, 0.3125000000000000000, 0.3166666666666666519, 0.3208333333333333592, 0.3250000000000000111, 0.3291666666666666630, 0.3333333333333333148, 0.3375000000000000222, 0.3416666666666666741, 0.3458333333333333259, 0.3499999999999999778, 0.3541666666666666852, 0.3583333333333333370, 0.3624999999999999889, 0.3666666666666666408, 0.3708333333333333481, 0.3750000000000000000, 0.3791666666666666519, 0.3833333333333333592, 0.3875000000000000111, 0.3916666666666666630, 0.3958333333333333148, 0.4000000000000000222, 0.4041666666666666741, 0.4083333333333333259, 0.4124999999999999778, 0.4166666666666666852, 0.4208333333333333370, 0.4249999999999999889, 0.4291666666666666408, 0.4333333333333333481, 0.4375000000000000000, 0.4416666666666666519, 0.4458333333333333592, 0.4500000000000000111, 0.4541666666666666630, 0.4583333333333333148, 0.4625000000000000222, 0.4666666666666666741, 0.4708333333333333259, 0.4749999999999999778, 0.4791666666666666852, 0.4833333333333333370, 0.4874999999999999889, 0.4916666666666666408, 0.4958333333333333481, 0.5000000000000000000, 0.5041666666666666519, 0.5083333333333333037, 0.5124999999999999556, 0.5166666666666667185, 0.5208333333333333703, 0.5250000000000000222, 0.5291666666666666741, 0.5333333333333333259, 0.5374999999999999778, 0.5416666666666666297, 0.5458333333333332815, 0.5500000000000000444, 0.5541666666666666963, 0.5583333333333333481, 0.5625000000000000000, 0.5666666666666666519, 0.5708333333333333037, 0.5749999999999999556, 0.5791666666666667185, 0.5833333333333333703, 0.5875000000000000222, 0.5916666666666666741, 0.5958333333333333259, 0.5999999999999999778, 0.6041666666666666297, 0.6083333333333332815, 0.6125000000000000444, 0.6166666666666666963, 0.6208333333333333481, 0.6250000000000000000, 0.6291666666666666519, 0.6333333333333333037, 0.6374999999999999556, 0.6416666666666667185, 0.6458333333333333703, 0.6500000000000000222, 0.6541666666666666741, 0.6583333333333333259, 0.6624999999999999778, 0.6666666666666666297, 0.6708333333333332815, 0.6750000000000000444, 0.6791666666666666963, 0.6833333333333333481, 0.6875000000000000000, 0.6916666666666666519, 0.6958333333333333037, 0.6999999999999999556, 0.7041666666666667185, 0.7083333333333333703, 0.7125000000000000222, 0.7166666666666666741, 0.7208333333333333259, 0.7249999999999999778, 0.7291666666666666297, 0.7333333333333332815, 0.7375000000000000444, 0.7416666666666666963, 0.7458333333333333481, 0.7500000000000000000, 0.7541666666666666519, 0.7583333333333333037, 0.7624999999999999556, 0.7666666666666667185, 0.7708333333333333703, 0.7750000000000000222, 0.7791666666666666741, 0.7833333333333333259, 0.7874999999999999778, 0.7916666666666666297, 0.7958333333333332815, 0.8000000000000000444, 0.8041666666666666963, 0.8083333333333333481, 0.8125000000000000000, 0.8166666666666666519, 0.8208333333333333037, 0.8249999999999999556, 0.8291666666666667185, 0.8333333333333333703, 0.8375000000000000222, 0.8416666666666666741, 0.8458333333333333259, 0.8499999999999999778, 0.8541666666666666297, 0.8583333333333332815, 0.8625000000000000444, 0.8666666666666666963, 0.8708333333333333481, 0.8750000000000000000, 0.8791666666666666519, 0.8833333333333333037, 0.8874999999999999556, 0.8916666666666667185, 0.8958333333333333703, 0.9000000000000000222, 0.9041666666666666741, 0.9083333333333333259, 0.9124999999999999778, 0.9166666666666666297, 0.9208333333333332815, 0.9250000000000000444, 0.9291666666666666963, 0.9333333333333333481, 0.9375000000000000000, 0.9416666666666666519, 0.9458333333333333037, 0.9499999999999999556, 0.9541666666666667185, 0.9583333333333333703, 0.9625000000000000222, 0.9666666666666666741, 0.9708333333333333259, 0.9749999999999999778, 0.9791666666666666297, 0.9833333333333332815, 0.9875000000000000444, 0.9916666666666666963, 0.9958333333333333481, 1.000000000000000000 ),
 .UNSPECIFIED. ) 
 GEOMETRIC_REPRESENTATION_ITEM ( )  RATIONAL_B_SPLINE_SURFACE ( (
 ( 1.000000000000000000, 0.8660254037844387076, 1.000000000000000000, 0.8660254037844387076, 1.000000000000000000, 0.8660254037844387076, 1.000000000000000000, 0.8660254037844387076, 1.000000000000000000, 0.8660254037844387076, 1.000000000000000000, 0.8660254037844387076, 1.000000000000000000, 0.8660254037844387076, 1.000000000000000000, 0.8660254037844387076, 1.000000000000000000, 0.8660254037844387076, 1.000000000000000000, 0.8660254037844387076, 1.000000000000000000, 0.8660254037844387076, 1.000000000000000000, 0.8660254037844387076, 1.000000000000000000, 0.8660254037844387076, 1.000000000000000000, 0.8660254037844387076, 1.000000000000000000, 0.8660254037844387076, 1.000000000000000000, 0.8660254037844387076, 1.000000000000000000, 0.8660254037844387076, 1.000000000000000000, 0.8660254037844387076, 1.000000000000000000, 0.8660254037844387076, 1.000000000000000000, 0.8660254037844387076, 1.000000000000000000, 0.8660254037844387076, 1.000000000000000000, 0.8660254037844387076, 1.000000000000000000, 0.8660254037844387076, 1.000000000000000000, 0.8660254037844387076, 1.000000000000000000, 0.8660254037844387076, 1.000000000000000000, 0.8660254037844387076, 1.000000000000000000, 0.8660254037844387076, 1.000000000000000000, 0.8660254037844387076, 1.000000000000000000, 0.8660254037844387076, 1.000000000000000000, 0.8660254037844387076, 1.000000000000000000, 0.8660254037844387076, 1.000000000000000000, 0.8660254037844387076, 1.000000000000000000, 0.8660254037844387076, 1.000000000000000000, 0.8660254037844387076, 1.000000000000000000, 0.8660254037844387076, 1.000000000000000000, 0.8660254037844387076, 1.000000000000000000, 0.8660254037844387076, 1.000000000000000000, 0.8660254037844387076, 1.000000000000000000, 0.8660254037844387076, 1.000000000000000000, 0.8660254037844387076, 1.000000000000000000, 0.8660254037844387076, 1.000000000000000000, 0.8660254037844387076, 1.000000000000000000, 0.8660254037844387076, 1.000000000000000000, 0.8660254037844387076, 1.000000000000000000, 0.8660254037844387076, 1.000000000000000000, 0.8660254037844387076, 1.000000000000000000, 0.8660254037844387076, 1.000000000000000000, 0.8660254037844387076, 1.000000000000000000, 0.8660254037844387076, 1.000000000000000000, 0.8660254037844387076, 1.000000000000000000, 0.8660254037844387076, 1.000000000000000000, 0.8660254037844387076, 1.000000000000000000, 0.8660254037844387076, 1.000000000000000000, 0.8660254037844387076, 1.000000000000000000, 0.8660254037844387076, 1.000000000000000000, 0.8660254037844387076, 1.000000000000000000, 0.8660254037844387076, 1.000000000000000000, 0.8660254037844387076, 1.000000000000000000, 0.8660254037844387076, 1.000000000000000000, 0.8660254037844387076, 1.000000000000000000, 0.8660254037844387076, 1.000000000000000000, 0.8660254037844387076, 1.000000000000000000, 0.8660254037844387076, 1.000000000000000000, 0.8660254037844387076, 1.000000000000000000, 0.8660254037844387076, 1.000000000000000000, 0.8660254037844387076, 1.000000000000000000, 0.8660254037844387076, 1.000000000000000000, 0.8660254037844387076, 1.000000000000000000, 0.8660254037844387076, 1.000000000000000000, 0.8660254037844387076, 1.000000000000000000, 0.8660254037844387076, 1.000000000000000000, 0.8660254037844387076, 1.000000000000000000, 0.8660254037844387076, 1.000000000000000000, 0.8660254037844387076, 1.000000000000000000, 0.8660254037844387076, 1.000000000000000000, 0.8660254037844387076, 1.000000000000000000, 0.8660254037844387076, 1.000000000000000000, 0.8660254037844387076, 1.000000000000000000, 0.8660254037844387076, 1.000000000000000000, 0.8660254037844387076, 1.000000000000000000, 0.8660254037844387076, 1.000000000000000000, 0.8660254037844387076, 1.000000000000000000, 0.8660254037844387076, 1.000000000000000000, 0.8660254037844387076, 1.000000000000000000, 0.8660254037844387076, 1.000000000000000000, 0.8660254037844387076, 1.000000000000000000, 0.8660254037844387076, 1.000000000000000000, 0.8660254037844387076, 1.000000000000000000, 0.8660254037844387076, 1.000000000000000000, 0.8660254037844387076, 1.000000000000000000, 0.8660254037844387076, 1.000000000000000000, 0.8660254037844387076, 1.000000000000000000, 0.8660254037844387076, 1.000000000000000000, 0.8660254037844387076, 1.000000000000000000, 0.8660254037844387076, 1.000000000000000000, 0.8660254037844387076, 1.000000000000000000, 0.8660254037844387076, 1.000000000000000000, 0.8660254037844387076, 1.000000000000000000, 0.8660254037844387076, 1.000000000000000000, 0.8660254037844387076, 1.000000000000000000, 0.8660254037844387076, 1.000000000000000000, 0.8660254037844387076, 1.000000000000000000, 0.8660254037844387076, 1.000000000000000000, 0.8660254037844387076, 1.000000000000000000, 0.8660254037844387076, 1.000000000000000000, 0.8660254037844387076, 1.000000000000000000, 0.8660254037844387076, 1.000000000000000000, 0.8660254037844387076, 1.000000000000000000, 0.8660254037844387076, 1.000000000000000000, 0.8660254037844387076, 1.000000000000000000, 0.8660254037844387076, 1.000000000000000000, 0.8660254037844387076, 1.000000000000000000, 0.8660254037844387076, 1.000000000000000000, 0.8660254037844387076, 1.000000000000000000, 0.8660254037844387076, 1.000000000000000000, 0.8660254037844387076, 1.000000000000000000, 0.8660254037844387076, 1.000000000000000000, 0.8660254037844387076, 1.000000000000000000, 0.8660254037844387076, 1.000000000000000000, 0.8660254037844387076, 1.000000000000000000, 0.8660254037844387076, 1.000000000000000000, 0.8660254037844387076, 1.000000000000000000, 0.8660254037844387076, 1.000000000000000000, 0.8660254037844387076, 1.000000000000000000, 0.8660254037844387076, 1.000000000000000000, 0.8660254037844387076, 1.000000000000000000, 0.8660254037844387076, 1.000000000000000000, 0.8660254037844387076, 1.000000000000000000, 0.8660254037844387076, 1.000000000000000000, 0.8660254037844387076, 1.000000000000000000, 0.8660254037844387076, 1.000000000000000000, 0.8660254037844387076, 1.000000000000000000, 0.8660254037844387076, 1.000000000000000000, 0.8660254037844387076, 1.000000000000000000, 0.8660254037844387076, 1.000000000000000000, 0.8660254037844387076, 1.000000000000000000, 0.8660254037844387076, 1.000000000000000000, 0.8660254037844387076, 1.000000000000000000, 0.8660254037844387076, 1.000000000000000000, 0.8660254037844387076, 1.000000000000000000, 0.8660254037844387076, 1.000000000000000000, 0.8660254037844387076, 1.000000000000000000, 0.8660254037844387076, 1.000000000000000000, 0.8660254037844387076, 1.000000000000000000, 0.8660254037844387076, 1.000000000000000000, 0.8660254037844387076, 1.000000000000000000, 0.8660254037844387076, 1.000000000000000000, 0.8660254037844387076, 1.000000000000000000, 0.8660254037844387076, 1.000000000000000000, 0.8660254037844387076, 1.000000000000000000, 0.8660254037844387076, 1.000000000000000000, 0.8660254037844387076, 1.000000000000000000, 0.8660254037844387076, 1.000000000000000000, 0.8660254037844387076, 1.000000000000000000, 0.8660254037844387076, 1.000000000000000000, 0.8660254037844387076, 1.000000000000000000, 0.8660254037844387076, 1.000000000000000000, 0.8660254037844387076, 1.000000000000000000, 0.8660254037844387076, 1.000000000000000000, 0.8660254037844387076, 1.000000000000000000, 0.8660254037844387076, 1.000000000000000000, 0.8660254037844387076, 1.000000000000000000, 0.8660254037844387076, 1.000000000000000000, 0.8660254037844387076, 1.000000000000000000, 0.8660254037844387076, 1.000000000000000000, 0.8660254037844387076, 1.000000000000000000, 0.8660254037844387076, 1.000000000000000000, 0.8660254037844387076, 1.000000000000000000, 0.8660254037844387076, 1.000000000000000000, 0.8660254037844387076, 1.000000000000000000, 0.8660254037844387076, 1.000000000000000000, 0.8660254037844387076, 1.000000000000000000, 0.8660254037844387076, 1.000000000000000000, 0.8660254037844387076, 1.000000000000000000, 0.8660254037844387076, 1.000000000000000000, 0.8660254037844387076, 1.000000000000000000, 0.8660254037844387076, 1.000000000000000000, 0.8660254037844387076, 1.000000000000000000, 0.8660254037844387076, 1.000000000000000000, 0.8660254037844387076, 1.000000000000000000, 0.8660254037844387076, 1.000000000000000000, 0.8660254037844387076, 1.000000000000000000, 0.8660254037844387076, 1.000000000000000000, 0.8660254037844387076, 1.000000000000000000, 0.8660254037844387076, 1.000000000000000000, 0.8660254037844387076, 1.000000000000000000, 0.8660254037844387076, 1.000000000000000000, 0.8660254037844387076, 1.000000000000000000, 0.8660254037844387076, 1.000000000000000000, 0.8660254037844387076, 1.000000000000000000, 0.8660254037844387076, 1.000000000000000000, 0.8660254037844387076, 1.000000000000000000, 0.8660254037844387076, 1.000000000000000000, 0.8660254037844387076, 1.000000000000000000, 0.8660254037844387076, 1.000000000000000000, 0.8660254037844387076, 1.000000000000000000, 0.8660254037844387076, 1.000000000000000000, 0.8660254037844387076, 1.000000000000000000, 0.8660254037844387076, 1.000000000000000000, 0.8660254037844387076, 1.000000000000000000, 0.8660254037844387076, 1.000000000000000000, 0.8660254037844387076, 1.000000000000000000, 0.8660254037844387076, 1.000000000000000000, 0.8660254037844387076, 1.000000000000000000, 0.8660254037844387076, 1.000000000000000000, 0.8660254037844387076, 1.000000000000000000, 0.8660254037844387076, 1.000000000000000000, 0.8660254037844387076, 1.000000000000000000, 0.8660254037844387076, 1.000000000000000000, 0.8660254037844387076, 1.000000000000000000, 0.8660254037844387076, 1.000000000000000000, 0.8660254037844387076, 1.000000000000000000, 0.8660254037844387076, 1.000000000000000000, 0.8660254037844387076, 1.000000000000000000, 0.8660254037844387076, 1.000000000000000000, 0.8660254037844387076, 1.000000000000000000, 0.8660254037844387076, 1.000000000000000000, 0.8660254037844387076, 1.000000000000000000, 0.8660254037844387076, 1.000000000000000000, 0.8660254037844387076, 1.000000000000000000, 0.8660254037844387076, 1.000000000000000000, 0.8660254037844387076, 1.000000000000000000, 0.8660254037844387076, 1.000000000000000000, 0.8660254037844387076, 1.000000000000000000, 0.8660254037844387076, 1.000000000000000000, 0.8660254037844387076, 1.000000000000000000, 0.8660254037844387076, 1.000000000000000000, 0.8660254037844387076, 1.000000000000000000, 0.8660254037844387076, 1.000000000000000000, 0.8660254037844387076, 1.000000000000000000, 0.8660254037844387076, 1.000000000000000000, 0.8660254037844387076, 1.000000000000000000, 0.8660254037844387076, 1.000000000000000000, 0.8660254037844387076, 1.000000000000000000, 0.8660254037844387076, 1.000000000000000000, 0.8660254037844387076, 1.000000000000000000, 0.8660254037844387076, 1.000000000000000000, 0.8660254037844387076, 1.000000000000000000, 0.8660254037844387076, 1.000000000000000000, 0.8660254037844387076, 1.000000000000000000),
 ( 1.000000000000000000, 0.8660254037844387076, 1.000000000000000000, 0.8660254037844387076, 1.000000000000000000, 0.8660254037844387076, 1.000000000000000000, 0.8660254037844387076, 1.000000000000000000, 0.8660254037844387076, 1.000000000000000000, 0.8660254037844387076, 1.000000000000000000, 0.8660254037844387076, 1.000000000000000000, 0.8660254037844387076, 1.000000000000000000, 0.8660254037844387076, 1.000000000000000000, 0.8660254037844387076, 1.000000000000000000, 0.8660254037844387076, 1.000000000000000000, 0.8660254037844387076, 1.000000000000000000, 0.8660254037844387076, 1.000000000000000000, 0.8660254037844387076, 1.000000000000000000, 0.8660254037844387076, 1.000000000000000000, 0.8660254037844387076, 1.000000000000000000, 0.8660254037844387076, 1.000000000000000000, 0.8660254037844387076, 1.000000000000000000, 0.8660254037844387076, 1.000000000000000000, 0.8660254037844387076, 1.000000000000000000, 0.8660254037844387076, 1.000000000000000000, 0.8660254037844387076, 1.000000000000000000, 0.8660254037844387076, 1.000000000000000000, 0.8660254037844387076, 1.000000000000000000, 0.8660254037844387076, 1.000000000000000000, 0.8660254037844387076, 1.000000000000000000, 0.8660254037844387076, 1.000000000000000000, 0.8660254037844387076, 1.000000000000000000, 0.8660254037844387076, 1.000000000000000000, 0.8660254037844387076, 1.000000000000000000, 0.8660254037844387076, 1.000000000000000000, 0.8660254037844387076, 1.000000000000000000, 0.8660254037844387076, 1.000000000000000000, 0.8660254037844387076, 1.000000000000000000, 0.8660254037844387076, 1.000000000000000000, 0.8660254037844387076, 1.000000000000000000, 0.8660254037844387076, 1.000000000000000000, 0.8660254037844387076, 1.000000000000000000, 0.8660254037844387076, 1.000000000000000000, 0.8660254037844387076, 1.000000000000000000, 0.8660254037844387076, 1.000000000000000000, 0.8660254037844387076, 1.000000000000000000, 0.8660254037844387076, 1.000000000000000000, 0.8660254037844387076, 1.000000000000000000, 0.8660254037844387076, 1.000000000000000000, 0.8660254037844387076, 1.000000000000000000, 0.8660254037844387076, 1.000000000000000000, 0.8660254037844387076, 1.000000000000000000, 0.8660254037844387076, 1.000000000000000000, 0.8660254037844387076, 1.000000000000000000, 0.8660254037844387076, 1.000000000000000000, 0.8660254037844387076, 1.000000000000000000, 0.8660254037844387076, 1.000000000000000000, 0.8660254037844387076, 1.000000000000000000, 0.8660254037844387076, 1.000000000000000000, 0.8660254037844387076, 1.000000000000000000, 0.8660254037844387076, 1.000000000000000000, 0.8660254037844387076, 1.000000000000000000, 0.8660254037844387076, 1.000000000000000000, 0.8660254037844387076, 1.000000000000000000, 0.8660254037844387076, 1.000000000000000000, 0.8660254037844387076, 1.000000000000000000, 0.8660254037844387076, 1.000000000000000000, 0.8660254037844387076, 1.000000000000000000, 0.8660254037844387076, 1.000000000000000000, 0.8660254037844387076, 1.000000000000000000, 0.8660254037844387076, 1.000000000000000000, 0.8660254037844387076, 1.000000000000000000, 0.8660254037844387076, 1.000000000000000000, 0.8660254037844387076, 1.000000000000000000, 0.8660254037844387076, 1.000000000000000000, 0.8660254037844387076, 1.000000000000000000, 0.8660254037844387076, 1.000000000000000000, 0.8660254037844387076, 1.000000000000000000, 0.8660254037844387076, 1.000000000000000000, 0.8660254037844387076, 1.000000000000000000, 0.8660254037844387076, 1.000000000000000000, 0.8660254037844387076, 1.000000000000000000, 0.8660254037844387076, 1.000000000000000000, 0.8660254037844387076, 1.000000000000000000, 0.8660254037844387076, 1.000000000000000000, 0.8660254037844387076, 1.000000000000000000, 0.8660254037844387076, 1.000000000000000000, 0.8660254037844387076, 1.000000000000000000, 0.8660254037844387076, 1.000000000000000000, 0.8660254037844387076, 1.000000000000000000, 0.8660254037844387076, 1.000000000000000000, 0.8660254037844387076, 1.000000000000000000, 0.8660254037844387076, 1.000000000000000000, 0.8660254037844387076, 1.000000000000000000, 0.8660254037844387076, 1.000000000000000000, 0.8660254037844387076, 1.000000000000000000, 0.8660254037844387076, 1.000000000000000000, 0.8660254037844387076, 1.000000000000000000, 0.8660254037844387076, 1.000000000000000000, 0.8660254037844387076, 1.000000000000000000, 0.8660254037844387076, 1.000000000000000000, 0.8660254037844387076, 1.000000000000000000, 0.8660254037844387076, 1.000000000000000000, 0.8660254037844387076, 1.000000000000000000, 0.8660254037844387076, 1.000000000000000000, 0.8660254037844387076, 1.000000000000000000, 0.8660254037844387076, 1.000000000000000000, 0.8660254037844387076, 1.000000000000000000, 0.8660254037844387076, 1.000000000000000000, 0.8660254037844387076, 1.000000000000000000, 0.8660254037844387076, 1.000000000000000000, 0.8660254037844387076, 1.000000000000000000, 0.8660254037844387076, 1.000000000000000000, 0.8660254037844387076, 1.000000000000000000, 0.8660254037844387076, 1.000000000000000000, 0.8660254037844387076, 1.000000000000000000, 0.8660254037844387076, 1.000000000000000000, 0.8660254037844387076, 1.000000000000000000, 0.8660254037844387076, 1.000000000000000000, 0.8660254037844387076, 1.000000000000000000, 0.8660254037844387076, 1.000000000000000000, 0.8660254037844387076, 1.000000000000000000, 0.8660254037844387076, 1.000000000000000000, 0.8660254037844387076, 1.000000000000000000, 0.8660254037844387076, 1.000000000000000000, 0.8660254037844387076, 1.000000000000000000, 0.8660254037844387076, 1.000000000000000000, 0.8660254037844387076, 1.000000000000000000, 0.8660254037844387076, 1.000000000000000000, 0.8660254037844387076, 1.000000000000000000, 0.8660254037844387076, 1.000000000000000000, 0.8660254037844387076, 1.000000000000000000, 0.8660254037844387076, 1.000000000000000000, 0.8660254037844387076, 1.000000000000000000, 0.8660254037844387076, 1.000000000000000000, 0.8660254037844387076, 1.000000000000000000, 0.8660254037844387076, 1.000000000000000000, 0.8660254037844387076, 1.000000000000000000, 0.8660254037844387076, 1.000000000000000000, 0.8660254037844387076, 1.000000000000000000, 0.8660254037844387076, 1.000000000000000000, 0.8660254037844387076, 1.000000000000000000, 0.8660254037844387076, 1.000000000000000000, 0.8660254037844387076, 1.000000000000000000, 0.8660254037844387076, 1.000000000000000000, 0.8660254037844387076, 1.000000000000000000, 0.8660254037844387076, 1.000000000000000000, 0.8660254037844387076, 1.000000000000000000, 0.8660254037844387076, 1.000000000000000000, 0.8660254037844387076, 1.000000000000000000, 0.8660254037844387076, 1.000000000000000000, 0.8660254037844387076, 1.000000000000000000, 0.8660254037844387076, 1.000000000000000000, 0.8660254037844387076, 1.000000000000000000, 0.8660254037844387076, 1.000000000000000000, 0.8660254037844387076, 1.000000000000000000, 0.8660254037844387076, 1.000000000000000000, 0.8660254037844387076, 1.000000000000000000, 0.8660254037844387076, 1.000000000000000000, 0.8660254037844387076, 1.000000000000000000, 0.8660254037844387076, 1.000000000000000000, 0.8660254037844387076, 1.000000000000000000, 0.8660254037844387076, 1.000000000000000000, 0.8660254037844387076, 1.000000000000000000, 0.8660254037844387076, 1.000000000000000000, 0.8660254037844387076, 1.000000000000000000, 0.8660254037844387076, 1.000000000000000000, 0.8660254037844387076, 1.000000000000000000, 0.8660254037844387076, 1.000000000000000000, 0.8660254037844387076, 1.000000000000000000, 0.8660254037844387076, 1.000000000000000000, 0.8660254037844387076, 1.000000000000000000, 0.8660254037844387076, 1.000000000000000000, 0.8660254037844387076, 1.000000000000000000, 0.8660254037844387076, 1.000000000000000000, 0.8660254037844387076, 1.000000000000000000, 0.8660254037844387076, 1.000000000000000000, 0.8660254037844387076, 1.000000000000000000, 0.8660254037844387076, 1.000000000000000000, 0.8660254037844387076, 1.000000000000000000, 0.8660254037844387076, 1.000000000000000000, 0.8660254037844387076, 1.000000000000000000, 0.8660254037844387076, 1.000000000000000000, 0.8660254037844387076, 1.000000000000000000, 0.8660254037844387076, 1.000000000000000000, 0.8660254037844387076, 1.000000000000000000, 0.8660254037844387076, 1.000000000000000000, 0.8660254037844387076, 1.000000000000000000, 0.8660254037844387076, 1.000000000000000000, 0.8660254037844387076, 1.000000000000000000, 0.8660254037844387076, 1.000000000000000000, 0.8660254037844387076, 1.000000000000000000, 0.8660254037844387076, 1.000000000000000000, 0.8660254037844387076, 1.000000000000000000, 0.8660254037844387076, 1.000000000000000000, 0.8660254037844387076, 1.000000000000000000, 0.8660254037844387076, 1.000000000000000000, 0.8660254037844387076, 1.000000000000000000, 0.8660254037844387076, 1.000000000000000000, 0.8660254037844387076, 1.000000000000000000, 0.8660254037844387076, 1.000000000000000000, 0.8660254037844387076, 1.000000000000000000, 0.8660254037844387076, 1.000000000000000000, 0.8660254037844387076, 1.000000000000000000, 0.8660254037844387076, 1.000000000000000000, 0.8660254037844387076, 1.000000000000000000, 0.8660254037844387076, 1.000000000000000000, 0.8660254037844387076, 1.000000000000000000, 0.8660254037844387076, 1.000000000000000000, 0.8660254037844387076, 1.000000000000000000, 0.8660254037844387076, 1.000000000000000000, 0.8660254037844387076, 1.000000000000000000, 0.8660254037844387076, 1.000000000000000000, 0.8660254037844387076, 1.000000000000000000, 0.8660254037844387076, 1.000000000000000000, 0.8660254037844387076, 1.000000000000000000, 0.8660254037844387076, 1.000000000000000000, 0.8660254037844387076, 1.000000000000000000, 0.8660254037844387076, 1.000000000000000000, 0.8660254037844387076, 1.000000000000000000, 0.8660254037844387076, 1.000000000000000000, 0.8660254037844387076, 1.000000000000000000, 0.8660254037844387076, 1.000000000000000000, 0.8660254037844387076, 1.000000000000000000, 0.8660254037844387076, 1.000000000000000000, 0.8660254037844387076, 1.000000000000000000, 0.8660254037844387076, 1.000000000000000000, 0.8660254037844387076, 1.000000000000000000, 0.8660254037844387076, 1.000000000000000000, 0.8660254037844387076, 1.000000000000000000, 0.8660254037844387076, 1.000000000000000000, 0.8660254037844387076, 1.000000000000000000, 0.8660254037844387076, 1.000000000000000000, 0.8660254037844387076, 1.000000000000000000, 0.8660254037844387076, 1.000000000000000000, 0.8660254037844387076, 1.000000000000000000, 0.8660254037844387076, 1.000000000000000000, 0.8660254037844387076, 1.000000000000000000, 0.8660254037844387076, 1.000000000000000000, 0.8660254037844387076, 1.000000000000000000, 0.8660254037844387076, 1.000000000000000000, 0.8660254037844387076, 1.000000000000000000, 0.8660254037844387076, 1.000000000000000000, 0.8660254037844387076, 1.000000000000000000) ) ) 
 REPRESENTATION_ITEM ( '' )  SURFACE ( )  );
#180781 = CARTESIAN_POINT ( 'NONE',  ( -4.731432421044883263, 5.582721248382882528, -1.082531754730543971 ) ) ;
#180782 = CARTESIAN_POINT ( 'NONE',  ( 6.356075086708249167, 6.309842444114747373, -0.7998128361456281477 ) ) ;
#180784 = EDGE_LOOP ( 'NONE', ( #119896, #98278, #33559, #73945 ) ) ;
#180783 = CARTESIAN_POINT ( 'NONE',  ( -0.1411974294642046046, 7.629137130509075604, -2.500278959528269063 ) ) ;
#180785 = CARTESIAN_POINT ( 'NONE',  ( 0.8844010234979463592, 1.624802019249080853, -0.8659260420235401767 ) ) ;
#180786 = VECTOR ( 'NONE', #81739, 1000.000000000000000 ) ;
#180787 = CARTESIAN_POINT ( 'NONE',  ( 6.586557750117827403, -2.163372447211810989, -0.4352210726449382006 ) ) ;
#180788 = CARTESIAN_POINT ( 'NONE',  ( 6.170896192875352959, 7.228408975556602556, 1.199719254218453823 ) ) ;
#180789 = CARTESIAN_POINT ( 'NONE',  ( 0.9663661119345479111, 1.064502738163356721, 1.881203019380036867 ) ) ;
#180790 = CARTESIAN_POINT ( 'NONE',  ( -3.741687207691642314, 6.348756928073427730, 1.082531754730560403 ) ) ;
#180791 = CARTESIAN_POINT ( 'NONE',  ( 2.395720570290179374, -1.993893129684479293, 0.3006499569925198956 ) ) ;
#180792 = CARTESIAN_POINT ( 'NONE',  ( 1.827921470121370850, -1.625240468190300103, 1.625389258475460563 ) ) ;
#180793 = CARTESIAN_POINT ( 'NONE',  ( -11.89197415570408900, 11.29999999999999893, -0.8055989572471861093 ) ) ;
#180794 = CARTESIAN_POINT ( 'NONE',  ( 0.1275333129481092398, -1.147091320445620566, -1.478225367208672703 ) ) ;
#180795 = CARTESIAN_POINT ( 'NONE',  ( 4.592626242060598329, -0.4308863251132522554, -1.923655822462609466 ) ) ;
#180796 = CARTESIAN_POINT ( 'NONE',  ( 5.032435514249763209, 0.5899841883351600869, 1.928258608204669766 ) ) ;
#180798 = DIRECTION ( 'NONE',  ( -0.000000000000000000, -1.000000000000000000, -0.000000000000000000 ) ) ;
#180797 = CARTESIAN_POINT ( 'NONE',  ( -1.364683531250000748, 1.759375000341421913, 0.000000000000000000 ) ) ;
#180800 = CARTESIAN_POINT ( 'NONE',  ( 6.059223728125719965, -1.805531155315470926, -1.083989359861557533 ) ) ;
#180799 = CARTESIAN_POINT ( 'NONE',  ( -5.065942953000576843, 9.062017211809330064, -0.7998128361456231517 ) ) ;
#180801 = CARTESIAN_POINT ( 'NONE',  ( 6.689897370947560873, -1.349224794794257720, -1.570457413003906177 ) ) ;
#180802 = CARTESIAN_POINT ( 'NONE',  ( 5.686755365928134687, 8.721966129303114101, 1.199719254218462483 ) ) ;
#180803 = CARTESIAN_POINT ( 'NONE',  ( -7.549192604710863286, 7.701812881784464437, -0.7998128361456291469 ) ) ;
#180804 = CARTESIAN_POINT ( 'NONE',  ( 6.539320575229292665, 4.694805244051019066, 2.565894911293948422 ) ) ;
#180805 = CARTESIAN_POINT ( 'NONE',  ( 5.361584196017279424, -1.594725845915157647, -1.239436484511841519 ) ) ;
#180806 = CARTESIAN_POINT ( 'NONE',  ( -1.500000000000015099, 0.9104166673494835660, -0.8660254037844313801 ) ) ;
#180807 = CARTESIAN_POINT ( 'NONE',  ( 3.387651152892924955, 2.086375235072422285, -0.9864360317304238235 ) ) ;
#180808 = CARTESIAN_POINT ( 'NONE',  ( 1.903259321421392425, -1.744647275545135212, 1.099889041785537813 ) ) ;
#180809 = CARTESIAN_POINT ( 'NONE',  ( 7.619319141200063150, 9.912291636198670375, 1.443375672974076540 ) ) ;
#180810 = CARTESIAN_POINT ( 'NONE',  ( 5.494797395288433250, 9.632623737803665875, 0.000000000000000000 ) ) ;
#180811 = CARTESIAN_POINT ( 'NONE',  ( 4.549643065837591038, 7.465611455855944101, -1.199719254218452047 ) ) ;
#180812 = CARTESIAN_POINT ( 'NONE',  ( -1.402160292154681736E-14, 1.259375000341419248, -1.575800808251659024 ) ) ;
#180813 = CARTESIAN_POINT ( 'NONE',  ( 7.104109303436412226, 7.390475063538369582, 1.040834085586084257E-14 ) ) ;
#180815 =( LENGTH_UNIT ( ) NAMED_UNIT ( * ) SI_UNIT ( .MILLI., .METRE. ) );
#180814 = CARTESIAN_POINT ( 'NONE',  ( 3.859984642892180684, -0.6334943099049659132, 2.076686793900458294 ) ) ;
#180817 = CARTESIAN_POINT ( 'NONE',  ( 2.384105128782065819, -0.3166398734758494315, -1.813660976904336808 ) ) ;
#180816 = CARTESIAN_POINT ( 'NONE',  ( -5.761852096127856981, 5.824508321678349532, 0.000000000000000000 ) ) ;
#180818 = CARTESIAN_POINT ( 'NONE',  ( -1.364683531250010295, 4.030208333674751842, 0.7879004041258379498 ) ) ;
#180819 = CARTESIAN_POINT ( 'NONE',  ( 4.089532599075940134, -0.8378280566024614018, 2.025282237563410526 ) ) ;
#180820 = CARTESIAN_POINT ( 'NONE',  ( 8.564503538342812305, 13.79480036990495861, 8.405811576776271110 ) ) ;
#180821 = CARTESIAN_POINT ( 'NONE',  ( 5.489262863951156923, 1.998152018339900415, -1.061309651537506227 ) ) ;
#180822 = CARTESIAN_POINT ( 'NONE',  ( 5.045036709957831711, 4.903268083610561767, 0.3063280728123271568 ) ) ;
#180823 = CARTESIAN_POINT ( 'NONE',  ( 4.653539691347775786, 8.417882268172059312, -0.4891605808478947104 ) ) ;
#180824 = AXIS2_PLACEMENT_3D ( 'NONE', #103679, #53854, #102605 ) ;
#180825 = CARTESIAN_POINT ( 'NONE',  ( -4.923019175093582334, 8.757623114335565617, 0.7216878364870267237 ) ) ;
#180826 = CARTESIAN_POINT ( 'NONE',  ( 3.268924434670684498, 6.827845917175511481, -1.734723475976807094E-15 ) ) ;
#180827 = CARTESIAN_POINT ( 'NONE',  ( 6.854783864179318620, -1.365764260946045860, 1.125274747944494891 ) ) ;
#180828 =( BOUNDED_CURVE ( )  B_SPLINE_CURVE ( 3, ( #110758, #160507, #176756, #211373 ),
 .UNSPECIFIED., .F., .T. ) 
 B_SPLINE_CURVE_WITH_KNOTS ( ( 4, 4 ),
 ( 0.7261627075363390471, 1.570796326794784870 ),
 .UNSPECIFIED. ) 
 CURVE ( )  GEOMETRIC_REPRESENTATION_ITEM ( )  RATIONAL_B_SPLINE_CURVE ( ( 1.000000000000000000, 0.9414278581754953468, 0.9414278581754953468, 1.000000000000000000 ) ) 
 REPRESENTATION_ITEM ( '' )  );
#180829 = CARTESIAN_POINT ( 'NONE',  ( 4.213543065054736303, 1.618255708775760970, 1.197237177376732964 ) ) ;
#180830 = CARTESIAN_POINT ( 'NONE',  ( 5.947222937888848371, 10.09017719417900416, 1.040834085586084257E-14 ) ) ;
#180831 = CARTESIAN_POINT ( 'NONE',  ( 3.364387735031381332, 0.9452183826245286191, 1.881983119561444040 ) ) ;
#180832 = CARTESIAN_POINT ( 'NONE',  ( 2.108866759644252298, 0.002224897612410503371, 1.915793139840407333 ) ) ;
#180833 = CARTESIAN_POINT ( 'NONE',  ( 4.844340958784499662, 4.546152628203684820, 0.7998128361456341429 ) ) ;
#180834 = CARTESIAN_POINT ( 'NONE',  ( 3.701571259021796845, -1.489687541828330852, -1.288469680017936048 ) ) ;
#180835 = CARTESIAN_POINT ( 'NONE',  ( 0.6900581440293825919, -1.856003987442723657, -0.2331820809091043056 ) ) ;
#180836 = CARTESIAN_POINT ( 'NONE',  ( 0.8187140321147531319, -1.423520202335259999, 1.350257566363553208 ) ) ;
#180838 = ORIENTED_EDGE ( 'NONE', *, *, #132234, .T. ) ;
#180837 = CARTESIAN_POINT ( 'NONE',  ( 0.5274218815167727170, -0.2782315536139517431, 1.891897276498944347 ) ) ;
#180839 = CARTESIAN_POINT ( 'NONE',  ( 3.863710590214593399, 7.451486755318259547, 1.040834085586084257E-14 ) ) ;
#180840 = CARTESIAN_POINT ( 'NONE',  ( -1.201851678989727383E-14, 1.134375000341418582, 1.575800808251672791 ) ) ;
#180841 = EDGE_CURVE ( 'NONE', #37868, #208182, #1620, .T. ) ;
#180842 = CARTESIAN_POINT ( 'NONE',  ( 6.491075539335432687, 1.626419376453295706, -0.9240138038444990487 ) ) ;
#180843 = DIRECTION ( 'NONE',  ( 0.000000000000000000, 0.000000000000000000, 1.000000000000000000 ) ) ;
#180844 = VERTEX_POINT ( 'NONE', #202484 ) ;
#180845 = CARTESIAN_POINT ( 'NONE',  ( 6.508651864089095795, 0.6437109847576475419, 1.967739590238902991 ) ) ;
#180846 = TOROIDAL_SURFACE ( 'NONE', #211921, 2.349999999999999645, 0.1000000000000000056 ) ;
#180847 =( LENGTH_UNIT ( ) NAMED_UNIT ( * ) SI_UNIT ( .MILLI., .METRE. ) );
#180848 = CARTESIAN_POINT ( 'NONE',  ( 0.5903903138861701372, 1.065687334306382184, -1.774900233272216798 ) ) ;
#180849 = CARTESIAN_POINT ( 'NONE',  ( -1.201851678989727383E-14, 1.212500000000025002, 1.732050807568877637 ) ) ;
#180850 = CARTESIAN_POINT ( 'NONE',  ( 7.284808609244363353, 7.393364887073558656, 0.7998128361456341429 ) ) ;
#180851 = CARTESIAN_POINT ( 'NONE',  ( -9.203287345578106127, 9.631590079462940324, 0.7998128361456462443 ) ) ;
#180852 = CARTESIAN_POINT ( 'NONE',  ( 5.987861119090863049, 7.014868056141362551, 1.199719254218452047 ) ) ;
#180853 = CARTESIAN_POINT ( 'NONE',  ( 5.180389117862056914, 1.045492054797515946, 1.844774357600783121 ) ) ;
#180854 = CARTESIAN_POINT ( 'NONE',  ( 3.953084306836263995, 6.769626237021087789, 1.199719254218452047 ) ) ;
#180855 = CARTESIAN_POINT ( 'NONE',  ( -1.364683531250012516, 1.530208333674756505, 0.7879004041258379498 ) ) ;
#180856 = VERTEX_POINT ( 'NONE', #58398 ) ;
#180857 = CARTESIAN_POINT ( 'NONE',  ( -1.499999999999997780, 1.900000000000019673, 0.000000000000000000 ) ) ;
#180859 = CARTESIAN_POINT ( 'NONE',  ( 2.998324526916512411, 6.649795714711241423, 0.000000000000000000 ) ) ;
#180858 = CARTESIAN_POINT ( 'NONE',  ( 6.355910407107248083, -0.6622273607519140182, 1.846833223631501264 ) ) ;
#180860 = CARTESIAN_POINT ( 'NONE',  ( 4.552111140598270822, 1.802141083034415781, -0.9039717811075360654 ) ) ;
#180861 = CARTESIAN_POINT ( 'NONE',  ( 3.274530738273524033, -0.3788105498489474088, -1.877706502262687760 ) ) ;
#180862 = CARTESIAN_POINT ( 'NONE',  ( -1.907692715643339199, 3.236394383240548400, -0.4609675857477846805 ) ) ;
#180863 = AXIS2_PLACEMENT_3D ( 'NONE', #34275, #84096, #1752 ) ;
#180864 = CARTESIAN_POINT ( 'NONE',  ( 1.277182604683280598, 2.023070758711601691, -0.8431670391453591762 ) ) ;
#180865 = CARTESIAN_POINT ( 'NONE',  ( 0.2331713839410394229, 1.378908429916062994, -2.211717543205340863 ) ) ;
#180866 = CARTESIAN_POINT ( 'NONE',  ( 3.690566713891149320, -0.3619836066245524786, -1.835009008997898761 ) ) ;
#180867 = CARTESIAN_POINT ( 'NONE',  ( 0.7499999999999867883, -0.1520833326505155458, -1.299038105676652899 ) ) ;
#180868 = CARTESIAN_POINT ( 'NONE',  ( -6.320072162264675164, 10.52516795595079557, 0.7998128361456481317 ) ) ;
#180870 = CARTESIAN_POINT ( 'NONE',  ( 5.132460035084068117, 0.6155034331737432307, 2.025765117643091529 ) ) ;
#180869 = CARTESIAN_POINT ( 'NONE',  ( -4.948362879307902418, 4.875437568721725512, 1.214306433183764966E-14 ) ) ;
#180871 = CARTESIAN_POINT ( 'NONE',  ( -0.6823417656250039265, 8.630208333674733723, -1.181850606188755259 ) ) ;
#180873 = CARTESIAN_POINT ( 'NONE',  ( -6.143440778383317813, 6.339971461045375456, 7.509178883279419847E-06 ) ) ;
#180872 = CARTESIAN_POINT ( 'NONE',  ( 2.173483749353939842, 1.288726691912587041, 1.646222326975780526 ) ) ;
#180875 = ORIENTED_EDGE ( 'NONE', *, *, #88421, .F. ) ;
#180874 = CARTESIAN_POINT ( 'NONE',  ( 0.2875850076352819973, -0.8198804995633873771, 1.517450437728053325 ) ) ;
#180876 = EDGE_CURVE ( 'NONE', #69090, #195242, #78891, .T. ) ;
#180877 = CARTESIAN_POINT ( 'NONE',  ( 6.693975156845185737, 8.832723654451292816, 1.599625672291281386 ) ) ;
#180878 = COLOUR_RGB ( '', 0.66274510, 0.83137255, 0.94901961) ;
#180879 = CYLINDRICAL_SURFACE ( 'NONE', #171903, 0.07999999999999998779 ) ;
#180880 = DIRECTION ( 'NONE',  ( -1.000000000000000000, 0.000000000000000000, 1.224646799147353207E-16 ) ) ;
#180882 = CARTESIAN_POINT ( 'NONE',  ( 10.03267048398825168, 10.80712977418221676, 0.000000000000000000 ) ) ;
#180881 = CARTESIAN_POINT ( 'NONE',  ( 5.686755365928134687, 8.721966129303114101, 1.199719254218462483 ) ) ;
#180884 = CARTESIAN_POINT ( 'NONE',  ( 1.189788175852508845, 1.078664940389061577, 1.455116354534333079 ) ) ;
#180883 = CARTESIAN_POINT ( 'NONE',  ( 7.042534447655770080, 7.180988041878682004, -0.7998128361456341429 ) ) ;
#180885 = CARTESIAN_POINT ( 'NONE',  ( -6.507023659554960204, 9.678945805201045971, 1.199719254218452047 ) ) ;
#180886 = CARTESIAN_POINT ( 'NONE',  ( 5.705283713252285338, 5.550585841749444249, -0.7998128361456211532 ) ) ;
#180887 = CARTESIAN_POINT ( 'NONE',  ( -6.147489916148834332, 6.992309281770507923, 0.9361876800342925353 ) ) ;
#180888 = CARTESIAN_POINT ( 'NONE',  ( 6.723917837734620484, 6.809268663637336516, 0.000000000000000000 ) ) ;
#180889 = CARTESIAN_POINT ( 'NONE',  ( 6.539320575229268684, 7.629137130509104026, 2.396737603865983779 ) ) ;
#180890 = CARTESIAN_POINT ( 'NONE',  ( 0.4019237886466816012, 9.176335450315372455, -1.499999999999998668 ) ) ;
#180891 = CARTESIAN_POINT ( 'NONE',  ( -11.41126283316785361, 11.25874606908456776, 3.405403429622881006 ) ) ;
#180892 = CARTESIAN_POINT ( 'NONE',  ( 10.22248463502393001, 11.02857961705718282, 0.7216878364870438212 ) ) ;
#180893 = ORIENTED_EDGE ( 'NONE', *, *, #37798, .T. ) ;
#180894 = CARTESIAN_POINT ( 'NONE',  ( 2.945584473374110779, 1.314022426170344815, 1.318171089286435560 ) ) ;
#180895 = CARTESIAN_POINT ( 'NONE',  ( 0.1576404624921414199, 1.103540182269863612, 1.565583644703759436 ) ) ;
#180896 = CARTESIAN_POINT ( 'NONE',  ( 6.370143239528382573, 0.9910226482379416169, 1.651782778771145432 ) ) ;
#180897 = CARTESIAN_POINT ( 'NONE',  ( 6.162566008723842081, -0.7415158119226210598, -1.933206815039355320 ) ) ;
#180898 = LINE ( 'NONE', #164657, #192153 ) ;
#180899 = CARTESIAN_POINT ( 'NONE',  ( 4.599920620972065777, 8.367456947080912144, 0.1478172174028801744 ) ) ;
#180900 = CARTESIAN_POINT ( 'NONE',  ( -5.124618876285560454, 5.081069565195661220, 0.7216878364870317197 ) ) ;
#180901 = CARTESIAN_POINT ( 'NONE',  ( 7.890482213473377193, 11.18901776815221716, -1.082531754730543083 ) ) ;
#180902 = CARTESIAN_POINT ( 'NONE',  ( 4.399236341264299632, -1.715665262265529734, 0.9668539646570695201 ) ) ;
#180904 = B_SPLINE_CURVE_WITH_KNOTS ( 'NONE', 3,
 ( #83052, #148080, #19114, #114572 ),
 .UNSPECIFIED., .F., .F.,
 ( 4, 4 ),
 ( 1.043091274928057275E-17, 0.0006764026532485904134 ),
 .UNSPECIFIED. ) ;
#180903 = CARTESIAN_POINT ( 'NONE',  ( 1.823052125313681993, 1.569171740784220281, -1.426411057285102979 ) ) ;
#180905 = CARTESIAN_POINT ( 'NONE',  ( -4.717347382551060342, 7.590990148696470818, 1.199719254218464037 ) ) ;
#180906 = CARTESIAN_POINT ( 'NONE',  ( -11.71938954792528698, 8.545439090133012172, 2.376335979313274560 ) ) ;
#180907 = FACE_OUTER_BOUND ( 'NONE', #87835, .T. ) ;
#180908 = CARTESIAN_POINT ( 'NONE',  ( 5.630878078874809844, -1.982435003639994031, 0.9343296635366815650 ) ) ;
#180909 = CARTESIAN_POINT ( 'NONE',  ( 3.621833129746810265, 4.096114899008192367, 2.420000000000023022 ) ) ;
#180910 = CARTESIAN_POINT ( 'NONE',  ( 4.067344539004444037, 0.2368424065766552566, -1.911724265930745847 ) ) ;
#180911 = CARTESIAN_POINT ( 'NONE',  ( -7.531718027591449705, 8.745758106066849891, 1.199719254218462483 ) ) ;
#180912 = CARTESIAN_POINT ( 'NONE',  ( 0.6744773098602949712, -1.717252091951677384, -0.6198786263262797691 ) ) ;
#180913 = CARTESIAN_POINT ( 'NONE',  ( 1.014635385311330795, -0.9952708415592588231, -1.969785480804244537 ) ) ;
#180914 = EDGE_CURVE ( 'NONE', #162715, #150994, #53459, .T. ) ;
#180915 = DIRECTION ( 'NONE',  ( 0.000000000000000000, 0.000000000000000000, 1.000000000000000000 ) ) ;
#180916 = ORIENTED_EDGE ( 'NONE', *, *, #72672, .T. ) ;
#180917 = CARTESIAN_POINT ( 'NONE',  ( -7.721398836998378812, -6.134628647623499909, 7.721398836998403681 ) ) ;
#180918 = EDGE_LOOP ( 'NONE', ( #11603, #9306, #107959, #125038 ) ) ;
#180919 = CARTESIAN_POINT ( 'NONE',  ( 6.192246204073627247, 0.9737480728593052026, -1.711826031884769339 ) ) ;
#180920 = CARTESIAN_POINT ( 'NONE',  ( 1.645936167706591569, 0.6108386606893880799, 1.843543891229272313 ) ) ;
#180921 = CARTESIAN_POINT ( 'NONE',  ( 6.327535152267887320, -1.632159162827769405, 1.618470562452605455 ) ) ;
#180923 = CARTESIAN_POINT ( 'NONE',  ( 5.471493298581291853, -0.2749614684036653656, 1.840407035693031546 ) ) ;
#180922 = CARTESIAN_POINT ( 'NONE',  ( -7.795011973214244883, 8.058878488363559356, 0.7998128361456341429 ) ) ;
#180924 = CARTESIAN_POINT ( 'NONE',  ( 6.496291879603339758, 7.608037276739255006, 1.199719254218452935 ) ) ;
#180925 = FACE_OUTER_BOUND ( 'NONE', #75895, .T. ) ;
#180926 = CARTESIAN_POINT ( 'NONE',  ( -5.961834861707238531, 7.978559976790334574, -1.599625672291263179 ) ) ;
#180927 = CARTESIAN_POINT ( 'NONE',  ( -3.317034467965191080, -0.9147500475860976810, 0.1576429056095928760 ) ) ;
#180928 = CARTESIAN_POINT ( 'NONE',  ( 1.365048776756357940, 0.1565470504056795942, -2.186014887712848243 ) ) ;
#180929 = CARTESIAN_POINT ( 'NONE',  ( 5.843201017809841247, 5.919415396974013532, 1.040834085586084257E-14 ) ) ;
#180930 = CARTESIAN_POINT ( 'NONE',  ( -2.273105066167321997, 5.702484939155337607, -2.420000000000000373 ) ) ;
#180932 = EDGE_CURVE ( 'NONE', #26714, #130448, #97907, .T. ) ;
#180931 = CARTESIAN_POINT ( 'NONE',  ( 1.330379832379691818, 1.758967509726565792, 0.4888242021733391618 ) ) ;
#180933 = CARTESIAN_POINT ( 'NONE',  ( -4.634189577772691138, 4.300976017023221409, 1.214306433183764966E-14 ) ) ;
#180934 = VECTOR ( 'NONE', #180959, 1000.000000000000000 ) ;
#180935 = CARTESIAN_POINT ( 'NONE',  ( -6.265495719280979259, 6.992744598377811371, -0.9808356887253886214 ) ) ;
#180936 = CARTESIAN_POINT ( 'NONE',  ( 6.509000000000010999, 0.004788705324892603143, 2.000274819378269786 ) ) ;
#180937 = CARTESIAN_POINT ( 'NONE',  ( 0.1331565106231328566, 1.371277436080810208, -2.201942895618694607 ) ) ;
#180938 = AXIS2_PLACEMENT_3D ( 'NONE', #41295, #173425, #45555 ) ;
#180939 = CARTESIAN_POINT ( 'NONE',  ( 0.1879448220486016896, -0.9096115147686645308, 1.698232400582524670 ) ) ;
#180940 = CARTESIAN_POINT ( 'NONE',  ( 4.117980938109369937, 1.947433809354440326, -0.2358448244534834815 ) ) ;
#180941 = CARTESIAN_POINT ( 'NONE',  ( -8.341290820905609138, 10.75459192918846618, 1.599625672291269396 ) ) ;
#180942 = CARTESIAN_POINT ( 'NONE',  ( 5.961834861707224320, 7.978559976790334574, -1.599625672291262513 ) ) ;
#180943 = CARTESIAN_POINT ( 'NONE',  ( 4.934296419935967570, -1.134874685878878520, -1.791058398909770588 ) ) ;
#180944 = CARTESIAN_POINT ( 'NONE',  ( 3.861010967126535576, 0.2669419790740577558, -2.175157288012785184 ) ) ;
#180945 = CARTESIAN_POINT ( 'NONE',  ( 3.825371897350130279, 7.614684313550482031, 0.7998128361456321445 ) ) ;
#180946 = CARTESIAN_POINT ( 'NONE',  ( 2.623957243734816647, 2.031168598393529034, -0.3995267358143372860 ) ) ;
#180948 = CARTESIAN_POINT ( 'NONE',  ( -1.364683531250014514, 0.05104166700808546175, -0.7879004041258359514 ) ) ;
#180947 = CARTESIAN_POINT ( 'NONE',  ( -3.239364772909965661E-16, -5.511313137147274333, -11.00000000000000178 ) ) ;
#180949 = ORIENTED_EDGE ( 'NONE', *, *, #86749, .T. ) ;
#180950 = CARTESIAN_POINT ( 'NONE',  ( 2.567332952821321790, -1.178922594190381146, 1.973231532614614148 ) ) ;
#180951 = CARTESIAN_POINT ( 'NONE',  ( 7.863365906246055914, 10.19701286208565705, -1.443375672974057666 ) ) ;
#180953 = CARTESIAN_POINT ( 'NONE',  ( 3.285556943749998737, -1.305208332855376296, -1.896917185911906500 ) ) ;
#180952 = CARTESIAN_POINT ( 'NONE',  ( 5.234856708652222856, 8.161064355852680308, 1.082531754730549078 ) ) ;
#180955 = ADVANCED_FACE ( 'NONE', ( #173233 ), #213844, .T. ) ;
#180954 = CARTESIAN_POINT ( 'NONE',  ( 6.620655732516623537, 7.629137130509068498, 2.426260288887295058 ) ) ;
#180956 = CARTESIAN_POINT ( 'NONE',  ( -10.42538027328838801, 5.087954508094563622, -5.944375093558058154 ) ) ;
#180957 = CARTESIAN_POINT ( 'NONE',  ( 3.240110121693033474, 0.4724093276110411521, 1.883494029347228871 ) ) ;
#180958 = ORIENTED_EDGE ( 'NONE', *, *, #138558, .T. ) ;
#180959 = DIRECTION ( 'NONE',  ( -0.7592566023652995710, -0.6507913734559650498, -0.000000000000000000 ) ) ;
#180960 = EDGE_CURVE ( 'NONE', #79990, #80159, #167557, .T. ) ;
#180961 = CARTESIAN_POINT ( 'NONE',  ( 3.498220628606643956, -0.9384276995785534314, 1.666209768436441419 ) ) ;
#180962 = CARTESIAN_POINT ( 'NONE',  ( 5.209832820053398983, -1.716139821054706749, 0.1720855783484842860 ) ) ;
#180963 = CARTESIAN_POINT ( 'NONE',  ( 3.186732694495420848, 1.586669336078951664, -1.244385354607212335 ) ) ;
#180964 = CARTESIAN_POINT ( 'NONE',  ( 5.643294731490863470, 0.9288382957042642385, 2.102849567203187053 ) ) ;
#180965 = CARTESIAN_POINT ( 'NONE',  ( 11.41381675112453387, 12.69999999999998153, 3.704697986577180746 ) ) ;
#180966 = CARTESIAN_POINT ( 'NONE',  ( 0.7334016978863610037, 0.1661181961954381059, 2.200687262777756725 ) ) ;
#180967 = CARTESIAN_POINT ( 'NONE',  ( -3.689227196694341515, 7.318199139536432973, -0.7216878364870458196 ) ) ;
#180968 = CARTESIAN_POINT ( 'NONE',  ( 5.676936032674533728, -0.04454931526533602304, -1.769330457910125443 ) ) ;
#180970 = CARTESIAN_POINT ( 'NONE',  ( 2.291363848578463980, 1.773334254936178356, 1.452501744581054632 ) ) ;
#180969 = CARTESIAN_POINT ( 'NONE',  ( 4.688087255275310561, 8.691461907788344377, -0.7998128361456381397 ) ) ;
#180971 = CARTESIAN_POINT ( 'NONE',  ( 0.9721243863554385189, -0.03892262269361351779, -1.740072766964487316 ) ) ;
#180972 = CARTESIAN_POINT ( 'NONE',  ( -7.944151662964566540, 8.232874793072271657, 0.000000000000000000 ) ) ;
#180973 = CIRCLE ( 'NONE', #177431, 0.08000000000000041800 ) ;
#180974 = CARTESIAN_POINT ( 'NONE',  ( 6.703104427915338448, -0.4847493572297522091, 2.145077170986497528 ) ) ;
#180975 = CARTESIAN_POINT ( 'NONE',  ( -5.517242166118370150, 5.401480380085008193, 0.7998128361456281477 ) ) ;
#180976 = CARTESIAN_POINT ( 'NONE',  ( -1.360316468750056851, 0.6510416670080609869, -0.7853790794158981292 ) ) ;
#180977 = CARTESIAN_POINT ( 'NONE',  ( -11.44779963594988814, 12.69999999999998153, 3.600000000000001421 ) ) ;
#180978 = CARTESIAN_POINT ( 'NONE',  ( 1.680376142759659075, -1.205403815041187210, -1.805639882349929781 ) ) ;
#180979 = CARTESIAN_POINT ( 'NONE',  ( 2.870327622459168726, -1.987497926849005836, -0.3399570244180456502 ) ) ;
#180980 = B_SPLINE_CURVE_WITH_KNOTS ( 'NONE', 3,
 ( #30020, #98226, #45219, #64642, #144874, #95035, #47354 ),
 .UNSPECIFIED., .F., .F.,
 ( 4, 3, 4 ),
 ( 0.0001932293135873452484, 0.0009000000018422023643, 0.002089330742406755349 ),
 .UNSPECIFIED. ) ;
#180981 = CARTESIAN_POINT ( 'NONE',  ( -1.500000000000015099, 0.4104166673494891726, -0.8660254037844383745 ) ) ;
#180982 = CARTESIAN_POINT ( 'NONE',  ( 5.356054764349521768, 1.924192155146129624, -0.09673933992536233595 ) ) ;
#180983 = CARTESIAN_POINT ( 'NONE',  ( -0.6823417656250003738, 12.90104166700806232, 1.181850606188754593 ) ) ;
#180984 = CARTESIAN_POINT ( 'NONE',  ( 2.250487404410873804, 1.042729518208513007, -1.961448655418545739 ) ) ;
#180985 = ORIENTED_EDGE ( 'NONE', *, *, #81885, .F. ) ;
#180986 = CARTESIAN_POINT ( 'NONE',  ( -3.667411383892738019, 3.520940564220485847, 2.447588313016640704 ) ) ;
#180987 = CARTESIAN_POINT ( 'NONE',  ( -0.1216878429548678975, 3.463015919485879834, -1.996294584693599994 ) ) ;
#180988 = CARTESIAN_POINT ( 'NONE',  ( 8.218213668177886788, 12.73966637951625813, 0.7998128361456462443 ) ) ;
#180989 = SURFACE_SIDE_STYLE ('',( #146394 ) ) ;
#180990 = CARTESIAN_POINT ( 'NONE',  ( 5.091228679354776965, -0.6197342532976670704, 1.626566373401008070 ) ) ;
#180991 = CARTESIAN_POINT ( 'NONE',  ( 3.209375601822930690, -1.602329130913646926, -1.131729396966949963 ) ) ;
#180993 = CARTESIAN_POINT ( 'NONE',  ( -7.876924059859742755, 8.292092279365579799, 1.040834085586084257E-14 ) ) ;
#180992 = CARTESIAN_POINT ( 'NONE',  ( 4.792970997630896512, 5.550553237779539018, 1.199719254218464037 ) ) ;
#180994 = CARTESIAN_POINT ( 'NONE',  ( 4.886124051547468206, -1.072500323723464932, 1.992072436074944219 ) ) ;
#180995 = COLOUR_RGB ( '', 0.40784314, 0.44705882, 0.49803922) ;
#180996 = COLOUR_RGB ( '', 0.09019608, 0.27058824, 0.51372549) ;
#180997 = CARTESIAN_POINT ( 'NONE',  ( 0.7837256325555241876, -1.959260395640700203, 0.6451903852672227213 ) ) ;
#180998 = CARTESIAN_POINT ( 'NONE',  ( -8.030507057996002729, 8.263346410617135263, 1.040834085586084257E-14 ) ) ;
#180999 = CARTESIAN_POINT ( 'NONE',  ( -2.290964770585000920, 5.616616632417037458, -0.7216878364870257245 ) ) ;
#181000 = CARTESIAN_POINT ( 'NONE',  ( 1.921153072736818013, 2.111338651666348376, 0.8135812809707074766 ) ) ;
#181001 = ORIENTED_EDGE ( 'NONE', *, *, #118553, .T. ) ;
#181002 = CARTESIAN_POINT ( 'NONE',  ( -1.500000000000013101, 1.202083334016148974, 0.8660254037844403729 ) ) ;
#181003 = CARTESIAN_POINT ( 'NONE',  ( 2.249088872875557144, -1.499603784168266563, -1.117866018216478574 ) ) ;
#181004 = CARTESIAN_POINT ( 'NONE',  ( 1.617354066682510805, 0.1696363612940926524, 1.725835137016252796 ) ) ;
#181005 = CARTESIAN_POINT ( 'NONE',  ( 4.775033345069852331, 2.044829088842615494, -0.7888500489584143738 ) ) ;
#181006 = CARTESIAN_POINT ( 'NONE',  ( 6.335062919620514599, 0.2175189359726207861, 2.297324976709664845 ) ) ;
#181007 = CARTESIAN_POINT ( 'NONE',  ( 1.375931059888847896, 1.226954981729235561, 1.655701539656707411 ) ) ;
#181008 = CARTESIAN_POINT ( 'NONE',  ( 4.083879184154452169, -1.920976184332440662, -0.2838548334032560683 ) ) ;
#181009 = CARTESIAN_POINT ( 'NONE',  ( -2.751941993449643409, 6.154423392425789174, 0.7216878364870317197 ) ) ;
#181010 = CARTESIAN_POINT ( 'NONE',  ( 6.591075523649926993, 1.627300515804396941, -0.9222108319836411772 ) ) ;
#181011 = CARTESIAN_POINT ( 'NONE',  ( 1.406250000000001332, 1.895863743164055926, -0.7852924748300647018 ) ) ;
#181012 = CARTESIAN_POINT ( 'NONE',  ( 4.041346116833469893, 7.538066791021210022, -0.4365389052301202333 ) ) ;
#181013 = CARTESIAN_POINT ( 'NONE',  ( 6.362657644764971643, -0.6818896071447739793, 1.897407954007489295 ) ) ;
#181014 = CARTESIAN_POINT ( 'NONE',  ( 1.042866153392195239, -3.232243495192089089, 3.126988198976878408 ) ) ;
#181015 = CARTESIAN_POINT ( 'NONE',  ( -1.360316468750046859, 0.6197916670081009549, -0.7853790794159322131 ) ) ;
#181017 = CARTESIAN_POINT ( 'NONE',  ( 5.871720251644387822, -0.2986239867289949834, -1.994071864161291119 ) ) ;
#181016 = AXIS2_PLACEMENT_3D ( 'NONE', #206347, #56910, #123083 ) ;
#181018 = CARTESIAN_POINT ( 'NONE',  ( -10.65400978224035811, 11.32409958890225710, 1.040834085586084257E-14 ) ) ;
#181019 = CARTESIAN_POINT ( 'NONE',  ( 7.283754839039659146, 9.520799950344851936, -1.599625672291262513 ) ) ;
#181020 = CARTESIAN_POINT ( 'NONE',  ( 4.065465959251388206, 5.836405933916976707, -1.599625672291269396 ) ) ;
#181022 = SURFACE_SIDE_STYLE ('',( #17430 ) ) ;
#181021 = CARTESIAN_POINT ( 'NONE',  ( 1.998415063578623085, -0.4859047700337820741, -1.759764234465097221 ) ) ;
#181023 = EDGE_CURVE ( 'NONE', #18660, #151743, #108884, .T. ) ;
#181024 = CARTESIAN_POINT ( 'NONE',  ( 1.499999999999990896, 5.275000000000022560, 1.214306433183764966E-14 ) ) ;
#181025 = CARTESIAN_POINT ( 'NONE',  ( -10.59782195348455680, 9.799999999999997158, -3.302675849420335652 ) ) ;
#181026 = ORIENTED_EDGE ( 'NONE', *, *, #99713, .T. ) ;
#181027 = CARTESIAN_POINT ( 'NONE',  ( -4.136646265500964148, 6.879818838842817641, -1.082531754730551743 ) ) ;
#181028 = UNCERTAINTY_MEASURE_WITH_UNIT (LENGTH_MEASURE( 1.000000000000000082E-05 ), #179827, 'distance_accuracy_value', 'NONE');
#181029 = CARTESIAN_POINT ( 'NONE',  ( 1.642778471875000035, -3.813541666188708490, -2.845375778867859751 ) ) ;
#181030 = CARTESIAN_POINT ( 'NONE',  ( -8.134002093194872884, 11.57708731111429401, 1.199719254218453823 ) ) ;
#181031 = CARTESIAN_POINT ( 'NONE',  ( 6.533853655515883041, -1.958494339806987394, 0.4928751659435038901 ) ) ;
#181032 = CARTESIAN_POINT ( 'NONE',  ( 0.01256502854718108061, -2.120115106878577294, -0.04748564598491820943 ) ) ;
#181033 = CIRCLE ( 'NONE', #87651, 0.04999999999999972522 ) ;
#181034 = ORIENTED_EDGE ( 'NONE', *, *, #162651, .F. ) ;
#181035 = CARTESIAN_POINT ( 'NONE',  ( -6.557303570864871034, 7.679217583210999010, -1.199719254218452047 ) ) ;
#181036 = CARTESIAN_POINT ( 'NONE',  ( 4.517891501851804215, 6.293959390292322986, -1.599625672291255185 ) ) ;
#181037 = CARTESIAN_POINT ( 'NONE',  ( 6.139539385720709674, -1.490912338237950108, -1.423074965643542411 ) ) ;
#181038 = CARTESIAN_POINT ( 'NONE',  ( 5.361953999179126740, -0.05229508359532940298, -2.015913028294749942 ) ) ;
#181039 = ORIENTED_EDGE ( 'NONE', *, *, #65677, .F. ) ;
#181040 = EDGE_LOOP ( 'NONE', ( #30224, #166508, #148413, #4567, #171055 ) ) ;
#181041 = CARTESIAN_POINT ( 'NONE',  ( -5.342823980928611327, 4.390142039796957718, 2.499999999999999112 ) ) ;
#181042 = DIRECTION ( 'NONE',  ( 0.6507913734559640506, -0.7592566023653004592, 0.000000000000000000 ) ) ;
#181044 = PLANE ( 'NONE',  #86067 ) ;
#181043 = CARTESIAN_POINT ( 'NONE',  ( -5.661411662158206681, 8.762674818229999829, -1.199719254218452047 ) ) ;
#181045 = CARTESIAN_POINT ( 'NONE',  ( 6.400241882075590638, 6.902609158730609096, 0.7749192096189911894 ) ) ;
#181046 = CARTESIAN_POINT ( 'NONE',  ( 4.675157572021750418, -0.8594996001172333644, -1.823839583407538267 ) ) ;
#181047 = CARTESIAN_POINT ( 'NONE',  ( 5.085823778388903982, -1.827637283562512538, -0.2220107604927607503 ) ) ;
#181048 = CARTESIAN_POINT ( 'NONE',  ( -1.154700538379266339, -4.295408888568413630, 2.602085213965210642E-15 ) ) ;
#181049 = CARTESIAN_POINT ( 'NONE',  ( 3.106426088690077858, -2.305020500623474522, 0.1135576804369240328 ) ) ;
#181050 = CARTESIAN_POINT ( 'NONE',  ( 6.692885107001518286, 7.837396042037102717, -1.199719254218452047 ) ) ;
#181051 = CARTESIAN_POINT ( 'NONE',  ( 5.905597126736788383, -0.5315564325061740147, 2.095088507090197893 ) ) ;
#181052 = CARTESIAN_POINT ( 'NONE',  ( 8.145751363712157911, 8.397798100619326078, -0.7998128361456281477 ) ) ;
#181053 = CARTESIAN_POINT ( 'NONE',  ( 1.188897196845212445, 1.471763766255501427, 1.267211023470141695 ) ) ;
#181054 = CARTESIAN_POINT ( 'NONE',  ( -3.273404022695637572, 5.906389562198459231, 1.199719254218462483 ) ) ;
#181055 = ORIENTED_EDGE ( 'NONE', *, *, #78162, .F. ) ;
#181056 = CARTESIAN_POINT ( 'NONE',  ( 4.710533686004090725, -1.772996550310073971, -1.462542180504990075 ) ) ;
#181057 = CARTESIAN_POINT ( 'NONE',  ( 1.123270288254022198, 2.908552654332631437, -0.7749999999939810591 ) ) ;
#181058 = CARTESIAN_POINT ( 'NONE',  ( -5.517242166118370150, 5.401480380085008193, 0.7998128361456281477 ) ) ;
#181059 = CARTESIAN_POINT ( 'NONE',  ( 3.028041890241763401, 1.040506211802554981, -1.554362669439563360 ) ) ;
#181062 = CARTESIAN_POINT ( 'NONE',  ( -4.776215253764153346, 8.794277906025310898, -0.7998128361456362523 ) ) ;
#181061 = CARTESIAN_POINT ( 'NONE',  ( -0.7500000000000215383, 0.7229166673494852313, 1.299038105676659116 ) ) ;
#181060 = CARTESIAN_POINT ( 'NONE',  ( 1.564566645345835116, 0.6029492335615972420, 1.814891859350221459 ) ) ;
#181063 = CARTESIAN_POINT ( 'NONE',  ( 2.965657822035951963, 0.3232568108629539361, -2.182957019552448141 ) ) ;
#181064 = CARTESIAN_POINT ( 'NONE',  ( -1.492681600543587006, 8.694743381153374528, -2.590460435319442922 ) ) ;
#181065 = CARTESIAN_POINT ( 'NONE',  ( 3.379006598303866848, 4.965260336153046516, -1.599625672291262513 ) ) ;
#181066 = CARTESIAN_POINT ( 'NONE',  ( 7.471952054462756010, 7.889901283060952508, 0.7216878364870267237 ) ) ;
#181067 = CARTESIAN_POINT ( 'NONE',  ( -3.002240950422295995, 5.590032644546251817, -1.199719254218452935 ) ) ;
#181068 = CARTESIAN_POINT ( 'NONE',  ( -7.119440060507479018, 8.439006504414422238, 1.082531754730549078 ) ) ;
#181069 = CARTESIAN_POINT ( 'NONE',  ( 0.5968690581132638506, 1.641441770537595435, -1.091469919712923176 ) ) ;
#181070 = CARTESIAN_POINT ( 'NONE',  ( 0.7808295286375503963, -1.278884537891399553, 1.920602667021213961 ) ) ;
#181071 = CARTESIAN_POINT ( 'NONE',  ( 1.205434515183744226, -1.544416933936803904, -1.209700862059132964 ) ) ;
#181072 = CARTESIAN_POINT ( 'NONE',  ( 5.664908073332702187, 1.565568307794177327, -1.342975779555633187 ) ) ;
#181073 = CARTESIAN_POINT ( 'NONE',  ( 5.341549334104194635, 6.294524313618772737, 1.082531754730558626 ) ) ;
#181074 = CARTESIAN_POINT ( 'NONE',  ( 6.638652492546827766, 7.774124658506663010, 1.199719254218452047 ) ) ;
#181075 = ORIENTED_EDGE ( 'NONE', *, *, #162333, .T. ) ;
#181076 = CARTESIAN_POINT ( 'NONE',  ( -0.6823417656250212460, 4.613541667008086655, 1.181850606188767472 ) ) ;
#181077 = CARTESIAN_POINT ( 'NONE',  ( -2.279984679289828176, 5.601133616484927025, -0.06592222766762731445 ) ) ;
#181078 = CARTESIAN_POINT ( 'NONE',  ( 4.487385655998888723, 4.337630808194552934, 0.7216878364870317197 ) ) ;
#181079 = CARTESIAN_POINT ( 'NONE',  ( 0.7257146478014552260, 0.2145687282662836204, -2.160472036209131197 ) ) ;
#181081 = CARTESIAN_POINT ( 'NONE',  ( 5.882333747326812023, -0.2767177626767613474, -1.820229446528654371 ) ) ;
#181080 = CARTESIAN_POINT ( 'NONE',  ( 0.6124999999999793943, 0.4791666673494773820, -1.060881119635969094 ) ) ;
#181082 = DIRECTION ( 'NONE',  ( 0.000000000000000000, 0.000000000000000000, 1.000000000000000000 ) ) ;
#181083 = CARTESIAN_POINT ( 'NONE',  ( -0.9311234436981532525, -1.678130369558482826, 3.474999999999999201 ) ) ;
#181084 = CARTESIAN_POINT ( 'NONE',  ( 1.440467042440606749, 0.3595057747620767907, 1.835501880432292010 ) ) ;
#181085 = CARTESIAN_POINT ( 'NONE',  ( 5.641917277892137150, 0.8817427965214555963, -1.973778517010720490 ) ) ;
#181087 = EDGE_CURVE ( 'NONE', #47238, #149901, #61590, .T. ) ;
#181086 = CARTESIAN_POINT ( 'NONE',  ( -6.082978790695654503, 6.030206930409384825, -0.4315292173028318912 ) ) ;
#181088 = CARTESIAN_POINT ( 'NONE',  ( -0.02264175331117417728, 6.946776101658422853, -2.684156320254589279 ) ) ;
#181089 = CARTESIAN_POINT ( 'NONE',  ( -1.402160292154681736E-14, -0.6781249996585819728, 1.575800808251672791 ) ) ;
#181090 = CARTESIAN_POINT ( 'NONE',  ( 1.295406243800485635, 1.766531960031037407, -0.7327172462580702206 ) ) ;
#181091 = TOROIDAL_SURFACE ( 'NONE', #170558, 5.799999999999999822, 0.4000000000000000222 ) ;
#181092 = CARTESIAN_POINT ( 'NONE',  ( 3.449836819150660538, 1.770032027316788437, 0.0008499603425977939660 ) ) ;
#181093 = CARTESIAN_POINT ( 'NONE',  ( 1.049298088506251947, -1.728493729547801117, 0.8183166869351958805 ) ) ;
#181095 = CARTESIAN_POINT ( 'NONE',  ( 5.202711523826980766, 1.771732004023411911, 0.7288693050919017313 ) ) ;
#181094 = CARTESIAN_POINT ( 'NONE',  ( 1.693866981432350594, -3.230387921952247332, 2.823574758769644255 ) ) ;
#181096 = CARTESIAN_POINT ( 'NONE',  ( -1.402160292154681736E-14, -1.037499999999977662, 1.732050807568877637 ) ) ;
#181097 = CARTESIAN_POINT ( 'NONE',  ( 6.127403468923573904, 0.1463605449630276667, -1.964188589371117954 ) ) ;
#181098 = CARTESIAN_POINT ( 'NONE',  ( -1.500000000000011324, 4.420833333333352044, 0.8660254037844403729 ) ) ;
#181100 = ADVANCED_FACE ( 'NONE', ( #45359 ), #60416, .F. ) ;
#181099 = CARTESIAN_POINT ( 'NONE',  ( 1.336355901170083849, -1.182550835430173919, -1.760063440837428272 ) ) ;
#181101 = CARTESIAN_POINT ( 'NONE',  ( 6.610000000000008313, 7.629137130509070275, 2.600000000000001421 ) ) ;
#181102 = CARTESIAN_POINT ( 'NONE',  ( 3.942156681999692491, 1.861596489644477437, 0.1839347620080991341 ) ) ;
#181104 = ORIENTED_EDGE ( 'NONE', *, *, #58523, .T. ) ;
#181103 = CARTESIAN_POINT ( 'NONE',  ( 0.9612317138737861422, 0.3586375672061762887, -1.789940867121169843 ) ) ;
#181105 = CARTESIAN_POINT ( 'NONE',  ( 4.442132104469964204, 0.9450947508268662256, -1.994404356956205326 ) ) ;
#181106 = CARTESIAN_POINT ( 'NONE',  ( 1.364683531249990311, 4.676041667008083103, 0.7879004041258500513 ) ) ;
#181107 = CARTESIAN_POINT ( 'NONE',  ( 2.102078608570765450, 0.7915390796853873923, -1.904948021121543711 ) ) ;
#181109 = EDGE_CURVE ( 'NONE', #98073, #60619, #101849, .T. ) ;
#181108 = CARTESIAN_POINT ( 'NONE',  ( 6.582647274634798151, 7.638508894284114170, 1.199719254218462483 ) ) ;
#181110 = CARTESIAN_POINT ( 'NONE',  ( -8.097244055859620815, 10.46987070330147063, -1.599625672291263179 ) ) ;
#181111 = CARTESIAN_POINT ( 'NONE',  ( -3.463051730202630019, -0.006534250585093354102, -0.1996569003990655289 ) ) ;
#181112 = CARTESIAN_POINT ( 'NONE',  ( 0.1753634416057739953, 5.721028741045294908, -2.738064866945366660 ) ) ;
#181113 = EDGE_LOOP ( 'NONE', ( #55487, #109377, #189840, #57892 ) ) ;
#181114 = CARTESIAN_POINT ( 'NONE',  ( 4.000488093070094564, 2.060113009926473726, 0.2059288336104248551 ) ) ;
#181115 = CARTESIAN_POINT ( 'NONE',  ( 1.499999999999989120, 5.504166666666685970, 0.8660254037844524744 ) ) ;
#181116 = CARTESIAN_POINT ( 'NONE',  ( 1.704591423195594535, -0.7763021076895927353, -2.017573427605146907 ) ) ;
#181117 = CARTESIAN_POINT ( 'NONE',  ( -5.543397514969483630, 7.443247485022737031, -1.247832777738608678 ) ) ;
#181118 = CARTESIAN_POINT ( 'NONE',  ( 2.526040989133854886, -1.997384215488164694, 0.2984307725432763236 ) ) ;
#181119 = CARTESIAN_POINT ( 'NONE',  ( 4.771998164587357927, 6.814557936359840085, -1.288453177375107783 ) ) ;
#181120 = VERTEX_POINT ( 'NONE', #109353 ) ;
#181122 = CARTESIAN_POINT ( 'NONE',  ( 7.619319141200051604, 11.83303006480134911, 0.7216878364870438212 ) ) ;
#181121 = CARTESIAN_POINT ( 'NONE',  ( 0.000000000000000000, -3.587500000000000355, -4.012584370867899430 ) ) ;
#181123 = CARTESIAN_POINT ( 'NONE',  ( 0.1653080603930551784, -5.324706741106330909, 10.99896775280371308 ) ) ;
#181124 = CARTESIAN_POINT ( 'NONE',  ( 0.05782782957228919940, 1.164991625563294386, 1.645756161228327130 ) ) ;
#181125 = CARTESIAN_POINT ( 'NONE',  ( 4.423480980095358284, -1.348712413769267426, -1.727291790683552541 ) ) ;
#181126 = CARTESIAN_POINT ( 'NONE',  ( -1.500000000000013101, 3.660416667349488673, -0.8660254037844313801 ) ) ;
#181127 = CARTESIAN_POINT ( 'NONE',  ( 4.078302138561982204, 0.9061299177482335931, 1.684124486321957104 ) ) ;
#181128 = CARTESIAN_POINT ( 'NONE',  ( -3.795392936821753604, 6.515376628678959392, -1.199719254218452047 ) ) ;
#181129 = CARTESIAN_POINT ( 'NONE',  ( 4.080641047588898118, 5.783833860318930320, -1.443375672974051449 ) ) ;
#181131 = CARTESIAN_POINT ( 'NONE',  ( 2.337517745082304810, 0.5350678814987767096, -1.944078148028173914 ) ) ;
#181130 = CARTESIAN_POINT ( 'NONE',  ( -8.622622508166983835, 13.00355065959610279, 1.040834085586084257E-14 ) ) ;
#181132 = CARTESIAN_POINT ( 'NONE',  ( 1.364683531249996529, 12.27604166700806054, 0.7879004041258405033 ) ) ;
#181133 = B_SPLINE_CURVE_WITH_KNOTS ( 'NONE', 3,
 ( #23591, #60366, #122271, #57179 ),
 .UNSPECIFIED., .F., .F.,
 ( 4, 4 ),
 ( 0.000000000000000000, 0.0007700259059032546743 ),
 .UNSPECIFIED. ) ;
#181135 = CARTESIAN_POINT ( 'NONE',  ( -2.844178363816758814, 6.540234867753325076, -0.7998128361456481317 ) ) ;
#181134 = CARTESIAN_POINT ( 'NONE',  ( 0.8730959291491724450, -0.06322356207747076295, -2.291674109354911781 ) ) ;
#181136 = CARTESIAN_POINT ( 'NONE',  ( 3.856244308521704411, 0.6209911617112495730, 1.609288963722750765 ) ) ;
#181137 = FACE_BOUND ( 'NONE', #88964, .T. ) ;
#181138 = CARTESIAN_POINT ( 'NONE',  ( 3.846762897975340767, 5.510976019103107859, -1.599625672291256295 ) ) ;
#181139 = CARTESIAN_POINT ( 'NONE',  ( 0.07755575628183573877, -0.002876890934064984216, -2.188974970840869005 ) ) ;
#181140 = CARTESIAN_POINT ( 'NONE',  ( 0.09234973940512071489, -0.4041859633337717694, -1.833079292876439670 ) ) ;
#181141 = CARTESIAN_POINT ( 'NONE',  ( 5.054492339796319733, 4.791329239384148231, -0.7998128361456211532 ) ) ;
#181142 = CARTESIAN_POINT ( 'NONE',  ( 0.1753634416057739953, 5.721028741045294908, -2.738064866945366660 ) ) ;
#181143 = ORIENTED_EDGE ( 'NONE', *, *, #105829, .F. ) ;
#181144 = PRESENTATION_STYLE_ASSIGNMENT (( #224 ) ) ;
#181145 = EDGE_LOOP ( 'NONE', ( #150382, #54251, #37864, #45132, #203213, #171282, #55333, #124245, #21355, #183310, #128924, #125574, #123743 ) ) ;
#181146 = CARTESIAN_POINT ( 'NONE',  ( 4.846265894328573687, 0.9266178045349574566, -1.556377301703376625 ) ) ;
#181147 = ORIENTED_EDGE ( 'NONE', *, *, #85714, .T. ) ;
#181148 = CARTESIAN_POINT ( 'NONE',  ( 5.204350862799327793, 7.165104988056252289, -1.599625672291281386 ) ) ;
#181149 = CARTESIAN_POINT ( 'NONE',  ( 0.000000000000000000, 4.000007913748540922, 0.000000000000000000 ) ) ;
#181150 = CARTESIAN_POINT ( 'NONE',  ( 5.584552742667589165, -1.144318741887658586, 1.404276898221923364 ) ) ;
#181151 = CARTESIAN_POINT ( 'NONE',  ( 6.224601922005513543, 7.395028676162137771, -1.082531754730548412 ) ) ;
#181152 = CARTESIAN_POINT ( 'NONE',  ( -11.88172094500852971, 9.720000056015496881, -1.685553348215898861 ) ) ;
#181153 = CARTESIAN_POINT ( 'NONE',  ( 2.502122453320880346, -0.8398649383675671487, -2.024319193490734303 ) ) ;
#181155 = CARTESIAN_POINT ( 'NONE',  ( 9.402743226277308963, 10.92862083786708816, -1.199719254218446718 ) ) ;
#181154 = CARTESIAN_POINT ( 'NONE',  ( 6.584420904419787668, 1.070383488754884649, -1.522209605261907406 ) ) ;
#181156 = CARTESIAN_POINT ( 'NONE',  ( 4.007376490896687571, -1.831982314510060883, 0.5597367571646000295 ) ) ;
#181157 = CARTESIAN_POINT ( 'NONE',  ( 2.449293598294706414E-16, -0.5000000000000004441, -2.000000000000000000 ) ) ;
#181158 =( NAMED_UNIT ( * ) PLANE_ANGLE_UNIT ( ) SI_UNIT ( $, .RADIAN. ) );
#181159 = CARTESIAN_POINT ( 'NONE',  ( 0.6823417656249882723, -0.1572916663252488245, 1.181850606188755259 ) ) ;
#181160 = AXIS2_PLACEMENT_3D ( 'NONE', #144308, #115013, #78180 ) ;
#181161 = CARTESIAN_POINT ( 'NONE',  ( 7.144783764721768904, 7.437928601704619780, 1.040834085586084257E-14 ) ) ;
#181163 = CARTESIAN_POINT ( 'NONE',  ( 5.384029865600029829, -2.117513407852515073, 0.002815966404249789501 ) ) ;
#181162 = CARTESIAN_POINT ( 'NONE',  ( -4.302014814237876017, 3.913438792899272212, 0.7998128361456341429 ) ) ;
#181164 = CARTESIAN_POINT ( 'NONE',  ( 0.8839147992780392871, 1.452536163361785260, 1.601146772000871188 ) ) ;
#181165 = CARTESIAN_POINT ( 'NONE',  ( -4.610654757099099221, 7.536791762327691657, 1.199719254218452935 ) ) ;
#181166 = CARTESIAN_POINT ( 'NONE',  ( 5.337069745634900997, 6.255611453776062980, 1.199719254218452047 ) ) ;
#181167 = CARTESIAN_POINT ( 'NONE',  ( 0.9205982885796895054, 1.684962172289593996, 0.7030880920091547859 ) ) ;
#181168 = CARTESIAN_POINT ( 'NONE',  ( -4.762992037102518950, 4.451245552908022596, -0.7998128361456221525 ) ) ;
#181169 = CARTESIAN_POINT ( 'NONE',  ( 3.346530664597209714, 0.4423686283943834563, 1.771051422834311051 ) ) ;
#181170 = EDGE_CURVE ( 'NONE', #180001, #105092, #122835, .T. ) ;
#181171 = CARTESIAN_POINT ( 'NONE',  ( 9.299556801071242162, 12.92894989638156922, -8.960987479870890837 ) ) ;
#181172 = ORIENTED_EDGE ( 'NONE', *, *, #129757, .F. ) ;
#181173 = CARTESIAN_POINT ( 'NONE',  ( 2.629305401816001808, 0.09940027615944720119, -1.967183499748959452 ) ) ;
#181174 = VERTEX_POINT ( 'NONE', #57331 ) ;
#181175 = CARTESIAN_POINT ( 'NONE',  ( 5.003436869212060323, -1.932333990966347503, 0.1943045992871711702 ) ) ;
#181176 = CARTESIAN_POINT ( 'NONE',  ( -6.994027139803241866, 9.253060644560830994, -1.599625672291271394 ) ) ;
#181178 = CARTESIAN_POINT ( 'NONE',  ( 5.818629517237746462, -0.7649446623404360102, -1.977987144599784086 ) ) ;
#181177 = CARTESIAN_POINT ( 'NONE',  ( 6.047819040147648373, 9.213483425884394507, 1.199719254218452047 ) ) ;
#181179 = CARTESIAN_POINT ( 'NONE',  ( -6.392116398764163598, 6.567141947922926271, -2.438447736784542297 ) ) ;
#181180 = CARTESIAN_POINT ( 'NONE',  ( 3.070860992347378637, -1.446505282863861375, 1.250851760459831041 ) ) ;
#181181 = CARTESIAN_POINT ( 'NONE',  ( 5.889294496748854968, 6.159041356224602026, -0.8323295365256941913 ) ) ;
#181182 = DIRECTION ( 'NONE',  ( 0.000000000000000000, 1.000000000000000000, 0.000000000000000000 ) ) ;
#181183 = CARTESIAN_POINT ( 'NONE',  ( 4.203910148689107729, 7.062256385849379647, -1.199719254218448494 ) ) ;
#181184 = CARTESIAN_POINT ( 'NONE',  ( 3.949861574111676266, -1.389792608731334811, -1.456582260380126392 ) ) ;
#181185 = PLANE ( 'NONE',  #192861 ) ;
#181186 = CARTESIAN_POINT ( 'NONE',  ( 5.127504350819418910, -1.732488751877172772, 0.5760870007271366999 ) ) ;
#181187 = CARTESIAN_POINT ( 'NONE',  ( 0.9419464005683106933, 1.389173191389100115, 1.535309223701806225 ) ) ;
#181188 = CARTESIAN_POINT ( 'NONE',  ( -7.185458225562757484, 11.32685899655781903, 0.7216878364870458196 ) ) ;
#181189 = CARTESIAN_POINT ( 'NONE',  ( -6.600870636098118638, 6.767368133241304484, -0.2259646751960984468 ) ) ;
#181190 = DIRECTION ( 'NONE',  ( 0.000000000000000000, 0.000000000000000000, 1.000000000000000000 ) ) ;
#181191 = CARTESIAN_POINT ( 'NONE',  ( 5.453920962983416665, 1.868457504587007545, -0.09292587778651077712 ) ) ;
#181192 = CARTESIAN_POINT ( 'NONE',  ( 7.962716289927667113, 8.184257181204083409, -0.7998128361456291469 ) ) ;
#181193 = CARTESIAN_POINT ( 'NONE',  ( -4.843287188579803448, 6.673587691474970107, -1.599625672291256517 ) ) ;
#181194 = CARTESIAN_POINT ( 'NONE',  ( 0.6823417656249934904, 10.00520833367472839, 1.181850606188764807 ) ) ;
#181195 = CARTESIAN_POINT ( 'NONE',  ( -3.913499895838973508, 7.717500311787445000, 1.040834085586084257E-14 ) ) ;
#181196 = CARTESIAN_POINT ( 'NONE',  ( -3.811250578772981346, 6.500190537660166079, -1.082531754730546636 ) ) ;
#181197 = CARTESIAN_POINT ( 'NONE',  ( -4.693093728624763372, 8.627026450037540428, 0.7998128361456481317 ) ) ;
#181198 = CARTESIAN_POINT ( 'NONE',  ( 0.7431355771655088205, -0.2497938498803170537, -2.055034051290441255 ) ) ;
#181199 = CARTESIAN_POINT ( 'NONE',  ( 2.636446987817195886, 0.7160595562910974099, 1.992577970932450704 ) ) ;
#181200 = CARTESIAN_POINT ( 'NONE',  ( 9.562578416340237197, 10.05076299535211781, 0.7998128361456462443 ) ) ;
#181201 = CARTESIAN_POINT ( 'NONE',  ( -0.1099460098626957039, 6.494484681433106310, 3.110387376256865011 ) ) ;
#181202 = CARTESIAN_POINT ( 'NONE',  ( 5.963751281166302043, -0.5086355806236466659, 2.006660534352236347 ) ) ;
#181203 = CARTESIAN_POINT ( 'NONE',  ( 4.469394083494863779, 7.278994484577430590, 1.251062204184281379 ) ) ;
#181204 = CARTESIAN_POINT ( 'NONE',  ( 4.690757960648221037, 7.456006139856155457, 1.082531754730558626 ) ) ;
#181206 = CARTESIAN_POINT ( 'NONE',  ( 3.673896439178926610, 7.230036912443287278, 0.7216878364870428220 ) ) ;
#181205 = CARTESIAN_POINT ( 'NONE',  ( 11.35610322553117157, 9.985783710708249217, -3.553412924323506861 ) ) ;
#181207 = CARTESIAN_POINT ( 'NONE',  ( 3.064699953192471682, -2.118106589925540906, -0.8768602481810504612 ) ) ;
#181210 = EDGE_CURVE ( 'NONE', #55379, #191858, #111002, .T. ) ;
#181209 = CARTESIAN_POINT ( 'NONE',  ( 0.2333690889706925009, 5.722554199285137422, -2.647406232470352894 ) ) ;
#181208 = CARTESIAN_POINT ( 'NONE',  ( -4.450244736157934256, 7.987476157872523963, 2.500000000000000444 ) ) ;
#181211 = CARTESIAN_POINT ( 'NONE',  ( 2.795058504854182946, -0.1448928079688660830, -1.906987441340234568 ) ) ;
#181212 = ORIENTED_EDGE ( 'NONE', *, *, #99318, .F. ) ;
#181213 = CARTESIAN_POINT ( 'NONE',  ( 7.470179451005385829, 8.777926116670192513, -1.082531754730537976 ) ) ;
#181214 = EDGE_CURVE ( 'NONE', #81693, #135497, #23054, .T. ) ;
#181215 = CARTESIAN_POINT ( 'NONE',  ( 0.8615886222705991804, -1.589730513765170938, -1.235154978249096036 ) ) ;
#181216 = CARTESIAN_POINT ( 'NONE',  ( 1.147228161472005681, 1.732707765124143817, -0.9198407203683529598 ) ) ;
#181217 = CARTESIAN_POINT ( 'NONE',  ( -9.657485491635913633, 10.16148791653038330, 1.040834085586084257E-14 ) ) ;
#181218 = CARTESIAN_POINT ( 'NONE',  ( -8.362681821530818738, 8.650883634741092010, -0.7998128361456291469 ) ) ;
#181219 = CARTESIAN_POINT ( 'NONE',  ( 1.642778471875001811, -0.4302083328553765740, 2.845375778867859751 ) ) ;
#181221 = CARTESIAN_POINT ( 'NONE',  ( 2.271989177565427287, -1.091335633969382490, 1.393213513506918133 ) ) ;
#181220 = CARTESIAN_POINT ( 'NONE',  ( 4.031257853796605062, -1.441737515256842572, -1.514218249133948868 ) ) ;
#181222 = DIRECTION ( 'NONE',  ( 0.000000000000000000, 0.000000000000000000, 1.000000000000000000 ) ) ;
#181224 = CARTESIAN_POINT ( 'NONE',  ( 5.507889418014947580, -1.026508118683837401, -2.049657838918368391 ) ) ;
#181223 = DIRECTION ( 'NONE',  ( 0.000000000000000000, 0.000000000000000000, 1.000000000000000000 ) ) ;
#181225 = CARTESIAN_POINT ( 'NONE',  ( 4.066134141799277124, -1.624876214689898957, -0.6237973674530649104 ) ) ;
#181226 = CARTESIAN_POINT ( 'NONE',  ( 9.565441069641300587, 11.11843498845840905, -1.199719254218440723 ) ) ;
#181227 =( NAMED_UNIT ( * ) PLANE_ANGLE_UNIT ( ) SI_UNIT ( $, .RADIAN. ) );
#181228 = CARTESIAN_POINT ( 'NONE',  ( 4.006995869149078793, 1.725434352394356052, 0.1705419362300845121 ) ) ;
#181229 = CARTESIAN_POINT ( 'NONE',  ( 4.475155579853315579, 1.983319414854123552, 0.8838481202026007288 ) ) ;
#181230 = CARTESIAN_POINT ( 'NONE',  ( 4.369805582306193870, 3.992528022312320957, 1.214306433183764966E-14 ) ) ;
#181231 = CARTESIAN_POINT ( 'NONE',  ( 5.208220363674559650, 1.197307938467083055, -1.622483861274232719 ) ) ;
#181232 = CARTESIAN_POINT ( 'NONE',  ( 0.8750000000000005551, 2.052068128417951609, -5.168192407616667353E-14 ) ) ;
#181233 = CARTESIAN_POINT ( 'NONE',  ( 0.7499999999999902300, 4.597916667349482012, -1.299038105676658228 ) ) ;
#181234 = CARTESIAN_POINT ( 'NONE',  ( 2.678635733147361808, -1.842946530311468045, -0.5607992601908852182 ) ) ;
#181235 = CARTESIAN_POINT ( 'NONE',  ( 0.7500000000000006661, 10.19791666734946922, -1.299038105676657340 ) ) ;
#181236 = CARTESIAN_POINT ( 'NONE',  ( 6.187741696929490054, 2.126074299989196614, -0.6436727651782292448 ) ) ;
#181237 = ORIENTED_EDGE ( 'NONE', *, *, #126637, .T. ) ;
#181238 = CARTESIAN_POINT ( 'NONE',  ( 6.983263157960404754, -0.005959781318053481922, 2.045923054782183392 ) ) ;
#181239 = CARTESIAN_POINT ( 'NONE',  ( -1.201851678989727383E-14, 3.212500000000018119, 1.732050807568877637 ) ) ;
#181240 = CARTESIAN_POINT ( 'NONE',  ( 6.287230548435207567, 8.358188277972981695, -1.599625672291262513 ) ) ;
#181241 = CARTESIAN_POINT ( 'NONE',  ( 1.788022372910631486, 2.124507586210178989, -0.6485351029156469771 ) ) ;
#181242 = CARTESIAN_POINT ( 'NONE',  ( 6.531700620877029628, 1.877769495358465157, -0.5682946464737672621 ) ) ;
#181243 = CARTESIAN_POINT ( 'NONE',  ( 9.259855728453651125, 9.905512559391842942, 1.040834085586084257E-14 ) ) ;
#181244 = CARTESIAN_POINT ( 'NONE',  ( 1.499999999999996891, 10.17708333401613174, -0.8660254037844378194 ) ) ;
#181245 = EDGE_CURVE ( 'NONE', #174590, #140877, #36130, .T. ) ;
#181246 = CIRCLE ( 'NONE', #115604, 0.08000000000000001554 ) ;
#181247 = CARTESIAN_POINT ( 'NONE',  ( 6.482206841109512396, 9.616306177052839743, -1.082531754730548412 ) ) ;
#181248 = CARTESIAN_POINT ( 'NONE',  ( -2.862179826260718762, 6.353310540697199471, 0.000000000000000000 ) ) ;
#181250 = CARTESIAN_POINT ( 'NONE',  ( 4.439923992641017669, 1.344862922493793578, 1.564070066283109295 ) ) ;
#181249 = CARTESIAN_POINT ( 'NONE',  ( 8.516493047678546091, 13.08765898893368629, -0.7998128361456352531 ) ) ;
#181251 = CARTESIAN_POINT ( 'NONE',  ( -4.497554271431319250, 6.270232621468402989, -1.599625672291256295 ) ) ;
#181252 =( NAMED_UNIT ( * ) SI_UNIT ( $, .STERADIAN. ) SOLID_ANGLE_UNIT ( ) );
#181253 = CARTESIAN_POINT ( 'NONE',  ( -0.6823417656250003738, -0.7822916663252423852, -1.181850606188749264 ) ) ;
#181254 = CARTESIAN_POINT ( 'NONE',  ( 5.641831084104285132, 0.7588036158820666843, -1.709917670604633066 ) ) ;
#181255 = CARTESIAN_POINT ( 'NONE',  ( 4.799290796133064418, 1.190976682166387413, -1.260762715536057899 ) ) ;
#181256 = CARTESIAN_POINT ( 'NONE',  ( 4.089206054525551970, -0.6613740077951230090, 1.610090703890323605 ) ) ;
#181257 = CARTESIAN_POINT ( 'NONE',  ( 4.955668840994886359, 5.740367388370866131, 1.199719254218462483 ) ) ;
#181258 = CARTESIAN_POINT ( 'NONE',  ( 2.103457651957148844, -0.4980181218575702173, 2.237485198869753944 ) ) ;
#181259 = CARTESIAN_POINT ( 'NONE',  ( -1.364683531250014514, -1.219791666325248602, 0.7879004041258379498 ) ) ;
#181260 = CARTESIAN_POINT ( 'NONE',  ( 6.005435553056907239, -2.074886976054179488, 0.2565860541952763585 ) ) ;
#181261 = CARTESIAN_POINT ( 'NONE',  ( 0.7086343398283838635, -0.2726298849291541870, 1.820711063333625646 ) ) ;
#181262 = CARTESIAN_POINT ( 'NONE',  ( 4.823331260782475205, 6.941738851361666462, 1.443736280540828032 ) ) ;
#181263 = SHAPE_REPRESENTATION_RELATIONSHIP ( 'NONE' , 'NONE' ,  #63688, #112039 ) ;
#181264 = CARTESIAN_POINT ( 'NONE',  ( 2.479138880926802901, -2.011204309026824344, -0.1455328587063598189 ) ) ;
#181265 = CARTESIAN_POINT ( 'NONE',  ( 1.236564921189796440, 0.4304113295856800692, 2.148598399174222351 ) ) ;
#181266 = CARTESIAN_POINT ( 'NONE',  ( 6.978933388731730858, 14.99484663357710801, -9.366624288252014097 ) ) ;
#181267 = CARTESIAN_POINT ( 'NONE',  ( -7.283754839039664475, 9.520799950344851936, -1.599625672291263179 ) ) ;
#181268 = CARTESIAN_POINT ( 'NONE',  ( 1.451716722110554025, 1.566445173006292935, 1.353826630019476562 ) ) ;
#181269 = CARTESIAN_POINT ( 'NONE',  ( 6.030679399980265920, 5.930214142932100252, -0.7998128361456281477 ) ) ;
#181270 = CARTESIAN_POINT ( 'NONE',  ( -0.6801582343750282034, 2.682291667008049441, 1.178068619123805227 ) ) ;
#181271 = CARTESIAN_POINT ( 'NONE',  ( 3.088655771522513582, -1.261447869382603004, 1.704333039148818507 ) ) ;
#181272 = CARTESIAN_POINT ( 'NONE',  ( -1.364683531250000748, -0.7406249996585803075, 0.000000000000000000 ) ) ;
#181273 = CARTESIAN_POINT ( 'NONE',  ( 0.3637320452541660254, 1.905723972499345997, -0.2814332051396683521 ) ) ;
#181274 = EDGE_LOOP ( 'NONE', ( #99907, #57387, #136567, #55684 ) ) ;
#181275 = CARTESIAN_POINT ( 'NONE',  ( -5.550083779947821760, 7.568460058062819407, -1.599625672291271394 ) ) ;
#181276 = CARTESIAN_POINT ( 'NONE',  ( 10.07100917685271035, 10.64393221595000938, 0.7998128361456462443 ) ) ;
#181277 = CARTESIAN_POINT ( 'NONE',  ( 6.007671464186825183, 8.102312356341712984, 1.443375672974064550 ) ) ;
#181278 = CARTESIAN_POINT ( 'NONE',  ( 3.475000000000000533, -2.231249999044084831, 0.000000000000000000 ) ) ;
#181279 = CARTESIAN_POINT ( 'NONE',  ( -4.557512192488103686, 8.468847991211438497, -0.7998128361456281477 ) ) ;
#181280 = CARTESIAN_POINT ( 'NONE',  ( 3.638929714444568919, 1.919204589499112323, 0.6297368113697666692 ) ) ;
#181281 = CARTESIAN_POINT ( 'NONE',  ( 6.563508857876433567, 0.3837567690821128696, -2.173003994120882076 ) ) ;
#181282 = CARTESIAN_POINT ( 'NONE',  ( -5.498713818794216834, 8.572860667638675380, -1.199719254218452047 ) ) ;
#181283 = CARTESIAN_POINT ( 'NONE',  ( 8.239604668803105270, 10.63595808506888396, -1.599625672291268286 ) ) ;
#181284 = CARTESIAN_POINT ( 'NONE',  ( 5.137489257405690957, 1.737274493258118113, -0.6675986409061424043 ) ) ;
#181285 = CARTESIAN_POINT ( 'NONE',  ( 7.995557903757111617, 10.35123685918189729, 1.599625672291281386 ) ) ;
#181286 = CARTESIAN_POINT ( 'NONE',  ( 11.78331023100045627, 13.79999999999999893, -1.800000000000001155 ) ) ;
#181287 = CARTESIAN_POINT ( 'NONE',  ( -3.846762897975357198, 5.510976019103107859, -1.599625672291256295 ) ) ;
#181288 = CARTESIAN_POINT ( 'NONE',  ( -5.845536785786364931, 9.971543350059432598, 0.000000000000000000 ) ) ;
#181289 = CARTESIAN_POINT ( 'NONE',  ( 6.702032673877901914, -2.060500267551836018, 0.04777910199381221051 ) ) ;
#181290 = ADVANCED_FACE ( 'NONE', ( #162300 ), #58891, .T. ) ;
#181292 = CARTESIAN_POINT ( 'NONE',  ( -4.956836104118029773, 6.830226236571708576, 1.450618959550575182 ) ) ;
#181291 = CARTESIAN_POINT ( 'NONE',  ( -6.882699257592852504, 8.058845884393651460, -1.199719254218452047 ) ) ;
#181293 = CARTESIAN_POINT ( 'NONE',  ( -1.364683531250000748, 1.009375000341421247, 0.000000000000000000 ) ) ;
#181294 = CARTESIAN_POINT ( 'NONE',  ( 1.299655142190193402, -1.570548766235444038, 0.7348691985549455907 ) ) ;
#181295 = CARTESIAN_POINT ( 'NONE',  ( 0.8842106040080777163, 1.536738824236941747, -0.8168212061390681678 ) ) ;
#181297 = CARTESIAN_POINT ( 'NONE',  ( 6.426201623197458801, 9.480690412830290015, -1.082531754730537088 ) ) ;
#181296 = CARTESIAN_POINT ( 'NONE',  ( 6.217413992247779575, -0.2892589651934658890, 2.289433544902704565 ) ) ;
#181298 = CARTESIAN_POINT ( 'NONE',  ( -11.37872555039425748, 6.127336012342636806, -3.407788289652350588 ) ) ;
#181299 = CARTESIAN_POINT ( 'NONE',  ( 2.899741356312244722, -0.6498117751948685461, 1.955694574617524495 ) ) ;
#181300 = CARTESIAN_POINT ( 'NONE',  ( 3.994848817520957773, 7.812407387083109001, 1.040834085586084257E-14 ) ) ;
#181301 = CARTESIAN_POINT ( 'NONE',  ( 1.071638489536786309, 1.528508772698907059, -1.314793605459969372 ) ) ;
#181302 = CARTESIAN_POINT ( 'NONE',  ( 9.168541482314250146, 14.15586233142781758, -7.671659664418466917 ) ) ;
#181304 = AXIS2_PLACEMENT_3D ( 'NONE', #6481, #174364, #124614 ) ;
#181303 = CARTESIAN_POINT ( 'NONE',  ( -4.827585214917754719, 7.789877296449459365, -1.199719254218453823 ) ) ;
#181305 = CARTESIAN_POINT ( 'NONE',  ( 6.772336237553374438, -1.148929780121176414, 1.476827877338216854 ) ) ;
#181306 = CIRCLE ( 'NONE', #105271, 0.08000000000000040412 ) ;
#181308 = CARTESIAN_POINT ( 'NONE',  ( -7.268579750702168774, 7.652633595340216921, -0.7216878364870338292 ) ) ;
#181307 = CARTESIAN_POINT ( 'NONE',  ( 5.133030909251353968, 1.769313487831367659, 0.7262901588861517821 ) ) ;
#181309 = CARTESIAN_POINT ( 'NONE',  ( 5.672569038193632451, -1.402732290180560337, 1.703733612381942653 ) ) ;
#181310 = CARTESIAN_POINT ( 'NONE',  ( -6.821160681006823268, 9.051383109298335228, 1.443375672974064550 ) ) ;
#181311 = CARTESIAN_POINT ( 'NONE',  ( 6.003228155800906407, 10.22579295840155744, 0.000000000000000000 ) ) ;
#181312 = CARTESIAN_POINT ( 'NONE',  ( -5.302647476276252547, 5.359045941843285199, 0.7216878364870257245 ) ) ;
#181313 = CARTESIAN_POINT ( 'NONE',  ( 6.586587867412674768, -1.305319418013479948, 1.671791285998667442 ) ) ;
#181314 = CARTESIAN_POINT ( 'NONE',  ( -1.040834085586084257E-14, -7.246166700194011767, -9.579665964935651701 ) ) ;
#181315 = CARTESIAN_POINT ( 'NONE',  ( 4.436755630409714435, 2.262211819008316027, 0.4546042144240244887 ) ) ;
#181316 = CARTESIAN_POINT ( 'NONE',  ( 4.527759979645433752, 1.903474890065796732, -0.4746247275292309609 ) ) ;
#181317 = EDGE_CURVE ( 'NONE', #107434, #90309, #171111, .T. ) ;
#181318 = CARTESIAN_POINT ( 'NONE',  ( 2.184356868638567928, 1.133688150830698627, -1.600809071968431807 ) ) ;
#181319 = CARTESIAN_POINT ( 'NONE',  ( 8.387690588348714726, 12.93738945304888333, 1.040834085586084257E-14 ) ) ;
#181320 = CARTESIAN_POINT ( 'NONE',  ( -9.490193176586279478, 14.79883486810179427, 7.238303200480997290 ) ) ;
#181321 = EDGE_LOOP ( 'NONE', ( #122916, #65086, #13734, #195640 ) ) ;
#181322 = CARTESIAN_POINT ( 'NONE',  ( 6.503150282362620160, -0.1410805869419759218, 1.984311032119711715 ) ) ;
#181324 = CARTESIAN_POINT ( 'NONE',  ( -7.147119532698295252, 11.49005655479003174, 0.000000000000000000 ) ) ;
#181323 = CARTESIAN_POINT ( 'NONE',  ( -4.894657149733403045, 5.669187081899118574, -1.199719254218446718 ) ) ;
#181325 = CARTESIAN_POINT ( 'NONE',  ( 0.7437973067255730930, 0.5320827018340993364, 1.762565881533173950 ) ) ;
#181326 = ORIENTED_EDGE ( 'NONE', *, *, #192671, .T. ) ;
#181327 = CARTESIAN_POINT ( 'NONE',  ( 4.803694799390169301, -1.674174935400191799, -1.382237342716886586 ) ) ;
#181328 = B_SPLINE_CURVE_WITH_KNOTS ( 'NONE', 3,
 ( #26626, #205365, #56999, #157719, #22331, #122089, #156648 ),
 .UNSPECIFIED., .F., .F.,
 ( 4, 3, 4 ),
 ( 0.000000000000000000, 2.778001202718471385E-05, 5.460790091229278642E-05 ),
 .UNSPECIFIED. ) ;
#181329 = CARTESIAN_POINT ( 'NONE',  ( 1.740644586495963431, 1.216819214799185866, -1.736574482785017359 ) ) ;
#181330 = CARTESIAN_POINT ( 'NONE',  ( 1.499999999999987121, 3.577083334016152527, -0.8660254037844262731 ) ) ;
#181331 = CARTESIAN_POINT ( 'NONE',  ( 8.076906825439115423, 10.44614393447756129, -1.599625672291262513 ) ) ;
#181332 = CARTESIAN_POINT ( 'NONE',  ( -1.870624324079490863, 2.481157652721496021, -2.472014912841812961 ) ) ;
#181333 = CARTESIAN_POINT ( 'NONE',  ( 6.225987253121650689, 7.022442755726078900, -1.008712875586889712 ) ) ;
#181334 = CARTESIAN_POINT ( 'NONE',  ( 1.563821040897996895, 2.030780823367520416, -0.3493207144565529942 ) ) ;
#181336 = CARTESIAN_POINT ( 'NONE',  ( 6.609000000000009756, 0.005669918681722525139, 1.900160851458797318 ) ) ;
#181335 = CARTESIAN_POINT ( 'NONE',  ( -9.677822722056413696, 10.18521468535430685, 1.040834085586084257E-14 ) ) ;
#181337 = CARTESIAN_POINT ( 'NONE',  ( 0.6823417656249899377, 3.926041667008085767, -1.181850606188754593 ) ) ;
#181338 = CARTESIAN_POINT ( 'NONE',  ( 0.07735805125223899070, 0.2300150639059690694, -2.122327182112139443 ) ) ;
#181339 = CARTESIAN_POINT ( 'NONE',  ( -3.289951133708679087, 7.658661826346113699, 2.499999999999998668 ) ) ;
#181340 = CARTESIAN_POINT ( 'NONE',  ( 6.182274467271689389, 0.9872068455926674702, 1.637624497839342830 ) ) ;
#181341 = CARTESIAN_POINT ( 'NONE',  ( 11.84103413958613160, 12.48995521526856578, -1.443924719788771682 ) ) ;
#181342 = CARTESIAN_POINT ( 'NONE',  ( 1.792605694782311243, -2.251445656634944559, -0.2226877779667023882 ) ) ;
#181343 = CARTESIAN_POINT ( 'NONE',  ( -8.948018195339354719, 12.42280974699582607, 1.082531754730560403 ) ) ;
#181344 = CARTESIAN_POINT ( 'NONE',  ( 1.089788312850032526, 1.080336570596603929, 1.454002670061284919 ) ) ;
#181345 = CARTESIAN_POINT ( 'NONE',  ( 1.903404652330241476, -1.857121539659777998, 0.4695605108672970540 ) ) ;
#181346 = CARTESIAN_POINT ( 'NONE',  ( 3.385274849524767316, 0.04804411014160993310, 2.069964801482151895 ) ) ;
#181347 = CARTESIAN_POINT ( 'NONE',  ( 0.6823417656249899377, 1.905208333674752952, 1.181850606188755259 ) ) ;
#181348 = ADVANCED_FACE ( 'NONE', ( #195399 ), #178093, .F. ) ;
#181349 = CARTESIAN_POINT ( 'NONE',  ( 1.076956826339631856, -0.04624765943369788662, -1.971079714834519159 ) ) ;
#181350 = CARTESIAN_POINT ( 'NONE',  ( 5.092375307706883625, -1.912163826771107855, -0.2340926620403842862 ) ) ;
#181352 = CARTESIAN_POINT ( 'NONE',  ( 6.321627859881460587, 6.858947107989728842, -0.6823232096292205506 ) ) ;
#181351 = CARTESIAN_POINT ( 'NONE',  ( 1.032322977361863847, -1.467698275133515695, -1.780829215104979157 ) ) ;
#181353 = CARTESIAN_POINT ( 'NONE',  ( -1.364683531250014514, 0.9885416670080898749, -0.7879004041258289570 ) ) ;
#181354 = CARTESIAN_POINT ( 'NONE',  ( 5.547355216851989290, 1.820699215414087302, -0.9693467284541881224 ) ) ;
#181355 = CARTESIAN_POINT ( 'NONE',  ( -4.713430959045263435, 8.650753218861462202, 0.7998128361456481317 ) ) ;
#181356 = CARTESIAN_POINT ( 'NONE',  ( 7.962716289927667113, 8.184257181204083409, -0.7998128361456291469 ) ) ;
#181357 = CARTESIAN_POINT ( 'NONE',  ( -1.270916165646622353, 2.915225491120026824, 0.7750000000000152323 ) ) ;
#181358 =( BOUNDED_CURVE ( )  B_SPLINE_CURVE ( 2, ( #200388, #187354, #105069, #85589, #34702, #53090, #171107, #83454, #70379 ),
 .UNSPECIFIED., .F., .T. ) 
 B_SPLINE_CURVE_WITH_KNOTS ( ( 3, 2, 2, 2, 3 ),
 ( 0.2708333333333333703, 0.2777777777777777901, 0.2916666666666666852, 0.3055555555555555802, 0.3125000000000000000 ),
 .UNSPECIFIED. ) 
 CURVE ( )  GEOMETRIC_REPRESENTATION_ITEM ( )  RATIONAL_B_SPLINE_CURVE ( ( 0.9330127018922194093, 0.9330127018922196314, 1.000000000000000000, 0.8660254037844387076, 1.000000000000000000, 0.8660254037844387076, 1.000000000000000000, 0.9330127018922194093, 0.9330127018922194093 ) ) 
 REPRESENTATION_ITEM ( '' )  );
#181361 = CARTESIAN_POINT ( 'NONE',  ( -0.7500000000000215383, 5.191666666666685082, 1.299038105676671107 ) ) ;
#181360 = CARTESIAN_POINT ( 'NONE',  ( 6.440466061264603859, 2.082495663875443714, 0.3126870252899079938 ) ) ;
#181359 = CIRCLE ( 'NONE', #11892, 2.725000000000000089 ) ;
#181362 = CARTESIAN_POINT ( 'NONE',  ( -1.364683531249997417, 2.821875000341422801, 1.214306433183764966E-14 ) ) ;
#181363 = CARTESIAN_POINT ( 'NONE',  ( 4.464260128311710041, 1.014592192358022338, 1.908665273222116321 ) ) ;
#181364 = CARTESIAN_POINT ( 'NONE',  ( 5.285809349500922849, 1.945818207184028426, -0.5408622128197750900 ) ) ;
#181365 = DIRECTION ( 'NONE',  ( 0.7592566023653004592, -0.6507913734559641616, -1.725633230170963105E-31 ) ) ;
#181366 = CARTESIAN_POINT ( 'NONE',  ( -5.910991785878183080, 5.998504626387068051, -0.7216878364870278340 ) ) ;
#181367 = AXIS2_PLACEMENT_3D ( 'NONE', #209629, #145767, #130614 ) ;
#181368 = ADVANCED_FACE ( 'NONE', ( #210562, #12353, #128353, #66417 ), #95783, .T. ) ;
#181371 = CARTESIAN_POINT ( 'NONE',  ( 3.877268743828258479, 7.467304601200877023, 0.7216878364870298324 ) ) ;
#181370 = CARTESIAN_POINT ( 'NONE',  ( 1.001543065824772753E-15, -1.771874999522040861, 3.793834371823811669 ) ) ;
#181369 = CARTESIAN_POINT ( 'NONE',  ( 6.933015448541703485, 9.181880338089085214, 1.599625672291268286 ) ) ;
#181372 = CARTESIAN_POINT ( 'NONE',  ( -6.317173229324657413, 6.334733287159020954, 0.000000000000000000 ) ) ;
#181373 = CARTESIAN_POINT ( 'NONE',  ( 3.608611488583326032, 1.916353073142588403, 0.6279913346786819561 ) ) ;
#181374 = CARTESIAN_POINT ( 'NONE',  ( -7.018317073368468328, 11.33978701890523233, -0.7998128361456291469 ) ) ;
#181376 = CARTESIAN_POINT ( 'NONE',  ( -10.99431798667095883, -5.199791778945004772, 0.3617173305618339163 ) ) ;
#181375 = CARTESIAN_POINT ( 'NONE',  ( -4.790108344329849110, 4.482881244673243337, 0.7998128361456341429 ) ) ;
#181377 = CARTESIAN_POINT ( 'NONE',  ( -0.6823417656249969321, 4.717708333674755394, -1.181850606188749264 ) ) ;
#181379 = CARTESIAN_POINT ( 'NONE',  ( 0.6823417656249969321, 9.776041667008065872, -1.181850606188757036 ) ) ;
#181378 = CARTESIAN_POINT ( 'NONE',  ( 4.575171270262055501, 0.003154952768896768234, -2.161883445794945846 ) ) ;
#181380 = LINE ( 'NONE', #198676, #127991 ) ;
#181381 = CARTESIAN_POINT ( 'NONE',  ( -11.95500993068053930, 8.101295389535254188, -0.2609214463033582843 ) ) ;
#181383 = CARTESIAN_POINT ( 'NONE',  ( 5.993767587909683670, -2.000856116866961187, 0.2496242821527286382 ) ) ;
#181382 = CARTESIAN_POINT ( 'NONE',  ( -6.358410854684783509, 9.401601182898824405, -1.082531754730537976 ) ) ;
#181384 = CARTESIAN_POINT ( 'NONE',  ( -1.364683531250000748, -0.1781249996585798634, 0.000000000000000000 ) ) ;
#181385 = CARTESIAN_POINT ( 'NONE',  ( 0.3281590906380106865, 1.648959081962350304, 0.5061492587876709193 ) ) ;
#181386 = CARTESIAN_POINT ( 'NONE',  ( 4.061549535745618833, 6.896169004081968090, -1.199719254218452047 ) ) ;
#181388 = CARTESIAN_POINT ( 'NONE',  ( 6.749980374757213575, 8.968339418673846097, 1.599625672291268286 ) ) ;
#181387 = CARTESIAN_POINT ( 'NONE',  ( 8.107412671292042461, 9.521364873671299023, 1.082531754730558626 ) ) ;
#181389 = CARTESIAN_POINT ( 'NONE',  ( -11.98824733424307709, 9.000663626117129112, 0.6135287215046117959 ) ) ;
#181390 = CARTESIAN_POINT ( 'NONE',  ( 6.397708313642382905, -0.6301307688901837123, 1.761319926792910495 ) ) ;
#181391 = CARTESIAN_POINT ( 'NONE',  ( 0.6451818603588607148, 0.1503996631540445994, 2.007543313942860674 ) ) ;
#181392 = CARTESIAN_POINT ( 'NONE',  ( 6.539320575229279342, 7.629137130509070275, 2.496737603865983868 ) ) ;
#181393 = CARTESIAN_POINT ( 'NONE',  ( 3.153566124713353513, -1.803153744294363481, -1.271922660818012973 ) ) ;
#181394 = CARTESIAN_POINT ( 'NONE',  ( -5.587368702163209910, 9.532697562583475559, 0.000000000000000000 ) ) ;
#181395 = ORIENTED_EDGE ( 'NONE', *, *, #12700, .T. ) ;
#181396 = CARTESIAN_POINT ( 'NONE',  ( 9.707274797260268429, 10.42750147299956964, 0.000000000000000000 ) ) ;
#181398 = CARTESIAN_POINT ( 'NONE',  ( 1.493767781312784981, -2.000855510370867840, 0.2496291452861176263 ) ) ;
#181397 = CARTESIAN_POINT ( 'NONE',  ( 2.192179715818479036, 1.306768369893403170, 1.669877806752372740 ) ) ;
#181399 = CARTESIAN_POINT ( 'NONE',  ( 2.302729407678519191, -0.3129977310964130455, -1.784170229015415332 ) ) ;
#181400 = CARTESIAN_POINT ( 'NONE',  ( 6.556249800660121529, 9.806652646482286073, 1.199719254218452047 ) ) ;
#181401 = ORIENTED_EDGE ( 'NONE', *, *, #30090, .F. ) ;
#181402 = CARTESIAN_POINT ( 'NONE',  ( 6.908042961362778733, 8.018137195466769285, 1.199719254218462483 ) ) ;
#181404 = CARTESIAN_POINT ( 'NONE',  ( 0.4267777427376097665, -1.641576225293687630, 0.9873106011929821957 ) ) ;
#181403 = CARTESIAN_POINT ( 'NONE',  ( -6.552668314106420588, 6.539201209412602189, -0.7998128361456291469 ) ) ;
#181405 = CYLINDRICAL_SURFACE ( 'NONE', #208092, 0.3999999999999997446 ) ;
#181406 = CARTESIAN_POINT ( 'NONE',  ( 5.843201017365476702, 6.879784610756938257, -1.082531754730543083 ) ) ;
#181407 = CARTESIAN_POINT ( 'NONE',  ( 1.364683531249986537, -0.2822916663252520997, -0.7879004041258309554 ) ) ;
#181408 = CARTESIAN_POINT ( 'NONE',  ( 0.000000000000000000, 0.000000000000000000, 0.000000000000000000 ) ) ;
#181409 = CARTESIAN_POINT ( 'NONE',  ( -8.809047120577080392, 11.30030761213851953, 1.599625672291269396 ) ) ;
#181410 = CARTESIAN_POINT ( 'NONE',  ( 3.942369626403975147, 2.151062187213080623, 0.2142938780915065733 ) ) ;
#181411 = CARTESIAN_POINT ( 'NONE',  ( -7.105881907338178038, 7.462819444748888920, -0.7216878364870338292 ) ) ;
#181412 = CARTESIAN_POINT ( 'NONE',  ( 4.245111494854632461, 7.966730820723463502, 0.000000000000000000 ) ) ;
#181413 = CARTESIAN_POINT ( 'NONE',  ( 2.478903650112133317, -1.459102030866548994, 1.539066919819010781 ) ) ;
#181414 = ADVANCED_FACE ( 'NONE', ( #80572 ), #81019, .T. ) ;
#181415 = CARTESIAN_POINT ( 'NONE',  ( 3.637922374042131590, 0.8895205046622333134, -1.759358583061757519 ) ) ;
#181416 = VERTEX_POINT ( 'NONE', #29702 ) ;
#181417 = CARTESIAN_POINT ( 'NONE',  ( 5.635196759804959044, -0.04649108105550652653, -1.969165932527061402 ) ) ;
#181418 = CARTESIAN_POINT ( 'NONE',  ( 1.710778446297245958, -0.2380136870633246249, 1.927241887951787858 ) ) ;
#181419 = ORIENTED_EDGE ( 'NONE', *, *, #124309, .F. ) ;
#181420 = CARTESIAN_POINT ( 'NONE',  ( -5.320648938720212051, 5.172121614787156929, 0.000000000000000000 ) ) ;
#181422 = CARTESIAN_POINT ( 'NONE',  ( 0.4630894006623479942, -6.442483420144672124, 11.24798772015295789 ) ) ;
#181421 = CARTESIAN_POINT ( 'NONE',  ( -5.302647476720585118, 9.200522799567075083, 0.000000000000000000 ) ) ;
#181424 = CARTESIAN_POINT ( 'NONE',  ( 6.958359152311676787, 9.141171649162195934, -1.599625672291262513 ) ) ;
#181423 = CARTESIAN_POINT ( 'NONE',  ( 2.871125768194443761, 1.984923283205226818, -0.6565763796619171755 ) ) ;
#181426 = CARTESIAN_POINT ( 'NONE',  ( 5.682275777458854371, 5.801945626556378244, 0.7216878364870328300 ) ) ;
#181425 = CARTESIAN_POINT ( 'NONE',  ( 6.714312387265682247, 8.856450423275211037, 1.599625672291281386 ) ) ;
#181428 = ORIENTED_EDGE ( 'NONE', *, *, #182631, .F. ) ;
#181427 = CARTESIAN_POINT ( 'NONE',  ( 6.164708882046985750, 0.6044385376218417427, 1.814302210532907411 ) ) ;
#181429 = CARTESIAN_POINT ( 'NONE',  ( 4.125739685719872263, -2.112183141943014153, 0.6395159525410462065 ) ) ;
#181430 = CARTESIAN_POINT ( 'NONE',  ( 1.817678338065799926, -0.2697497798337232244, 2.190168480848574628 ) ) ;
#181431 = CARTESIAN_POINT ( 'NONE',  ( 1.270994156678442596E-16, -6.530144695498194096, -11.00000000000000178 ) ) ;
#181432 = CARTESIAN_POINT ( 'NONE',  ( 1.172351427048579531, 0.7757545017167380985, 1.748050575570128329 ) ) ;
#181433 =( BOUNDED_CURVE ( )  B_SPLINE_CURVE ( 2, ( #41583, #156389, #204022, #27437, #7975, #93535, #74063 ),
 .UNSPECIFIED., .F., .T. ) 
 B_SPLINE_CURVE_WITH_KNOTS ( ( 3, 2, 2, 3 ),
 ( 0.1625000000000002276, 0.1666666666666669072, 0.1708333333333336146, 0.1750000000000002942 ),
 .UNSPECIFIED. ) 
 CURVE ( )  GEOMETRIC_REPRESENTATION_ITEM ( )  RATIONAL_B_SPLINE_CURVE ( ( 0.9999999999999928946, 0.8660254037844458130, 1.000000000000000000, 0.8660254037844387076, 1.000000000000000000, 0.8660254037844289376, 1.000000000000009770 ) ) 
 REPRESENTATION_ITEM ( '' )  );
#181434 = DIRECTION ( 'NONE',  ( 2.949029909160572061E-17, 1.000000000000000000, -8.673600428462429131E-15 ) ) ;
#181435 = DIRECTION ( 'NONE',  ( 0.000000000000000000, 1.000000000000000000, 0.000000000000000000 ) ) ;
#181436 = CARTESIAN_POINT ( 'NONE',  ( 3.930184216435282707, 1.147649575447948100, 1.722966636330313328 ) ) ;
#181437 = CARTESIAN_POINT ( 'NONE',  ( -6.437424008390261854, 6.404749519410410485, 0.7998128361456341429 ) ) ;
#181439 = CARTESIAN_POINT ( 'NONE',  ( 2.131903390035182255, -1.411712784473453830, -1.637176306262012826 ) ) ;
#181438 = DIRECTION ( 'NONE',  ( 0.000000000000000000, 1.000000000000000000, 0.000000000000000000 ) ) ;
#181440 = CARTESIAN_POINT ( 'NONE',  ( 3.825867475279482566, 1.171244075711602051, -1.852137614134836907 ) ) ;
#181441 = FACE_OUTER_BOUND ( 'NONE', #76365, .T. ) ;
#181442 =( LENGTH_UNIT ( ) NAMED_UNIT ( * ) SI_UNIT ( .MILLI., .METRE. ) );
#181443 = CARTESIAN_POINT ( 'NONE',  ( 0.7500000000000006661, 12.83333333333333570, 1.299038105676657340 ) ) ;
#181444 = CARTESIAN_POINT ( 'NONE',  ( -1.364683531250014514, 14.90104166700806410, -0.7879004041258335089 ) ) ;
#181445 = CARTESIAN_POINT ( 'NONE',  ( -5.829079699232685208, 5.765290835385048496, 0.000000000000000000 ) ) ;
#181447 = CARTESIAN_POINT ( 'NONE',  ( 5.871638708485903635, -0.2633594344273459398, -1.713904792762838136 ) ) ;
#181446 = VECTOR ( 'NONE', #111750, 1000.000000000000000 ) ;
#181448 = CARTESIAN_POINT ( 'NONE',  ( -9.978437869977959451, 10.74385839117019614, -0.7216878364870267237 ) ) ;
#181449 = CARTESIAN_POINT ( 'NONE',  ( 4.856339096887199780, -2.069677458173447171, -0.05615216265978521804 ) ) ;
#181450 = CARTESIAN_POINT ( 'NONE',  ( 5.677400705446850715, 1.603760038662904286, 1.382376383168891998 ) ) ;
#181451 = AXIS2_PLACEMENT_3D ( 'NONE', #84727, #19719, #105269 ) ;
#181452 = CARTESIAN_POINT ( 'NONE',  ( 6.043183783389218355, 8.073467052085995022, 1.599625672291267398 ) ) ;
#181453 = CARTESIAN_POINT ( 'NONE',  ( 9.622977958535759768, 4.242291508015313184, 7.169920593678671850 ) ) ;
#181454 = CARTESIAN_POINT ( 'NONE',  ( 4.047672669870348905, 1.423397643995693684, 1.361350234347382226 ) ) ;
#181455 = CARTESIAN_POINT ( 'NONE',  ( 5.595737365542901465, -2.292435212557204949, -0.004933362929348399616 ) ) ;
#181457 = EDGE_CURVE ( 'NONE', #160336, #213592, #50070, .T. ) ;
#181456 = CARTESIAN_POINT ( 'NONE',  ( 3.334410585898534674, 1.781380905032422746, 0.3990451814587444024 ) ) ;
#181458 = CARTESIAN_POINT ( 'NONE',  ( 3.715816618597135523, 6.492813934075403637, -1.199719254218453823 ) ) ;
#181459 = CARTESIAN_POINT ( 'NONE',  ( 3.782361668088245921, 6.396210465202840645, -1.082531754730548412 ) ) ;
#181460 = CARTESIAN_POINT ( 'NONE',  ( -5.520141099058386125, 9.591915048876776595, 0.000000000000000000 ) ) ;
#181461 = CARTESIAN_POINT ( 'NONE',  ( 4.369470645354133431, 8.319742529546998000, 0.7998128361456271485 ) ) ;
#181462 = ORIENTED_EDGE ( 'NONE', *, *, #108010, .F. ) ;
#181463 = CARTESIAN_POINT ( 'NONE',  ( 3.691655806294301900, 1.894216563707728396, -0.6821535943304660732 ) ) ;
#181464 = AXIS2_PLACEMENT_3D ( 'NONE', #44293, #110415, #176418 ) ;
#181465 = CARTESIAN_POINT ( 'NONE',  ( 4.803538753074391821, -1.513872852549098091, -1.247617340562396926 ) ) ;
#181466 = CARTESIAN_POINT ( 'NONE',  ( -5.910464900553636269, 8.982960586366182554, -1.199719254218440723 ) ) ;
#181467 = CARTESIAN_POINT ( 'NONE',  ( -4.599240423533815125, 6.388866465587984322, 1.599625672291267398 ) ) ;
#181468 = EDGE_CURVE ( 'NONE', #198620, #101986, #205733, .T. ) ;
#181470 = CARTESIAN_POINT ( 'NONE',  ( 5.594547536969180612, -0.4332151766474266474, -1.715878325482506517 ) ) ;
#181469 = CARTESIAN_POINT ( 'NONE',  ( 0.1872078708128835645, 1.551958633911882934, 1.401156373025253421 ) ) ;
#181471 = LINE ( 'NONE', #33101, #136847 ) ;
#181472 = CARTESIAN_POINT ( 'NONE',  ( 1.465048628566959055, 0.1585425061045864503, -2.185770122351132994 ) ) ;
#181473 = CARTESIAN_POINT ( 'NONE',  ( 1.047962540061377679, -1.372746097444921043, 1.069743175550162295 ) ) ;
#181474 = CARTESIAN_POINT ( 'NONE',  ( 5.341022448779654930, 8.318611059296550536, 1.199719254218462483 ) ) ;
#181475 = CARTESIAN_POINT ( 'NONE',  ( 0.1335669894368292088, 2.005130876877735613, -2.568368839946821414 ) ) ;
#181476 = CARTESIAN_POINT ( 'NONE',  ( 1.207153632009206223, -0.4226329412084055548, 1.672169654609439116 ) ) ;
#181477 = CARTESIAN_POINT ( 'NONE',  ( 2.085717061910817183, -0.9337068281064246911, 1.982830571388309204 ) ) ;
#181478 = CARTESIAN_POINT ( 'NONE',  ( 3.334799921508072806, 2.153101868192684343, 0.4835390122766567433 ) ) ;
#181479 = CARTESIAN_POINT ( 'NONE',  ( 1.622189073652591240, 2.139406107190901185, -0.3685050674664645531 ) ) ;
#181480 = CARTESIAN_POINT ( 'NONE',  ( 0.1174333910212103232, -1.791171220025630895, 0.3524246893974944395 ) ) ;
#181481 = CARTESIAN_POINT ( 'NONE',  ( 1.956417434996825522, -1.298217783395636316, 1.672616391537498526 ) ) ;
#181482 = AXIS2_PLACEMENT_3D ( 'NONE', #205407, #26668, #92772 ) ;
#181483 = CARTESIAN_POINT ( 'NONE',  ( 6.661184042391356641, -7.215568602681155852, -6.773376348128788749 ) ) ;
#181484 = CARTESIAN_POINT ( 'NONE',  ( 6.036148348713140876, 0.9492135318787934262, -1.676240969703364891 ) ) ;
#181485 = ORIENTED_EDGE ( 'NONE', *, *, #102016, .T. ) ;
#181487 = CARTESIAN_POINT ( 'NONE',  ( 1.364683531249988757, 0.1968750003414204697, 0.000000000000000000 ) ) ;
#181486 = CARTESIAN_POINT ( 'NONE',  ( 2.841680536636710386, 0.8224841172943345713, -2.139919992735066945 ) ) ;
#181488 = PLANE ( 'NONE',  #26217 ) ;
#181489 = CARTESIAN_POINT ( 'NONE',  ( 6.179819089730593795, 6.104210447640811665, 1.040834085586084257E-14 ) ) ;
#181490 = CARTESIAN_POINT ( 'NONE',  ( 5.268325480127796112, 2.218825861875061811, -0.1076023827350883894 ) ) ;
#181491 = CARTESIAN_POINT ( 'NONE',  ( -8.080296364064746939, 9.489729181906076505, 1.082531754730558626 ) ) ;
#181492 = CYLINDRICAL_SURFACE ( 'NONE', #66626, 0.08000000000000020983 ) ;
#181493 = CARTESIAN_POINT ( 'NONE',  ( 5.355107487717867265, 5.349972945200037522, 1.040834085586084257E-14 ) ) ;
#181494 = CARTESIAN_POINT ( 'NONE',  ( -7.849807752188049825, 8.260456587081938196, 0.7216878364870578100 ) ) ;
#181495 = EDGE_CURVE ( 'NONE', #153986, #81793, #145623, .T. ) ;
#181496 = CARTESIAN_POINT ( 'NONE',  ( 4.095971805104285934, 6.832365301713403838, 1.082531754730549078 ) ) ;
#181497 = EDGE_LOOP ( 'NONE', ( #66819, #159117, #33799 ) ) ;
#181498 = CARTESIAN_POINT ( 'NONE',  ( 2.830704105008190030, 0.7231396562890278767, -1.882474209725725434 ) ) ;
#181500 = CARTESIAN_POINT ( 'NONE',  ( 0.9540547974491294658, -0.7459001080754708024, 1.923128640884926410 ) ) ;
#181499 = CARTESIAN_POINT ( 'NONE',  ( 7.772902139336337335, 7.962807338847539107, 0.7998128361456341429 ) ) ;
#181501 = CARTESIAN_POINT ( 'NONE',  ( 4.588505019226127857, 4.929507493212790692, 0.7728389572207298164 ) ) ;
#181502 = CARTESIAN_POINT ( 'NONE',  ( 4.204437033569277560, 7.919277282557212416, 0.000000000000000000 ) ) ;
#181503 = CARTESIAN_POINT ( 'NONE',  ( 0.6823417656249917140, 3.842708333674754506, 1.181850606188765695 ) ) ;
#181504 = CARTESIAN_POINT ( 'NONE',  ( 3.943468035136340255, 0.7389761752502190806, -2.063229655756371628 ) ) ;
#181505 = CARTESIAN_POINT ( 'NONE',  ( 1.143204175302305670, 0.8197749522141674072, 1.842446510343001442 ) ) ;
#181506 = CARTESIAN_POINT ( 'NONE',  ( 0.6086344939593493208, -0.2706599535906920040, 1.821105742621460744 ) ) ;
#181507 = COLOUR_RGB ( '', 0.31764706, 0.68627451, 0.89019608) ;
#181508 = CARTESIAN_POINT ( 'NONE',  ( 8.284195553149872993, 9.623648552551724578, -1.199719254218445830 ) ) ;
#181509 =( NAMED_UNIT ( * ) PLANE_ANGLE_UNIT ( ) SI_UNIT ( $, .RADIAN. ) );
#181510 = CARTESIAN_POINT ( 'NONE',  ( 5.157177646623883227, -1.542991646335686973, -0.9753701268572569916 ) ) ;
#181511 = CARTESIAN_POINT ( 'NONE',  ( 5.625625018759272677, 0.3960990390993284205, 1.976956468877195894 ) ) ;
#181512 = CARTESIAN_POINT ( 'NONE',  ( -7.720478407978036195, 11.09464301169468037, -1.199719254218446718 ) ) ;
#181514 = CARTESIAN_POINT ( 'NONE',  ( -5.661411662158206681, 8.762674818229999829, -1.199719254218452047 ) ) ;
#181513 = CARTESIAN_POINT ( 'NONE',  ( 4.715850076732730045, -2.219782111298532978, 0.4368881197941154038 ) ) ;
#181515 = CARTESIAN_POINT ( 'NONE',  ( 0.6101635361662772761, -2.095732242510168764, 0.2083838208960953620 ) ) ;
#181516 = CARTESIAN_POINT ( 'NONE',  ( -6.424584688029276514, 8.588711117491191871, 1.599625672291269396 ) ) ;
#181517 = CARTESIAN_POINT ( 'NONE',  ( 4.844224204019831781, -0.9789346907586125024, 1.824324395707350943 ) ) ;
#181518 = CARTESIAN_POINT ( 'NONE',  ( 7.879259827836241570, 12.34422023245099176, 1.040834085586084257E-14 ) ) ;
#181519 = CARTESIAN_POINT ( 'NONE',  ( 4.726684935852882852, 4.891486930089099516, -0.8194250277325197951 ) ) ;
#181520 = APPLICATION_PROTOCOL_DEFINITION ( 'draft international standard', 'automotive_design', 1998, #81028 ) ;
#181521 = CARTESIAN_POINT ( 'NONE',  ( -8.528242318195895066, 9.908369778438709474, 1.199719254218462483 ) ) ;
#181522 = UNCERTAINTY_MEASURE_WITH_UNIT (LENGTH_MEASURE( 1.000000000000000082E-05 ), #154558, 'distance_accuracy_value', 'NONE');
#181523 = CARTESIAN_POINT ( 'NONE',  ( -5.097502569058280031, 5.049433873430397846, -0.7216878364869820928 ) ) ;
#181524 = CARTESIAN_POINT ( 'NONE',  ( 6.526270840131753737, 8.707344961610770540, -1.599625672291283607 ) ) ;
#181525 = CARTESIAN_POINT ( 'NONE',  ( 5.512200117181983217, 6.216449928263548586, -0.9568283335872149742 ) ) ;
#181526 = CARTESIAN_POINT ( 'NONE',  ( -8.663296969452339624, 13.05100419776235299, 1.040834085586084257E-14 ) ) ;
#181528 = CARTESIAN_POINT ( 'NONE',  ( 1.828696429707490578, -1.052382519090878654, -1.956348917980913260 ) ) ;
#181527 = CARTESIAN_POINT ( 'NONE',  ( 0.2289750728588327566, 1.457791096766167360, -1.540313549178488284 ) ) ;
#181529 = CARTESIAN_POINT ( 'NONE',  ( -5.608755560901242276, 5.628057139458180202, 0.4582055134699433707 ) ) ;
#181530 = CARTESIAN_POINT ( 'NONE',  ( -6.074935347375019390, 9.245119117649618801, 1.199719254218452047 ) ) ;
#181531 = CARTESIAN_POINT ( 'NONE',  ( 4.950698647284403009, 8.927565521807144577, 1.040834085586084257E-14 ) ) ;
#181532 = CARTESIAN_POINT ( 'NONE',  ( 3.226955236329264398, -1.811681696138227160, -0.7532884077038404236 ) ) ;
#181533 = CARTESIAN_POINT ( 'NONE',  ( 5.799137018343234473, 7.788745826199009237, -1.599625672291262513 ) ) ;
#181534 = CARTESIAN_POINT ( 'NONE',  ( -4.167566996647928512, 7.418725663478599408, 0.7529690952402002813 ) ) ;
#181535 = CARTESIAN_POINT ( 'NONE',  ( 3.334415713957098681, 5.977569868670206787, -1.199719254218446718 ) ) ;
#181536 = CARTESIAN_POINT ( 'NONE',  ( -4.800995793014949165, 8.615262501910491366, 0.7216878364870267237 ) ) ;
#181537 = CARTESIAN_POINT ( 'NONE',  ( -7.049876689426103127, 10.20831132343037062, -1.082531754730537976 ) ) ;
#181538 = CARTESIAN_POINT ( 'NONE',  ( 2.865608904542978674, -1.736054085904148669, -1.217558864107195715 ) ) ;
#181539 = CARTESIAN_POINT ( 'NONE',  ( -5.773793314573309132, 7.829454515125894964, 1.599625672291263179 ) ) ;
#181540 = CARTESIAN_POINT ( 'NONE',  ( 3.982823771651412770, 1.862158852298421152, 0.6176278068941787325 ) ) ;
#181541 = CARTESIAN_POINT ( 'NONE',  ( 3.432649856329002880, 2.108609624295390006, 0.4754391814798044069 ) ) ;
#181542 = EDGE_CURVE ( 'NONE', #135502, #162623, #14974, .T. ) ;
#181543 = CARTESIAN_POINT ( 'NONE',  ( 3.263068207883256466, 1.795673413606920565, -0.4063787724192802209 ) ) ;
#181544 = CARTESIAN_POINT ( 'NONE',  ( -4.047760499819613500, 7.578451897646762525, -0.3740945913360635977 ) ) ;
#181545 = CARTESIAN_POINT ( 'NONE',  ( -1.364683531250014514, -1.157291666325248158, 0.7879004041258379498 ) ) ;
#181546 = CARTESIAN_POINT ( 'NONE',  ( 5.085792842222247145, -1.727793525551263087, -0.2079256833047369302 ) ) ;
#181547 = DIRECTION ( 'NONE',  ( 0.000000000000000000, -1.000000000000000000, 2.168404344971004924E-15 ) ) ;
#181548 = CARTESIAN_POINT ( 'NONE',  ( 5.531363484695522637, 5.555604941673978558, -0.7216878364870207285 ) ) ;
#181549 = CARTESIAN_POINT ( 'NONE',  ( -1.192622389734054877E-15, -8.030730635398791506, 11.29670623088188464 ) ) ;
#181550 = CARTESIAN_POINT ( 'NONE',  ( 2.096749907087645415, -0.5762017740289016032, -2.083436276955972222 ) ) ;
#181551 = AXIS2_PLACEMENT_3D ( 'NONE', #14011, #180798, #32423 ) ;
#181552 = CARTESIAN_POINT ( 'NONE',  ( 4.288435361214689046, -1.930121902525683053, 0.5825675424541224556 ) ) ;
#181553 = CARTESIAN_POINT ( 'NONE',  ( -8.880227426826648340, 11.38335130276301754, 1.443375672974064550 ) ) ;
#181554 = CARTESIAN_POINT ( 'NONE',  ( 1.411231610350563992, 1.906656261001705488, 1.018656936289302539 ) ) ;
#181555 = CARTESIAN_POINT ( 'NONE',  ( 2.583225839741074115, 1.803852637447726392, -0.7955871043755156080 ) ) ;
#181556 = CARTESIAN_POINT ( 'NONE',  ( 6.509000000000037645, 2.054060622569788386, 2.307050226316338382 ) ) ;
#181557 = CARTESIAN_POINT ( 'NONE',  ( 3.597155123818120082, -0.5607282099057244729, 1.859368625674643782 ) ) ;
#181560 = VERTEX_POINT ( 'NONE', #196461 ) ;
#181559 = CARTESIAN_POINT ( 'NONE',  ( -3.960390268967665328, 6.674186842887300131, 1.082531754730549967 ) ) ;
#181558 = DIRECTION ( 'NONE',  ( 0.7592566023653005702, 0.6507913734559639396, 0.000000000000000000 ) ) ;
#181561 = CARTESIAN_POINT ( 'NONE',  ( -7.553827861469316396, 8.841829255582865699, -1.199719254218452047 ) ) ;
#181562 = CARTESIAN_POINT ( 'NONE',  ( 5.571474780572990504, 5.464751763615448787, 0.7998128361456352531 ) ) ;
#181563 = CARTESIAN_POINT ( 'NONE',  ( -6.089547271193396227, 7.133501900260939443, -1.199719254218453823 ) ) ;
#181564 = CARTESIAN_POINT ( 'NONE',  ( -8.798878505144649864, 11.28844422746735532, -1.443375672974058777 ) ) ;
#181565 = CARTESIAN_POINT ( 'NONE',  ( 1.554063478550568256, 0.6399170599369340406, -2.111937735441645980 ) ) ;
#181566 = CARTESIAN_POINT ( 'NONE',  ( 3.285556943750000070, -2.734374999522042771, 0.000000000000000000 ) ) ;
#181567 = CARTESIAN_POINT ( 'NONE',  ( 5.137533780887935997, 1.831872034461759835, -0.7024582609849658876 ) ) ;
#181568 = ORIENTED_EDGE ( 'NONE', *, *, #37635, .T. ) ;
#181569 = CARTESIAN_POINT ( 'NONE',  ( 3.432911303685074689, -1.728510519573158266, 1.222591858268074150 ) ) ;
#181570 = CARTESIAN_POINT ( 'NONE',  ( -0.7500000000000006661, 2.389583334016155636, -1.299038105676652011 ) ) ;
#181571 = CARTESIAN_POINT ( 'NONE',  ( 0.1747926744264660381, 7.629137130509078268, -2.455305974604498953 ) ) ;
#181572 = CARTESIAN_POINT ( 'NONE',  ( 4.365079047384805122, 1.785254547683400306, -0.4496667978745386152 ) ) ;
#181573 = ORIENTED_EDGE ( 'NONE', *, *, #185183, .T. ) ;
#181574 = CARTESIAN_POINT ( 'NONE',  ( -7.486073373039941359, 11.88550270185529278, -0.7998128361456291469 ) ) ;
#181575 = CARTESIAN_POINT ( 'NONE',  ( 0.4307572970102366283, 3.041534709929996527, 0.4240169840790947164 ) ) ;
#181576 = CARTESIAN_POINT ( 'NONE',  ( 5.097945154717048233, 1.425953928781589886, 1.569717048080176314 ) ) ;
#181577 = CARTESIAN_POINT ( 'NONE',  ( -0.1106727585415930720, -0.002281114264979212502, -2.003378291782103027 ) ) ;
#181578 = CARTESIAN_POINT ( 'NONE',  ( 5.113396490648394632, 9.117379672398465473, 1.040834085586084257E-14 ) ) ;
#181579 = CARTESIAN_POINT ( 'NONE',  ( 5.061820804786828276, 2.038956591669589535, -0.2981446164109917696 ) ) ;
#181582 = CARTESIAN_POINT ( 'NONE',  ( 2.665370095338463585, 0.9869154847663293983, 1.554228294351194473 ) ) ;
#181581 = CARTESIAN_POINT ( 'NONE',  ( 0.9239872072115723478, 0.9125040393608827571, 1.621899335316509649 ) ) ;
#181580 = CARTESIAN_POINT ( 'NONE',  ( -15.75000000000000000, 10.90000000000000036, -3.200000000000001510 ) ) ;
#181583 = CARTESIAN_POINT ( 'NONE',  ( 6.909851844459134362, 11.21324425184434936, -0.7998128361456291469 ) ) ;
#181584 = CARTESIAN_POINT ( 'NONE',  ( 0.000000000000000000, 4.006659545634088992, 0.000000000000000000 ) ) ;
#181585 = DIRECTION ( 'NONE',  ( 0.000000000000000000, 0.000000000000000000, -1.000000000000000000 ) ) ;
#181587 = ORIENTED_EDGE ( 'NONE', *, *, #163792, .F. ) ;
#181586 = FACE_OUTER_BOUND ( 'NONE', #106860, .T. ) ;
#181588 = CARTESIAN_POINT ( 'NONE',  ( 2.912931060594741162, 1.598032330669514778, -1.522282275181946032 ) ) ;
#181589 = CARTESIAN_POINT ( 'NONE',  ( 5.061948053633171796, 2.238818834584723749, -0.3250485201948364877 ) ) ;
#181590 = CARTESIAN_POINT ( 'NONE',  ( -7.537970219518091319, 7.896646132300314314, -0.7216878364870278340 ) ) ;
#181591 = CARTESIAN_POINT ( 'NONE',  ( 5.256058454422637638, 0.7267480909730811289, -1.659609831382781397 ) ) ;
#181592 = CARTESIAN_POINT ( 'NONE',  ( 5.348823992091742419, -1.734843432642660721, -0.8128511771108116735 ) ) ;
#181593 = FACE_OUTER_BOUND ( 'NONE', #182516, .T. ) ;
#181594 = EDGE_CURVE ( 'NONE', #182051, #24037, #48103, .T. ) ;
#181595 = CARTESIAN_POINT ( 'NONE',  ( 5.559403950928493821, 0.3636877230743483236, -1.834782481876767291 ) ) ;
#181596 = CARTESIAN_POINT ( 'NONE',  ( 5.969184020103408095, 1.641702931788184383, 0.8765767931452476125 ) ) ;
#181597 = CARTESIAN_POINT ( 'NONE',  ( -1.364683531249997417, 5.259375000341425022, 1.214306433183764966E-14 ) ) ;
#181598 = AXIS2_PLACEMENT_3D ( 'NONE', #183353, #96010, #83714 ) ;
#181599 = CARTESIAN_POINT ( 'NONE',  ( 6.315310819269446263, -0.2119676446582714757, 1.757049200028695690 ) ) ;
#181600 = CARTESIAN_POINT ( 'NONE',  ( 0.3215004009857677092, -1.429452135790244549, -1.422604240635255479 ) ) ;
#181602 = CARTESIAN_POINT ( 'NONE',  ( 3.317110013156245873, 1.904127318671836600, 0.9001942471269042123 ) ) ;
#181601 = CARTESIAN_POINT ( 'NONE',  ( -3.917943204224921150, 5.594019709727598766, -1.443375672974051449 ) ) ;
#181603 = CARTESIAN_POINT ( 'NONE',  ( 8.211434591371064684, 12.73175745657494851, -0.7998128361456352531 ) ) ;
#181605 = CARTESIAN_POINT ( 'NONE',  ( -1.232288786374426959, 2.852001308287894332, -0.7749999999999979128 ) ) ;
#181604 = CARTESIAN_POINT ( 'NONE',  ( -2.788906526875773208E-15, 11.96875000068279604, -1.499999999999998446 ) ) ;
#181606 = DIRECTION ( 'NONE',  ( 0.000000000000000000, 0.000000000000000000, 1.000000000000000000 ) ) ;
#181607 = CARTESIAN_POINT ( 'NONE',  ( 1.705338084499245843, 1.755316507598453368, -0.9991084507309263563 ) ) ;
#181608 = CARTESIAN_POINT ( 'NONE',  ( -1.364683531250012516, 1.780208333674757615, 0.7879004041258379498 ) ) ;
#181609 = CARTESIAN_POINT ( 'NONE',  ( 3.846762897975340767, 5.510976019103107859, -1.599625672291256295 ) ) ;
#181610 = CARTESIAN_POINT ( 'NONE',  ( 3.163507678178357541, 0.3205598832158839673, -2.137589075770351066 ) ) ;
#181611 = CARTESIAN_POINT ( 'NONE',  ( 6.620655732516652847, 2.468432086671234149, 2.210906647470804565 ) ) ;
#181613 = CARTESIAN_POINT ( 'NONE',  ( 3.557915510932077918, 4.150901429420823519, -2.419999999999995044 ) ) ;
#181612 = CARTESIAN_POINT ( 'NONE',  ( 2.898410978271408922, 6.603506251283770112, -0.7998128361456362523 ) ) ;
#181614 =( BOUNDED_CURVE ( )  B_SPLINE_CURVE ( 2, ( #43113, #109228, #77710, #111352, #175238, #178429, #177357 ),
 .UNSPECIFIED., .F., .T. ) 
 B_SPLINE_CURVE_WITH_KNOTS ( ( 3, 2, 2, 3 ),
 ( 0.1874999999999999167, 0.1916666666666665964, 0.1958333333333332760, 0.1999999999999999556 ),
 .UNSPECIFIED. ) 
 CURVE ( )  GEOMETRIC_REPRESENTATION_ITEM ( )  RATIONAL_B_SPLINE_CURVE ( ( 1.000000000000002665, 0.8660254037844360431, 1.000000000000000000, 0.8660254037844387076, 1.000000000000000000, 0.8660254037844404840, 0.9999999999999982236 ) ) 
 REPRESENTATION_ITEM ( '' )  );
#181615 = CARTESIAN_POINT ( 'NONE',  ( 9.707274797260268429, 10.42750147299956964, 0.000000000000000000 ) ) ;
#181616 = CARTESIAN_POINT ( 'NONE',  ( -8.074422843256325422, -6.701288531901958834, 7.470306724221552841 ) ) ;
#181617 = CARTESIAN_POINT ( 'NONE',  ( -8.026063749610061748, 9.426457798375635022, -1.082531754730543971 ) ) ;
#181618 = CARTESIAN_POINT ( 'NONE',  ( 0.8904706703079521279, -0.5376514911656914419, -2.124458794526106864 ) ) ;
#181619 = CARTESIAN_POINT ( 'NONE',  ( -4.475070042639309520, 5.445751865460756846, 1.284222742053057642 ) ) ;
#181620 = CARTESIAN_POINT ( 'NONE',  ( 1.727766546026089145, -2.130035881452702728, 0.7632205929882311946 ) ) ;
#181621 = CARTESIAN_POINT ( 'NONE',  ( -7.374745490829552885, 10.69128794168811680, -1.199719254218446718 ) ) ;
#181622 = CARTESIAN_POINT ( 'NONE',  ( -5.233084104750526322, 5.207612331738130429, 0.000000000000000000 ) ) ;
#181623 = CARTESIAN_POINT ( 'NONE',  ( 1.364683531249990311, 3.696875000341416584, 1.214306433183764966E-14 ) ) ;
#181624 = CARTESIAN_POINT ( 'NONE',  ( 4.678042868546113731, 8.270637144445508682, 0.5573067791126932180 ) ) ;
#181625 = CARTESIAN_POINT ( 'NONE',  ( 1.500000000000001332, 11.62499999999999645, 0.000000000000000000 ) ) ;
#181626 = CARTESIAN_POINT ( 'NONE',  ( 4.523580528814945545, 5.306540700819438960, 1.199719254218452047 ) ) ;
#181627 = CARTESIAN_POINT ( 'NONE',  ( 3.127930002535435516, 0.9861435696450934207, -1.469289397387682161 ) ) ;
#181629 = STYLED_ITEM ( 'NONE', ( #213072 ), #91529 ) ;
#181628 = CARTESIAN_POINT ( 'NONE',  ( 6.036183878773405453, 1.092744051193066834, -1.917163762461614240 ) ) ;
#181630 = CARTESIAN_POINT ( 'NONE',  ( -1.364683531250014514, 14.40104166700806410, -0.7879004041258335089 ) ) ;
#181631 = ORIENTED_EDGE ( 'NONE', *, *, #139225, .F. ) ;
#181632 = CARTESIAN_POINT ( 'NONE',  ( -4.423703259808839938, 8.383013913077441259, 0.7998128361456352531 ) ) ;
#181633 = CARTESIAN_POINT ( 'NONE',  ( 5.536732523015378327, -1.587826920732600122, 1.242742243127918700 ) ) ;
#181635 = VERTEX_POINT ( 'NONE', #213736 ) ;
#181634 = CARTESIAN_POINT ( 'NONE',  ( 4.922017755325088118, -1.802143800875387614, 0.1849416998233286979 ) ) ;
#181636 = CARTESIAN_POINT ( 'NONE',  ( 2.236979667955760309, -1.672073921526989748, 0.8388852543278202401 ) ) ;
#181637 = CARTESIAN_POINT ( 'NONE',  ( 2.747004861044194612, -0.3495022371792326221, -2.040372298647576965 ) ) ;
#181638 = CARTESIAN_POINT ( 'NONE',  ( -7.065207446052813367, 8.375735120883982532, -1.082531754730549967 ) ) ;
#181639 = CARTESIAN_POINT ( 'NONE',  ( 1.793074957647671663, -0.09724762972821224261, -1.910064080951429100 ) ) ;
#181641 =( GEOMETRIC_REPRESENTATION_CONTEXT ( 3 ) GLOBAL_UNCERTAINTY_ASSIGNED_CONTEXT ( ( #47548 ) ) GLOBAL_UNIT_ASSIGNED_CONTEXT ( ( #4115, #204449, #124390 ) ) REPRESENTATION_CONTEXT ( 'NONE', 'WORKASPACE' ) );
#181640 = CARTESIAN_POINT ( 'NONE',  ( -0.4153311931459131578, 3.780306491160339011, 0.5000000000000066613 ) ) ;
#181642 = CARTESIAN_POINT ( 'NONE',  ( -9.645406396194509568, 4.042443384815813445, -6.587269312116742270 ) ) ;
#181643 = CARTESIAN_POINT ( 'NONE',  ( -4.025218236631250335, 7.648764168548251696, 0.3240912158420958256 ) ) ;
#181644 = CARTESIAN_POINT ( 'NONE',  ( 0.6823417656249899377, 4.738541667008086655, -1.181850606188754593 ) ) ;
#181645 = CARTESIAN_POINT ( 'NONE',  ( 1.353610510645312237, -1.387278792934818705, -1.316581319992945920 ) ) ;
#181646 = AXIS2_PLACEMENT_3D ( 'NONE', #168676, #151378, #85292 ) ;
#181647 = CARTESIAN_POINT ( 'NONE',  ( 6.875393295905841917, 7.193916064744513506, 0.000000000000000000 ) ) ;
#181648 = CARTESIAN_POINT ( 'NONE',  ( 3.051168888765115828, 1.684027830550902882, -1.006202029777767848 ) ) ;
#181649 = CARTESIAN_POINT ( 'NONE',  ( 0.2982036909132765867, -1.844429998007334648, 0.8144978490535054183 ) ) ;
#181650 = CARTESIAN_POINT ( 'NONE',  ( -4.878955176071358757, 6.785476686873604280, -1.599625672291271394 ) ) ;
#181652 = CARTESIAN_POINT ( 'NONE',  ( 10.97113184882213943, -5.223163831703878657, -0.3618152180564628284 ) ) ;
#181651 = CARTESIAN_POINT ( 'NONE',  ( 9.935427640716063991, 10.48575375712389679, -0.7998128361456281477 ) ) ;
#181653 = CARTESIAN_POINT ( 'NONE',  ( 6.749300054864300513, -1.582014061365591751, -1.175997427595596445 ) ) ;
#181654 = CARTESIAN_POINT ( 'NONE',  ( -1.201851678989727383E-14, 2.696875000341417916, -1.575800808251660134 ) ) ;
#181655 = CARTESIAN_POINT ( 'NONE',  ( 2.250246052928657203, 0.9454230575737303521, -1.777374461261713279 ) ) ;
#181657 = CARTESIAN_POINT ( 'NONE',  ( 1.353279953590967644, 0.1518699462816820722, -2.111824974118434728 ) ) ;
#181656 = CARTESIAN_POINT ( 'NONE',  ( -7.212574532790100079, 9.437756259720353924, -1.443375672974059665 ) ) ;
#181658 = CARTESIAN_POINT ( 'NONE',  ( 9.285642839235046964, 11.47635228829340370, -7.530412293235562160 ) ) ;
#181659 = CARTESIAN_POINT ( 'NONE',  ( 3.209495720308676248, -1.691010085789945716, -1.194244797349801157 ) ) ;
#181660 = CARTESIAN_POINT ( 'NONE',  ( 5.273195401072370281, 5.116759154198018855, -0.7998128361456481317 ) ) ;
#181662 = CARTESIAN_POINT ( 'NONE',  ( 4.029797971759831121, 5.724516938518342535, -1.599625672291255185 ) ) ;
#181661 = CARTESIAN_POINT ( 'NONE',  ( 5.894497796308646009, 1.709714471583067885, -1.202884697265863778 ) ) ;
#181664 = ORIENTED_EDGE ( 'NONE', *, *, #212020, .F. ) ;
#181663 = CARTESIAN_POINT ( 'NONE',  ( 4.102439050647597618, -0.5725816820084869141, -1.733541218493547476 ) ) ;
#181665 = CARTESIAN_POINT ( 'NONE',  ( 10.22692794340986921, 10.82583744360002243, 0.000000000000000000 ) ) ;
#181666 = CARTESIAN_POINT ( 'NONE',  ( 1.029210992452657125, 2.808910805765225227, -1.137835564023402135 ) ) ;
#181667 = CARTESIAN_POINT ( 'NONE',  ( 9.263131865311954982, 13.58559029627111592, -6.818719126704674949 ) ) ;
#181668 = CARTESIAN_POINT ( 'NONE',  ( 5.051906976816819217, 0.6964463896041681590, -2.094057263239030853 ) ) ;
#181669 = CARTESIAN_POINT ( 'NONE',  ( 0.6823417656249934904, 10.00520833367472839, 1.181850606188764807 ) ) ;
#181670 = VERTEX_POINT ( 'NONE', #65360 ) ;
#181671 = CARTESIAN_POINT ( 'NONE',  ( 4.020093958671668410, -1.906945023982812515, 0.1437811316862200317 ) ) ;
#181672 = CARTESIAN_POINT ( 'NONE',  ( -8.597841969360544567, 13.18256606422934674, 0.7998128361456341429 ) ) ;
#181673 = CARTESIAN_POINT ( 'NONE',  ( 6.446011968293428041, 9.607765498729298415, -1.199719254218440723 ) ) ;
#181674 = CARTESIAN_POINT ( 'NONE',  ( -1.360316468749998675, 1.442708333674736831, 0.7853790794158961308 ) ) ;
#181675 = CARTESIAN_POINT ( 'NONE',  ( 5.816084710138150093, 5.887779704690372817, -0.7216878364870257245 ) ) ;
#181676 = CARTESIAN_POINT ( 'NONE',  ( 6.589320575229280053, 7.629137130509070275, 2.496737603865983868 ) ) ;
#181677 = CARTESIAN_POINT ( 'NONE',  ( 0.000000000000000000, 8.500000000000000000, -9.999999999999996447 ) ) ;
#181678 = CARTESIAN_POINT ( 'NONE',  ( 0.04610459085982109018, -1.479553692838073475, 1.095721268101347734 ) ) ;
#181679 = ORIENTED_EDGE ( 'NONE', *, *, #92241, .F. ) ;
#181680 = DIRECTION ( 'NONE',  ( 0.000000000000000000, 1.000000000000000000, 0.000000000000000000 ) ) ;
#181681 = CARTESIAN_POINT ( 'NONE',  ( 5.061713478001653499, 1.850364105758989020, -0.2730526881008291662 ) ) ;
#181682 = CARTESIAN_POINT ( 'NONE',  ( -6.770610912236888268, -7.154544010627095219, -6.663994888585867749 ) ) ;
#181683 = CARTESIAN_POINT ( 'NONE',  ( -1.499999999999996003, 8.266799604812621993, -3.162088779278208417 ) ) ;
#181684 = CIRCLE ( 'NONE', #119469, 0.08000000000000020983 ) ;
#181685 = CARTESIAN_POINT ( 'NONE',  ( -6.887178846062123938, 8.097758744236356776, -1.082531754730544860 ) ) ;
#181686 = CARTESIAN_POINT ( 'NONE',  ( 5.508690485854129903, 5.321227076451600091, 1.040834085586084257E-14 ) ) ;
#181687 = CARTESIAN_POINT ( 'NONE',  ( 1.147236149642312242, 1.739494102415694243, -0.9234435978164361458 ) ) ;
#181688 = CARTESIAN_POINT ( 'NONE',  ( 1.950796209937825321, -1.844718841590715863, -0.8146091914792084054 ) ) ;
#181689 = CARTESIAN_POINT ( 'NONE',  ( -8.565000355531095622, 11.01558638625153286, -1.599625672291263179 ) ) ;
#181690 = CARTESIAN_POINT ( 'NONE',  ( 7.018280793729500644, 8.217024343219755167, -1.199719254218452047 ) ) ;
#181691 = SURFACE_SIDE_STYLE ('',( #194757 ) ) ;
#181692 = CARTESIAN_POINT ( 'NONE',  ( 2.607599380506659514, -2.167453834138896696, 0.3226137089109848421 ) ) ;
#181693 = CARTESIAN_POINT ( 'NONE',  ( 6.182242880246401562, -0.9723386526096773341, 1.545037271442825100 ) ) ;
#181694 = CARTESIAN_POINT ( 'NONE',  ( -10.64723070543352712, 11.31619066596094392, 0.7998128361456462443 ) ) ;
#181695 = CARTESIAN_POINT ( 'NONE',  ( 10.46159335054553807, 1.264806443676224967, -5.593087811558966393 ) ) ;
#181696 = CARTESIAN_POINT ( 'NONE',  ( 5.587368702607580673, 5.691220705896524734, -0.7216878364870458196 ) ) ;
#181697 = CARTESIAN_POINT ( 'NONE',  ( 9.284636267260101050, 9.726497154758602548, -0.7998128361456281477 ) ) ;
#181698 = CARTESIAN_POINT ( 'NONE',  ( 4.376584659113025744, 4.000436945253625254, 0.7998128361456341429 ) ) ;
#181699 = CARTESIAN_POINT ( 'NONE',  ( 5.668717624289557833, 8.667235424096215723, -1.082531754730548412 ) ) ;
#181700 = ORIENTED_EDGE ( 'NONE', *, *, #135941, .F. ) ;
#181702 = CARTESIAN_POINT ( 'NONE',  ( 0.3990879006048999589, -0.2487020831964822098, -1.997621932491387531 ) ) ;
#181701 = CARTESIAN_POINT ( 'NONE',  ( 4.845164456061270997, 0.5726227986864868003, -1.750029900461601340 ) ) ;
#181703 = CARTESIAN_POINT ( 'NONE',  ( 2.988014862494779322, 2.163403104293510459, 0.7763308700806015317 ) ) ;
#181705 = CARTESIAN_POINT ( 'NONE',  ( 1.199803204733034923, 0.7606819372595281514, -1.698589668608577963 ) ) ;
#181704 = FACE_OUTER_BOUND ( 'NONE', #50580, .T. ) ;
#181706 = CARTESIAN_POINT ( 'NONE',  ( -1.737500000000000266, -0.05833333333333384774, -3.009438278150923907 ) ) ;
#181707 = CARTESIAN_POINT ( 'NONE',  ( -2.442440228756222353, 6.001264033524212671, -0.7998128361456281477 ) ) ;
#181708 = FACE_OUTER_BOUND ( 'NONE', #57553, .T. ) ;
#181709 = CARTESIAN_POINT ( 'NONE',  ( 4.377155534175989793, -1.710687068321177007, -0.8549628122409487219 ) ) ;
#181710 = CARTESIAN_POINT ( 'NONE',  ( -9.169391961543940539, 9.592045464756413509, 1.040834085586084257E-14 ) ) ;
#181711 = EDGE_CURVE ( 'NONE', #123093, #111396, #197510, .T. ) ;
#181712 = CARTESIAN_POINT ( 'NONE',  ( -6.075462232699549325, 9.141770800574526845, 1.082531754730549967 ) ) ;
#181714 = CARTESIAN_POINT ( 'NONE',  ( 2.658895327995167701, -1.626580691111865207, -0.9237732865615968514 ) ) ;
#181713 = CARTESIAN_POINT ( 'NONE',  ( 3.316043925569078787, 1.324660045548868181, -1.617576387421674866 ) ) ;
#181715 = CARTESIAN_POINT ( 'NONE',  ( 8.134528978519385944, 8.592631351135175066, -0.7216878364870267237 ) ) ;
#181716 = CARTESIAN_POINT ( 'NONE',  ( -11.86145016429273191, 13.40000000000000036, 1.099999999999996758 ) ) ;
#181717 = CARTESIAN_POINT ( 'NONE',  ( 6.005383971424570255, -1.826508537601937432, 0.2321369796495567073 ) ) ;
#181718 = CARTESIAN_POINT ( 'NONE',  ( 5.034155109375821446, 4.767602470560229122, -0.7998128361456221525 ) ) ;
#181719 = CARTESIAN_POINT ( 'NONE',  ( 0.3282377607281140031, 1.073664549684631986, 1.224999999999960565 ) ) ;
#181720 = CARTESIAN_POINT ( 'NONE',  ( 4.529763579968347997, -1.064299448457445729, -1.357287084437068803 ) ) ;
#181721 = CARTESIAN_POINT ( 'NONE',  ( -7.562750758324527922, 7.717630727667075696, 1.040834085586084257E-14 ) ) ;
#181722 = CARTESIAN_POINT ( 'NONE',  ( 0.3165338080420940781, 0.8936020571472038654, -1.485981903106075031 ) ) ;
#181723 = PRESENTATION_STYLE_ASSIGNMENT (( #115731 ) ) ;
#181724 = FACE_OUTER_BOUND ( 'NONE', #197415, .T. ) ;
#181725 = CARTESIAN_POINT ( 'NONE',  ( 4.733362013637422372, 0.006437197247223526778, -2.171239809022653677 ) ) ;
#181726 = CARTESIAN_POINT ( 'NONE',  ( 3.193790821891542731, -0.7392406677243367197, 1.669511829839696260 ) ) ;
#181727 = CARTESIAN_POINT ( 'NONE',  ( 1.428482823135175606, -1.248714028858177061, 1.512975372890807524 ) ) ;
#181728 = CARTESIAN_POINT ( 'NONE',  ( 5.876184115051023227, -2.107333617329323783, -0.2052446207758129582 ) ) ;
#181730 = CARTESIAN_POINT ( 'NONE',  ( -1.201851678989727383E-14, 3.634375000341422357, 1.575800808251672791 ) ) ;
#181729 = CARTESIAN_POINT ( 'NONE',  ( 5.987847201643853978, -2.280908734910926938, -0.2287418647285797413 ) ) ;
#181731 = CARTESIAN_POINT ( 'NONE',  ( 9.887974103068218668, 10.43039129653476493, 0.7998128361456462443 ) ) ;
#181732 = CARTESIAN_POINT ( 'NONE',  ( 1.207859650372544280, 1.608047128250057689, 1.382383069919224106 ) ) ;
#181733 = CARTESIAN_POINT ( 'NONE',  ( -4.270455198624581783, 7.926022131796578662, 1.040834085586084257E-14 ) ) ;
#181734 = TOROIDAL_SURFACE ( 'NONE', #88387, 1.749999999999999778, 0.5000000000000007772 ) ;
#181735 = CARTESIAN_POINT ( 'NONE',  ( -4.731432421044877934, 6.543090462684225450, -1.443375672974051449 ) ) ;
#181736 = EDGE_CURVE ( 'NONE', #52005, #76056, #46678, .T. ) ;
#181737 = CARTESIAN_POINT ( 'NONE',  ( 6.332918745153389928, -2.058942774313234025, -0.6888473222384088324 ) ) ;
#181739 = CARTESIAN_POINT ( 'NONE',  ( -1.500000000000015099, 12.76041666734946567, -0.8660254037844309360 ) ) ;
#181738 = CARTESIAN_POINT ( 'NONE',  ( 6.883263157960364254, 2.431740398616466070, 2.435552827938294751 ) ) ;
#181742 = VERTEX_POINT ( 'NONE', #55539 ) ;
#181741 = CARTESIAN_POINT ( 'NONE',  ( 2.491161192834326688, -2.126536535197431022, -0.6419364700022185399 ) ) ;
#181740 = VECTOR ( 'NONE', #7248, 1000.000000000000000 ) ;
#181743 = CARTESIAN_POINT ( 'NONE',  ( -0.01642261062154842799, -2.298356651571492826, -0.04744217504730821600 ) ) ;
#181745 = CARTESIAN_POINT ( 'NONE',  ( 4.733292769410803125, 0.005207392524877744490, -2.062741129207305235 ) ) ;
#181744 = CARTESIAN_POINT ( 'NONE',  ( 4.202137545231717120, 6.989912005157271402, 1.199719254218462483 ) ) ;
#181746 = CARTESIAN_POINT ( 'NONE',  ( 5.716698046817569434, 6.698511138489155137, -1.199719254218452047 ) ) ;
#181747 = CARTESIAN_POINT ( 'NONE',  ( 5.306037014901791693, 7.283738832175834510, 1.599625672291269396 ) ) ;
#181748 = CARTESIAN_POINT ( 'NONE',  ( -1.642778471875000035, -3.055208332855375630, -2.845375778867859751 ) ) ;
#181749 = SURFACE_STYLE_FILL_AREA ( #198008 ) ;
#181750 = CARTESIAN_POINT ( 'NONE',  ( 0.9375778709549039691, 0.8456052968917522339, -1.912177616049218098 ) ) ;
#181751 = CARTESIAN_POINT ( 'NONE',  ( 4.247483403459266782, 1.840758003770435414, -0.04960325993209198370 ) ) ;
#181752 = CARTESIAN_POINT ( 'NONE',  ( 5.301401758143367893, 6.143722458377430584, 1.199719254218462483 ) ) ;
#181753 = CARTESIAN_POINT ( 'NONE',  ( 2.309205411980755240, -0.3811568730716380915, 1.681943839628738058 ) ) ;
#181754 = CARTESIAN_POINT ( 'NONE',  ( -0.01248194115436446205, -0.5331630387654020531, 1.944732228473695868 ) ) ;
#181755 = CARTESIAN_POINT ( 'NONE',  ( 1.670936656956054644, 1.588967112724626096, 1.661273962566457874 ) ) ;
#181756 = CARTESIAN_POINT ( 'NONE',  ( 1.364683531249988535, 3.926041667008087543, 0.7879004041258500513 ) ) ;
#181757 = CARTESIAN_POINT ( 'NONE',  ( 1.722331603166191050, -1.256259422768091216, -1.881381621351454037 ) ) ;
#181758 = CARTESIAN_POINT ( 'NONE',  ( 4.125680639212436773, -2.015421878069530326, 0.6112012065569141228 ) ) ;
#181759 = CARTESIAN_POINT ( 'NONE',  ( -4.390861645979385663, 6.216034235099629157, -1.599625672291271394 ) ) ;
#181760 = CARTESIAN_POINT ( 'NONE',  ( 2.653260118625869080, 0.4764888685691510140, -1.704286641089979959 ) ) ;
#181761 = ADVANCED_BREP_SHAPE_REPRESENTATION ( '', ( #167773, #200407 ), #124768 ) ;
#181762 = CARTESIAN_POINT ( 'NONE',  ( 5.262536180398716290, 9.291375977107183104, -0.7998128361456291469 ) ) ;
#181763 = CARTESIAN_POINT ( 'NONE',  ( 4.204437033569277560, 7.919277282557212416, 0.000000000000000000 ) ) ;
#181764 = CARTESIAN_POINT ( 'NONE',  ( -4.903245109636583443, 8.872203061218007392, -0.7998128361456281477 ) ) ;
#181765 = CARTESIAN_POINT ( 'NONE',  ( 5.409340101728155936, 8.294351971116089572, -1.082531754730543971 ) ) ;
#181766 = CARTESIAN_POINT ( 'NONE',  ( 0.7499999999999902300, 2.233333333333351156, 1.299038105676669330 ) ) ;
#181767 = CARTESIAN_POINT ( 'NONE',  ( -2.937312835655025101, 6.578615408239493867, 1.040834085586084257E-14 ) ) ;
#181768 = CARTESIAN_POINT ( 'NONE',  ( 5.115582552657226501, 1.816446842268246931, 1.278514946224351689 ) ) ;
#181769 = CARTESIAN_POINT ( 'NONE',  ( 3.152458698460915532, -1.659165413833121550, 1.431739491984926449 ) ) ;
#181770 = CARTESIAN_POINT ( 'NONE',  ( -5.599681137644054729, 6.491715067794862293, 1.199719254218450271 ) ) ;
#181771 = CARTESIAN_POINT ( 'NONE',  ( -3.311934663488232733, 7.085950550703385531, -0.7998128361456481317 ) ) ;
#181772 = CARTESIAN_POINT ( 'NONE',  ( 6.164709077089638001, 0.6648188651474650213, 2.013622499735030491 ) ) ;
#181773 = CARTESIAN_POINT ( 'NONE',  ( -1.364683531250012516, 3.738541667008087099, -0.7879004041258300672 ) ) ;
#181774 = CARTESIAN_POINT ( 'NONE',  ( 6.609999999999971010, 7.629137130509032971, 2.319999999999996287 ) ) ;
#181776 = CARTESIAN_POINT ( 'NONE',  ( -3.578989364327652467, 6.158942777482099729, 1.082531754730560403 ) ) ;
#181775 = VECTOR ( 'NONE', #109366, 1000.000000000000000 ) ;
#181777 = CARTESIAN_POINT ( 'NONE',  ( 5.326475955075804514, -0.9554483686352827077, -1.893264085526874974 ) ) ;
#181778 = CARTESIAN_POINT ( 'NONE',  ( -7.268579750702168774, 7.652633595340216921, -0.7216878364870338292 ) ) ;
#181779 = ORIENTED_EDGE ( 'NONE', *, *, #88556, .T. ) ;
#181781 = CARTESIAN_POINT ( 'NONE',  ( -1.438722679664437232, 7.870294296420953906, -3.684004759497620185 ) ) ;
#181780 = CARTESIAN_POINT ( 'NONE',  ( -5.506019780925599960, 5.596313630600862510, 0.7216878364870257245 ) ) ;
#181782 = CARTESIAN_POINT ( 'NONE',  ( 5.087333953625774008, 6.958308917361963886, 1.599625672291267398 ) ) ;
#181783 = CARTESIAN_POINT ( 'NONE',  ( 5.829618728418341611, 0.9018330327132916269, -1.605192750430362025 ) ) ;
#181784 = CARTESIAN_POINT ( 'NONE',  ( 1.224999999999961231, 0.9583333340161364067, -0.7072540797573237947 ) ) ;
#181785 = CARTESIAN_POINT ( 'NONE',  ( 1.364683531249990311, 2.696875000341415696, 1.214306433183764966E-14 ) ) ;
#181786 = CARTESIAN_POINT ( 'NONE',  ( 1.188542350144041304, 1.317171145998846216, 1.137751157100845623 ) ) ;
#181787 = CARTESIAN_POINT ( 'NONE',  ( 2.347533153460546806, 5.890539112345938300, 0.000000000000000000 ) ) ;
#181788 = CARTESIAN_POINT ( 'NONE',  ( 0.2562055958934654210, -1.961350414083770977, -0.05204156388862594962 ) ) ;
#181789 = CARTESIAN_POINT ( 'NONE',  ( 1.364683531249986537, -0.5739583329919174526, 0.7879004041258500513 ) ) ;
#181790 = CARTESIAN_POINT ( 'NONE',  ( -0.4000000000000118461, 3.372708439410149417, -0.5000000000000247580 ) ) ;
#181792 = EDGE_CURVE ( 'NONE', #93109, #182484, #61424, .T. ) ;
#181791 = CARTESIAN_POINT ( 'NONE',  ( 5.506754051192107369, 1.639644015412666800, -1.408845030788405506 ) ) ;
#181793 = CARTESIAN_POINT ( 'NONE',  ( -2.625475302540713152, 6.214804952939456228, -0.7998128361456281477 ) ) ;
#181794 = CARTESIAN_POINT ( 'NONE',  ( -7.009202228140755331, 8.240119356661432803, -1.082531754730543083 ) ) ;
#181795 = AXIS2_PLACEMENT_3D ( 'NONE', #126917, #44530, #94354 ) ;
#181796 = CARTESIAN_POINT ( 'NONE',  ( 4.821240550277555492, -0.1094919189667045711, 2.159058991224649393 ) ) ;
#181798 = ORIENTED_EDGE ( 'NONE', *, *, #175858, .T. ) ;
#181797 = CARTESIAN_POINT ( 'NONE',  ( -5.320648938720212051, 5.172121614787156929, 0.000000000000000000 ) ) ;
#181799 = CARTESIAN_POINT ( 'NONE',  ( -1.364683531250012516, 3.280208333674756727, 0.7879004041258379498 ) ) ;
#181800 = CARTESIAN_POINT ( 'NONE',  ( 5.501234710350423107, 1.610096860432849830, 1.137200068526170060 ) ) ;
#181801 = CARTESIAN_POINT ( 'NONE',  ( 5.553917692138156781, 1.528130387303320514, -0.8190655202615308994 ) ) ;
#181803 = CARTESIAN_POINT ( 'NONE',  ( 2.331793494658142230, 1.030094174309360344, -1.934364310732391345 ) ) ;
#181802 = CARTESIAN_POINT ( 'NONE',  ( 1.360316468749967589, -0.2552083329918390930, 0.7853790794158500566 ) ) ;
#181804 = CARTESIAN_POINT ( 'NONE',  ( 3.118547318853508887, -1.136067310315771905, -2.008477146686512782 ) ) ;
#181805 = CARTESIAN_POINT ( 'NONE',  ( 4.552062217129227761, 2.060418430787996691, -0.04653940209857834048 ) ) ;
#181806 = CARTESIAN_POINT ( 'NONE',  ( 0.4275465750286939204, 0.9991681100989335818, -1.665045846455282863 ) ) ;
#181807 = CARTESIAN_POINT ( 'NONE',  ( -5.978782553502159480, 8.958701498185728695, 1.082531754730548412 ) ) ;
#181808 = AXIS2_PLACEMENT_3D ( 'NONE', #205168, #122979, #54672 ) ;
#181809 = CARTESIAN_POINT ( 'NONE',  ( -3.871735385154307263, 6.674719161725423788, -1.199719254218450271 ) ) ;
#181810 = DIRECTION ( 'NONE',  ( 0.000000000000000000, -1.000000000000000000, 0.000000000000000000 ) ) ;
#181811 = CARTESIAN_POINT ( 'NONE',  ( 4.465154236216789307, -1.701427117168831549, 1.265499569954648962 ) ) ;
#181812 = CARTESIAN_POINT ( 'NONE',  ( 1.143204175302305670, 0.8197749522141674072, 1.842446510343001442 ) ) ;
#181813 = CARTESIAN_POINT ( 'NONE',  ( -5.707619481228814351, 9.602713794834864203, -0.7216878364870207285 ) ) ;
#181814 = CARTESIAN_POINT ( 'NONE',  ( 4.911249081476436018, 1.917979745144289261, 1.091307337132418454 ) ) ;
#181815 = CARTESIAN_POINT ( 'NONE',  ( -3.285556943750000070, -1.596874999522043037, 0.000000000000000000 ) ) ;
#181816 = CARTESIAN_POINT ( 'NONE',  ( 3.475000000000000533, -1.881249999044085186, 0.000000000000000000 ) ) ;
#181817 = FACE_OUTER_BOUND ( 'NONE', #80329, .T. ) ;
#181818 = CARTESIAN_POINT ( 'NONE',  ( -9.500338091956020747, -7.818966704647505317, -0.03919461954075445509 ) ) ;
#181820 = CARTESIAN_POINT ( 'NONE',  ( 6.825078400183550720, 7.629137130509051623, 2.844348168701658075 ) ) ;
#181819 = CARTESIAN_POINT ( 'NONE',  ( -5.143355005462953322, 7.892534720870457043, -1.245665949277234841 ) ) ;
#181821 = CARTESIAN_POINT ( 'NONE',  ( 0.01837953348866276301, 7.054063922337711290, 3.955400951015632938 ) ) ;
#181822 = ORIENTED_EDGE ( 'NONE', *, *, #87194, .F. ) ;
#181823 = CARTESIAN_POINT ( 'NONE',  ( 3.573166805712838734, 0.05218571934602388163, -2.060405206736420247 ) ) ;
#181824 = CARTESIAN_POINT ( 'NONE',  ( -1.360316468750056851, 1.369791667008064540, -0.7853790794159101196 ) ) ;
#181825 = CARTESIAN_POINT ( 'NONE',  ( -5.392392409933270514, 7.314210449720692786, 1.599625672291269396 ) ) ;
#181826 = CARTESIAN_POINT ( 'NONE',  ( 3.070967880043346199, -1.527814596969854000, 1.321012706414641524 ) ) ;
#181827 = CARTESIAN_POINT ( 'NONE',  ( -1.402160292154681736E-14, 0.08750000000001964540, -1.732050807568870754 ) ) ;
#181828 = CARTESIAN_POINT ( 'NONE',  ( 3.816783937446950770, 4.411668334231586996, 1.199719254218464037 ) ) ;
#181829 = CARTESIAN_POINT ( 'NONE',  ( 3.221608841920938993, -1.986550002599724252, 0.5482939856576442006 ) ) ;
#181830 = CARTESIAN_POINT ( 'NONE',  ( -4.243338890952904841, 5.973648010910253880, -1.443375672974051449 ) ) ;
#181831 = CARTESIAN_POINT ( 'NONE',  ( 6.179819089730593795, 6.104210447640811665, 1.040834085586084257E-14 ) ) ;
#181832 = CARTESIAN_POINT ( 'NONE',  ( -0.1408020194049912077, 0.6951682901239358836, -2.180991432481160341 ) ) ;
#181833 = CARTESIAN_POINT ( 'NONE',  ( 1.200829095903386046, -0.4490931065196464012, 1.785404219219708377 ) ) ;
#181834 = CARTESIAN_POINT ( 'NONE',  ( 0.1711457161924005987, -1.502117798334397403, 1.751973695569712497 ) ) ;
#181835 = CARTESIAN_POINT ( 'NONE',  ( 6.710359684120930091, 6.793450817754725257, 0.7998128361456352531 ) ) ;
#181836 = CARTESIAN_POINT ( 'NONE',  ( 2.020999711022552159, 2.016103727727487804, 0.7800470891412072394 ) ) ;
#181837 = CARTESIAN_POINT ( 'NONE',  ( -2.819732761962332024, 6.233512622357263666, -0.7216878364870267237 ) ) ;
#181838 = CARTESIAN_POINT ( 'NONE',  ( 2.149625371984189126, 1.976669504256656218, -0.3981124878784659815 ) ) ;
#181839 = EDGE_CURVE ( 'NONE', #66830, #212186, #120974, .T. ) ;
#181840 = DIRECTION ( 'NONE',  ( -3.330669073875478496E-16, 1.665334536937734318E-16, 1.000000000000000000 ) ) ;
#181841 = CARTESIAN_POINT ( 'NONE',  ( 0.5494049127674709432, 0.5909524230637287490, -1.774924738581270089 ) ) ;
#181842 = CARTESIAN_POINT ( 'NONE',  ( -4.274563570058511175, 8.209017608368725405, 0.000000000000000000 ) ) ;
#181843 = CARTESIAN_POINT ( 'NONE',  ( 4.293796034307355569, -0.7555264168055545460, 1.821139111365249308 ) ) ;
#181844 = CARTESIAN_POINT ( 'NONE',  ( 5.120327457147888950, 1.987497208294352280, 0.3399611521368098854 ) ) ;
#181846 = CARTESIAN_POINT ( 'NONE',  ( 9.531018800282605952, 11.18223869082697597, 1.082531754730548412 ) ) ;
#181845 = CARTESIAN_POINT ( 'NONE',  ( -0.6823417656250003738, 2.217708333674753174, -1.181850606188749264 ) ) ;
#181848 = CARTESIAN_POINT ( 'NONE',  ( 6.340466044077378349, 2.082889313809291654, 0.3107213310214774760 ) ) ;
#181847 = CARTESIAN_POINT ( 'NONE',  ( -8.037286134802835491, 8.271255333558444889, -0.7998128361456291469 ) ) ;
#181849 = CARTESIAN_POINT ( 'NONE',  ( 4.826661161267837841, -1.354893614093263254, 1.565527137264411728 ) ) ;
#181850 = CARTESIAN_POINT ( 'NONE',  ( 7.983053520348166288, 8.207983950027992748, -0.7998128361456281477 ) ) ;
#181851 = CARTESIAN_POINT ( 'NONE',  ( -7.413611068574208041, 7.543634422958360730, 0.7998128361456341429 ) ) ;
#181852 = CARTESIAN_POINT ( 'NONE',  ( 1.906195883197611129, 3.231669652568789353, -0.4612786727878129822 ) ) ;
#181853 = CARTESIAN_POINT ( 'NONE',  ( 4.974870412032891487, -1.460018184141493647, 1.395898791055903976 ) ) ;
#181854 = CARTESIAN_POINT ( 'NONE',  ( 0.7499999999999867883, -1.152083332650516434, -1.299038105676652011 ) ) ;
#181855 = CARTESIAN_POINT ( 'NONE',  ( 3.616130377633751003, -2.273733826016415716, 0.3936331181264277612 ) ) ;
#181856 = EDGE_CURVE ( 'NONE', #167726, #123196, #98160, .T. ) ;
#181857 = CARTESIAN_POINT ( 'NONE',  ( 1.323174825800084609, -1.862915942116917689, -0.8856262590048938899 ) ) ;
#181858 = CARTESIAN_POINT ( 'NONE',  ( 9.110716038703335684, 9.731516254683127087, -0.7216878364870197293 ) ) ;
#181859 = CARTESIAN_POINT ( 'NONE',  ( 7.015418140428412386, 7.149352350113456822, 0.7998128361456331437 ) ) ;
#181860 = CARTESIAN_POINT ( 'NONE',  ( 5.550083779947807550, 7.568460058062819407, -1.599625672291283607 ) ) ;
#181861 = CARTESIAN_POINT ( 'NONE',  ( -1.364683531250012516, 0.5927083336747520637, 0.7879004041258379498 ) ) ;
#181862 = CARTESIAN_POINT ( 'NONE',  ( 3.867818961648523235, 7.734482231890414283, 1.040834085586084257E-14 ) ) ;
#181863 = CARTESIAN_POINT ( 'NONE',  ( 6.846504384776753049, 9.010674420371453053, -1.443375672974058777 ) ) ;
#181865 = CARTESIAN_POINT ( 'NONE',  ( -6.181864745680308637, 5.311701037653689284, -2.438145240001343250 ) ) ;
#181864 = CARTESIAN_POINT ( 'NONE',  ( 3.719319017856066445, -1.913190415241170728, -1.026542932298198485 ) ) ;
#181866 = CARTESIAN_POINT ( 'NONE',  ( 0.4499999999999851341, 4.000000000000003553, 0.8338124244295520571 ) ) ;
#181868 = CARTESIAN_POINT ( 'NONE',  ( 2.612652284633736777, -0.1782932461553646819, 1.832575692395449485 ) ) ;
#181867 = CARTESIAN_POINT ( 'NONE',  ( -5.260200412422220140, 5.239248024021764039, -0.7216878364870207285 ) ) ;
#181869 = CARTESIAN_POINT ( 'NONE',  ( -0.6823417656250212460, 5.051041667008086655, 1.181850606188767472 ) ) ;
#181870 = CARTESIAN_POINT ( 'NONE',  ( 4.757479570170550787, 2.167726397749652367, -0.3216086267831194112 ) ) ;
#181871 = CARTESIAN_POINT ( 'NONE',  ( 7.323366971182228902, 14.46633393321924999, 9.509224143632334147 ) ) ;
#181872 = CARTESIAN_POINT ( 'NONE',  ( 5.366221907327076046, 1.110187712879026956, 1.971344288924305799 ) ) ;
#181873 = CARTESIAN_POINT ( 'NONE',  ( -4.695925055628692668, 7.055611427533158064, -1.405632220554285272 ) ) ;
#181874 = CARTESIAN_POINT ( 'NONE',  ( 4.722521264130603136, 8.336029038342307018, -0.7037175076533495055 ) ) ;
#181875 = CARTESIAN_POINT ( 'NONE',  ( -6.753369912938502750, 7.051555451282599307, 0.000000000000000000 ) ) ;
#181876 = CARTESIAN_POINT ( 'NONE',  ( 3.594320121398666856, 7.207474218358159490, -1.734723475976807094E-15 ) ) ;
#181877 = CARTESIAN_POINT ( 'NONE',  ( 6.696582006438861256, -0.4751199114862921791, -1.704715723353955381 ) ) ;
#181878 = CARTESIAN_POINT ( 'NONE',  ( 3.703774327200870076, 1.459685083667804362, 1.386552827976398339 ) ) ;
#181879 = CARTESIAN_POINT ( 'NONE',  ( 6.096362627639171805, 10.26417349888772179, -0.7998128361456291469 ) ) ;
#181880 = CARTESIAN_POINT ( 'NONE',  ( 3.171027762369707848, -1.945216043820027663, -0.8074606443248407706 ) ) ;
#181881 = CARTESIAN_POINT ( 'NONE',  ( 0.5443723441289443077, -1.386745921179835417, 1.321778134454040687 ) ) ;
#181883 = EDGE_CURVE ( 'NONE', #169854, #7144, #184549, .T. ) ;
#181882 = CARTESIAN_POINT ( 'NONE',  ( 2.686486993802192913, 6.285985259411197568, 0.7998128361456362523 ) ) ;
#181884 = CARTESIAN_POINT ( 'NONE',  ( 1.680066331807037905, -1.091455746017004014, -1.639250758224161775 ) ) ;
#181885 = CARTESIAN_POINT ( 'NONE',  ( 0.8482696660519238874, 0.5391449902514727777, 1.791282564952957124 ) ) ;
#181886 = CARTESIAN_POINT ( 'NONE',  ( 1.082386330805637398, 1.171445227557347923, -1.573568114121715933 ) ) ;
#181888 = ORIENTED_EDGE ( 'NONE', *, *, #148090, .T. ) ;
#181887 = CARTESIAN_POINT ( 'NONE',  ( 0.4746845637013075159, -1.383529810647101455, 1.320479256824915071 ) ) ;
#181889 = CARTESIAN_POINT ( 'NONE',  ( 4.961921032921539521, 7.772363057508363759, -1.082531754730549078 ) ) ;
#181890 = CARTESIAN_POINT ( 'NONE',  ( -1.364683531250012516, 1.342708333674755616, 0.7879004041258379498 ) ) ;
#181892 = CARTESIAN_POINT ( 'NONE',  ( 6.262560305340551636, -1.321439916381482060, 1.324322166508178356 ) ) ;
#181891 = AXIS2_PLACEMENT_3D ( 'NONE', #42793, #23285, #92612 ) ;
#181893 = CARTESIAN_POINT ( 'NONE',  ( 10.85277107007934205, 3.956598013261175772, -3.932872935640606915 ) ) ;
#181894 = CARTESIAN_POINT ( 'NONE',  ( -1.806654366501805775, 0.000000000000000000, 2.500000000000000444 ) ) ;
#181895 = DIRECTION ( 'NONE',  ( 0.000000000000000000, 0.000000000000000000, 1.000000000000000000 ) ) ;
#181896 = CARTESIAN_POINT ( 'NONE',  ( 1.293514844328220281, -1.872496763586928514, 0.8835221827151735763 ) ) ;
#181898 = CARTESIAN_POINT ( 'NONE',  ( -0.7500000000000006661, 2.108333333333357817, -1.299038105676652011 ) ) ;
#181897 = COLOUR_RGB ( '', 0.08235294, 0.09019608, 0.10196078) ;
#181899 = CARTESIAN_POINT ( 'NONE',  ( 5.615048174354031474, 9.702639970055050966, 0.7998128361456462443 ) ) ;
#181900 = CARTESIAN_POINT ( 'NONE',  ( -9.040589502214116280, 9.441775928871617651, 0.7998128361456462443 ) ) ;
#181901 = CARTESIAN_POINT ( 'NONE',  ( 5.890091390494168522, 5.836471141856793388, 0.000000000000000000 ) ) ;
#181903 = EDGE_CURVE ( 'NONE', #212637, #93781, #111978, .T. ) ;
#181902 = CARTESIAN_POINT ( 'NONE',  ( 5.145234815219777325, 0.1564148900096741512, 2.114790009947895122 ) ) ;
#181904 = CARTESIAN_POINT ( 'NONE',  ( 5.422335090822693715, 5.290755458906732933, 0.000000000000000000 ) ) ;
#181905 = CARTESIAN_POINT ( 'NONE',  ( 0.6823417656249899377, 1.592708333674752730, 1.181850606188755259 ) ) ;
#181906 = ORIENTED_EDGE ( 'NONE', *, *, #178529, .T. ) ;
#181907 = ADVANCED_FACE ( 'NONE', ( #184456 ), #103175, .T. ) ;
#181908 = CARTESIAN_POINT ( 'NONE',  ( 1.499999999999989120, 3.004166666666689522, 0.8660254037844524744 ) ) ;
#181910 = CARTESIAN_POINT ( 'NONE',  ( 2.849184837166184536, 6.475799410002530898, 0.7998128361456362523 ) ) ;
#181909 = CARTESIAN_POINT ( 'NONE',  ( 6.531700620877029628, 1.877769495358465157, -0.5682946464737671510 ) ) ;
#181911 = CARTESIAN_POINT ( 'NONE',  ( 3.339220083777879378, -1.203169880011810022, 1.617570133648409847 ) ) ;
#181912 = CARTESIAN_POINT ( 'NONE',  ( 3.819475811356612738, -1.325201190313522792, -1.383632964731799531 ) ) ;
#181913 = CARTESIAN_POINT ( 'NONE',  ( -1.910130646976128110, 3.278792710263301657, -0.4195261609911116740 ) ) ;
#181914 = CARTESIAN_POINT ( 'NONE',  ( 1.540847765565691807, -1.849059859674206496, 1.176127931831471907 ) ) ;
#181915 = CARTESIAN_POINT ( 'NONE',  ( 1.852123800559039468, 0.000000000000000000, 0.4894596299587841703 ) ) ;
#181916 = CARTESIAN_POINT ( 'NONE',  ( 3.409304255485625657, -0.3681080166235695117, 1.833790788056933962 ) ) ;
#181917 = CARTESIAN_POINT ( 'NONE',  ( 1.499999999999987121, -0.2145833326505137972, 0.8660254037844524744 ) ) ;
#181918 = CARTESIAN_POINT ( 'NONE',  ( 4.658451966079163675, 2.008086622728368464, 0.1439865329972197516 ) ) ;
#181919 = APPLICATION_CONTEXT ( 'automotive_design' ) ;
#181920 = CARTESIAN_POINT ( 'NONE',  ( -7.344766530301162000, 9.591980256816594164, 1.599625672291295375 ) ) ;
#181922 = CARTESIAN_POINT ( 'NONE',  ( 6.151990787553828888, 1.088749021807510431, 1.815729776765177661 ) ) ;
#181921 = CARTESIAN_POINT ( 'NONE',  ( -4.772106882330247046, 4.669805572247793357, -0.7216878364870207285 ) ) ;
#181923 = CARTESIAN_POINT ( 'NONE',  ( -4.858757509019071996, 5.629766575900002401, 7.500000000000000000 ) ) ;
#181924 = FACE_OUTER_BOUND ( 'NONE', #41578, .T. ) ;
#181926 = DIRECTION ( 'NONE',  ( 1.000000000000000000, 0.000000000000000000, 0.000000000000000000 ) ) ;
#181925 = CARTESIAN_POINT ( 'NONE',  ( 2.648082478619179003, 0.7070732986501033768, 1.967675578925948354 ) ) ;
#181928 = VERTEX_POINT ( 'NONE', #183400 ) ;
#181927 = CARTESIAN_POINT ( 'NONE',  ( 0.2524154375680361939, -1.389930774942317759, 1.021034751394875428 ) ) ;
#181929 = CARTESIAN_POINT ( 'NONE',  ( 7.623762449586013901, 7.788811034138823253, 1.040834085586084257E-14 ) ) ;
#181930 = CARTESIAN_POINT ( 'NONE',  ( 8.396038884180011763, 15.16511954447424593, 8.575115785561168380 ) ) ;
#181931 = CARTESIAN_POINT ( 'NONE',  ( -0.08506230894392234620, -9.914238990527385553, -9.499619272424258298 ) ) ;
#181932 = CARTESIAN_POINT ( 'NONE',  ( -10.30047605039691128, 4.688744718740807116, 5.507884344589919934 ) ) ;
#181933 = CARTESIAN_POINT ( 'NONE',  ( 6.521108698048765362, 8.631046119188804155, -1.443375672974058777 ) ) ;
#181934 = CARTESIAN_POINT ( 'NONE',  ( -11.89942855770814134, 11.37999999999999901, 0.6999999999999992895 ) ) ;
#181936 = CARTESIAN_POINT ( 'NONE',  ( 0.6447925058646056806, 0.1317677938489550116, 1.806752140514777283 ) ) ;
#181935 = CARTESIAN_POINT ( 'NONE',  ( 4.857564175446106525, 8.889184981320973122, 0.7998128361456331437 ) ) ;
#181938 = CARTESIAN_POINT ( 'NONE',  ( -5.696397096036042385, 9.797547045350714967, -0.7998128361456231517 ) ) ;
#181937 = CIRCLE ( 'NONE', #64298, 3.099999999999999201 ) ;
#181939 = CARTESIAN_POINT ( 'NONE',  ( 4.355193658487811703, 6.104145239700998538, -1.599625672291255185 ) ) ;
#181940 = CARTESIAN_POINT ( 'NONE',  ( -5.998939594393441155, 7.096481464931535754, 1.069142741232721461 ) ) ;
#181941 = CARTESIAN_POINT ( 'NONE',  ( 5.013482942003290255, 9.071090208970993274, -0.7998128361456481317 ) ) ;
#181942 = CARTESIAN_POINT ( 'NONE',  ( 6.639320575229231025, 3.706874577532508486, 2.311316081152973823 ) ) ;
#181943 = DIRECTION ( 'NONE',  ( -0.000000000000000000, 1.000000000000000000, -0.000000000000000000 ) ) ;
#181944 = CARTESIAN_POINT ( 'NONE',  ( 4.037125735401803084, 7.543859425723234757, -0.4173421496808590869 ) ) ;
#181945 = CARTESIAN_POINT ( 'NONE',  ( 8.568389894156670294, 12.94027927658408217, -0.7216878364870257245 ) ) ;
#181946 = ORIENTED_EDGE ( 'NONE', *, *, #198939, .F. ) ;
#181947 = CARTESIAN_POINT ( 'NONE',  ( 2.857670863715315424, -0.5868061553097079219, 1.766171933019081042 ) ) ;
#181948 = CARTESIAN_POINT ( 'NONE',  ( -0.1236200418614826352, -0.4170706148690634385, -1.876090511053402965 ) ) ;
#181949 = CARTESIAN_POINT ( 'NONE',  ( 6.176777841581622575, -1.829441475422811436, -0.6035904912435466896 ) ) ;
#181950 = CARTESIAN_POINT ( 'NONE',  ( -1.846004154127505403, 8.940320519588478732, 0.7750000000000013545 ) ) ;
#181951 = CIRCLE ( 'NONE', #199258, 0.07999999999999994615 ) ;
#181952 = CARTESIAN_POINT ( 'NONE',  ( 4.893454165248502186, 8.027304163657891678, -0.9628252682179049282 ) ) ;
#181953 = CARTESIAN_POINT ( 'NONE',  ( -11.41381675112460670, 11.03016735491473810, 3.704697986577268232 ) ) ;
#181954 = CARTESIAN_POINT ( 'NONE',  ( -2.982430605326321427, 6.423326772948587227, -0.7216878364870267237 ) ) ;
#181955 = CARTESIAN_POINT ( 'NONE',  ( 7.917598520700710019, 12.18102267421877727, -0.7216878364870328300 ) ) ;
#181956 = CARTESIAN_POINT ( 'NONE',  ( 4.451979310445155491, -0.7576744193203123201, 1.818072383216073007 ) ) ;
#181957 = CARTESIAN_POINT ( 'NONE',  ( 1.278162280329109279, 2.088516533416693743, -0.3659721813360562459 ) ) ;
#181958 = CARTESIAN_POINT ( 'NONE',  ( -4.934277840369690971, 7.844075682818238526, -1.199719254218452047 ) ) ;
#181959 = DIRECTION ( 'NONE',  ( 5.578564026256490882E-16, 1.000000000000000000, 9.066213480720158442E-32 ) ) ;
#181960 = CARTESIAN_POINT ( 'NONE',  ( 0.9311234436981579154, -2.553130369558483270, -3.474999999999996536 ) ) ;
#181961 = VECTOR ( 'NONE', #188695, 1000.000000000000000 ) ;
#181962 = CARTESIAN_POINT ( 'NONE',  ( 6.193348084369689310, -0.7418380161853586063, 2.062208804312585020 ) ) ;
#181963 = CARTESIAN_POINT ( 'NONE',  ( 4.723400270955312230, 6.733595400378874274, 1.377748641254195716 ) ) ;
#181964 = CARTESIAN_POINT ( 'NONE',  ( 3.873980538081963854, 1.069312750484844088, 1.602167800089354222 ) ) ;
#181965 = CARTESIAN_POINT ( 'NONE',  ( -5.910464900553636269, 8.982960586366182554, -1.199719254218440723 ) ) ;
#181966 = CARTESIAN_POINT ( 'NONE',  ( 1.541937560865791479, -1.600244427420342896, -1.519961040588948986 ) ) ;
#181967 = DIRECTION ( 'NONE',  ( -1.000000000000000000, 5.782411586589355667E-16, 0.000000000000000000 ) ) ;
#181968 = ORIENTED_EDGE ( 'NONE', *, *, #16746, .F. ) ;
#181969 = FACE_OUTER_BOUND ( 'NONE', #89689, .T. ) ;
#181970 = ORIENTED_EDGE ( 'NONE', *, *, #70055, .T. ) ;
#181971 = CARTESIAN_POINT ( 'NONE',  ( 5.946149452469858154, -0.8887192358506822432, 1.757629817417952767 ) ) ;
#181972 = CARTESIAN_POINT ( 'NONE',  ( 1.874458991091961568, -0.09742729390963811298, -1.939748921942837878 ) ) ;
#181973 = CARTESIAN_POINT ( 'NONE',  ( 0.1751529202326657098, -0.8592662624449104447, -1.822031250676876768 ) ) ;
#181975 = CARTESIAN_POINT ( 'NONE',  ( 3.889374201350876525, -1.720966249256241865, 0.7085912657165122086 ) ) ;
#181974 = CARTESIAN_POINT ( 'NONE',  ( -7.632314129850253259, 7.869064337772231355, 0.7998128361456341429 ) ) ;
#181976 = CARTESIAN_POINT ( 'NONE',  ( 7.038618024149998043, 8.240751112043669835, -1.199719254218452047 ) ) ;
#181977 = CARTESIAN_POINT ( 'NONE',  ( 2.449293598294706414E-16, 5.499999999999998224, 2.000000000000000000 ) ) ;
#181978 = CARTESIAN_POINT ( 'NONE',  ( 1.436838838544550523, 7.449283400311791148, -4.203727439823577328 ) ) ;
#181979 = CARTESIAN_POINT ( 'NONE',  ( -6.715366157470410435, 6.729015360003925750, -0.7998128361456291469 ) ) ;
#181980 = EDGE_CURVE ( 'NONE', #49964, #95100, #139599, .T. ) ;
#181981 = CARTESIAN_POINT ( 'NONE',  ( 0.4686481397476391364, -2.065551408369214137, -0.7328327568804984260 ) ) ;
#181982 = CARTESIAN_POINT ( 'NONE',  ( 4.528060117284232966, 6.305822774963486310, 1.443375672974062551 ) ) ;
#181983 = CARTESIAN_POINT ( 'NONE',  ( -2.788906526875773208E-15, 12.46875000068279782, -1.499999999999998446 ) ) ;
#181984 = DIRECTION ( 'NONE',  ( 0.6507913734559641616, -0.7592566023653004592, 0.000000000000000000 ) ) ;
#181985 = CARTESIAN_POINT ( 'NONE',  ( 1.664397423953474009, -1.292156093668932693, 1.290017532847971271 ) ) ;
#181986 = CARTESIAN_POINT ( 'NONE',  ( -3.815730167242251003, 6.539103397502874948, -1.199719254218452047 ) ) ;
#181987 = CARTESIAN_POINT ( 'NONE',  ( 3.322662972295143291, 0.7760272377477626105, -1.550874960589002871 ) ) ;
#181988 = CARTESIAN_POINT ( 'NONE',  ( 0.1054570145121075109, 2.614151819895196294, -2.076146791065091701 ) ) ;
#181989 = CARTESIAN_POINT ( 'NONE',  ( 6.609000000000042618, 6.036791015687303918, 2.594900324319386886 ) ) ;
#181990 = CARTESIAN_POINT ( 'NONE',  ( 6.164658409365947556, -1.287482145768016339, 1.294691480910937775 ) ) ;
#181991 = CARTESIAN_POINT ( 'NONE',  ( 4.979329090789969214, -0.1002203015587413149, 1.959344625532564610 ) ) ;
#181992 = CARTESIAN_POINT ( 'NONE',  ( -7.181014916732457287, 11.52960116949655678, -0.7998128361456291469 ) ) ;
#181993 = CARTESIAN_POINT ( 'NONE',  ( 4.801558957534076022, 8.753569217098425170, 0.7998128361456462443 ) ) ;
#181994 = CARTESIAN_POINT ( 'NONE',  ( 4.793665170694914046, 1.978287127071875151, -0.7638792978137475265 ) ) ;
#181995 = EDGE_CURVE ( 'NONE', #86578, #205093, #187660, .T. ) ;
#181996 = CARTESIAN_POINT ( 'NONE',  ( -8.833300774503376473, 10.26427131079744193, 1.199719254218462483 ) ) ;
#181997 = DIRECTION ( 'NONE',  ( 0.000000000000000000, 0.000000000000000000, 1.000000000000000000 ) ) ;
#181998 = CARTESIAN_POINT ( 'NONE',  ( 2.377862429009020229, -2.009158356589606953, 0.4988364127441884399 ) ) ;
#182000 = CARTESIAN_POINT ( 'NONE',  ( -1.364683531250014514, -0.6572916663252459379, 0.7879004041258379498 ) ) ;
#181999 = CARTESIAN_POINT ( 'NONE',  ( 6.520158902582592120, 5.290451655907108197, -2.438235897557449849 ) ) ;
#182001 = ORIENTED_EDGE ( 'NONE', *, *, #48333, .T. ) ;
#182002 = CARTESIAN_POINT ( 'NONE',  ( 3.270466940867942984, 2.077131924838520050, -0.9849289250120364381 ) ) ;
#182003 = CARTESIAN_POINT ( 'NONE',  ( 9.436111725431318931, 10.11114455586577776, -0.7216878364870257245 ) ) ;
#182005 = CARTESIAN_POINT ( 'NONE',  ( 1.001543065824772753E-15, -3.171874999522042327, 3.793834371823811669 ) ) ;
#182004 = CARTESIAN_POINT ( 'NONE',  ( 5.397554552016212703, 8.350878506444006533, 1.082531754730547524 ) ) ;
#182006 =( LENGTH_UNIT ( ) NAMED_UNIT ( * ) SI_UNIT ( .MILLI., .METRE. ) );
#182007 = ORIENTED_EDGE ( 'NONE', *, *, #98017, .F. ) ;
#182008 = CARTESIAN_POINT ( 'NONE',  ( -2.331034670843834533E-15, -6.920331743278509862, 9.905860218026841579 ) ) ;
#182009 = CARTESIAN_POINT ( 'NONE',  ( 4.359561026920276916, -1.481784043772149229, -1.208992945495937610 ) ) ;
#182010 = DIRECTION ( 'NONE',  ( 1.000000000000000000, 0.000000000000000000, -2.345077562848777574E-16 ) ) ;
#182011 = CARTESIAN_POINT ( 'NONE',  ( 5.772382705887088683, -1.090832958316660273, 1.335977363661453809 ) ) ;
#182012 = CARTESIAN_POINT ( 'NONE',  ( 3.801970467005914678, -1.040791964576088358, -1.727064642965264740 ) ) ;
#182013 = CARTESIAN_POINT ( 'NONE',  ( 4.887441975664971849, -0.7727101442582262614, -2.165022144963870243 ) ) ;
#182014 = CARTESIAN_POINT ( 'NONE',  ( -11.48784849554596121, 12.26950472818065663, -3.469614872287748231 ) ) ;
#182015 = CARTESIAN_POINT ( 'NONE',  ( 1.278255639411193245, 1.316999024263129092, 1.770685722221450709 ) ) ;
#182016 = CARTESIAN_POINT ( 'NONE',  ( -5.207740401424942434, 6.208690235484773723, 1.082531754730549078 ) ) ;
#182017 = CARTESIAN_POINT ( 'NONE',  ( 5.430809967973590169, 0.1307738731834498513, 1.764929826691101100 ) ) ;
#182018 = PRESENTATION_LAYER_ASSIGNMENT (  '', '', ( #140649 ) ) ;
#182020 = CARTESIAN_POINT ( 'NONE',  ( 2.326505592738498329, 2.223965110380062615, 0.5549310701656160472 ) ) ;
#182019 = CARTESIAN_POINT ( 'NONE',  ( 6.333594036239346359, 7.418223126147930557, 1.199719254218453823 ) ) ;
#182021 = CARTESIAN_POINT ( 'NONE',  ( -0.02397475188680147154, -0.1303385410800334265, -1.711279094490937069 ) ) ;
#182022 = CARTESIAN_POINT ( 'NONE',  ( -6.583366107887490770, 9.838288338247510367, 1.199719254218452935 ) ) ;
#182023 = DIRECTION ( 'NONE',  ( -0.000000000000000000, -1.000000000000000000, -0.000000000000000000 ) ) ;
#182024 = CARTESIAN_POINT ( 'NONE',  ( -4.329849954717889915, 6.144853928627882489, 1.599625672291270506 ) ) ;
#182025 = FACE_OUTER_BOUND ( 'NONE', #34178, .T. ) ;
#182026 = DIRECTION ( 'NONE',  ( 8.659560562354853972E-17, -0.7071067811865540120, 0.7071067811865410224 ) ) ;
#182027 =( BOUNDED_CURVE ( )  B_SPLINE_CURVE ( 2, ( #82324, #198201, #163603, #14113, #15185 ),
 .UNSPECIFIED., .F., .T. ) 
 B_SPLINE_CURVE_WITH_KNOTS ( ( 3, 2, 3 ),
 ( 0.1229971016045081911, 0.1250000000000000000, 0.1273350245274847969 ),
 .UNSPECIFIED. ) 
 CURVE ( )  GEOMETRIC_REPRESENTATION_ITEM ( )  RATIONAL_B_SPLINE_CURVE ( ( 0.9331125556462563919, 0.9355989990887654262, 1.000000000000000000, 0.9249198476264304247, 0.9339904139662593696 ) ) 
 REPRESENTATION_ITEM ( '' )  );
#182028 = CARTESIAN_POINT ( 'NONE',  ( 0.7487581336349375949, -2.154818914559033072, -0.2656684361399003214 ) ) ;
#182029 = CARTESIAN_POINT ( 'NONE',  ( 1.780482797753998092, -0.5424726148271253878, -1.942096288550937411 ) ) ;
#182030 = CARTESIAN_POINT ( 'NONE',  ( -1.500000000000001332, 0.4312500006828159926, 0.000000000000000000 ) ) ;
#182031 = CARTESIAN_POINT ( 'NONE',  ( 5.233004834321499210, 0.1438781470856145273, 1.921186297865638215 ) ) ;
#182032 = CARTESIAN_POINT ( 'NONE',  ( 0.6823417656249969321, 11.52604166700806765, -1.181850606188757036 ) ) ;
#182033 = CARTESIAN_POINT ( 'NONE',  ( 2.479030958227887549, -1.528377378988081015, 1.612298682912993275 ) ) ;
#182034 = ORIENTED_EDGE ( 'NONE', *, *, #48267, .T. ) ;
#182035 = CARTESIAN_POINT ( 'NONE',  ( -1.217323170181725756, 3.236755683774203085, 0.7750000000000100142 ) ) ;
#182036 = DIRECTION ( 'NONE',  ( 1.000000000000000000, 0.000000000000000000, 0.000000000000000000 ) ) ;
#182037 = CARTESIAN_POINT ( 'NONE',  ( 7.879259827836241570, 12.34422023245099176, 1.040834085586084257E-14 ) ) ;
#182038 = CARTESIAN_POINT ( 'NONE',  ( -11.84668730067608600, 19.00000000000000000, -1.320000000000001616 ) ) ;
#182039 = CARTESIAN_POINT ( 'NONE',  ( 4.265022598847971302, 1.686782405526715545, -0.4282675217706712889 ) ) ;
#182040 = CARTESIAN_POINT ( 'NONE',  ( 4.053139552913617827, 1.658577106941661272, -1.047563642765911185 ) ) ;
#182042 = CARTESIAN_POINT ( 'NONE',  ( -6.941411460516810017, 8.161030127766803588, 1.082531754730549967 ) ) ;
#182041 = CARTESIAN_POINT ( 'NONE',  ( 5.196852952739813070, 4.957416621151553571, -0.7998128361456221525 ) ) ;
#182043 = EDGE_CURVE ( 'NONE', #91680, #162762, #52343, .T. ) ;
#182044 = CARTESIAN_POINT ( 'NONE',  ( 0.000000000000000000, 0.08000000000000020983, 0.000000000000000000 ) ) ;
#182045 = CARTESIAN_POINT ( 'NONE',  ( 10.55232363013785246, 11.20546574478267132, 0.000000000000000000 ) ) ;
#182046 = AXIS2_PLACEMENT_3D ( 'NONE', #46606, #212266, #44478 ) ;
#182047 = CARTESIAN_POINT ( 'NONE',  ( 1.064971659385913316, 1.563282549206745475, -1.345778378556292676 ) ) ;
#182048 = CARTESIAN_POINT ( 'NONE',  ( -8.505042434474312074, 8.816971016508505343, -0.7998128361456291469 ) ) ;
#182049 = CARTESIAN_POINT ( 'NONE',  ( -2.928197990427299668, 6.360055388899728435, 1.040834085586084257E-14 ) ) ;
#182050 = CARTESIAN_POINT ( 'NONE',  ( 0.6907310396802420760, -2.245820052064306349, -0.2739839911451089627 ) ) ;
#182051 = VERTEX_POINT ( 'NONE', #18750 ) ;
#182052 = CARTESIAN_POINT ( 'NONE',  ( 1.499999999999989120, 0.3062500006828158816, 0.000000000000000000 ) ) ;
#182053 = CARTESIAN_POINT ( 'NONE',  ( 2.987410616422137899, 1.320145714686842497, 1.325460448179466066 ) ) ;
#182054 = CARTESIAN_POINT ( 'NONE',  ( 1.072469862579095379, -0.7803941858975007584, 1.548669665330544953 ) ) ;
#182055 = CARTESIAN_POINT ( 'NONE',  ( 5.390230798962840630, -0.5317533105795355652, -2.125930911514521959 ) ) ;
#182056 = CARTESIAN_POINT ( 'NONE',  ( 0.2181801407958559869, -2.163675782650812618, 0.4331315337846516900 ) ) ;
#182057 = CARTESIAN_POINT ( 'NONE',  ( 1.235309500465184396, -1.863545150897191416, 0.8803144705526543268 ) ) ;
#182058 = CARTESIAN_POINT ( 'NONE',  ( 2.994010707676255212, -0.5641155714235489560, -1.858205125314008832 ) ) ;
#182059 = CARTESIAN_POINT ( 'NONE',  ( -3.565431210269599749, 7.103494145382415859, 0.7216878364870317197 ) ) ;
#182060 = CARTESIAN_POINT ( 'NONE',  ( 5.659403934932580427, 0.3656299861228041737, -1.834283699791404043 ) ) ;
#182061 = CARTESIAN_POINT ( 'NONE',  ( 1.093750000000000666, -1.895863743164112547, -0.7852924748299294766 ) ) ;
#182062 = CARTESIAN_POINT ( 'NONE',  ( 0.1858884387159591145, 13.28951043065277737, 1.441950245016251575 ) ) ;
#182063 = CARTESIAN_POINT ( 'NONE',  ( 6.345077344222471716, -1.080897578067066878, 1.701688803805063266 ) ) ;
#182064 = CARTESIAN_POINT ( 'NONE',  ( -5.358255402162534516E-14, 1.328125000341439987, -1.570758158831820239 ) ) ;
#182065 = CARTESIAN_POINT ( 'NONE',  ( 4.149064681782777875, 0.9530105817698063531, 1.777011888912001014 ) ) ;
#182066 = CARTESIAN_POINT ( 'NONE',  ( -2.426546306721660606, 5.774795091243142053, 0.7216878364870317197 ) ) ;
#182067 = CARTESIAN_POINT ( 'NONE',  ( 8.772289083241844310, 10.19309100432570148, -1.199719254218446718 ) ) ;
#182068 = CARTESIAN_POINT ( 'NONE',  ( 4.740510986633625024, 5.559626234941203116, -1.199719254218450271 ) ) ;
#182070 = CARTESIAN_POINT ( 'NONE',  ( -4.167966236947438396, 7.861110150953528830, 0.1643318641706831840 ) ) ;
#182069 = CARTESIAN_POINT ( 'NONE',  ( 2.420285107995377327, 1.192830232448302441, -1.382225081888274643 ) ) ;
#182071 = DIRECTION ( 'NONE',  ( 0.000000000000000000, -1.000000000000000000, 0.000000000000000000 ) ) ;
#182072 = CARTESIAN_POINT ( 'NONE',  ( -10.33392256004288079, 4.765625372279607141, 5.445010993851796322 ) ) ;
#182073 = VERTEX_POINT ( 'NONE', #84835 ) ;
#182074 = CARTESIAN_POINT ( 'NONE',  ( -4.787437638956920871, 8.599444655509458357, -0.7216878364870338292 ) ) ;
#182075 = DIRECTION ( 'NONE',  ( 3.330669073875479482E-16, -3.330669073875479482E-16, -1.000000000000000000 ) ) ;
#182076 = CARTESIAN_POINT ( 'NONE',  ( -7.971304249830880373, 11.38727316052296601, 1.199719254218453823 ) ) ;
#182077 = CARTESIAN_POINT ( 'NONE',  ( -0.2048590494372501680, -0.1558505989666530422, -1.986559690435693026 ) ) ;
#182078 = CARTESIAN_POINT ( 'NONE',  ( 6.287741706623968696, 2.126563164181693555, -0.6417273904879957636 ) ) ;
#182079 = EDGE_CURVE ( 'NONE', #197822, #43527, #8142, .T. ) ;
#182080 = ORIENTED_EDGE ( 'NONE', *, *, #114896, .T. ) ;
#182081 = CARTESIAN_POINT ( 'NONE',  ( -5.576146316970437944, 9.727530813099326323, 0.000000000000000000 ) ) ;
#182082 = CARTESIAN_POINT ( 'NONE',  ( 5.518332215962025167, 6.396807992499198292, -1.199719254218445830 ) ) ;
#182083 = CARTESIAN_POINT ( 'NONE',  ( 6.455941844152293996, 2.055567607077302128, -0.1488206295068068841 ) ) ;
#182084 = CARTESIAN_POINT ( 'NONE',  ( 5.625625018759272677, 0.3960990390993284205, 1.976956468877195894 ) ) ;
#182085 = EDGE_LOOP ( 'NONE', ( #160384, #122646, #119546, #210443 ) ) ;
#182086 = CARTESIAN_POINT ( 'NONE',  ( 2.880374247444865254, 6.438789554985836716, 0.3607768799173494689 ) ) ;
#182087 = CARTESIAN_POINT ( 'NONE',  ( -0.6125000000000296874, 0.3541666673494772710, 1.060881119635899816 ) ) ;
#182088 = AXIS2_PLACEMENT_3D ( 'NONE', #204827, #106345, #122640 ) ;
#182089 =( BOUNDED_CURVE ( )  B_SPLINE_CURVE ( 3, ( #41829, #101730, #59111, #25541 ),
 .UNSPECIFIED., .F., .T. ) 
 B_SPLINE_CURVE_WITH_KNOTS ( ( 4, 4 ),
 ( 0.4999999999999967248, 1.000000000000000000 ),
 .UNSPECIFIED. ) 
 CURVE ( )  GEOMETRIC_REPRESENTATION_ITEM ( )  RATIONAL_B_SPLINE_CURVE ( ( 1.000000000000004663, 0.3333333333333334814, 0.3333333333333290960, 1.000000000000000222 ) ) 
 REPRESENTATION_ITEM ( '' )  );
#182091 = CARTESIAN_POINT ( 'NONE',  ( -1.284279953904132077, 3.159610286488902187, -0.7749999999999935829 ) ) ;
#182090 = CARTESIAN_POINT ( 'NONE',  ( -4.796552484184649856, 8.818004674849227342, -0.7998128361456362523 ) ) ;
#182092 = CARTESIAN_POINT ( 'NONE',  ( 4.598366155629488361, 8.485928551783258555, 0.1149073004905968448 ) ) ;
#182093 = CARTESIAN_POINT ( 'NONE',  ( 5.149767453795408123, -0.2439937967673235231, -2.001204641050558397 ) ) ;
#182094 = CARTESIAN_POINT ( 'NONE',  ( 4.734224819668921391, 0.3176365174208677367, 1.813369535050498360 ) ) ;
#182095 = CARTESIAN_POINT ( 'NONE',  ( 0.07661050522430287724, 1.422454998960010153, -1.972067596371825715 ) ) ;
#182096 = CARTESIAN_POINT ( 'NONE',  ( 2.825201024400230132, 2.173230126089547909, 0.7765846127750095640 ) ) ;
#182097 = CARTESIAN_POINT ( 'NONE',  ( 7.452141709366786770, 8.723195411463290583, 1.199719254218452047 ) ) ;
#182098 = ADVANCED_FACE ( 'NONE', ( #201757 ), #185522, .T. ) ;
#182099 = CARTESIAN_POINT ( 'NONE',  ( 5.114612887932482366, 1.494710344919391476, -1.561737693111686642 ) ) ;
#182100 = CARTESIAN_POINT ( 'NONE',  ( 6.988338112840064120, 10.24047933403371502, 1.199719254218460707 ) ) ;
#182101 = CARTESIAN_POINT ( 'NONE',  ( 1.663517674946796143, 1.000093669912437644, 1.664638661912527962 ) ) ;
#182102 = CARTESIAN_POINT ( 'NONE',  ( -5.271422797614987665, 5.044414773505913274, -0.7998128361456221525 ) ) ;
#182103 = AXIS2_PLACEMENT_3D ( 'NONE', #202318, #122259, #120103 ) ;
#182104 = CARTESIAN_POINT ( 'NONE',  ( 4.042538402956846966, 2.165829419810465950, -0.7696314825454602104 ) ) ;
#182105 = CARTESIAN_POINT ( 'NONE',  ( 2.680610894905853137, 0.4704162359921160164, -0.1034257855107231783 ) ) ;
#182106 = CARTESIAN_POINT ( 'NONE',  ( -5.829079699232685208, 5.765290835385048496, 0.000000000000000000 ) ) ;
#182107 = CARTESIAN_POINT ( 'NONE',  ( 2.922558825391399662, 1.760836971185793187, 0.6318509464167121337 ) ) ;
#182110 = CARTESIAN_POINT ( 'NONE',  ( -7.259464905474441565, 7.434073576000447048, -0.7998128361456362523 ) ) ;
#182109 = CARTESIAN_POINT ( 'NONE',  ( -1.402160292154681736E-14, -0.6312499993171797330, -1.732050807568870754 ) ) ;
#182108 = CARTESIAN_POINT ( 'NONE',  ( 1.054777118923880597, 0.3758132965740559883, 1.874924941132802836 ) ) ;
#182111 = CARTESIAN_POINT ( 'NONE',  ( 3.246891520140795517, 0.5363302883765566076, 2.140594385818309409 ) ) ;
#182112 = FACE_OUTER_BOUND ( 'NONE', #174956, .T. ) ;
#182113 = CARTESIAN_POINT ( 'NONE',  ( -3.623772196602547346, 7.449761006003425834, 0.000000000000000000 ) ) ;
#182114 = CARTESIAN_POINT ( 'NONE',  ( 4.841670253411575864, 8.662716039039905169, -0.7216878364870458196 ) ) ;
#182115 = CARTESIAN_POINT ( 'NONE',  ( -2.937312835655025101, 6.578615408239493867, 1.040834085586084257E-14 ) ) ;
#182116 = AXIS2_PLACEMENT_3D ( 'NONE', #29865, #130629, #180369 ) ;
#182117 = CARTESIAN_POINT ( 'NONE',  ( -5.912764388891193157, 9.912325863766124456, 0.000000000000000000 ) ) ;
#182118 = CARTESIAN_POINT ( 'NONE',  ( 0.7023363917650466970, -0.6599406036866415359, -1.857761218813491988 ) ) ;
#182119 = CARTESIAN_POINT ( 'NONE',  ( 0.5347316126107805045, 1.182704979252725108, -1.981343935211031138 ) ) ;
#182121 = ADVANCED_FACE ( 'NONE', ( #21931 ), #170345, .T. ) ;
#182120 = CARTESIAN_POINT ( 'NONE',  ( 1.732786548908150870, -1.861864252656076912, -0.6185235971247133868 ) ) ;
#182122 = CARTESIAN_POINT ( 'NONE',  ( 4.856332268735650715, -2.061987677746464076, -0.05593471103338721467 ) ) ;
#182123 = CARTESIAN_POINT ( 'NONE',  ( 4.351804120306567825, 8.020929207092235558, 1.040834085586084257E-14 ) ) ;
#182124 = CARTESIAN_POINT ( 'NONE',  ( 7.028976294042106332, 7.165170195996068969, 0.000000000000000000 ) ) ;
#182125 = ORIENTED_EDGE ( 'NONE', *, *, #115854, .F. ) ;
#182126 = CARTESIAN_POINT ( 'NONE',  ( 8.229436053370676518, 9.663725486096376827, 1.082531754730558626 ) ) ;
#182127 = CARTESIAN_POINT ( 'NONE',  ( 1.364683531249988535, 5.217708333674750065, -0.7879004041258300672 ) ) ;
#182128 = CARTESIAN_POINT ( 'NONE',  ( -10.16842870470028437, 3.679487716134552944, -6.373158935749277276 ) ) ;
#182129 = CARTESIAN_POINT ( 'NONE',  ( 3.023105065722948126, 6.470780310077995701, 0.7216878364870338292 ) ) ;
#182130 = CARTESIAN_POINT ( 'NONE',  ( 0.4796376738960402841, -0.1079922143863345368, 2.168524981076371372 ) ) ;
#182131 = CARTESIAN_POINT ( 'NONE',  ( 9.491602870538727643, -9.241975548351300418, -0.4178506376739458683 ) ) ;
#182132 = CARTESIAN_POINT ( 'NONE',  ( 0.000000000000000000, 0.000000000000000000, -0.4856446947087145194 ) ) ;
#182133 = CARTESIAN_POINT ( 'NONE',  ( 2.000000000000003553, 8.900000000000018119, 2.449293598294762621E-16 ) ) ;
#182134 = CARTESIAN_POINT ( 'NONE',  ( 1.053721402318724021, 1.868689351376726204, -0.08586956420430363890 ) ) ;
#182135 = CARTESIAN_POINT ( 'NONE',  ( 5.307972821619873827, -2.151738229465068653, 0.2060058040841972193 ) ) ;
#182136 = CARTESIAN_POINT ( 'NONE',  ( -6.131443063645894753, 6.000026256920684808, -0.1528826387674747100 ) ) ;
#182137 = DIRECTION ( 'NONE',  ( -0.000000000000000000, -1.000000000000000000, -0.000000000000000000 ) ) ;
#182138 = CARTESIAN_POINT ( 'NONE',  ( 5.894874513638865388, 7.262872338272549300, -1.253420816524719150 ) ) ;
#182139 = CARTESIAN_POINT ( 'NONE',  ( 1.364683531249990311, 5.426041667008086655, 0.7879004041258500513 ) ) ;
#182140 = CARTESIAN_POINT ( 'NONE',  ( 1.471198412684338486, -1.640640410176617658, -0.9821394255850326438 ) ) ;
#182141 = CARTESIAN_POINT ( 'NONE',  ( 2.606023559441010828, -0.6750964425338638053, -1.636234759011189421 ) ) ;
#182142 = CARTESIAN_POINT ( 'NONE',  ( 0.8735180803765253410, 0.3724630581584260081, -1.875478908130092215 ) ) ;
#182144 = CARTESIAN_POINT ( 'NONE',  ( 6.011341193797766103, -1.801927099207595084, 0.6504362055675115828 ) ) ;
#182143 = CARTESIAN_POINT ( 'NONE',  ( 1.905568696376195970, -3.159541454813609374, -2.771379219291199458 ) ) ;
#182145 = CARTESIAN_POINT ( 'NONE',  ( -1.402160292154681736E-14, -0.9124999999999769962, -1.732050807568870754 ) ) ;
#182146 = CARTESIAN_POINT ( 'NONE',  ( 0.1392002015415672034, -0.1474423581745692435, -2.037351525059682977 ) ) ;
#182147 = CARTESIAN_POINT ( 'NONE',  ( 1.389100911873580646, -2.015333191458138273, -0.6601287711371638389 ) ) ;
#182148 = DIRECTION ( 'NONE',  ( -1.000000000000000000, 0.000000000000000000, 0.000000000000000000 ) ) ;
#182149 = CARTESIAN_POINT ( 'NONE',  ( 3.994877460428855276, 1.580554378303768992, -1.000287695324620252 ) ) ;
#182151 = EDGE_LOOP ( 'NONE', ( #115283, #134467, #19601, #208943, #30394 ) ) ;
#182150 = CARTESIAN_POINT ( 'NONE',  ( 0.7502976729042536430, 0.5272139720400963459, 1.747899773703022408 ) ) ;
#182153 = CARTESIAN_POINT ( 'NONE',  ( 9.797921721691059460, 3.956598013261175772, 6.103348209225848642 ) ) ;
#182152 = CARTESIAN_POINT ( 'NONE',  ( 2.948105999307056635, 0.7938017206191756436, -2.059354589195587337 ) ) ;
#182154 = CARTESIAN_POINT ( 'NONE',  ( -0.6823417656250212460, 4.363541667008085767, 1.181850606188767472 ) ) ;
#182155 = CARTESIAN_POINT ( 'NONE',  ( 1.768110600389400933, -2.047337470793224146, 0.2504565381693297788 ) ) ;
#182156 = CARTESIAN_POINT ( 'NONE',  ( 5.666418135507635512, 8.698239360479199433, 1.199719254218462483 ) ) ;
#182157 = CARTESIAN_POINT ( 'NONE',  ( -8.045874094706015001, 11.47427131287732927, -1.199719254218446718 ) ) ;
#182158 = CARTESIAN_POINT ( 'NONE',  ( -8.867053104062382118, 4.021557182957048227, -7.983930475901429347 ) ) ;
#182159 = CARTESIAN_POINT ( 'NONE',  ( -3.441837234280166413, -0.01368419061246708458, -0.3627113057276946106 ) ) ;
#182160 = DIRECTION ( 'NONE',  ( 5.828670879282089587E-16, -0.8656921114426507913, 0.5005768354468322912 ) ) ;
#182161 = ORIENTED_EDGE ( 'NONE', *, *, #20526, .F. ) ;
#182162 = CARTESIAN_POINT ( 'NONE',  ( 4.158688916442685013, -0.6465363538536235133, -1.966910096795893681 ) ) ;
#182163 = CARTESIAN_POINT ( 'NONE',  ( -1.499999999999997780, 5.900000000000023448, 1.214306433183764966E-14 ) ) ;
#182164 = CARTESIAN_POINT ( 'NONE',  ( 1.546389740860309781, 2.159050155192781872, 0.1077149563947499555 ) ) ;
#182165 = CARTESIAN_POINT ( 'NONE',  ( -5.221311770390402174, 7.721201550036163042, -1.200461426208466076 ) ) ;
#182167 = EDGE_CURVE ( 'NONE', #110540, #71536, #84205, .T. ) ;
#182166 = CARTESIAN_POINT ( 'NONE',  ( 2.262373273732374290, 2.019286824851754591, 0.04726863806006965929 ) ) ;
#182168 = DIRECTION ( 'NONE',  ( 0.000000000000000000, 1.000000000000000000, 0.000000000000000000 ) ) ;
#182169 = ORIENTED_EDGE ( 'NONE', *, *, #97288, .F. ) ;
#182170 = EDGE_CURVE ( 'NONE', #26907, #138623, #167720, .T. ) ;
#182172 = CARTESIAN_POINT ( 'NONE',  ( 7.117667457494414762, 11.24776976714476184, 1.040834085586084257E-14 ) ) ;
#182171 = CARTESIAN_POINT ( 'NONE',  ( 3.475000000000000533, -2.595833333333334103, -2.006292185433951047 ) ) ;
#182173 = CARTESIAN_POINT ( 'NONE',  ( 6.802112138117927920, -1.802125342305498146, 0.9040232568291312054 ) ) ;
#182174 = CARTESIAN_POINT ( 'NONE',  ( 0.1632964843477149597, 1.879801964727344732, -0.7303121171872913875 ) ) ;
#182175 = FACE_OUTER_BOUND ( 'NONE', #19057, .T. ) ;
#182176 = CARTESIAN_POINT ( 'NONE',  ( 4.862908538974716421, 0.2148362657848034984, -2.180980218048253150 ) ) ;
#182178 = AXIS2_PLACEMENT_3D ( 'NONE', #199122, #165585, #83253 ) ;
#182177 = CARTESIAN_POINT ( 'NONE',  ( 1.499999999999989120, 3.535416667349488229, 0.8660254037844524744 ) ) ;
#182179 = CARTESIAN_POINT ( 'NONE',  ( 3.550944491985886575, 0.2853618425060593378, 1.890879049853078087 ) ) ;
#182180 = B_SPLINE_CURVE_WITH_KNOTS ( 'NONE', 3,
 ( #177235, #194535, #45122, #47255, #13647, #162058, #193478 ),
 .UNSPECIFIED., .F., .F.,
 ( 4, 3, 4 ),
 ( -5.999999999944987321E-08, 0.000000000000000000, 8.562056648505256864E-06 ),
 .UNSPECIFIED. ) ;
#182181 = CARTESIAN_POINT ( 'NONE',  ( -6.240830780992103755, 6.175390754112560110, 1.040834085586084257E-14 ) ) ;
#182182 = CARTESIAN_POINT ( 'NONE',  ( 3.131570294632282092, 5.636953862837537521, -1.082531754730543971 ) ) ;
#182184 = CARTESIAN_POINT ( 'NONE',  ( 1.704704067347760699, 1.882482151684254923, 0.7231221989368596947 ) ) ;
#182183 = LINE ( 'NONE', #18619, #197791 ) ;
#182185 = CARTESIAN_POINT ( 'NONE',  ( 1.364683531249996529, 12.02604166700806765, 0.7879004041258405033 ) ) ;
#182187 = CARTESIAN_POINT ( 'NONE',  ( -5.818384198920079520, 6.817144982608731141, 1.199719254218452935 ) ) ;
#182186 = CARTESIAN_POINT ( 'NONE',  ( 0.6445460132639491135, 0.6724220840489106843, 2.191533042908066165 ) ) ;
#182188 = CARTESIAN_POINT ( 'NONE',  ( 3.944159270863063060, 1.716513557549454339, 0.1685945156147239388 ) ) ;
#182189 = CARTESIAN_POINT ( 'NONE',  ( 5.854088466050551887, 10.05179665369283981, 0.7998128361456341429 ) ) ;
#182190 = CARTESIAN_POINT ( 'NONE',  ( 5.007038802148489509, 4.735966778795008381, 0.7998128361456341429 ) ) ;
#182191 = CARTESIAN_POINT ( 'NONE',  ( -11.35605497252127094, 12.48581854048354423, -3.553547709190210124 ) ) ;
#182192 = CARTESIAN_POINT ( 'NONE',  ( 1.592165322863370980, 0.9698756732311950568, -1.705302290208744687 ) ) ;
#182193 = CARTESIAN_POINT ( 'NONE',  ( -1.500000000000022427, 8.226407212580419070, 3.114167208185206981 ) ) ;
#182194 = CARTESIAN_POINT ( 'NONE',  ( 4.843287188579786573, 6.673587691474970107, -1.599625672291256295 ) ) ;
#182195 = CARTESIAN_POINT ( 'NONE',  ( 0.07556134207192893859, 1.990881419511018935, -2.657973000608151448 ) ) ;
#182196 = EDGE_CURVE ( 'NONE', #10112, #171541, #56552, .T. ) ;
#182197 = ORIENTED_EDGE ( 'NONE', *, *, #2823, .T. ) ;
#182198 = CYLINDRICAL_SURFACE ( 'NONE', #179192, 1.250000000000000000 ) ;
#182199 = VERTEX_POINT ( 'NONE', #23009 ) ;
#182200 = CARTESIAN_POINT ( 'NONE',  ( 4.740750167454264918, 1.734909645891765662, 0.5210944610908369024 ) ) ;
#182201 = ORIENTED_EDGE ( 'NONE', *, *, #76416, .T. ) ;
#182202 = CARTESIAN_POINT ( 'NONE',  ( 5.169401708560450004, 9.252995436621013425, 0.000000000000000000 ) ) ;
#182203 = DIRECTION ( 'NONE',  ( 0.000000000000000000, 0.000000000000000000, 1.000000000000000000 ) ) ;
#182204 = CARTESIAN_POINT ( 'NONE',  ( 6.516260798181108704, -1.810903427820510503, 0.05229752674829404868 ) ) ;
#182205 = CARTESIAN_POINT ( 'NONE',  ( 6.549997608733495902, 7.774656977344789333, -1.082531754730548412 ) ) ;
#182206 = CARTESIAN_POINT ( 'NONE',  ( -11.78331023100045627, 9.799999999999998934, -1.800000000000001155 ) ) ;
#182207 = CARTESIAN_POINT ( 'NONE',  ( 5.849792259110643933, 6.002811869646802911, -0.3480847251615213356 ) ) ;
#182208 = ORIENTED_EDGE ( 'NONE', *, *, #120145, .T. ) ;
#182209 = ORIENTED_EDGE ( 'NONE', *, *, #154305, .T. ) ;
#182210 = TOROIDAL_SURFACE ( 'NONE', #109636, 1.821370322827223553, 0.2000000000000000111 ) ;
#182212 = CARTESIAN_POINT ( 'NONE',  ( 8.920375002787457319, 12.49452237230570084, 1.199719254218450271 ) ) ;
#182211 = CARTESIAN_POINT ( 'NONE',  ( 5.863677653134839574, -0.4517109595482105555, 1.805248464757176041 ) ) ;
#182213 = CARTESIAN_POINT ( 'NONE',  ( 3.989770193594462722, -1.910233455636681787, 0.1444642847954723808 ) ) ;
#182214 = CARTESIAN_POINT ( 'NONE',  ( -6.637758778446696262, -7.996947095390848581, -6.849430810391457847 ) ) ;
#182215 =( LENGTH_UNIT ( ) NAMED_UNIT ( * ) SI_UNIT ( .MILLI., .METRE. ) );
#182216 = CARTESIAN_POINT ( 'NONE',  ( 11.33772463945037323, 13.50902469614648815, 3.599999999999999201 ) ) ;
#182217 = CARTESIAN_POINT ( 'NONE',  ( 6.995644074971448134, 7.263932296995902149, -0.7216878364870257245 ) ) ;
#182219 = CARTESIAN_POINT ( 'NONE',  ( 5.647700563513772920, 2.085583167219496215, -0.3645771090082204902 ) ) ;
#182218 = CARTESIAN_POINT ( 'NONE',  ( -10.16825202056928390, 10.96530823352674133, 0.7216878364870438212 ) ) ;
#182220 = CARTESIAN_POINT ( 'NONE',  ( 0.7081719773709762578, -2.151164098719647200, 0.2130325561137471624 ) ) ;
#182221 = CARTESIAN_POINT ( 'NONE',  ( -6.445975688654487001, 6.485002823043819475, -0.7998128361456362523 ) ) ;
#182222 = CARTESIAN_POINT ( 'NONE',  ( 3.878514461961128479, 6.682628084666728085, -1.199719254218448494 ) ) ;
#182223 = CARTESIAN_POINT ( 'NONE',  ( 1.184280053745472738, -1.780106929851841491, -0.4042017716930704219 ) ) ;
#182224 = CARTESIAN_POINT ( 'NONE',  ( -3.632695093457760649, 6.325562478087638496, -1.199719254218452047 ) ) ;
#182225 = CARTESIAN_POINT ( 'NONE',  ( 3.487140482124751362, 1.650829432287181264, -0.7796944959364560113 ) ) ;
#182226 = CARTESIAN_POINT ( 'NONE',  ( 13.13649811952651270, 6.591446614545316329, 1.105413235251222925 ) ) ;
#182227 = EDGE_LOOP ( 'NONE', ( #141237, #76871, #192306, #161216 ) ) ;
#182228 = CARTESIAN_POINT ( 'NONE',  ( 2.699605434738296506, -1.457443026130700758, -1.324932107022150918 ) ) ;
#182229 = CARTESIAN_POINT ( 'NONE',  ( 4.810071659083087425, 1.336522264689719686, -1.409242981738271894 ) ) ;
#182230 = CARTESIAN_POINT ( 'NONE',  ( -6.400331034103001748, 9.624747418832267698, 1.199719254218452935 ) ) ;
#182232 = CARTESIAN_POINT ( 'NONE',  ( 5.273731010124149243, 0.4114677744767555878, -2.080124947408354963 ) ) ;
#182231 = CARTESIAN_POINT ( 'NONE',  ( 7.679767667498067496, 7.924426798361372093, 0.000000000000000000 ) ) ;
#182233 = CARTESIAN_POINT ( 'NONE',  ( 0.01083140255523393387, -7.162053774861991684, 9.500385102287575378 ) ) ;
#182234 = CARTESIAN_POINT ( 'NONE',  ( 3.281800106729782840, 1.865104756965057620, -0.4213900744019505318 ) ) ;
#182235 = CARTESIAN_POINT ( 'NONE',  ( 6.112956004491900686, 6.016961049888108981, 0.08799760576284378077 ) ) ;
#182236 = LINE ( 'NONE', #33860, #129026 ) ;
#182237 = CARTESIAN_POINT ( 'NONE',  ( -1.364683531250010740, 12.88020833367473372, 0.7879004041258445001 ) ) ;
#182238 = CARTESIAN_POINT ( 'NONE',  ( 3.878514461961128479, 6.682628084666728085, -1.199719254218448494 ) ) ;
#182239 = CARTESIAN_POINT ( 'NONE',  ( 4.792970997630896512, 5.550553237779539018, 1.199719254218464037 ) ) ;
#182240 = CARTESIAN_POINT ( 'NONE',  ( -0.07171210202241015685, 2.519999999999996021, 2.000000000000000444 ) ) ;
#182241 = CARTESIAN_POINT ( 'NONE',  ( 4.564971734551386717, -1.632036996880025903, -0.8184370388232551363 ) ) ;
#182242 = LINE ( 'NONE', #152959, #142488 ) ;
#182243 = CARTESIAN_POINT ( 'NONE',  ( -8.134528978519403708, 11.47373899403920205, 1.082531754730549967 ) ) ;
#182244 = AXIS2_PLACEMENT_3D ( 'NONE', #213360, #1032, #50883 ) ;
#182245 = CARTESIAN_POINT ( 'NONE',  ( -6.035068427865825313, 7.156668563632000435, 1.186355232826277417 ) ) ;
#182246 = CARTESIAN_POINT ( 'NONE',  ( -0.3000000000000260791, 3.975028841772316301, -0.9637995837462940418 ) ) ;
#182247 = CARTESIAN_POINT ( 'NONE',  ( 5.137510444216992767, -1.323429205136433140, -1.322332877454430955 ) ) ;
#182248 = CARTESIAN_POINT ( 'NONE',  ( 7.613066949273408213, 8.840665181362512115, -1.199719254218441611 ) ) ;
#182249 = CARTESIAN_POINT ( 'NONE',  ( -3.588104209110990706, 7.337872010604796991, 1.040834085586084257E-14 ) ) ;
#182250 = AXIS2_PLACEMENT_3D ( 'NONE', #8665, #111576, #62745 ) ;
#182251 = CARTESIAN_POINT ( 'NONE',  ( 2.381428537494710618, 5.930083727052461562, 0.7998128361456462443 ) ) ;
#182252 = CARTESIAN_POINT ( 'NONE',  ( -8.012344526598182026E-15, 10.85937500034139624, -1.575800808251669460 ) ) ;
#182253 = CARTESIAN_POINT ( 'NONE',  ( -5.762378981008047241, 6.681529218386182301, 1.199719254218450271 ) ) ;
#182254 = CARTESIAN_POINT ( 'NONE',  ( 4.532503425670185493, 4.182342172903648070, 1.214306433183764966E-14 ) ) ;
#182255 = CARTESIAN_POINT ( 'NONE',  ( -5.112833325684928987, 5.137596099486740897, -0.7216878364870338292 ) ) ;
#182256 = CARTESIAN_POINT ( 'NONE',  ( -5.368138756007025947, 8.350246751061767725, 1.199719254218452047 ) ) ;
#182257 = CARTESIAN_POINT ( 'NONE',  ( 6.491115304390381979, 0.2044268322529273207, 2.161409909153473752 ) ) ;
#182258 = CARTESIAN_POINT ( 'NONE',  ( 2.583745723679788497, -0.6611301898758483730, 2.011445711247431323 ) ) ;
#182259 = CARTESIAN_POINT ( 'NONE',  ( 9.413438726589914651, 9.876766690643398405, 0.000000000000000000 ) ) ;
#182260 = CARTESIAN_POINT ( 'NONE',  ( 11.55950211276791251, 12.22000000000000064, -3.221476510067114329 ) ) ;
#182261 = CARTESIAN_POINT ( 'NONE',  ( 6.368043163206878354, -2.055323469740528264, 0.2474699835256082281 ) ) ;
#182262 = CARTESIAN_POINT ( 'NONE',  ( 4.359152798643180837, 7.157646611464889119, -1.047953017514296370 ) ) ;
#182263 = CARTESIAN_POINT ( 'NONE',  ( 5.666945020832170776, 7.634521829102760115, 1.443375672974062551 ) ) ;
#182265 = CARTESIAN_POINT ( 'NONE',  ( 0.2458932500721333070, 6.514853439382787492, 3.140456330564937559 ) ) ;
#182264 = CARTESIAN_POINT ( 'NONE',  ( -1.734723475976807094E-15, 2.999999999999988898, -6.938893903907228378E-15 ) ) ;
#182266 = CARTESIAN_POINT ( 'NONE',  ( 2.449550052152906332, 0.6095859302821411418, -2.209661595554306412 ) ) ;
#182268 = CARTESIAN_POINT ( 'NONE',  ( 3.879041346841291649, 7.539648981374564407, 1.040834085586084257E-14 ) ) ;
#182267 = CARTESIAN_POINT ( 'NONE',  ( -9.499668754385634628, -7.559700871049417792, -0.07933194154487524519 ) ) ;
#182269 = CARTESIAN_POINT ( 'NONE',  ( 2.091926199050548441, 1.179367891222588005, 1.505316542580182659 ) ) ;
#182270 = AXIS2_PLACEMENT_3D ( 'NONE', #185750, #37383, #150087 ) ;
#182271 = VERTEX_POINT ( 'NONE', #77111 ) ;
#182272 = CARTESIAN_POINT ( 'NONE',  ( 7.904040366642699489, 8.323727970612377902, 0.7216878364870458196 ) ) ;
#182273 = CARTESIAN_POINT ( 'NONE',  ( 0.7209482731112315523, 1.521806550355369492, -1.318046908132961104 ) ) ;
#182274 = CARTESIAN_POINT ( 'NONE',  ( 0.7077677203753615087, 0.6208407433182620005, -1.860969989990405749 ) ) ;
#182275 = CARTESIAN_POINT ( 'NONE',  ( -11.78331023100045627, 13.79999999999998295, 1.799999999999999600 ) ) ;
#182276 = CARTESIAN_POINT ( 'NONE',  ( -6.855619230004478482, 11.14997286831390788, -0.7998128361456291469 ) ) ;
#182278 = CARTESIAN_POINT ( 'NONE',  ( 2.025891818203702233, 1.021928659931588435, -1.444778566663025954 ) ) ;
#182277 = CARTESIAN_POINT ( 'NONE',  ( 3.820331522234471144, 1.985175722263971654, 0.6558375257153716831 ) ) ;
#182279 = DIRECTION ( 'NONE',  ( 0.000000000000000000, 0.000000000000000000, 1.000000000000000000 ) ) ;
#182281 = CARTESIAN_POINT ( 'NONE',  ( 5.525394443818422374, -1.450416979558573072, -1.775029086184358507 ) ) ;
#182280 = DIRECTION ( 'NONE',  ( -0.000000000000000000, -1.000000000000000000, -0.000000000000000000 ) ) ;
#182282 = CARTESIAN_POINT ( 'NONE',  ( 3.486021976759791308, -0.3410757193606011040, -1.706382030880509104 ) ) ;
#182283 = ADVANCED_FACE ( 'NONE', ( #57680 ), #139241, .T. ) ;
#182284 = CARTESIAN_POINT ( 'NONE',  ( 3.891353782322113375, 4.498666486585943147, -1.199719254218446718 ) ) ;
#182285 = CARTESIAN_POINT ( 'NONE',  ( 3.874598038455354665, 7.742391154831718580, -0.7998128361456361413 ) ) ;
#182286 = CARTESIAN_POINT ( 'NONE',  ( 3.004952549044386245, 1.720378813442688282, 0.2150250689552536121 ) ) ;
#182287 = CARTESIAN_POINT ( 'NONE',  ( 3.701788104937975721, -1.641978770885927252, -1.420606208986204155 ) ) ;
#182288 = CARTESIAN_POINT ( 'NONE',  ( 3.985207087413062066, 6.736826471035503694, -1.199719254218452047 ) ) ;
#182289 = CARTESIAN_POINT ( 'NONE',  ( 5.559779856078610472, 1.205038519190555268, 1.616695979245158066 ) ) ;
#182290 = CARTESIAN_POINT ( 'NONE',  ( 0.7187500000000003331, -0.7852924748299483504, 1.895863743164105220 ) ) ;
#182291 = CARTESIAN_POINT ( 'NONE',  ( -1.499999999999997780, 4.431250000682819490, 1.214306433183764966E-14 ) ) ;
#182292 = CARTESIAN_POINT ( 'NONE',  ( 2.555585810550043302, 0.5154765373659023764, -1.856070933656640332 ) ) ;
#182293 = CARTESIAN_POINT ( 'NONE',  ( 1.364683531249997417, 15.23437500034140157, 2.602085213965210642E-15 ) ) ;
#182294 = CARTESIAN_POINT ( 'NONE',  ( 5.888988880356018640, -2.109219445749145994, -0.6973366327849057633 ) ) ;
#182295 = VERTEX_POINT ( 'NONE', #41449 ) ;
#182296 = CARTESIAN_POINT ( 'NONE',  ( 6.983263157960340806, 6.037546352565132501, 2.441087094350186337 ) ) ;
#182297 = CARTESIAN_POINT ( 'NONE',  ( -1.402160292154681736E-14, 1.337500000000025446, -1.732050807568863648 ) ) ;
#182298 = CARTESIAN_POINT ( 'NONE',  ( 7.287671262545424966, 8.461036880179857889, -1.199719254218451159 ) ) ;
#182299 = CARTESIAN_POINT ( 'NONE',  ( 4.975479186090857375, 5.867442474269873642, 1.082531754730560403 ) ) ;
#182300 = EDGE_CURVE ( 'NONE', #186457, #172991, #63508, .T. ) ;
#182301 = DIRECTION ( 'NONE',  ( -0.000000000000000000, -1.000000000000000000, -0.000000000000000000 ) ) ;
#182302 = CARTESIAN_POINT ( 'NONE',  ( 9.273413882067330860, 9.921330405274451536, -0.7216878364870257245 ) ) ;
#182303 = ADVANCED_FACE ( 'NONE', ( #188736 ), #8603, .F. ) ;
#182304 = CARTESIAN_POINT ( 'NONE',  ( -15.75000000000000000, 13.79999999999999893, -1.800000000000001155 ) ) ;
#182305 = CARTESIAN_POINT ( 'NONE',  ( 4.203910148689107729, 7.062256385849379647, -1.199719254218448494 ) ) ;
#182306 = CARTESIAN_POINT ( 'NONE',  ( -5.180624094197616714, 5.216685329418210948, 0.7216878364870257245 ) ) ;
#182307 = CARTESIAN_POINT ( 'NONE',  ( 4.721170020219593866, -1.840989660556498597, -0.9304453918272929114 ) ) ;
#182308 = CARTESIAN_POINT ( 'NONE',  ( -4.822949958159302497, 6.649860922651058992, -1.599625672291256295 ) ) ;
#182309 = CARTESIAN_POINT ( 'NONE',  ( -0.7499999999999972244, 3.389583334016149863, -1.299038105676652011 ) ) ;
#182310 = CARTESIAN_POINT ( 'NONE',  ( -1.364683531250014514, -0.9697916663252473812, 0.7879004041258379498 ) ) ;
#182311 = CARTESIAN_POINT ( 'NONE',  ( 5.483624757375023862, 1.255567903217995829, 1.386730702750748945 ) ) ;
#182312 = CARTESIAN_POINT ( 'NONE',  ( 4.359819935191601381, -0.006009022472676025205, -1.734343005118470726 ) ) ;
#182313 = CARTESIAN_POINT ( 'NONE',  ( 3.931004251652202353, -1.203735069864294571, -1.257276804044287655 ) ) ;
#182314 = CARTESIAN_POINT ( 'NONE',  ( 5.522248639467795428, 5.337044922334209573, -0.7998128361456231517 ) ) ;
#182315 = CARTESIAN_POINT ( 'NONE',  ( 1.435548669473255323, -1.664339209632224481, -1.576619915386682447 ) ) ;
#182316 = CARTESIAN_POINT ( 'NONE',  ( 0.6823417656249917140, 5.155208333674749177, 1.181850606188765695 ) ) ;
#182317 = CARTESIAN_POINT ( 'NONE',  ( 6.163634092203726489, 1.075319730316869560, 1.792882302630414593 ) ) ;
#182318 = CARTESIAN_POINT ( 'NONE',  ( 0.5855841007226803008, -1.826885663252286740, -0.2280376995877145263 ) ) ;
#182319 = DIRECTION ( 'NONE',  ( -0.7927788072566357425, 0.000000000000000000, -0.6095094443605826307 ) ) ;
#182320 =( NAMED_UNIT ( * ) SI_UNIT ( $, .STERADIAN. ) SOLID_ANGLE_UNIT ( ) );
#182321 = CARTESIAN_POINT ( 'NONE',  ( 2.127577483945505055, 0.4445034925110411539, 1.966644524931899563 ) ) ;
#182322 = DIRECTION ( 'NONE',  ( 1.000000000000000000, 2.090028284309406390E-15, 0.000000000000000000 ) ) ;
#182323 = CARTESIAN_POINT ( 'NONE',  ( 9.148157776457804147, 13.34235666145839616, -9.071852530902138056 ) ) ;
#182324 = CARTESIAN_POINT ( 'NONE',  ( -7.172426956829277778, 8.326585190177668849, -1.199719254218452935 ) ) ;
#182325 = CARTESIAN_POINT ( 'NONE',  ( 6.342516933094585418, 6.294024598232139667, 1.040834085586084257E-14 ) ) ;
#182326 = CARTESIAN_POINT ( 'NONE',  ( -1.953008978358306879E-14, 1.828125000341410678, -1.570758158831798257 ) ) ;
#182327 = CARTESIAN_POINT ( 'NONE',  ( 3.862070080935349203, 0.7130468835700142227, -1.997148454185311506 ) ) ;
#182328 = AXIS2_PLACEMENT_3D ( 'NONE', #158060, #42180, #208898 ) ;
#182329 = CARTESIAN_POINT ( 'NONE',  ( 0.6823417656249882723, -0.3239583329919110133, -1.181850606188749264 ) ) ;
#182330 = CARTESIAN_POINT ( 'NONE',  ( 5.813091150998386247, 1.612263477354998864, 0.8566026058636074803 ) ) ;
#182331 = ORIENTED_EDGE ( 'NONE', *, *, #130852, .T. ) ;
#182332 = CARTESIAN_POINT ( 'NONE',  ( -7.605197822622922210, 7.837428646007010613, -0.7998128361456362523 ) ) ;
#182333 = PLANE ( 'NONE',  #46967 ) ;
#182334 = CARTESIAN_POINT ( 'NONE',  ( 1.001543065824772753E-15, -1.968749999044084653, 4.012584370867899430 ) ) ;
#182335 = CARTESIAN_POINT ( 'NONE',  ( -7.203459687562382641, 7.298457811777897319, -0.7998128361456291469 ) ) ;
#182336 = CARTESIAN_POINT ( 'NONE',  ( 3.023699206349286239, -0.3898671064326043045, 1.981619672226095918 ) ) ;
#182337 = CARTESIAN_POINT ( 'NONE',  ( 6.370183515248876382, 1.128980158350336049, 1.895982279999992359 ) ) ;
#182338 = CARTESIAN_POINT ( 'NONE',  ( 10.38962578677386084, 11.01565159419135043, 0.000000000000000000 ) ) ;
#182339 = CARTESIAN_POINT ( 'NONE',  ( 3.871788065385643574, -1.834046284760854961, 0.3141801383321814467 ) ) ;
#182340 = CARTESIAN_POINT ( 'NONE',  ( 9.511208455186636712, 11.05516360492796935, 1.199719254218453823 ) ) ;
#182341 = CARTESIAN_POINT ( 'NONE',  ( 11.81911962874442068, 13.75710573484113475, -1.591749704452471326 ) ) ;
#182342 = CARTESIAN_POINT ( 'NONE',  ( -2.927671105547157371, 5.503034492191895666, 1.199719254218462483 ) ) ;
#182343 = CARTESIAN_POINT ( 'NONE',  ( -6.835281999583978418, 11.12624609948998966, -0.7998128361456291469 ) ) ;
#182345 = CARTESIAN_POINT ( 'NONE',  ( 0.1105426557568081891, -0.9253945370547181914, -1.951590883024490353 ) ) ;
#182344 = B_SPLINE_CURVE_WITH_KNOTS ( 'NONE', 3,
 ( #155571, #68942, #2872, #7154, #86291, #185903 ),
 .UNSPECIFIED., .F., .F.,
 ( 4, 2, 4 ),
 ( 0.000000000000000000, 0.0003767011250903910184, 0.0007534022501807818200 ),
 .UNSPECIFIED. ) ;
#182347 = CARTESIAN_POINT ( 'NONE',  ( -4.211465482254622472, 7.549728682704877514, 0.9859626088348661943 ) ) ;
#182346 = CARTESIAN_POINT ( 'NONE',  ( -7.584860592202423035, 7.813701877183096833, -0.7998128361456362523 ) ) ;
#182348 = CARTESIAN_POINT ( 'NONE',  ( 1.364683531249988757, -0.1156249996585798079, 0.000000000000000000 ) ) ;
#182349 = CARTESIAN_POINT ( 'NONE',  ( 1.176590053548575598, -0.7728590343649595074, -1.552129106697144989 ) ) ;
#182350 = CARTESIAN_POINT ( 'NONE',  ( 1.763200577577472172, 0.8928190760214287369, 1.493706742695336764 ) ) ;
#182352 = CARTESIAN_POINT ( 'NONE',  ( 9.273413882067330860, 9.921330405274451536, -0.7216878364870257245 ) ) ;
#182351 = CARTESIAN_POINT ( 'NONE',  ( 6.199901738523720951, -0.7837251098280417771, 2.170682987836409783 ) ) ;
#182353 = CARTESIAN_POINT ( 'NONE',  ( 5.225741863424510747, 5.061396693608882558, 0.7998128361456352531 ) ) ;
#182354 = CARTESIAN_POINT ( 'NONE',  ( 1.493510409444120057, 1.558468831475682492, 1.348393839584006493 ) ) ;
#182355 = CARTESIAN_POINT ( 'NONE',  ( 6.193377243344257543, 6.120028293523423812, -0.7998128361456281477 ) ) ;
#182356 = CARTESIAN_POINT ( 'NONE',  ( 0.4739822347885510601, 1.752760637641921360, 0.9961516927870717186 ) ) ;
#182357 = CYLINDRICAL_SURFACE ( 'NONE', #175975, 1.500000000000000222 ) ;
#182358 = CARTESIAN_POINT ( 'NONE',  ( -6.123442655227560927, 7.173046514967467147, 1.199719254218452047 ) ) ;
#182359 = CARTESIAN_POINT ( 'NONE',  ( 6.614126560844452385, -0.8839695271746010885, -1.648598838400926692 ) ) ;
#182361 = CARTESIAN_POINT ( 'NONE',  ( -5.966997003790221576, 9.015228033513643879, -1.082531754730549967 ) ) ;
#182360 = CARTESIAN_POINT ( 'NONE',  ( 5.045129621168108258, 0.1466893748028277877, 1.906852434080000824 ) ) ;
#182362 = CARTESIAN_POINT ( 'NONE',  ( 6.393228082638676923, 1.922373441260841087, -1.083778638264052852 ) ) ;
#182363 = CARTESIAN_POINT ( 'NONE',  ( -6.902509602688821744, 8.185920970292658083, -1.082531754730549967 ) ) ;
#182364 = CARTESIAN_POINT ( 'NONE',  ( 4.434925645001613681, 5.307073019657559065, -1.082531754730548412 ) ) ;
#182365 = CARTESIAN_POINT ( 'NONE',  ( -3.648552735408990166, 6.310376387068841630, -1.082531754730546636 ) ) ;
#182366 = CARTESIAN_POINT ( 'NONE',  ( 0.1529977018510132181, 0.3474608822290006782, 1.989397386523162226 ) ) ;
#182367 = VERTEX_POINT ( 'NONE', #123837 ) ;
#182368 = CARTESIAN_POINT ( 'NONE',  ( 2.995503060082918889, 1.979820613015465858, -1.185208598768563881 ) ) ;
#182370 = EDGE_CURVE ( 'NONE', #184579, #178469, #8913, .T. ) ;
#182369 = CARTESIAN_POINT ( 'NONE',  ( 4.685966490639408732, -1.205361723144786845, -1.547842780461285761 ) ) ;
#182371 = CARTESIAN_POINT ( 'NONE',  ( 1.850371385673426294, -1.951817131159512719, -0.1975377159662907445 ) ) ;
#182372 = CARTESIAN_POINT ( 'NONE',  ( 9.049177462117294013, 12.64479190819049670, -1.199719254218446718 ) ) ;
#182373 = CARTESIAN_POINT ( 'NONE',  ( 2.580963302752299349, 0.4788041664877049075, 0.000000000000000000 ) ) ;
#182374 = CARTESIAN_POINT ( 'NONE',  ( 0.6204977360529799757, 2.087120111646578291, 0.3555802741468729877 ) ) ;
#182376 = CARTESIAN_POINT ( 'NONE',  ( -9.182950115157607840, 9.607863310639020327, 0.7998128361456462443 ) ) ;
#182375 = CARTESIAN_POINT ( 'NONE',  ( -5.382750679825375251, 6.238629533673094585, -1.199719254218446718 ) ) ;
#182377 = CARTESIAN_POINT ( 'NONE',  ( 0.3570341529223716726, 1.821527202347131169, -0.2672101559373847857 ) ) ;
#182378 = CARTESIAN_POINT ( 'NONE',  ( 4.750930541093643100, -0.4693155065514472701, -2.119606683777853995 ) ) ;
#182379 = CARTESIAN_POINT ( 'NONE',  ( -0.3960368903851408384, 2.881569912824395896, 1.962180772919328353 ) ) ;
#182380 = CARTESIAN_POINT ( 'NONE',  ( 1.705496241919310707, 1.842552997918958768, -1.049655202612943095 ) ) ;
#182381 = CARTESIAN_POINT ( 'NONE',  ( -0.7500000000000215383, 2.722916667349486897, 1.299038105676671107 ) ) ;
#182382 = CARTESIAN_POINT ( 'NONE',  ( 10.16199982864259788, 11.81442020729326536, 1.199719254218452047 ) ) ;
#182383 = CARTESIAN_POINT ( 'NONE',  ( 11.88237951145550220, 11.25680652621284494, -0.9087114598430711121 ) ) ;
#182384 = CARTESIAN_POINT ( 'NONE',  ( 6.265786130652515773, 6.994708711910199384, -0.9640221254198673151 ) ) ;
#182385 = ORIENTED_EDGE ( 'NONE', *, *, #85850, .T. ) ;
#182386 = CARTESIAN_POINT ( 'NONE',  ( 2.143891142268034677, 0.7916089892260335104, -1.902880034897576733 ) ) ;
#182388 = CARTESIAN_POINT ( 'NONE',  ( 7.006712406718516029, 14.55305236961725690, -9.688386885671178561 ) ) ;
#182387 = CARTESIAN_POINT ( 'NONE',  ( -7.316596452869116973, 11.68777962832266049, 0.7998128361456481317 ) ) ;
#182389 = CARTESIAN_POINT ( 'NONE',  ( 1.364683531249988535, 1.863541667008086211, 0.7879004041258500513 ) ) ;
#182390 = CARTESIAN_POINT ( 'NONE',  ( -1.500000000000008216, 9.250000000000001776, 3.469446951953614189E-15 ) ) ;
#182391 = ADVANCED_FACE ( 'NONE', ( #176755 ), #212431, .T. ) ;
#182392 = CARTESIAN_POINT ( 'NONE',  ( 5.639433180129016066, 7.452461152751827633, -1.378512499824318116 ) ) ;
#182393 = VERTEX_POINT ( 'NONE', #64073 ) ;
#182394 = CARTESIAN_POINT ( 'NONE',  ( 4.828717125059535320, 1.315996081294769304, -1.387672938220223307 ) ) ;
#182395 =( GEOMETRIC_REPRESENTATION_CONTEXT ( 3 ) GLOBAL_UNCERTAINTY_ASSIGNED_CONTEXT ( ( #61955 ) ) GLOBAL_UNIT_ASSIGNED_CONTEXT ( ( #41497, #205018, #169339 ) ) REPRESENTATION_CONTEXT ( 'NONE', 'WORKASPACE' ) );
#182396 = CARTESIAN_POINT ( 'NONE',  ( 0.7500000000000006661, 9.364583334016129967, 1.299038105676657340 ) ) ;
#182397 = CARTESIAN_POINT ( 'NONE',  ( 1.195004664211458456, -0.5499296976853912389, -2.194457269061194982 ) ) ;
#182398 = CARTESIAN_POINT ( 'NONE',  ( -10.03267048443264109, 11.76749898900197877, 1.082531754730558626 ) ) ;
#182399 = CARTESIAN_POINT ( 'NONE',  ( 1.810541516808946039, -0.4857983738905074511, -1.745121406981971157 ) ) ;
#182400 = CARTESIAN_POINT ( 'NONE',  ( 1.446349702961244876, -1.352062789758176731, 1.357433777346368498 ) ) ;
#182401 = CARTESIAN_POINT ( 'NONE',  ( 3.068866956829822801, 1.501395149897828851, -1.425812640530661479 ) ) ;
#182402 = CARTESIAN_POINT ( 'NONE',  ( 1.364683531249986537, 0.9677083336747538400, -0.7879004041258239610 ) ) ;
#182403 =( GEOMETRIC_REPRESENTATION_CONTEXT ( 3 ) GLOBAL_UNCERTAINTY_ASSIGNED_CONTEXT ( ( #126783 ) ) GLOBAL_UNIT_ASSIGNED_CONTEXT ( ( #1300, #49029, #67359 ) ) REPRESENTATION_CONTEXT ( 'NONE', 'WORKASPACE' ) );
#182404 = CARTESIAN_POINT ( 'NONE',  ( 0.6902270635062581761, -1.956280663680696197, -0.2437950987402882630 ) ) ;
#182405 = CARTESIAN_POINT ( 'NONE',  ( 5.637312448503878137, -1.740617781635974248, 0.8259078106758013238 ) ) ;
#182407 = CARTESIAN_POINT ( 'NONE',  ( 5.583942420111207561, 7.395222456726187943, -1.242479836444350783 ) ) ;
#182406 = CARTESIAN_POINT ( 'NONE',  ( 1.647554839532150872, -1.947651944554330772, 1.237524531948221096 ) ) ;
#182408 = CARTESIAN_POINT ( 'NONE',  ( 1.364683531249988757, 2.134375000341422357, 1.214306433183764966E-14 ) ) ;
#182409 = CARTESIAN_POINT ( 'NONE',  ( 5.178211798877670802, -1.100624681205965461, -1.744318484351764509 ) ) ;
#182410 = CARTESIAN_POINT ( 'NONE',  ( -6.551614543901706611, 8.666636272683888365, 1.599625672291283607 ) ) ;
#182411 = CARTESIAN_POINT ( 'NONE',  ( 7.995557903757111617, 10.35123685918189729, 1.599625672291281386 ) ) ;
#182412 = CARTESIAN_POINT ( 'NONE',  ( -15.75000000000000000, 10.19999999999999929, -1.400000000000001910 ) ) ;
#182414 = CARTESIAN_POINT ( 'NONE',  ( -1.499999999999997780, 3.650000000000021227, 1.214306433183764966E-14 ) ) ;
#182413 = CARTESIAN_POINT ( 'NONE',  ( 4.928798221971478988, 2.014404525830254311, 0.6141583887315901213 ) ) ;
#182415 = CARTESIAN_POINT ( 'NONE',  ( 0.6823417656249899377, 2.155208333674753174, 1.181850606188767472 ) ) ;
#182416 = CARTESIAN_POINT ( 'NONE',  ( 5.202478051755599964, -0.7228594145181690411, -2.037298988101433839 ) ) ;
#182418 = EDGE_CURVE ( 'NONE', #104249, #105884, #73863, .T. ) ;
#182417 = CARTESIAN_POINT ( 'NONE',  ( 5.461584154626091703, -1.593396655685812124, -1.240940796477793873 ) ) ;
#182419 = CARTESIAN_POINT ( 'NONE',  ( -5.260200412422213923, 6.199617238323108737, -1.082531754730544860 ) ) ;
#182420 = CIRCLE ( 'NONE', #89071, 0.09999999999999971412 ) ;
#182421 = EDGE_CURVE ( 'NONE', #143658, #29860, #147467, .T. ) ;
#182424 = CARTESIAN_POINT ( 'NONE',  ( 6.805829924380118356, 7.042482454639357847, 0.7216878364870317197 ) ) ;
#182423 = CARTESIAN_POINT ( 'NONE',  ( -1.642778471874998480, -2.501041666188707158, 2.845375778867863303 ) ) ;
#182422 = CARTESIAN_POINT ( 'NONE',  ( 8.174640274396848483, 8.501778173076651512, 0.7998128361456291469 ) ) ;
#182425 = CARTESIAN_POINT ( 'NONE',  ( -4.959250327548641479, 9.007818825440551791, -0.7998128361456362523 ) ) ;
#182426 = CARTESIAN_POINT ( 'NONE',  ( 4.083220446344194343, 1.622485107653489633, 1.197306254465977826 ) ) ;
#182427 = CARTESIAN_POINT ( 'NONE',  ( -9.179033691651859783, 10.66762638080401260, 1.199719254218462483 ) ) ;
#182429 = CARTESIAN_POINT ( 'NONE',  ( -1.499999999999997780, 6.280000000000042881, -2.873333333333329520 ) ) ;
#182428 = CARTESIAN_POINT ( 'NONE',  ( -10.31739171031960822, 11.13930453823545186, 1.040834085586084257E-14 ) ) ;
#182430 = CARTESIAN_POINT ( 'NONE',  ( -1.364683531250010295, 5.738541667008088432, -0.7879004041258300672 ) ) ;
#182432 = CARTESIAN_POINT ( 'NONE',  ( -1.402160292154681736E-14, 8.421875000341403350, 1.575800808251682339 ) ) ;
#182431 = CARTESIAN_POINT ( 'NONE',  ( 4.891577088959510711, 1.599438101461609918, 1.454397306527709155 ) ) ;
#182433 = DIRECTION ( 'NONE',  ( 2.935049515055183778E-17, -0.8987940462991643731, 0.4383711467890826219 ) ) ;
#182434 = CARTESIAN_POINT ( 'NONE',  ( 6.720655732516672920, 1.239197277384354035, 2.287559680360019332 ) ) ;
#182436 = CARTESIAN_POINT ( 'NONE',  ( 5.273064617572334356, 1.777004185780726386, -0.9530273427700783895 ) ) ;
#182435 = CARTESIAN_POINT ( 'NONE',  ( -7.253248993186740989, 9.485209796849769504, 1.443375672974090751 ) ) ;
#182437 = CARTESIAN_POINT ( 'NONE',  ( 1.499999999999990896, 4.775000000000022560, 1.214306433183764966E-14 ) ) ;
#182438 = CARTESIAN_POINT ( 'NONE',  ( 0.3106396986791125081, 1.498014557929911117, 0.8549171915634717900 ) ) ;
#182439 = CARTESIAN_POINT ( 'NONE',  ( 5.194709132691408549, 6.089524072008651423, 1.199719254218452935 ) ) ;
#182441 = CARTESIAN_POINT ( 'NONE',  ( 5.318541398310776103, 9.426991741329731056, -0.7998128361456481317 ) ) ;
#182440 = CARTESIAN_POINT ( 'NONE',  ( 7.944714827928043732, 10.29191993738131927, 1.443375672974076540 ) ) ;
#182442 = CARTESIAN_POINT ( 'NONE',  ( -11.63070519946230874, 8.357210500689234323, 2.967829092913087941 ) ) ;
#182443 = CARTESIAN_POINT ( 'NONE',  ( 6.221928862670094595, -1.039020359566013907, -1.555222851818117924 ) ) ;
#182444 = CARTESIAN_POINT ( 'NONE',  ( 0.9439945835589347300, -1.278642754803262171, -1.554848376591860815 ) ) ;
#182445 = CARTESIAN_POINT ( 'NONE',  ( -15.75000000000000000, 13.79999999999999893, 0.6999999999999992895 ) ) ;
#182446 = CARTESIAN_POINT ( 'NONE',  ( 2.535011535630975477, 5.901337858304024131, 0.7216878364870438212 ) ) ;
#182447 = CARTESIAN_POINT ( 'NONE',  ( -6.495764994278840021, 8.671754808115688107, 1.443375672974064550 ) ) ;
#182448 = ORIENTED_EDGE ( 'NONE', *, *, #66344, .T. ) ;
#182449 = CARTESIAN_POINT ( 'NONE',  ( 8.880227426826634129, 11.38335130276301754, 1.443375672974076540 ) ) ;
#182451 = CARTESIAN_POINT ( 'NONE',  ( 2.249625261780491492, 1.976952429928409805, -0.3961248688731587309 ) ) ;
#182450 = CARTESIAN_POINT ( 'NONE',  ( 1.823052125313682215, 1.569171740784220281, -1.426411057285102979 ) ) ;
#182452 = CARTESIAN_POINT ( 'NONE',  ( 1.986290607305480460, -1.112306265806988437, 1.429831149274364721 ) ) ;
#182453 = CARTESIAN_POINT ( 'NONE',  ( 6.003228155800906407, 10.22579295840155744, 0.000000000000000000 ) ) ;
#182454 = CARTESIAN_POINT ( 'NONE',  ( 6.737200384369169903, -1.933438233944266837, 0.9670071574134843084 ) ) ;
#182455 = VERTEX_POINT ( 'NONE', #92 ) ;
#182456 = CARTESIAN_POINT ( 'NONE',  ( 6.642605195691581699, 9.837124264027149678, 1.199719254218462483 ) ) ;
#182458 = CARTESIAN_POINT ( 'NONE',  ( 0.3916159773660661259, -1.906239802237769787, 0.1905982916604181676 ) ) ;
#182457 = CARTESIAN_POINT ( 'NONE',  ( -5.850506979496850057, 6.784345216623154151, -1.199719254218446718 ) ) ;
#182459 = CARTESIAN_POINT ( 'NONE',  ( -11.96217875511318063, 9.771456334210229855, -0.9561995067075080845 ) ) ;
#182460 = DIRECTION ( 'NONE',  ( -1.000000000000000000, -3.451266460341925773E-31, -8.638326563840809144E-31 ) ) ;
#182461 = CARTESIAN_POINT ( 'NONE',  ( 6.127922243252466039, 6.251590159990418449, 1.040834085586084257E-14 ) ) ;
#182462 = CARTESIAN_POINT ( 'NONE',  ( 1.364683531249988757, 0.1968750003414204697, 0.000000000000000000 ) ) ;
#182463 = CARTESIAN_POINT ( 'NONE',  ( 3.551873057100287223, 5.166937871415542283, 1.443375672974062551 ) ) ;
#182464 = CARTESIAN_POINT ( 'NONE',  ( -8.459397779922852578, 11.95671561229694824, 1.199719254218453823 ) ) ;
#182465 = CARTESIAN_POINT ( 'NONE',  ( 4.434552454296070145, 2.119417814153037316, 0.4246342833542292028 ) ) ;
#182466 = CARTESIAN_POINT ( 'NONE',  ( -6.292392690518214593, 7.474117906093608710, -1.082531754730549967 ) ) ;
#182467 = CARTESIAN_POINT ( 'NONE',  ( 4.584065335196261692, 7.401807753487379848, 1.082531754730549078 ) ) ;
#182468 = CARTESIAN_POINT ( 'NONE',  ( 1.846092968827160119, -1.388944967848893430, -1.602481653760478020 ) ) ;
#182469 = DIRECTION ( 'NONE',  ( 0.000000000000000000, -1.000000000000000000, 0.000000000000000000 ) ) ;
#182470 = CARTESIAN_POINT ( 'NONE',  ( 3.532457849674102590, 1.922574350601889082, 0.4351428330651128662 ) ) ;
#182471 = CARTESIAN_POINT ( 'NONE',  ( 5.484596585704371918, -1.208295678440996390, 1.482354609825987435 ) ) ;
#182472 = VERTEX_POINT ( 'NONE', #28370 ) ;
#182473 = DIRECTION ( 'NONE',  ( 0.000000000000000000, -1.000000000000000000, 0.000000000000000000 ) ) ;
#182474 = CARTESIAN_POINT ( 'NONE',  ( 5.564895475732142494, 1.492515675241333772, -1.285245034736775649 ) ) ;
#182475 = CARTESIAN_POINT ( 'NONE',  ( 1.095531938664672911, -1.942124713061957220, -0.0005026242578913541230 ) ) ;
#182476 = ORIENTED_EDGE ( 'NONE', *, *, #31832, .T. ) ;
#182477 = CARTESIAN_POINT ( 'NONE',  ( -3.623772196602547346, 7.449761006003425834, 0.000000000000000000 ) ) ;
#182479 = CARTESIAN_POINT ( 'NONE',  ( 8.039058738260216330, 8.343599714250547805, -0.7998128361456341429 ) ) ;
#182478 = CARTESIAN_POINT ( 'NONE',  ( -5.641601317062233001, 9.595968946632336127, -0.7216878364870338292 ) ) ;
#182480 = CARTESIAN_POINT ( 'NONE',  ( 7.494959990256193194, 7.638541498254023843, -0.7998128361456281477 ) ) ;
#182482 = CARTESIAN_POINT ( 'NONE',  ( 5.194182247366878613, 6.192872389083746043, 1.082531754730549078 ) ) ;
#182481 = CARTESIAN_POINT ( 'NONE',  ( 6.307567778855705853, 8.381915046796901692, -1.599625672291262513 ) ) ;
#182484 = VERTEX_POINT ( 'NONE', #179959 ) ;
#182483 = CARTESIAN_POINT ( 'NONE',  ( 5.795548653916324788, 1.765151677092157811, -0.7360495477024899813 ) ) ;
#182485 = CARTESIAN_POINT ( 'NONE',  ( 3.018423772948013006, -1.088090592406821155, -1.919924466345590108 ) ) ;
#182486 = CARTESIAN_POINT ( 'NONE',  ( 1.940722911589174204, 2.182806717142399489, 0.3235914145361811767 ) ) ;
#182487 = CARTESIAN_POINT ( 'NONE',  ( 0.3999999999999701572, 3.322650755865473648, -0.5865692111442885048 ) ) ;
#182488 = CARTESIAN_POINT ( 'NONE',  ( 0.8910925258837493201, -0.04752833427993513604, -1.911862225341356858 ) ) ;
#182489 = CARTESIAN_POINT ( 'NONE',  ( -10.51568781791557328, 12.48743269796084299, 3.554797817682051164 ) ) ;
#182490 = FACE_OUTER_BOUND ( 'NONE', #176633, .T. ) ;
#182491 = CARTESIAN_POINT ( 'NONE',  ( 4.492674960910642667, 2.029786422369950216, 0.4070406814440513665 ) ) ;
#182492 = CARTESIAN_POINT ( 'NONE',  ( -4.466521540698216164, 7.298359999868178960, -1.199719254218452047 ) ) ;
#182493 = AXIS2_PLACEMENT_3D ( 'NONE', #168435, #54682, #52551 ) ;
#182495 = CARTESIAN_POINT ( 'NONE',  ( 1.938557520917514987, 2.138169252768943984, 0.3173444169591658204 ) ) ;
#182494 = CARTESIAN_POINT ( 'NONE',  ( -3.253066792275140173, 5.882662793374543675, 1.199719254218462483 ) ) ;
#182496 = CARTESIAN_POINT ( 'NONE',  ( 3.527062600443749307, -2.024233912922444478, 0.8403589366152917073 ) ) ;
#182497 = CARTESIAN_POINT ( 'NONE',  ( -5.329149442624137478, 7.114720453792309662, 1.278927581188280760 ) ) ;
#182498 = CARTESIAN_POINT ( 'NONE',  ( 1.364683531249997417, 15.04687500034139447, 2.602085213965210642E-15 ) ) ;
#182499 = CARTESIAN_POINT ( 'NONE',  ( -5.010620288702242853, 8.003418215864698482, -1.199719254218453823 ) ) ;
#182500 = PRODUCT_DEFINITION_CONTEXT ( 'detailed design', #198672, 'design' ) ;
#182501 = CARTESIAN_POINT ( 'NONE',  ( 6.152912852923398290, 0.8997199139058277284, 1.482343192998013537 ) ) ;
#182502 = CARTESIAN_POINT ( 'NONE',  ( -8.500599126088349777, 12.86119004717103209, 1.040834085586084257E-14 ) ) ;
#182503 = AXIS2_PLACEMENT_3D ( 'NONE', #131892, #52727, #20213 ) ;
#182504 = CARTESIAN_POINT ( 'NONE',  ( 3.063400401570901543, 1.746483293306470674, 1.111379191485066364 ) ) ;
#182505 = CARTESIAN_POINT ( 'NONE',  ( 5.712555019607242990, 2.040694153135207412, 0.5639581637400041814 ) ) ;
#182506 = CARTESIAN_POINT ( 'NONE',  ( 5.178324605415663306, 8.128796908705222535, 1.199719254218462483 ) ) ;
#182507 = CARTESIAN_POINT ( 'NONE',  ( -1.364683531250012516, 4.488541667008091096, -0.7879004041258300672 ) ) ;
#182508 = CARTESIAN_POINT ( 'NONE',  ( 3.098452163322249042, 1.954020348291004794, 0.2456459092235723785 ) ) ;
#182509 = CARTESIAN_POINT ( 'NONE',  ( 0.6504702201592416078, 1.884490048413577368, 0.3244712162126031085 ) ) ;
#182510 = CARTESIAN_POINT ( 'NONE',  ( 5.771479170232404421, 1.361120583587755783, 1.844262159060359174 ) ) ;
#182511 = CARTESIAN_POINT ( 'NONE',  ( 2.631258204695927194, -1.703542010001803275, 0.6570300758180421807 ) ) ;
#182512 = CARTESIAN_POINT ( 'NONE',  ( 4.309512724297349884, 6.121127159803966933, 1.599625672291261402 ) ) ;
#182513 = CARTESIAN_POINT ( 'NONE',  ( 3.809477975315569864, 7.388215371269402532, -0.7216878364870197293 ) ) ;
#182514 = CARTESIAN_POINT ( 'NONE',  ( -6.938021921891187382, 9.117444880338284818, -1.599625672291263179 ) ) ;
#182515 = ORIENTED_EDGE ( 'NONE', *, *, #61767, .F. ) ;
#182516 = EDGE_LOOP ( 'NONE', ( #114127, #94729, #169692, #43455 ) ) ;
#182517 = CARTESIAN_POINT ( 'NONE',  ( 4.342045473679829293, -1.241779438462310203, -1.584497923379190931 ) ) ;
#182518 = CARTESIAN_POINT ( 'NONE',  ( 3.871884822249270108, -1.933460040528666379, 0.3310023857948928838 ) ) ;
#182519 = CARTESIAN_POINT ( 'NONE',  ( -5.845536785786364931, 9.971543350059432598, 0.000000000000000000 ) ) ;
#182520 = CARTESIAN_POINT ( 'NONE',  ( -5.773074481320628948, 5.629675071162500544, 0.000000000000000000 ) ) ;
#182521 = CARTESIAN_POINT ( 'NONE',  ( 0.07536363704230969462, 1.333366039338843789, -2.397125032416930424 ) ) ;
#182523 = CARTESIAN_POINT ( 'NONE',  ( 5.330810035471644781, 0.1327828994084866154, 1.764904742964703122 ) ) ;
#182522 = CARTESIAN_POINT ( 'NONE',  ( 0.06416430596320726876, -1.362578676618180884, 1.585857439420575776 ) ) ;
#182524 = DIRECTION ( 'NONE',  ( -1.000000000000000000, 5.578564026256490882E-16, 2.058387550816952846E-48 ) ) ;
#182525 = B_SPLINE_CURVE_WITH_KNOTS ( 'NONE', 3,
 ( #47147, #28742, #45012, #113263, #179268, #43941 ),
 .UNSPECIFIED., .F., .F.,
 ( 4, 2, 4 ),
 ( 0.000000000000000000, 0.0003168911866439334617, 0.0006337823732878669234 ),
 .UNSPECIFIED. ) ;
#182526 = CARTESIAN_POINT ( 'NONE',  ( 1.816621679704206516, 2.045545470589833492, 0.7867152234099920038 ) ) ;
#182527 = CARTESIAN_POINT ( 'NONE',  ( 0.5205769134342881355, -1.653362465512813184, 0.5437448749807861637 ) ) ;
#182528 = CARTESIAN_POINT ( 'NONE',  ( 6.612626235163189925, 8.737816579155630592, -1.599625672291262513 ) ) ;
#182529 = CARTESIAN_POINT ( 'NONE',  ( 0.2333690889706925009, 5.722554199285137422, -2.647406232470352894 ) ) ;
#182530 = CARTESIAN_POINT ( 'NONE',  ( 0.5919146312290176626, -1.711225830157696137, -0.2159481953097255325 ) ) ;
#182531 = CARTESIAN_POINT ( 'NONE',  ( 0.4393512522801552023, 1.325809523182071237, 1.877307722886724317 ) ) ;
#182532 = CARTESIAN_POINT ( 'NONE',  ( 1.031118135130421498, -1.979082047791239418, 0.9416876394413642437 ) ) ;
#182533 = CARTESIAN_POINT ( 'NONE',  ( 6.204387268089465834, -1.258339971413184433, -1.193046581750532464 ) ) ;
#182534 = CARTESIAN_POINT ( 'NONE',  ( 3.123846942790895476, -2.126788776302591888, 0.5888931905130634359 ) ) ;
#182535 = CONICAL_SURFACE ( 'NONE', #13095, 2.324999999999998845, 0.7853981633974461696 ) ;
#182536 = CARTESIAN_POINT ( 'NONE',  ( 1.727621483090465926, 0.1626789094613217412, -2.165059144495153021 ) ) ;
#182537 = CARTESIAN_POINT ( 'NONE',  ( -1.284279953904152949, 2.952889714876734573, 0.7750000000000152323 ) ) ;
#182538 = CARTESIAN_POINT ( 'NONE',  ( 2.729822841111886333, 0.7574698553451510996, -1.977403127767562552 ) ) ;
#182539 = CARTESIAN_POINT ( 'NONE',  ( 6.727182134110239353, -0.007837387828812587484, 2.289081727344749684 ) ) ;
#182540 = CARTESIAN_POINT ( 'NONE',  ( 5.543948526327937998, 0.7806568236609288114, -1.761304856208524283 ) ) ;
#182541 = EDGE_LOOP ( 'NONE', ( #152807, #212661, #167559, #201708 ) ) ;
#182543 = CARTESIAN_POINT ( 'NONE',  ( 1.499999999999990896, 5.775000000000023448, 1.040834085586084257E-14 ) ) ;
#182542 = CARTESIAN_POINT ( 'NONE',  ( 3.052548088455210973, -1.734419513972422555, 1.498989523525402934 ) ) ;
#182544 = CARTESIAN_POINT ( 'NONE',  ( 4.142179624174931796, 4.791296635414242111, 1.199719254218464037 ) ) ;
#182545 = CARTESIAN_POINT ( 'NONE',  ( 4.143988507271280319, 7.986403691791820414, -0.7998128361456221525 ) ) ;
#182547 = EDGE_CURVE ( 'NONE', #14623, #68331, #81384, .T. ) ;
#182546 = AXIS2_PLACEMENT_3D ( 'NONE', #43451, #41321, #142032 ) ;
#182548 = CARTESIAN_POINT ( 'NONE',  ( 4.705860574468672120, 1.645629519818484932, 1.492201155203516150 ) ) ;
#182549 = CARTESIAN_POINT ( 'NONE',  ( -7.863365906246068349, 9.236643647784308797, -1.082531754730543971 ) ) ;
#182550 = DIRECTION ( 'NONE',  ( -1.000000000000000000, 0.000000000000000000, 0.000000000000000000 ) ) ;
#182551 = CARTESIAN_POINT ( 'NONE',  ( 5.585596099150174965, 7.539614753807099667, -1.443375672974057666 ) ) ;
#182552 = CARTESIAN_POINT ( 'NONE',  ( -9.286972035236635392, 9.937148250638648150, -0.7216878364870267237 ) ) ;
#182553 = CARTESIAN_POINT ( 'NONE',  ( 6.048345925472191631, 7.189396680206621149, 1.082531754730549967 ) ) ;
#182554 = VERTEX_POINT ( 'NONE', #160504 ) ;
#182555 = CARTESIAN_POINT ( 'NONE',  ( 2.848279904836711118, 0.2930702634792031747, -1.994869876753922799 ) ) ;
#182557 = CARTESIAN_POINT ( 'NONE',  ( 0.7958482667242804398, -1.455889974409400045, -1.461266501696573794 ) ) ;
#182556 = CARTESIAN_POINT ( 'NONE',  ( 6.154511665599609493, 9.267681812253174556, 1.199719254218462483 ) ) ;
#182558 = CARTESIAN_POINT ( 'NONE',  ( -11.86239285000045740, 13.87999999999998302, 1.812080536912751283 ) ) ;
#182559 = CARTESIAN_POINT ( 'NONE',  ( 5.682275777458846377, 7.722684055159064975, 1.443375672974064550 ) ) ;
#182560 = DIRECTION ( 'NONE',  ( 0.000000000000000000, 0.000000000000000000, 1.000000000000000000 ) ) ;
#182561 = CARTESIAN_POINT ( 'NONE',  ( -1.364683531250012516, 3.738541667008087099, -0.7879004041258300672 ) ) ;
#182562 = CARTESIAN_POINT ( 'NONE',  ( 3.679775893577118318, -1.080384588543949809, 1.906543112819548913 ) ) ;
#182563 = CARTESIAN_POINT ( 'NONE',  ( 1.758435621656749603, 1.928751379572872571, -0.5880216644931559600 ) ) ;
#182564 = CARTESIAN_POINT ( 'NONE',  ( 0.5031362391596030381, -1.832460416942282011, 0.1798594046882526221 ) ) ;
#182565 = CARTESIAN_POINT ( 'NONE',  ( 5.741781754149911876, 2.289535525127144311, 0.1160191304092756254 ) ) ;
#182566 = CARTESIAN_POINT ( 'NONE',  ( 4.769393013670423009, 1.062472638025207416, 1.503447196605799174 ) ) ;
#182567 = CARTESIAN_POINT ( 'NONE',  ( 8.121497709785879593, 9.433834401960398353, -1.199719254218445830 ) ) ;
#182569 = EDGE_CURVE ( 'NONE', #154238, #38200, #212219, .T. ) ;
#182568 = SURFACE_SIDE_STYLE ('',( #116574 ) ) ;
#182570 = CARTESIAN_POINT ( 'NONE',  ( 4.084828617465196210, -0.1788469021064206521, -1.816781805555576668 ) ) ;
#182571 = CARTESIAN_POINT ( 'NONE',  ( 4.483046177357690176, -2.016033783801042034, -0.04667830911464498911 ) ) ;
#182572 = CARTESIAN_POINT ( 'NONE',  ( -7.666245793523398078, 11.03137162816423356, 1.199719254218453823 ) ) ;
#182574 = CARTESIAN_POINT ( 'NONE',  ( -5.284646014276622950, 9.387447126623207794, -0.7998128361456362523 ) ) ;
#182573 = CARTESIAN_POINT ( 'NONE',  ( 4.733442339874294191, -2.070396585149585356, 0.9127746130930917134 ) ) ;
#182575 = CARTESIAN_POINT ( 'NONE',  ( 6.352575683687115671, 0.6571560004794211318, 2.000881423421707161 ) ) ;
#182576 = CARTESIAN_POINT ( 'NONE',  ( -1.963753466588807894, 3.754052640047090161, -0.4000000000001296963 ) ) ;
#182577 = CARTESIAN_POINT ( 'NONE',  ( 4.914543119725925280, 0.7892175071393169317, 1.914236960262293508 ) ) ;
#182578 = CARTESIAN_POINT ( 'NONE',  ( 10.05067194643221207, 10.62020544712608938, 0.7998128361456462443 ) ) ;
#182579 = CARTESIAN_POINT ( 'NONE',  ( 11.89942855770814312, 11.29999999999999893, 0.6999999999999992895 ) ) ;
#182580 = SHAPE_DEFINITION_REPRESENTATION ( #194171, #135824 ) ;
#182582 = CARTESIAN_POINT ( 'NONE',  ( 2.402848698864976207, 1.547341197487204001, -1.147474368762817498 ) ) ;
#182581 = CARTESIAN_POINT ( 'NONE',  ( -7.343712760096452463, 11.71941532008788833, -0.7998128361456291469 ) ) ;
#182583 = CYLINDRICAL_SURFACE ( 'NONE', #178971, 1.250000000000000000 ) ;
#182584 = CARTESIAN_POINT ( 'NONE',  ( 6.702011354250313246, 0.7569246535186587854, -1.818382958529676019 ) ) ;
#182585 = CARTESIAN_POINT ( 'NONE',  ( 7.862802741282558294, 8.137967717776607657, 0.000000000000000000 ) ) ;
#182586 = CARTESIAN_POINT ( 'NONE',  ( 5.206864636422387171, 6.427350532134703087, -1.171562478298654231 ) ) ;
#182587 = CARTESIAN_POINT ( 'NONE',  ( -2.764973262183167968, 5.313220341600567664, 1.199719254218462483 ) ) ;
#182589 = CARTESIAN_POINT ( 'NONE',  ( 1.846216761830053787, -1.455271069044868693, -1.678405531801461903 ) ) ;
#182588 = CARTESIAN_POINT ( 'NONE',  ( 1.195735321641926197, 1.957225868588155837, -0.8166992996602240318 ) ) ;
#182590 = CARTESIAN_POINT ( 'NONE',  ( 3.838982076996471982, 0.3068427722541127722, 2.083350420514245016 ) ) ;
#182591 = CARTESIAN_POINT ( 'NONE',  ( -6.505933609711270549, 8.683618192786854095, -1.599625672291271394 ) ) ;
#182592 = CARTESIAN_POINT ( 'NONE',  ( 6.103141704446003679, 10.27208242182903142, 0.7998128361456462443 ) ) ;
#182593 = CARTESIAN_POINT ( 'NONE',  ( 2.717183929654675811, -1.705535211757349456, -0.9694657131227711888 ) ) ;
#182594 = CARTESIAN_POINT ( 'NONE',  ( 6.810273232766058449, 6.839740281182199233, 1.040834085586084257E-14 ) ) ;
#182595 = CARTESIAN_POINT ( 'NONE',  ( -4.088362842241233253, 7.522098425605555860, -0.5455919966513862462 ) ) ;
#182596 = CARTESIAN_POINT ( 'NONE',  ( 5.495132332240461714, 5.305409230568988832, 0.7998128361456341429 ) ) ;
#182597 = CARTESIAN_POINT ( 'NONE',  ( -6.455090533882206216, 7.663932056684933158, -1.082531754730549967 ) ) ;
#182598 = CARTESIAN_POINT ( 'NONE',  ( -8.188761592974058701, 8.655902734665618325, -0.7216878364870278340 ) ) ;
#182599 = CARTESIAN_POINT ( 'NONE',  ( 2.742561299210785286, 1.174483946500170184, -1.765453564165630596 ) ) ;
#182600 = CARTESIAN_POINT ( 'NONE',  ( -5.098748287191073203, 8.106234214101666780, 1.199719254218452935 ) ) ;
#182602 = CARTESIAN_POINT ( 'NONE',  ( 4.809014631063706524, -1.576880339463518022, 1.167019128429528374 ) ) ;
#182601 = CARTESIAN_POINT ( 'NONE',  ( -2.954552044183079750E-14, 1.062499999999981126, 1.414508159514567431 ) ) ;
#182603 = CARTESIAN_POINT ( 'NONE',  ( 3.081113354808207916, -0.1575343947536785305, -2.156009052512488200 ) ) ;
#182604 = CARTESIAN_POINT ( 'NONE',  ( 2.542321706073047416, -1.529623444112483632, 1.024600984555257277 ) ) ;
#182605 = UNCERTAINTY_MEASURE_WITH_UNIT (LENGTH_MEASURE( 1.000000000000000082E-05 ), #147972, 'distance_accuracy_value', 'NONE');
#182606 = CARTESIAN_POINT ( 'NONE',  ( -4.209440762792112878, 7.367024337791516331, -0.8326445619948764643 ) ) ;
#182607 = CARTESIAN_POINT ( 'NONE',  ( -1.364683531250000748, -0.9281249996585805295, 0.000000000000000000 ) ) ;
#182608 = CARTESIAN_POINT ( 'NONE',  ( 4.822041096100106117, 1.666637052750892911, 0.5010418475075908429 ) ) ;
#182610 = AXIS2_PLACEMENT_3D ( 'NONE', #182132, #99840, #120427 ) ;
#182609 = CARTESIAN_POINT ( 'NONE',  ( 1.000000047849771923, 15.00000000000000888, -11.64874984998672502 ) ) ;
#182611 = CARTESIAN_POINT ( 'NONE',  ( 6.480434237652135998, 6.662854153456708950, 0.7216878364870317197 ) ) ;
#182612 = CARTESIAN_POINT ( 'NONE',  ( -10.91449010664383223, 5.922815305582411760, 6.336942051301835299 ) ) ;
#182613 = CARTESIAN_POINT ( 'NONE',  ( 1.973706723050288936, 2.068691090354588091, -0.6273066937243013674 ) ) ;
#182614 = CARTESIAN_POINT ( 'NONE',  ( 4.763045971468515383, -2.015604388477490350, -0.05228862439247972116 ) ) ;
#182615 = DIRECTION ( 'NONE',  ( 0.000000000000000000, 0.000000000000000000, 1.000000000000000000 ) ) ;
#182616 = CARTESIAN_POINT ( 'NONE',  ( 1.481558191429487970, 1.997200094811113491, -0.8276061316847342919 ) ) ;
#182617 =( BOUNDED_CURVE ( )  B_SPLINE_CURVE ( 2, ( #1219, #168016, #169075 ),
 .UNSPECIFIED., .F., .T. ) 
 B_SPLINE_CURVE_WITH_KNOTS ( ( 3, 3 ),
 ( 0.1229783203405389463, 0.1249999999999998751 ),
 .UNSPECIFIED. ) 
 CURVE ( )  GEOMETRIC_REPRESENTATION_ITEM ( )  RATIONAL_B_SPLINE_CURVE ( ( 0.9330713687540070911, 0.9349951081471579162, 0.9999999999999960032 ) ) 
 REPRESENTATION_ITEM ( '' )  );
#182618 = CARTESIAN_POINT ( 'NONE',  ( 2.869950281991093810, 1.053363813896515788, 1.666286737264175866 ) ) ;
#182619 = CARTESIAN_POINT ( 'NONE',  ( 6.509000000000012776, 6.036089120385641493, 2.694901645009006863 ) ) ;
#182620 = CARTESIAN_POINT ( 'NONE',  ( 3.175267148988625721, 1.234016112977231794, 1.499580727898646604 ) ) ;
#182623 = VERTEX_POINT ( 'NONE', #177831 ) ;
#182622 = CARTESIAN_POINT ( 'NONE',  ( -3.472296738875691346, 6.104744391113324120, 1.082531754730549967 ) ) ;
#182621 = CARTESIAN_POINT ( 'NONE',  ( -9.286972035236626510, 11.85788667924133399, -1.443375672974058777 ) ) ;
#182624 = CARTESIAN_POINT ( 'NONE',  ( -7.445362632559989535, 8.715286488521982733, 1.199719254218452047 ) ) ;
#182625 = DIRECTION ( 'NONE',  ( 0.000000000000000000, 0.000000000000000000, 1.000000000000000000 ) ) ;
#182627 = VERTEX_POINT ( 'NONE', #12109 ) ;
#182626 = CARTESIAN_POINT ( 'NONE',  ( -6.493429226302317225, 6.540365283632955773, 0.7998128361456341429 ) ) ;
#182628 = CARTESIAN_POINT ( 'NONE',  ( -8.446366511189330240, 12.79791866312216442, 0.7216878364870317197 ) ) ;
#182629 = CARTESIAN_POINT ( 'NONE',  ( 0.8685540286928781217, 1.089157903960279672, 1.919174906450902274 ) ) ;
#182631 = EDGE_CURVE ( 'NONE', #57833, #126082, #123683, .T. ) ;
#182630 = CARTESIAN_POINT ( 'NONE',  ( 1.001543065824772753E-15, -2.821874999522044458, 3.793834371823811669 ) ) ;
#182632 = CARTESIAN_POINT ( 'NONE',  ( 4.891432378139471737, -1.795214109662087942, 0.7913882323652280393 ) ) ;
#182633 = CARTESIAN_POINT ( 'NONE',  ( 1.512342498431101134, -1.897697209584522815, 0.6819976561535445736 ) ) ;
#182634 = ORIENTED_EDGE ( 'NONE', *, *, #62843, .T. ) ;
#182635 = CARTESIAN_POINT ( 'NONE',  ( 3.520818605202329810, 0.3149718393082919232, 2.093694903831443188 ) ) ;
#182636 = CARTESIAN_POINT ( 'NONE',  ( -1.499999999999997780, 2.431250000682817713, 1.214306433183764966E-14 ) ) ;
#182638 = CARTESIAN_POINT ( 'NONE',  ( -4.693093728624763372, 8.627026450037540428, 0.7998128361456481317 ) ) ;
#182637 = CARTESIAN_POINT ( 'NONE',  ( 9.500350659417458488, -7.217450603046484225, -0.002323312720761049489 ) ) ;
#182639 = CARTESIAN_POINT ( 'NONE',  ( 4.505690185649424251, -0.7896136771840707169, -1.663358820747300237 ) ) ;
#182640 = ORIENTED_EDGE ( 'NONE', *, *, #117124, .F. ) ;
#182641 = UNCERTAINTY_MEASURE_WITH_UNIT (LENGTH_MEASURE( 1.000000000000000082E-05 ), #164668, 'distance_accuracy_value', 'NONE');
#182642 = CARTESIAN_POINT ( 'NONE',  ( -8.565000355531095622, 11.01558638625153286, -1.599625672291263179 ) ) ;
#182643 = CARTESIAN_POINT ( 'NONE',  ( 0.4516138619287866085, 3.070015318549083272, 0.4124855346667386513 ) ) ;
#182644 = CARTESIAN_POINT ( 'NONE',  ( 4.763993809689464065, 0.6627061821620899851, -2.014485251161435286 ) ) ;
#182645 = CARTESIAN_POINT ( 'NONE',  ( -0.2106725631050176684, -0.004273297132624804921, -2.003483006309700887 ) ) ;
#182646 = CARTESIAN_POINT ( 'NONE',  ( 6.582647274634798151, 7.638508894284114170, 1.199719254218462483 ) ) ;
#182647 = CARTESIAN_POINT ( 'NONE',  ( 6.028604891774052454, 1.984808026635048961, 0.5540661066990509864 ) ) ;
#182650 = CARTESIAN_POINT ( 'NONE',  ( 2.981803241483144351, -1.814435276338403735, -0.3121031562058202424 ) ) ;
#182649 = CARTESIAN_POINT ( 'NONE',  ( 0.6778921365368529850, -0.9907528278601520633, -1.575212976145045518 ) ) ;
#182648 = CARTESIAN_POINT ( 'NONE',  ( 10.56513397747884397, 12.34099903485656213, 3.405015282931167508 ) ) ;
#182651 = CARTESIAN_POINT ( 'NONE',  ( 9.582915646760733708, 10.07448976417602893, 0.7998128361456462443 ) ) ;
#182652 = CARTESIAN_POINT ( 'NONE',  ( 1.253848497529134409, -2.775557561562891351E-14, 0.5275650105875644424 ) ) ;
#182653 = CARTESIAN_POINT ( 'NONE',  ( -5.935437387732586778, 10.14670372898850381, -0.7998128361456362523 ) ) ;
#182654 = CARTESIAN_POINT ( 'NONE',  ( -0.08000000000000194456, -8.407420853759283830, -10.91970695577494865 ) ) ;
#182655 = AXIS2_PLACEMENT_3D ( 'NONE', #123754, #107479, #74913 ) ;
#182656 = CARTESIAN_POINT ( 'NONE',  ( 2.069229996397306426, -2.018448871333050842, -0.8927042923378907258 ) ) ;
#182657 = CARTESIAN_POINT ( 'NONE',  ( 4.358826825731692445, -1.680320932299755210, 1.515136896344573270 ) ) ;
#182658 = CARTESIAN_POINT ( 'NONE',  ( -8.365017589951714072, 8.861534731139549592, 1.040834085586084257E-14 ) ) ;
#182659 = CARTESIAN_POINT ( 'NONE',  ( 5.238451434589118882, 1.072694688086765158, -1.459716015685054602 ) ) ;
#182660 = CARTESIAN_POINT ( 'NONE',  ( 5.770691199759951040, -0.2880491948782157308, -1.893834403066462446 ) ) ;
#182661 = CARTESIAN_POINT ( 'NONE',  ( 0.6823417656249917140, 5.155208333674749177, 1.181850606188765695 ) ) ;
#182662 = CARTESIAN_POINT ( 'NONE',  ( 4.592568387165754551, -0.4099775813008778025, -1.825014511474598589 ) ) ;
#182663 = CARTESIAN_POINT ( 'NONE',  ( 5.371493315669001234, -0.2729949515532895110, 1.840801060123838706 ) ) ;
#182664 = CARTESIAN_POINT ( 'NONE',  ( 0.09999999999985714760, -10.00000000000009592, 9.579478065114059859 ) ) ;
#182665 = CARTESIAN_POINT ( 'NONE',  ( 5.910986595158141732, 1.562736066445655769, 0.8308124446602130897 ) ) ;
#182666 = CARTESIAN_POINT ( 'NONE',  ( 0.2511858651975951151, 0.1928294586405615574, -2.007256720055437871 ) ) ;
#182668 = CARTESIAN_POINT ( 'NONE',  ( 1.383574010005955701, 1.945322680536746063, -0.8074913105669545565 ) ) ;
#182667 = CARTESIAN_POINT ( 'NONE',  ( -3.212919216314315207, 5.731860938133201522, 1.082531754730560403 ) ) ;
#182669 = CARTESIAN_POINT ( 'NONE',  ( 8.075853055234393452, 12.57357899774884658, 0.7998128361456462443 ) ) ;
#182671 = CARTESIAN_POINT ( 'NONE',  ( -8.306341666666730461, 12.84248237775322643, 1.040834085586084257E-14 ) ) ;
#182670 = CARTESIAN_POINT ( 'NONE',  ( 1.673838217086941410E-16, 2.099999999999997868, 2.500000000000000000 ) ) ;
#182672 = DIRECTION ( 'NONE',  ( -5.551115123125764829E-17, 0.000000000000000000, 1.000000000000000000 ) ) ;
#182674 = EDGE_CURVE ( 'NONE', #86477, #6643, #63976, .T. ) ;
#182673 = CARTESIAN_POINT ( 'NONE',  ( 2.127218876063118103, 1.806125448131710387, 0.9042179360667053079 ) ) ;
#182675 = CARTESIAN_POINT ( 'NONE',  ( -0.6823417656250003738, 1.717708333674752730, -1.181850606188749264 ) ) ;
#182676 = CARTESIAN_POINT ( 'NONE',  ( 6.620655732516648406, 2.482285041548700111, 2.111775279032622521 ) ) ;
#182677 = CARTESIAN_POINT ( 'NONE',  ( 4.467575310902914154, 5.170924936596891008, 1.199719254218464037 ) ) ;
#182678 = VERTEX_POINT ( 'NONE', #107367 ) ;
#182679 = CARTESIAN_POINT ( 'NONE',  ( 2.144033130777025065, 0.8294244109963678779, -1.996327601563187670 ) ) ;
#182680 = DIRECTION ( 'NONE',  ( 1.000000000000000000, 1.084202172485501594E-14, 0.000000000000000000 ) ) ;
#182683 = DIRECTION ( 'NONE',  ( -0.7592566023652994600, 0.6507913734559651608, 0.000000000000000000 ) ) ;
#182682 = CARTESIAN_POINT ( 'NONE',  ( -5.378281411895262210, 4.339595938922584217, -2.499999999999995559 ) ) ;
#182681 = CARTESIAN_POINT ( 'NONE',  ( 4.411198876399872404, 6.239761003923544713, -1.599625672291273171 ) ) ;
#182684 = CARTESIAN_POINT ( 'NONE',  ( 9.910647101465253073, 11.62513837554007168, -1.082531754730537088 ) ) ;
#182685 = CARTESIAN_POINT ( 'NONE',  ( 11.86686399458719521, 9.990712702246625554, -1.056461745586973588 ) ) ;
#182686 = CARTESIAN_POINT ( 'NONE',  ( -7.375272376154096143, 8.667201196010339004, -1.082531754730544860 ) ) ;
#182687 = EDGE_CURVE ( 'NONE', #199511, #133821, #53756, .T. ) ;
#182688 = CARTESIAN_POINT ( 'NONE',  ( 0.5740950506661415265, -1.212703583203307511, 1.825263377225619266 ) ) ;
#182689 = CARTESIAN_POINT ( 'NONE',  ( 0.4396101492294202662, 7.376551424357187692, 2.043156636846811036 ) ) ;
#182690 = CARTESIAN_POINT ( 'NONE',  ( 1.464152659907109966, 2.228779883755461100, -0.3883945716754066968 ) ) ;
#182691 = CARTESIAN_POINT ( 'NONE',  ( -6.886651960737580680, 10.12184548991413457, -1.199719254218440723 ) ) ;
#182692 = CARTESIAN_POINT ( 'NONE',  ( -3.267151830768946663, 6.755501535964989479, -0.7216878364870257245 ) ) ;
#182693 = CARTESIAN_POINT ( 'NONE',  ( 1.364683531249988535, 3.176041667008084435, 0.7879004041258500513 ) ) ;
#182694 = DIRECTION ( 'NONE',  ( 0.000000000000000000, 1.000000000000000000, 0.000000000000000000 ) ) ;
#182695 = CARTESIAN_POINT ( 'NONE',  ( -6.009258394948636914E-15, 11.18749999999999645, -1.732050807568875195 ) ) ;
#182696 = CARTESIAN_POINT ( 'NONE',  ( 6.943184063974162434, 9.193743722760251202, -1.443375672974064550 ) ) ;
#182697 = CARTESIAN_POINT ( 'NONE',  ( 3.250976011129117715, -1.444759545231928843, -1.021753751062564497 ) ) ;
#182698 = PRESENTATION_LAYER_ASSIGNMENT (  '', '', ( #61646 ) ) ;
#182699 =( BOUNDED_SURFACE ( )  B_SPLINE_SURFACE ( 3, 2, ( 
 ( #101941, #149628, #135521 ),
 ( #197301, #18543, #133412 ),
 ( #48941, #199419, #32674 ),
 ( #201542, #98753, #117185 ),
 ( #183186, #19613, #34791 ),
 ( #164810, #151773, #3345 ),
 ( #16402, #82480, #69414 ),
 ( #150709, #100866, #166952 ),
 ( #153898, #5467, #27888 ),
 ( #137657, #110277, #87828 ),
 ( #158962, #76631, #71549 ),
 ( #127620, #209818, #203677 ),
 ( #190372, #26814, #152825 ),
 ( #142746, #58258, #176286 ),
 ( #124414, #38011, #170132 ),
 ( #160027, #191437, #141686 ),
 ( #70473, #10557, #193584 ),
 ( #175229, #192505, #93985 ) ),
 .UNSPECIFIED., .F., .F., .F. ) 
 B_SPLINE_SURFACE_WITH_KNOTS ( ( 4, 2, 2, 2, 2, 2, 2, 2, 4 ),
 ( 3, 3 ),
 ( 2.412349833780247366E-18, 8.835779862913541985E-05, 0.0001767155972582684273, 0.0003534311945165344152, 0.0007068623890330664452, 0.001060293583549598529, 0.001237009180807864626, 0.001325366979436997565, 0.001413724778066130505 ),
 ( 0.000000000000000000, 1.000000000000000000 ),
 .UNSPECIFIED. ) 
 GEOMETRIC_REPRESENTATION_ITEM ( )  RATIONAL_B_SPLINE_SURFACE ( (
 ( 1.000000000000000000, 0.8509629433930240294, 1.000000000000000000),
 ( 1.000000000000000000, 0.8498006689708330619, 1.000000000000000000),
 ( 1.000000000000000000, 0.8320552336068607335, 1.000000000000000000),
 ( 1.000000000000000000, 0.8099185496895315861, 1.000000000000000000),
 ( 1.000000000000000000, 0.8026556248574672203, 1.000000000000000000),
 ( 1.000000000000000000, 0.7864057361600924612, 1.000000000000000000),
 ( 1.000000000000000000, 0.7820376697136646182, 1.000000000000000000),
 ( 1.000000000000000000, 0.7712304172528938739, 1.000000000000000000),
 ( 1.000000000000000000, 0.7693781127658743113, 1.000000000000000000),
 ( 1.000000000000000000, 0.7693828318226363372, 1.000000000000000000),
 ( 1.000000000000000000, 0.7713025106372017881, 1.000000000000000000),
 ( 1.000000000000000000, 0.7820120508712598006, 1.000000000000000000),
 ( 1.000000000000000000, 0.7865355378789550267, 1.000000000000000000),
 ( 1.000000000000000000, 0.8025478247494930439, 1.000000000000000000),
 ( 1.000000000000000000, 0.8098425554835826379, 1.000000000000000000),
 ( 1.000000000000000000, 0.8320142507518490937, 1.000000000000000000),
 ( 1.000000000000000000, 0.8496692035686509437, 1.000000000000000000),
 ( 1.000000000000000000, 0.8509629433917188512, 1.000000000000000000) ) ) 
 REPRESENTATION_ITEM ( '' )  SURFACE ( )  );
#182700 = CARTESIAN_POINT ( 'NONE',  ( 0.1125219251090440048, -0.9011682483198739657, -1.901734387108368063 ) ) ;
#182701 = CARTESIAN_POINT ( 'NONE',  ( -1.402160292154681736E-14, 14.98437500034140157, 1.575800808251682339 ) ) ;
#182702 = ORIENTED_EDGE ( 'NONE', *, *, #57965, .F. ) ;
#182703 = CARTESIAN_POINT ( 'NONE',  ( -5.529746549527323474, 7.544733289238903851, -1.599625672291271394 ) ) ;
#182704 = CARTESIAN_POINT ( 'NONE',  ( 5.483999976877721672, -2.016598147233912730, 0.002826481282774962345 ) ) ;
#182706 = ORIENTED_EDGE ( 'NONE', *, *, #208798, .F. ) ;
#182705 = CARTESIAN_POINT ( 'NONE',  ( 4.798965708296219823, -0.2289270959113845205, -1.797013726050479709 ) ) ;
#182707 = CARTESIAN_POINT ( 'NONE',  ( 2.606148294764852213, -0.7140300644919925777, -1.729217693616967644 ) ) ;
#182708 = CARTESIAN_POINT ( 'NONE',  ( 2.272408084759574454, -0.9721198248324285363, -1.827787434591138238 ) ) ;
#182709 = EDGE_CURVE ( 'NONE', #98321, #190021, #147475, .T. ) ;
#182710 = CARTESIAN_POINT ( 'NONE',  ( -5.763624699140868834, 9.738329559057408602, -0.7216878364870338292 ) ) ;
#182711 = CARTESIAN_POINT ( 'NONE',  ( 2.197387184563174944, 1.746976956643018442, -0.7784620831182070821 ) ) ;
#182712 = CARTESIAN_POINT ( 'NONE',  ( 1.499999999999959588, 8.500000000000000000, -10.89724735885168805 ) ) ;
#182713 = CARTESIAN_POINT ( 'NONE',  ( -9.857748099689047194, 5.276144085703439401, -6.217795349555793827 ) ) ;
#182714 = CARTESIAN_POINT ( 'NONE',  ( 1.419999999999989049, 6.120000000000041851, -2.499999999999995115 ) ) ;
#182715 = CARTESIAN_POINT ( 'NONE',  ( -1.364683531250010295, 3.842708333674751398, 0.7879004041258379498 ) ) ;
#182716 = CARTESIAN_POINT ( 'NONE',  ( 0.5274218815167727170, -0.2782315536139517431, 1.891897276498944347 ) ) ;
#182717 = CARTESIAN_POINT ( 'NONE',  ( 5.641601317062233001, 7.675230518029648508, -1.443375672974078761 ) ) ;
#182718 = CARTESIAN_POINT ( 'NONE',  ( 1.750371521623844462, -1.952110535733902585, -0.1955497077021361163 ) ) ;
#182719 = CYLINDRICAL_SURFACE ( 'NONE', #172175, 1.250000000000000000 ) ;
#182720 = CARTESIAN_POINT ( 'NONE',  ( -4.447956913735107598, 7.346977611736363656, 1.199719254218452935 ) ) ;
#182721 = CARTESIAN_POINT ( 'NONE',  ( 5.168275554957600271, 2.118074532352266282, -0.1063875075708180934 ) ) ;
#182723 = CARTESIAN_POINT ( 'NONE',  ( -11.69243366784185945, 8.407932920124673970, 1.097391832464843286 ) ) ;
#182722 = CARTESIAN_POINT ( 'NONE',  ( 9.236128959407556849, 11.79856975744075598, -1.599625672291262513 ) ) ;
#182724 = CARTESIAN_POINT ( 'NONE',  ( 0.3154175708385241750, -1.835744252435017598, 0.3582649291258357960 ) ) ;
#182725 = CARTESIAN_POINT ( 'NONE',  ( -1.364683531250012516, 2.738541667008090208, -0.7879004041258289570 ) ) ;
#182726 = CARTESIAN_POINT ( 'NONE',  ( 1.564699064445768784, 0.6353654490140858702, 1.910354371721780797 ) ) ;
#182728 = CARTESIAN_POINT ( 'NONE',  ( 0.8084048693777341477, 1.257526981011043654, -1.703196666993979536 ) ) ;
#182727 = CARTESIAN_POINT ( 'NONE',  ( -6.941411460516810017, 8.161030127766803588, 1.082531754730549967 ) ) ;
#182729 = CARTESIAN_POINT ( 'NONE',  ( 11.87808349579980671, 6.802413298898714267, -1.723793258986091370 ) ) ;
#182730 = CARTESIAN_POINT ( 'NONE',  ( 2.523957353938070192, 2.030885678308389952, -0.4015143504868187718 ) ) ;
#182731 = CARTESIAN_POINT ( 'NONE',  ( 3.379725431556547477, 7.165039780116438273, -1.734723475976807094E-15 ) ) ;
#182732 = CARTESIAN_POINT ( 'NONE',  ( 5.194709132691408549, 6.089524072008651423, 1.199719254218452935 ) ) ;
#182733 = ORIENTED_EDGE ( 'NONE', *, *, #70182, .F. ) ;
#182735 = CARTESIAN_POINT ( 'NONE',  ( 2.869522067586683711, 6.499526178826442013, 0.7998128361456362523 ) ) ;
#182734 = CARTESIAN_POINT ( 'NONE',  ( 6.193323979940683621, -0.7056316722037699884, 1.968093674265839477 ) ) ;
#182738 = ORIENTED_EDGE ( 'NONE', *, *, #43463, .F. ) ;
#182737 = CARTESIAN_POINT ( 'NONE',  ( 2.930093016812723050, -0.8946826049299866357, -1.575034454935933859 ) ) ;
#182736 = CARTESIAN_POINT ( 'NONE',  ( 4.770415466175468744, -1.191763575130764696, 1.382976834283907053 ) ) ;
#182739 = CARTESIAN_POINT ( 'NONE',  ( 10.06423010004587759, 10.63602329300870153, 0.000000000000000000 ) ) ;
#182740 = COLOUR_RGB ( '', 0.31764706, 0.68627451, 0.89019608) ;
#182741 = CARTESIAN_POINT ( 'NONE',  ( 6.890000000000050306, -0.002781820520068867264, 1.999840353888074240 ) ) ;
#182742 = CARTESIAN_POINT ( 'NONE',  ( 9.309616742661452449, 13.13421366227010445, -6.702222026789643294 ) ) ;
#182743 = CARTESIAN_POINT ( 'NONE',  ( 5.719807747550186505, -2.154180246964752410, 0.4782370604126117142 ) ) ;
#182744 = CARTESIAN_POINT ( 'NONE',  ( -1.402160292154681736E-14, 10.23437500034139447, 1.575800808251682339 ) ) ;
#182745 = ORIENTED_EDGE ( 'NONE', *, *, #22206, .T. ) ;
#182746 = CARTESIAN_POINT ( 'NONE',  ( 4.037688526304391345, -1.829018870347882242, 0.5580751363460645376 ) ) ;
#182747 = CARTESIAN_POINT ( 'NONE',  ( -4.298098390732130625, 4.973201863064262263, 1.199719254218462483 ) ) ;
#182748 = CARTESIAN_POINT ( 'NONE',  ( 7.121056995675668411, 9.330985799753529264, -1.599625672291262513 ) ) ;
#182749 = CARTESIAN_POINT ( 'NONE',  ( -1.360316468750038865, 1.192708333674735721, 0.7853790794158880262 ) ) ;
#182750 = CARTESIAN_POINT ( 'NONE',  ( 4.324687812634887329, 6.068555086205916105, 1.443375672974062551 ) ) ;
#182751 = CARTESIAN_POINT ( 'NONE',  ( -0.4800000000000244071, 2.999999999999999112, 2.500000000000000444 ) ) ;
#182752 = DIRECTION ( 'NONE',  ( 0.9782075119096779181, 0.1245777785628398998, -0.1661037047504532738 ) ) ;
#182753 = CARTESIAN_POINT ( 'NONE',  ( -0.02423404108400224397, -1.785672699080865566, -0.4486397487279416563 ) ) ;
#182754 = VECTOR ( 'NONE', #154993, 1000.000000000000000 ) ;
#182755 = DIRECTION ( 'NONE',  ( 0.000000000000000000, 1.000000000000000000, 0.000000000000000000 ) ) ;
#182756 = CARTESIAN_POINT ( 'NONE',  ( 3.690566713891149320, -0.3619836066245524786, -1.835009008997898539 ) ) ;
#182757 = CARTESIAN_POINT ( 'NONE',  ( 7.343676480457483002, 8.596652644402405841, -1.199719254218452047 ) ) ;
#182758 = CARTESIAN_POINT ( 'NONE',  ( 6.764690511086886823E-16, -5.511313137147262786, 11.00000000000000178 ) ) ;
#182759 = CARTESIAN_POINT ( 'NONE',  ( -5.748293942514169252, 9.650167333001109071, -0.7216878364870207285 ) ) ;
#182760 = CARTESIAN_POINT ( 'NONE',  ( 3.798255590122797898, 7.583048621785260401, -0.7998128361456221525 ) ) ;
#182761 = CARTESIAN_POINT ( 'NONE',  ( 6.860220180191213935, -2.069926439015772335, 0.04462916171246725239 ) ) ;
#182763 = CARTESIAN_POINT ( 'NONE',  ( 2.214470461757975794, 1.956567829827577931, 0.4871813834786202224 ) ) ;
#182762 = B_SPLINE_CURVE_WITH_KNOTS ( 'NONE', 3,
 ( #145316, #211320, #148477, #62944 ),
 .UNSPECIFIED., .F., .F.,
 ( 4, 4 ),
 ( 0.000000000000000000, 0.0002908967400263822562 ),
 .UNSPECIFIED. ) ;
#182764 = CARTESIAN_POINT ( 'NONE',  ( -9.345647958521597687, 9.797677461230342999, 0.7998128361456462443 ) ) ;
#182765 = CARTESIAN_POINT ( 'NONE',  ( 6.530187263637528439, 7.647581891445782709, -1.199719254218452047 ) ) ;
#182766 = CARTESIAN_POINT ( 'NONE',  ( 6.772457744868908947, -7.185026885899450377, 6.662118508819615315 ) ) ;
#182767 = CARTESIAN_POINT ( 'NONE',  ( 2.396645607016957502, 1.759237466006560391, -1.306522788049699679 ) ) ;
#182768 = CARTESIAN_POINT ( 'NONE',  ( 6.621730190220365131, -1.769489810573118049, 0.4491385735008179836 ) ) ;
#182769 = CARTESIAN_POINT ( 'NONE',  ( -4.946027110887008860, 4.664786472323266153, -0.7998128361456221525 ) ) ;
#182770 = DIRECTION ( 'NONE',  ( -0.000000000000000000, -1.000000000000000000, -0.000000000000000000 ) ) ;
#182771 = CARTESIAN_POINT ( 'NONE',  ( 5.397554552016226914, 6.430140077841320689, 1.082531754730549078 ) ) ;
#182772 = CARTESIAN_POINT ( 'NONE',  ( 7.736899214892750010, 12.17813285068358020, 1.040834085586084257E-14 ) ) ;
#182773 = CARTESIAN_POINT ( 'NONE',  ( 2.866659414285625651, 5.431854185720147221, -1.199719254218446718 ) ) ;
#182774 = CARTESIAN_POINT ( 'NONE',  ( 6.373741612200162443, 8.529394195690610303, 1.443375672974065660 ) ) ;
#182775 = ORIENTED_EDGE ( 'NONE', *, *, #178800, .T. ) ;
#182777 = CARTESIAN_POINT ( 'NONE',  ( 0.6451818603588607148, 0.1503996631540445994, 2.007543313942860674 ) ) ;
#182776 = CARTESIAN_POINT ( 'NONE',  ( 4.159580895514263688, 0.8717668643758098579, 1.621812032879976329 ) ) ;
#182778 = CARTESIAN_POINT ( 'NONE',  ( 2.689158180196444814, -1.321807234245642615, -1.880123443969876629 ) ) ;
#182780 = CARTESIAN_POINT ( 'NONE',  ( 1.428301029171385794, -1.185968821734217027, 1.434052760600286858 ) ) ;
#182779 = CARTESIAN_POINT ( 'NONE',  ( 4.229780737783593203, 4.037091736943370535, -0.7216878364870188411 ) ) ;
#182781 = CARTESIAN_POINT ( 'NONE',  ( -3.285556943749998737, -3.230208332855375897, 1.896917185911908499 ) ) ;
#182782 = CARTESIAN_POINT ( 'NONE',  ( -6.091691091241777656, 6.001394449403842479, 0.7998128361456341429 ) ) ;
#182783 = DIRECTION ( 'NONE',  ( 1.000000000000000000, 0.000000000000000000, 0.000000000000000000 ) ) ;
#182784 = CARTESIAN_POINT ( 'NONE',  ( 4.869353489999923568, -1.618680692612521455, -1.018082601613921723 ) ) ;
#182785 = CARTESIAN_POINT ( 'NONE',  ( -7.537443334193545397, 10.88110209227943770, -1.199719254218446718 ) ) ;
#182786 = CARTESIAN_POINT ( 'NONE',  ( 6.307155384238837037, 6.868572428096745064, 0.7081091520576547893 ) ) ;
#182787 = CARTESIAN_POINT ( 'NONE',  ( -7.295696057929500711, 7.684269287105433222, 0.7216878364870317197 ) ) ;
#182789 = CARTESIAN_POINT ( 'NONE',  ( 2.061206331123175861, 0.3224310286589862629, -1.842498087946140561 ) ) ;
#182788 = CARTESIAN_POINT ( 'NONE',  ( 3.685174051874222201, 1.515783366363635531, 1.440268600269165589 ) ) ;
#182790 = CARTESIAN_POINT ( 'NONE',  ( 6.643132081016111634, 9.733775946952057723, 1.082531754730558626 ) ) ;
#182791 = CARTESIAN_POINT ( 'NONE',  ( 0.6823417656249917140, 5.405208333674749177, 1.181850606188765695 ) ) ;
#182792 = CARTESIAN_POINT ( 'NONE',  ( 5.530750200611445067, -1.661959182355336795, 0.7928504710919548337 ) ) ;
#182793 = CARTESIAN_POINT ( 'NONE',  ( 4.359110081993588182, 5.044382169536003602, -1.199719254218452047 ) ) ;
#182795 = CARTESIAN_POINT ( 'NONE',  ( 5.529027716274630855, 5.344953845275508542, 1.040834085586084257E-14 ) ) ;
#182794 = DIRECTION ( 'NONE',  ( 0.9885327375000381167, 0.000000000000000000, 0.1510067114093955609 ) ) ;
#182796 = CARTESIAN_POINT ( 'NONE',  ( 4.283650633623343751, 1.129305773815322711, 1.303882612223838500 ) ) ;
#182797 = CARTESIAN_POINT ( 'NONE',  ( -5.554036483092550824, 9.631459663583308739, -0.7998128361456231517 ) ) ;
#182798 = CARTESIAN_POINT ( 'NONE',  ( 0.2286474287733000488, 1.729290747967014097, 0.1301698663358965002 ) ) ;
#182799 = CARTESIAN_POINT ( 'NONE',  ( -1.403499169903600574, 7.376709478543776122, 4.304123474983186703 ) ) ;
#182800 = CARTESIAN_POINT ( 'NONE',  ( 6.983263157960365675, 2.037486384657179350, 2.358487060789053569 ) ) ;
#182801 = CIRCLE ( 'NONE', #172473, 10.99999999999733369 ) ;
#182802 = DIRECTION ( 'NONE',  ( -0.7592566023653004592, 0.6507913734559639396, 0.000000000000000000 ) ) ;
#182803 = CARTESIAN_POINT ( 'NONE',  ( 4.627881963378519536, 2.107464937132212501, -0.5213077441503320975 ) ) ;
#182804 = CARTESIAN_POINT ( 'NONE',  ( 3.633261591126951018, -1.686358373764598406, 0.7000054678709469735 ) ) ;
#182805 = CARTESIAN_POINT ( 'NONE',  ( 1.481223165768187133, -0.05357505548480785695, 1.961209554040027170 ) ) ;
#182806 = CARTESIAN_POINT ( 'NONE',  ( 6.087133394233009476, 1.761630753581880704, 1.174362570269470218 ) ) ;
#182807 = EDGE_LOOP ( 'NONE', ( #204450, #45557, #144084, #4637 ) ) ;
#182809 = CARTESIAN_POINT ( 'NONE',  ( -1.364683531250012516, 3.342708333674756727, 0.7879004041258379498 ) ) ;
#182808 = CARTESIAN_POINT ( 'NONE',  ( 5.548434679399758984, -1.809038938731177160, 1.407827746306972827 ) ) ;
#182810 = CARTESIAN_POINT ( 'NONE',  ( 7.214910300766615769, 11.56914578420308715, -0.7998128361456291469 ) ) ;
#182811 = EDGE_CURVE ( 'NONE', #129023, #82463, #194920, .T. ) ;
#182812 = CARTESIAN_POINT ( 'NONE',  ( 1.436355765274465623, -1.180822252328097344, -1.761085815303937929 ) ) ;
#182813 = CARTESIAN_POINT ( 'NONE',  ( -5.585596099150199834, 5.618876325204420930, -0.7216878364870207285 ) ) ;
#182814 = CARTESIAN_POINT ( 'NONE',  ( 4.229780737783593203, 4.037091736943370535, -0.7216878364870188411 ) ) ;
#182815 = CARTESIAN_POINT ( 'NONE',  ( -5.409340101728186134, 5.413244328212063472, 0.7216878364870317197 ) ) ;
#182816 =( GEOMETRIC_REPRESENTATION_CONTEXT ( 3 ) GLOBAL_UNCERTAINTY_ASSIGNED_CONTEXT ( ( #148250 ) ) GLOBAL_UNIT_ASSIGNED_CONTEXT ( ( #121366, #171092, #58419 ) ) REPRESENTATION_CONTEXT ( 'NONE', 'WORKASPACE' ) );
#182817 = CARTESIAN_POINT ( 'NONE',  ( 6.455955546751245500, -0.7393474466994474081, 2.041418194955111787 ) ) ;
#182819 = CARTESIAN_POINT ( 'NONE',  ( 1.499999999999997113, 12.42708333401612819, -0.8660254037844378194 ) ) ;
#182818 = CARTESIAN_POINT ( 'NONE',  ( 6.983263157960331036, 2.967600560354208383, 2.406739638166929041 ) ) ;
#182821 = ORIENTED_EDGE ( 'NONE', *, *, #117712, .T. ) ;
#182820 = CARTESIAN_POINT ( 'NONE',  ( 1.629831963231648029, -0.2677717415913836718, 2.205032603725831652 ) ) ;
#182822 = CARTESIAN_POINT ( 'NONE',  ( 6.012342310302175363, -1.897698807000438359, 0.6819931642896917001 ) ) ;
#182824 = CARTESIAN_POINT ( 'NONE',  ( 4.258677893805890236, -0.6421077783588696741, -1.960174235369451123 ) ) ;
#182823 = CARTESIAN_POINT ( 'NONE',  ( 3.388648328411762556, 6.040841252200647382, 1.199719254218462483 ) ) ;
#182826 = CARTESIAN_POINT ( 'NONE',  ( 2.665787487727776295, -3.982249430249628297, -2.473491247225932721 ) ) ;
#182825 = CARTESIAN_POINT ( 'NONE',  ( 5.006703865196457492, 9.063181286029688977, 0.000000000000000000 ) ) ;
#182827 = CARTESIAN_POINT ( 'NONE',  ( 5.224688093219824303, 7.188831756880171397, -1.599625672291283607 ) ) ;
#182828 = CARTESIAN_POINT ( 'NONE',  ( 0.000000000000000000, -3.784374999522044369, -3.793834371823813001 ) ) ;
#182829 = CARTESIAN_POINT ( 'NONE',  ( 1.270904146967307025, 2.996556430829583118, 0.7750000000000065725 ) ) ;
#182830 = CARTESIAN_POINT ( 'NONE',  ( 0.005962723626575306898, -0.8962717426808585186, -1.887145544106306083 ) ) ;
#182831 = CARTESIAN_POINT ( 'NONE',  ( 4.184220324914634581, 1.621181886760931778, 1.198861198883696799 ) ) ;
#182832 = CARTESIAN_POINT ( 'NONE',  ( 3.948646536499214932, -1.533023199436277961, -1.019512891124202403 ) ) ;
#182833 = CARTESIAN_POINT ( 'NONE',  ( 6.193377243344257543, 6.120028293523423812, -0.7998128361456281477 ) ) ;
#182834 = FILL_AREA_STYLE ('',( #103739 ) ) ;
#182835 = CARTESIAN_POINT ( 'NONE',  ( 1.975234724782324980, 1.651647476387863467, -0.4968862749653804589 ) ) ;
#182836 = CARTESIAN_POINT ( 'NONE',  ( -0.2058462039469660110, -0.8663896114125648751, -1.819200108291472606 ) ) ;
#182837 = CARTESIAN_POINT ( 'NONE',  ( 1.653414166010831243, 1.186659091926351106, 1.968620417403597944 ) ) ;
#182838 = CARTESIAN_POINT ( 'NONE',  ( -6.410307701162927252, 6.373113827645189744, -0.7998128361456291469 ) ) ;
#182839 = CARTESIAN_POINT ( 'NONE',  ( 0.9665587677401198397, 1.115807381107810192, 1.968008997871427468 ) ) ;
#182840 = CARTESIAN_POINT ( 'NONE',  ( 3.018300108557407935, -1.038308444602775271, -1.832253800920932596 ) ) ;
#182841 = CARTESIAN_POINT ( 'NONE',  ( -5.147255595043616516, 6.034161611419515125, 1.199719254218452935 ) ) ;
#182842 = CARTESIAN_POINT ( 'NONE',  ( 7.800018446563675489, 7.994443030612759848, -0.7998128361456281477 ) ) ;
#182843 = CARTESIAN_POINT ( 'NONE',  ( 5.031484404002878996, 7.923796667095108326, 1.082531754730548412 ) ) ;
#182844 = CARTESIAN_POINT ( 'NONE',  ( 6.437500000220395258, 1.451031294483499545, -1.451031289061371021 ) ) ;
#182845 = CARTESIAN_POINT ( 'NONE',  ( -4.089755892816631544, 7.923132308261379819, -0.7998128361456281477 ) ) ;
#182846 = CARTESIAN_POINT ( 'NONE',  ( 0.7499999999999885647, 2.566666666666689522, -1.299038105676658228 ) ) ;
#182847 = CARTESIAN_POINT ( 'NONE',  ( -2.598358995313378550, 6.183169261174235487, 0.7998128361456341429 ) ) ;
#182848 = CARTESIAN_POINT ( 'NONE',  ( 4.605860659110106781, 1.647066397540638993, 1.490795591097130002 ) ) ;
#182849 = CARTESIAN_POINT ( 'NONE',  ( 3.099763004921416876, -2.188912590334081809, 0.1079765428157742069 ) ) ;
#182850 = CARTESIAN_POINT ( 'NONE',  ( -6.437424008390261854, 6.404749519410410485, 0.7998128361456341429 ) ) ;
#182852 = TOROIDAL_SURFACE ( 'NONE', #89503, 12.17999951260719804, 0.5000000000000008882 ) ;
#182851 = CARTESIAN_POINT ( 'NONE',  ( -11.94105722165067363, 10.07417237917041497, 1.187919369849792295 ) ) ;
#182853 = CARTESIAN_POINT ( 'NONE',  ( -1.364683531250012516, 3.488541667008085767, -0.7879004041258300672 ) ) ;
#182854 = CARTESIAN_POINT ( 'NONE',  ( -2.277406616971334508, 5.600798786534425311, 1.040834085586084257E-14 ) ) ;
#182855 = CARTESIAN_POINT ( 'NONE',  ( -3.931501358282937009, 7.530575984731317618, 0.7216878364870317197 ) ) ;
#182856 = CARTESIAN_POINT ( 'NONE',  ( 5.344028447597857223, -1.346983732444573256, -1.637812552581649594 ) ) ;
#182857 = CARTESIAN_POINT ( 'NONE',  ( -5.641601317062233001, 9.595968946632336127, -0.7216878364870338292 ) ) ;
#182858 = ORIENTED_EDGE ( 'NONE', *, *, #82593, .T. ) ;
#182860 = DIRECTION ( 'NONE',  ( -5.551115123125765446E-17, 0.000000000000000000, 1.000000000000000000 ) ) ;
#182859 = CARTESIAN_POINT ( 'NONE',  ( -4.828112100242283766, 7.686528979374367410, -1.082531754730549967 ) ) ;
#182861 = CARTESIAN_POINT ( 'NONE',  ( 5.952193131599331721, 6.902979060742733708, 1.199719254218462483 ) ) ;
#182862 = CARTESIAN_POINT ( 'NONE',  ( -0.7499999999999972244, 3.108333333333358706, -1.299038105676652011 ) ) ;
#182863 = UNCERTAINTY_MEASURE_WITH_UNIT (LENGTH_MEASURE( 1.000000000000000082E-05 ), #183635, 'distance_accuracy_value', 'NONE');
#182864 =( NAMED_UNIT ( * ) SI_UNIT ( $, .STERADIAN. ) SOLID_ANGLE_UNIT ( ) );
#182865 = CARTESIAN_POINT ( 'NONE',  ( 0.6823417656249899377, 3.238541667008085323, -1.181850606188754593 ) ) ;
#182866 = CARTESIAN_POINT ( 'NONE',  ( 1.663200723894017852, 0.8946008992836312901, 1.492777717291964512 ) ) ;
#182867 = CARTESIAN_POINT ( 'NONE',  ( 3.602716132929354664, 5.226254793216122074, 1.599625672291267398 ) ) ;
#182868 = DIRECTION ( 'NONE',  ( 0.000000000000000000, 1.000000000000000000, -8.546850786086437571E-32 ) ) ;
#182869 = CARTESIAN_POINT ( 'NONE',  ( 0.6823417656249882723, 0.2385416670080825474, -1.181850606188749264 ) ) ;
#182870 = CARTESIAN_POINT ( 'NONE',  ( 8.776573235218638303, 13.27486625357122385, -8.183627694784497919 ) ) ;
#182871 = CARTESIAN_POINT ( 'NONE',  ( 5.454052192070485638, 2.159419290912270029, -0.1019294599445344784 ) ) ;
#182872 = CARTESIAN_POINT ( 'NONE',  ( -4.810445574750349174, 4.506608013497163334, 0.7998128361456341429 ) ) ;
#182873 = CARTESIAN_POINT ( 'NONE',  ( -7.985389288324703294, 9.379004260209384825, -1.082531754730543083 ) ) ;
#182874 = CARTESIAN_POINT ( 'NONE',  ( 4.698204674003193304, -2.161138953124014161, -0.05634304724232848394 ) ) ;
#182875 = ORIENTED_EDGE ( 'NONE', *, *, #178529, .F. ) ;
#182876 = CARTESIAN_POINT ( 'NONE',  ( -0.6823417656250212460, 2.551041667008084435, 1.181850606188767472 ) ) ;
#182877 = CARTESIAN_POINT ( 'NONE',  ( 6.186792457355818620, -0.2869052490914354991, -1.950236548312431317 ) ) ;
#182878 = CARTESIAN_POINT ( 'NONE',  ( 4.762897148713774342, -1.733524727309469382, -0.04171941676067019572 ) ) ;
#182880 = CARTESIAN_POINT ( 'NONE',  ( 1.804482060849887270, 1.621174160030929068, -1.474864209862189579 ) ) ;
#182879 = CARTESIAN_POINT ( 'NONE',  ( -5.508486862036250636E-15, -0.6718749996586012019, -1.570758158831788265 ) ) ;
#182881 = CARTESIAN_POINT ( 'NONE',  ( 2.063905019644726835, 0.3937302209732340685, -2.273608288252434662 ) ) ;
#182882 = CARTESIAN_POINT ( 'NONE',  ( 4.833308404897187494, -1.885807738700072678, 0.8313965460460555068 ) ) ;
#182883 = CARTESIAN_POINT ( 'NONE',  ( 0.4451279286748652808, 0.6098585162058448583, -1.843775557458992687 ) ) ;
#182884 = CARTESIAN_POINT ( 'NONE',  ( -6.195713011320790109, 9.211787032307496403, -1.082531754730537976 ) ) ;
#182885 = CARTESIAN_POINT ( 'NONE',  ( -3.142457743317409680, 6.888227477170756785, 0.7998128361456352531 ) ) ;
#182886 = DIRECTION ( 'NONE',  ( -0.000000000000000000, -1.000000000000000000, -0.000000000000000000 ) ) ;
#182887 = CARTESIAN_POINT ( 'NONE',  ( 3.375340920106313813, -1.871962376360849056, -0.9962781187466958066 ) ) ;
#182888 = DIRECTION ( 'NONE',  ( 0.000000000000000000, 0.000000000000000000, -1.000000000000000000 ) ) ;
#182889 = CARTESIAN_POINT ( 'NONE',  ( 1.195935645703485539, 1.779627574718087635, 0.9480385367472210500 ) ) ;
#182890 = CARTESIAN_POINT ( 'NONE',  ( -7.524412065460066579, 7.880828285899290186, 0.7216878364870317197 ) ) ;
#182891 = CARTESIAN_POINT ( 'NONE',  ( 4.331241739176756589, 0.1049304944579672605, 2.204394592675275710 ) ) ;
#182892 = CARTESIAN_POINT ( 'NONE',  ( -1.642778471874998480, -2.938541666188707602, 2.845375778867863303 ) ) ;
#182893 = CARTESIAN_POINT ( 'NONE',  ( 1.621681814730125515, 1.834508062647151272, -0.3115270159769789604 ) ) ;
#182894 =( BOUNDED_SURFACE ( )  B_SPLINE_SURFACE ( 1, 2, ( 
 ( #76824, #139734, #77897, #125669, #73635, #140812, #157039, #205758, #75772, #144018, #191631, #127820, #193775, #43295, #23807, #142944, #190571, #44352, #108343, #89912, #60580, #155964, #109415, #90977, #207889, #27004, #174363, #126738, #206824, #7550, #57388, #92049, #192698, #123552, #176474, #25942, #189516, #58458, #158106, #41162, #9695, #107271, #173291, #141880, #24873, #45421, #13944, #82155, #149301, #63779, #80027, #145078, #133088, #882, #12880, #181780, #47563, #198038, #146130, #111537, #177545, #213212, #78956, #33413, #32355, #31297, #212143, #99492, #165549, #29156, #196978, #147187, #95246, #211081, #17142, #83219, #128865, #164485, #161294, #62704, #66948, #49668, #194847, #15007, #48617, #114732, #46480, #112604, #132028, #178615, #30225, #129938, #81098, #96309, #162365, #180730, #179677, #130987, #97372, #163430, #64841, #195926, #115791, #113673, #98420, #16071, #148247, #214249, #65880, #52869, #182859, #87516, #70160, #34477, #202291, #199086, #100549, #116858, #84298, #3023, #53943, #103768, #18214, #36608, #37691, #169819, #69091, #19287, #21406, #4089, #166622, #150383, #151451, #1954, #120080, #50732, #117936, #134156, #101619, #20355, #71227, #68015, #167686, #186056, #200164, #51818, #153581, #152505, #183930, #35542, #135213, #201228, #5150, #119004, #86440, #184982, #137342, #85369, #102694, #168752, #136271, #131666, #1577, #82856, #196622, #116489, #48261, #100178, #16772, #166243, #49313, #163069, #65521, #197669, #114375, #115430, #64488, #13593, #211785, #164130, #181421, #29866, #34106, #180370, #66573, #80744, #31994, #95949, #212851, #198720, #79667, #98075, #133785, #178253, #146832, #505, #67638, #15714, #130630, #63423, #51438, #199793, #145782, #17833, #81799, #182478, #147882, #162004, #129575, #33051, #195562, #83916, #165178, #213898, #99129, #150007, #47198, #113313, #148932, #132715, #179319, #30940, #97015, #14650, #50366, #22087, #183552, #151080, #139096, #55690, #205123, #87125, #54627, #186754, #84989, #18905, #204041, #200842, #167318, #86060, #153195 ),
 ( #117558, #185678, #37307, #201908, #121846, #35159, #103381, #53560, #118623, #52493, #187817, #155332, #69781, #19976, #3705, #2644, #68718, #169443, #4767, #101236, #39443, #119693, #5846, #152137, #21028, #134839, #135890, #138026, #184610, #70844, #72993, #36227, #136960, #154272, #6916, #202987, #120774, #102306, #168379, #38376, #104457, #105537, #170504, #171571, #88198, #71917, #23168, #89284, #160671, #159600, #44811, #25323, #207272, #75154, #92500, #93556, #10136, #57829, #188889, #156409, #122932, #90340, #157485, #41608, #9080, #173746, #172663, #123991, #58903, #144466, #107719, #125056, #76211, #191011, #42679, #143391, #110915, #40530, #158539, #126117, #106634, #108786, #175870, #192077, #61033, #142321, #56766, #174812, #26388, #141264, #209389, #24238, #208331, #59962, #189958, #140179, #127194, #94628, #43743, #91424, #109856, #77279, #11198, #27458, #176921, #193161, #206201, #28536, #7996, #12266, #78343, #74088, #173500, #75972, #90104, #5594, #170260, #40280, #71674, #89039, #137787, #7750, #174568, #57593, #26144, #208089, #205960, #142075, #157237, #56526, #190770, #122686, #92258, #91178, #158304, #123750, #22924, #139933, #189711, #188649, #41364, #9895, #106390, #42432, #8832, #107475, #24002, #59717, #203807, #125876, #25075, #156169, #6680, #38141, #104213, #21845, #74909, #141017, #87953, #55452, #154027, #121604, #187576, #207025, #39201, #105293, #171329, #108538, #155095, #73837, #58656, #124809, #72757, #138854, #204871, #172413, #27210, #160421, #161506, #159352, #147383, #129081, #111741, #62912, #177747, #95457, #13086, #28286, #47769, #12027, #78098, #178822, #65031, #93316, #193976, #79166, #10949, #163633, #14141, #175623, #146333, #43498, #77023, #109618, #143153, #29362, #212347, #113882, #209147, #211288, #196129, #179877, #145282, #112809, #15216, #195052, #60786, #126945, #45624, #192902, #94381, #44558, #46691, #31502, #30434, #97576, #213409, #96520, #81306, #162568, #210219, #130140, #61855, #191835, #80234, #110674, #63988, #176674, #144225, #128022, #149500 ) ),
 .UNSPECIFIED., .F., .F., .T. ) 
 B_SPLINE_SURFACE_WITH_KNOTS ( ( 2, 2 ),
 ( 3, 2, 2, 2, 2, 2, 2, 2, 2, 2, 2, 2, 2, 2, 2, 2, 2, 2, 2, 2, 2, 2, 2, 2, 2, 2, 2, 2, 2, 2, 2, 2, 2, 2, 2, 2, 2, 2, 2, 2, 2, 2, 2, 2, 2, 2, 2, 2, 2, 2, 2, 2, 2, 2, 2, 2, 2, 2, 2, 2, 2, 2, 2, 2, 2, 2, 2, 2, 2, 2, 2, 2, 2, 2, 2, 2, 2, 2, 2, 2, 2, 2, 2, 2, 2, 2, 2, 2, 2, 2, 2, 2, 2, 2, 2, 2, 2, 2, 2, 2, 2, 2, 2, 2, 2, 2, 2, 2, 2, 2, 2, 2, 2, 2, 2, 2, 2, 2, 2, 2, 3 ),
 ( 0.000000000000000000, 1.000000000000000000 ),
 ( 0.000000000000000000, 0.008333333333333333218, 0.01666666666666666644, 0.02500000000000000139, 0.03333333333333333287, 0.04166666666666666435, 0.05000000000000000278, 0.05833333333333333426, 0.06666666666666666574, 0.07499999999999999722, 0.08333333333333332871, 0.09166666666666666019, 0.1000000000000000056, 0.1083333333333333370, 0.1166666666666666685, 0.1250000000000000000, 0.1333333333333333315, 0.1416666666666666630, 0.1499999999999999944, 0.1583333333333333259, 0.1666666666666666574, 0.1749999999999999889, 0.1833333333333333204, 0.1916666666666666796, 0.2000000000000000111, 0.2083333333333333426, 0.2166666666666666741, 0.2250000000000000056, 0.2333333333333333370, 0.2416666666666666685, 0.2500000000000000000, 0.2583333333333333592, 0.2666666666666666630, 0.2750000000000000222, 0.2833333333333333259, 0.2916666666666666852, 0.2999999999999999889, 0.3083333333333333481, 0.3166666666666666519, 0.3250000000000000111, 0.3333333333333333148, 0.3416666666666666741, 0.3499999999999999778, 0.3583333333333333370, 0.3666666666666666408, 0.3750000000000000000, 0.3833333333333333592, 0.3916666666666666630, 0.4000000000000000222, 0.4083333333333333259, 0.4166666666666666852, 0.4249999999999999889, 0.4333333333333333481, 0.4416666666666666519, 0.4500000000000000111, 0.4583333333333333148, 0.4666666666666666741, 0.4749999999999999778, 0.4833333333333333370, 0.4916666666666666408, 0.5000000000000000000, 0.5083333333333333037, 0.5166666666666667185, 0.5250000000000000222, 0.5333333333333333259, 0.5416666666666666297, 0.5500000000000000444, 0.5583333333333333481, 0.5666666666666666519, 0.5749999999999999556, 0.5833333333333333703, 0.5916666666666666741, 0.5999999999999999778, 0.6083333333333332815, 0.6166666666666666963, 0.6250000000000000000, 0.6333333333333333037, 0.6416666666666667185, 0.6500000000000000222, 0.6583333333333333259, 0.6666666666666666297, 0.6750000000000000444, 0.6833333333333333481, 0.6916666666666666519, 0.6999999999999999556, 0.7083333333333333703, 0.7166666666666666741, 0.7249999999999999778, 0.7333333333333332815, 0.7416666666666666963, 0.7500000000000000000, 0.7583333333333333037, 0.7666666666666667185, 0.7750000000000000222, 0.7833333333333333259, 0.7916666666666666297, 0.8000000000000000444, 0.8083333333333333481, 0.8166666666666666519, 0.8249999999999999556, 0.8333333333333333703, 0.8416666666666666741, 0.8499999999999999778, 0.8583333333333332815, 0.8666666666666666963, 0.8750000000000000000, 0.8833333333333333037, 0.8916666666666667185, 0.9000000000000000222, 0.9083333333333333259, 0.9166666666666666297, 0.9250000000000000444, 0.9333333333333333481, 0.9416666666666666519, 0.9499999999999999556, 0.9583333333333333703, 0.9666666666666666741, 0.9749999999999999778, 0.9833333333333332815, 0.9916666666666666963, 1.000000000000000000 ),
 .UNSPECIFIED. ) 
 GEOMETRIC_REPRESENTATION_ITEM ( )  RATIONAL_B_SPLINE_SURFACE ( (
 ( 1.000000000000000000, 0.8660254037844387076, 1.000000000000000000, 0.8660254037844387076, 1.000000000000000000, 0.8660254037844387076, 1.000000000000000000, 0.8660254037844387076, 1.000000000000000000, 0.8660254037844387076, 1.000000000000000000, 0.8660254037844387076, 1.000000000000000000, 0.8660254037844387076, 1.000000000000000000, 0.8660254037844387076, 1.000000000000000000, 0.8660254037844387076, 1.000000000000000000, 0.8660254037844387076, 1.000000000000000000, 0.8660254037844387076, 1.000000000000000000, 0.8660254037844387076, 1.000000000000000000, 0.8660254037844387076, 1.000000000000000000, 0.8660254037844387076, 1.000000000000000000, 0.8660254037844387076, 1.000000000000000000, 0.8660254037844387076, 1.000000000000000000, 0.8660254037844387076, 1.000000000000000000, 0.8660254037844387076, 1.000000000000000000, 0.8660254037844387076, 1.000000000000000000, 0.8660254037844387076, 1.000000000000000000, 0.8660254037844387076, 1.000000000000000000, 0.8660254037844387076, 1.000000000000000000, 0.8660254037844387076, 1.000000000000000000, 0.8660254037844387076, 1.000000000000000000, 0.8660254037844387076, 1.000000000000000000, 0.8660254037844387076, 1.000000000000000000, 0.8660254037844387076, 1.000000000000000000, 0.8660254037844387076, 1.000000000000000000, 0.8660254037844387076, 1.000000000000000000, 0.8660254037844387076, 1.000000000000000000, 0.8660254037844387076, 1.000000000000000000, 0.8660254037844387076, 1.000000000000000000, 0.8660254037844387076, 1.000000000000000000, 0.8660254037844387076, 1.000000000000000000, 0.8660254037844387076, 1.000000000000000000, 0.8660254037844387076, 1.000000000000000000, 0.8660254037844387076, 1.000000000000000000, 0.8660254037844387076, 1.000000000000000000, 0.8660254037844387076, 1.000000000000000000, 0.8660254037844387076, 1.000000000000000000, 0.8660254037844387076, 1.000000000000000000, 0.8660254037844387076, 1.000000000000000000, 0.8660254037844387076, 1.000000000000000000, 0.8660254037844387076, 1.000000000000000000, 0.8660254037844387076, 1.000000000000000000, 0.8660254037844387076, 1.000000000000000000, 0.8660254037844387076, 1.000000000000000000, 0.8660254037844387076, 1.000000000000000000, 0.8660254037844387076, 1.000000000000000000, 0.8660254037844387076, 1.000000000000000000, 0.8660254037844387076, 1.000000000000000000, 0.8660254037844387076, 1.000000000000000000, 0.8660254037844387076, 1.000000000000000000, 0.8660254037844387076, 1.000000000000000000, 0.8660254037844387076, 1.000000000000000000, 0.8660254037844387076, 1.000000000000000000, 0.8660254037844387076, 1.000000000000000000, 0.8660254037844387076, 1.000000000000000000, 0.8660254037844387076, 1.000000000000000000, 0.8660254037844387076, 1.000000000000000000, 0.8660254037844387076, 1.000000000000000000, 0.8660254037844387076, 1.000000000000000000, 0.8660254037844387076, 1.000000000000000000, 0.8660254037844387076, 1.000000000000000000, 0.8660254037844387076, 1.000000000000000000, 0.8660254037844387076, 1.000000000000000000, 0.8660254037844387076, 1.000000000000000000, 0.8660254037844387076, 1.000000000000000000, 0.8660254037844387076, 1.000000000000000000, 0.8660254037844387076, 1.000000000000000000, 0.8660254037844387076, 1.000000000000000000, 0.8660254037844387076, 1.000000000000000000, 0.8660254037844387076, 1.000000000000000000, 0.8660254037844387076, 1.000000000000000000, 0.8660254037844387076, 1.000000000000000000, 0.8660254037844387076, 1.000000000000000000, 0.8660254037844387076, 1.000000000000000000, 0.8660254037844387076, 1.000000000000000000, 0.8660254037844387076, 1.000000000000000000, 0.8660254037844387076, 1.000000000000000000, 0.8660254037844387076, 1.000000000000000000, 0.8660254037844387076, 1.000000000000000000, 0.8660254037844387076, 1.000000000000000000, 0.8660254037844387076, 1.000000000000000000, 0.8660254037844387076, 1.000000000000000000, 0.8660254037844387076, 1.000000000000000000, 0.8660254037844387076, 1.000000000000000000, 0.8660254037844387076, 1.000000000000000000, 0.8660254037844387076, 1.000000000000000000, 0.8660254037844387076, 1.000000000000000000, 0.8660254037844387076, 1.000000000000000000, 0.8660254037844387076, 1.000000000000000000, 0.8660254037844387076, 1.000000000000000000, 0.8660254037844387076, 1.000000000000000000, 0.8660254037844387076, 1.000000000000000000, 0.8660254037844387076, 1.000000000000000000, 0.8660254037844387076, 1.000000000000000000, 0.8660254037844387076, 1.000000000000000000, 0.8660254037844387076, 1.000000000000000000, 0.8660254037844387076, 1.000000000000000000, 0.8660254037844387076, 1.000000000000000000, 0.8660254037844387076, 1.000000000000000000, 0.8660254037844387076, 1.000000000000000000, 0.8660254037844387076, 1.000000000000000000, 0.8660254037844387076, 1.000000000000000000, 0.8660254037844387076, 1.000000000000000000, 0.8660254037844387076, 1.000000000000000000, 0.8660254037844387076, 1.000000000000000000, 0.8660254037844387076, 1.000000000000000000, 0.8660254037844387076, 1.000000000000000000, 0.8660254037844387076, 1.000000000000000000, 0.8660254037844387076, 1.000000000000000000, 0.8660254037844387076, 1.000000000000000000, 0.8660254037844387076, 1.000000000000000000, 0.8660254037844387076, 1.000000000000000000, 0.8660254037844387076, 1.000000000000000000, 0.8660254037844387076, 1.000000000000000000, 0.8660254037844387076, 1.000000000000000000, 0.8660254037844387076, 1.000000000000000000, 0.8660254037844387076, 1.000000000000000000),
 ( 1.000000000000000000, 0.8660254037844387076, 1.000000000000000000, 0.8660254037844387076, 1.000000000000000000, 0.8660254037844387076, 1.000000000000000000, 0.8660254037844387076, 1.000000000000000000, 0.8660254037844387076, 1.000000000000000000, 0.8660254037844387076, 1.000000000000000000, 0.8660254037844387076, 1.000000000000000000, 0.8660254037844387076, 1.000000000000000000, 0.8660254037844387076, 1.000000000000000000, 0.8660254037844387076, 1.000000000000000000, 0.8660254037844387076, 1.000000000000000000, 0.8660254037844387076, 1.000000000000000000, 0.8660254037844387076, 1.000000000000000000, 0.8660254037844387076, 1.000000000000000000, 0.8660254037844387076, 1.000000000000000000, 0.8660254037844387076, 1.000000000000000000, 0.8660254037844387076, 1.000000000000000000, 0.8660254037844387076, 1.000000000000000000, 0.8660254037844387076, 1.000000000000000000, 0.8660254037844387076, 1.000000000000000000, 0.8660254037844387076, 1.000000000000000000, 0.8660254037844387076, 1.000000000000000000, 0.8660254037844387076, 1.000000000000000000, 0.8660254037844387076, 1.000000000000000000, 0.8660254037844387076, 1.000000000000000000, 0.8660254037844387076, 1.000000000000000000, 0.8660254037844387076, 1.000000000000000000, 0.8660254037844387076, 1.000000000000000000, 0.8660254037844387076, 1.000000000000000000, 0.8660254037844387076, 1.000000000000000000, 0.8660254037844387076, 1.000000000000000000, 0.8660254037844387076, 1.000000000000000000, 0.8660254037844387076, 1.000000000000000000, 0.8660254037844387076, 1.000000000000000000, 0.8660254037844387076, 1.000000000000000000, 0.8660254037844387076, 1.000000000000000000, 0.8660254037844387076, 1.000000000000000000, 0.8660254037844387076, 1.000000000000000000, 0.8660254037844387076, 1.000000000000000000, 0.8660254037844387076, 1.000000000000000000, 0.8660254037844387076, 1.000000000000000000, 0.8660254037844387076, 1.000000000000000000, 0.8660254037844387076, 1.000000000000000000, 0.8660254037844387076, 1.000000000000000000, 0.8660254037844387076, 1.000000000000000000, 0.8660254037844387076, 1.000000000000000000, 0.8660254037844387076, 1.000000000000000000, 0.8660254037844387076, 1.000000000000000000, 0.8660254037844387076, 1.000000000000000000, 0.8660254037844387076, 1.000000000000000000, 0.8660254037844387076, 1.000000000000000000, 0.8660254037844387076, 1.000000000000000000, 0.8660254037844387076, 1.000000000000000000, 0.8660254037844387076, 1.000000000000000000, 0.8660254037844387076, 1.000000000000000000, 0.8660254037844387076, 1.000000000000000000, 0.8660254037844387076, 1.000000000000000000, 0.8660254037844387076, 1.000000000000000000, 0.8660254037844387076, 1.000000000000000000, 0.8660254037844387076, 1.000000000000000000, 0.8660254037844387076, 1.000000000000000000, 0.8660254037844387076, 1.000000000000000000, 0.8660254037844387076, 1.000000000000000000, 0.8660254037844387076, 1.000000000000000000, 0.8660254037844387076, 1.000000000000000000, 0.8660254037844387076, 1.000000000000000000, 0.8660254037844387076, 1.000000000000000000, 0.8660254037844387076, 1.000000000000000000, 0.8660254037844387076, 1.000000000000000000, 0.8660254037844387076, 1.000000000000000000, 0.8660254037844387076, 1.000000000000000000, 0.8660254037844387076, 1.000000000000000000, 0.8660254037844387076, 1.000000000000000000, 0.8660254037844387076, 1.000000000000000000, 0.8660254037844387076, 1.000000000000000000, 0.8660254037844387076, 1.000000000000000000, 0.8660254037844387076, 1.000000000000000000, 0.8660254037844387076, 1.000000000000000000, 0.8660254037844387076, 1.000000000000000000, 0.8660254037844387076, 1.000000000000000000, 0.8660254037844387076, 1.000000000000000000, 0.8660254037844387076, 1.000000000000000000, 0.8660254037844387076, 1.000000000000000000, 0.8660254037844387076, 1.000000000000000000, 0.8660254037844387076, 1.000000000000000000, 0.8660254037844387076, 1.000000000000000000, 0.8660254037844387076, 1.000000000000000000, 0.8660254037844387076, 1.000000000000000000, 0.8660254037844387076, 1.000000000000000000, 0.8660254037844387076, 1.000000000000000000, 0.8660254037844387076, 1.000000000000000000, 0.8660254037844387076, 1.000000000000000000, 0.8660254037844387076, 1.000000000000000000, 0.8660254037844387076, 1.000000000000000000, 0.8660254037844387076, 1.000000000000000000, 0.8660254037844387076, 1.000000000000000000, 0.8660254037844387076, 1.000000000000000000, 0.8660254037844387076, 1.000000000000000000, 0.8660254037844387076, 1.000000000000000000, 0.8660254037844387076, 1.000000000000000000, 0.8660254037844387076, 1.000000000000000000, 0.8660254037844387076, 1.000000000000000000, 0.8660254037844387076, 1.000000000000000000, 0.8660254037844387076, 1.000000000000000000, 0.8660254037844387076, 1.000000000000000000, 0.8660254037844387076, 1.000000000000000000, 0.8660254037844387076, 1.000000000000000000, 0.8660254037844387076, 1.000000000000000000, 0.8660254037844387076, 1.000000000000000000, 0.8660254037844387076, 1.000000000000000000, 0.8660254037844387076, 1.000000000000000000, 0.8660254037844387076, 1.000000000000000000, 0.8660254037844387076, 1.000000000000000000, 0.8660254037844387076, 1.000000000000000000, 0.8660254037844387076, 1.000000000000000000, 0.8660254037844387076, 1.000000000000000000, 0.8660254037844387076, 1.000000000000000000, 0.8660254037844387076, 1.000000000000000000, 0.8660254037844387076, 1.000000000000000000, 0.8660254037844387076, 1.000000000000000000) ) ) 
 REPRESENTATION_ITEM ( '' )  SURFACE ( )  );
#182895 = CARTESIAN_POINT ( 'NONE',  ( -0.1288028175206907822, 6.946859453142047336, -2.869069570226709498 ) ) ;
#182896 = CARTESIAN_POINT ( 'NONE',  ( -11.84668730067608244, 12.59363775091779125, 1.399999999999998357 ) ) ;
#182897 = CARTESIAN_POINT ( 'NONE',  ( 6.135296122173847344, 5.374195598252329731, -2.500000000000000444 ) ) ;
#182899 = CARTESIAN_POINT ( 'NONE',  ( 6.925078400183545035, 2.404074903924419804, 2.624186486869657831 ) ) ;
#182898 = CARTESIAN_POINT ( 'NONE',  ( -5.797436685056675643, 7.335035436452395530, -1.304849551618554981 ) ) ;
#182900 = ORIENTED_EDGE ( 'NONE', *, *, #37073, .T. ) ;
#182901 = CARTESIAN_POINT ( 'NONE',  ( 3.766525121192493941, -1.385455288492474235, 1.525868174829993373 ) ) ;
#182902 = CARTESIAN_POINT ( 'NONE',  ( -2.353626204688216217E-14, 2.453125000341405570, 1.570758158831792262 ) ) ;
#182903 = CARTESIAN_POINT ( 'NONE',  ( -5.473741331615264549, 7.409117525016355010, -1.599625672291256295 ) ) ;
#182904 = CARTESIAN_POINT ( 'NONE',  ( 2.438154291397228501, -1.164718066671111885, -1.649793688766809430 ) ) ;
#182905 = CARTESIAN_POINT ( 'NONE',  ( 1.499999999999987121, -0.4958333333333110882, 0.8660254037844524744 ) ) ;
#182906 = CIRCLE ( 'NONE', #44561, 0.4000000000000001332 ) ;
#182907 = CARTESIAN_POINT ( 'NONE',  ( 4.532503425670185493, 4.182342172903648070, 1.214306433183764966E-14 ) ) ;
#182908 = CARTESIAN_POINT ( 'NONE',  ( 1.709912189389639403, -2.045452440186873666, 0.2511061956092154324 ) ) ;
#182910 = CARTESIAN_POINT ( 'NONE',  ( 0.6823417656249934904, 12.94270833367473017, 1.181850606188764807 ) ) ;
#182909 = CARTESIAN_POINT ( 'NONE',  ( -9.445420027513423022, 15.31879668566292985, -7.300025634049747580 ) ) ;
#182911 = CARTESIAN_POINT ( 'NONE',  ( 5.035963992472171746, 7.962709526937818083, 1.199719254218462483 ) ) ;
#182913 = VERTEX_POINT ( 'NONE', #135549 ) ;
#182912 = CARTESIAN_POINT ( 'NONE',  ( -0.1409997244346088141, 4.088373444016307978, -2.555100908668860082 ) ) ;
#182914 = CARTESIAN_POINT ( 'NONE',  ( 1.060217833243476182, -1.663605802054025418, -0.7890760572396152694 ) ) ;
#182915 = CARTESIAN_POINT ( 'NONE',  ( 5.285833163787800437, 1.479997892162682849, 1.637210856327932618 ) ) ;
#182916 = CARTESIAN_POINT ( 'NONE',  ( 5.468734858265785093, 7.473552982767158070, 1.599625672291269396 ) ) ;
#182917 = CARTESIAN_POINT ( 'NONE',  ( 1.388190569347878212, -0.9732202972718406730, 1.930209198840258100 ) ) ;
#182918 = AXIS2_PLACEMENT_3D ( 'NONE', #90093, #106379, #123739 ) ;
#182919 = CARTESIAN_POINT ( 'NONE',  ( -4.934804725694236893, 4.859619722839116918, -0.7216878364870207285 ) ) ;
#182920 = CARTESIAN_POINT ( 'NONE',  ( 2.132046339962359038, 2.016188815772378629, 0.04465230659478347519 ) ) ;
#182921 = CARTESIAN_POINT ( 'NONE',  ( -4.290995968093258561, 3.987448345753906498, 0.1285802912755794336 ) ) ;
#182922 = CARTESIAN_POINT ( 'NONE',  ( -0.4746061814645892718, 6.848527939983842572, 3.764703919983649616 ) ) ;
#182923 = CARTESIAN_POINT ( 'NONE',  ( 3.145207314826885092, 6.442628614629879458, -0.6582494395028383183 ) ) ;
#182924 = CARTESIAN_POINT ( 'NONE',  ( 4.452002833372045387, 1.971050344634683427, -0.04741254548742446229 ) ) ;
#182925 = CARTESIAN_POINT ( 'NONE',  ( 3.872279980006509970, -1.995268062538615883, -0.2910826752766728642 ) ) ;
#182927 = CARTESIAN_POINT ( 'NONE',  ( 8.554831740098642001, 12.92446143018304916, 0.7216878364870438212 ) ) ;
#182926 = CARTESIAN_POINT ( 'NONE',  ( -1.364683531250012516, 1.780208333674757615, 0.7879004041258379498 ) ) ;
#182929 = CARTESIAN_POINT ( 'NONE',  ( 5.777981411418616098, 1.253425007971820326, 1.692306578934036798 ) ) ;
#182928 = CARTESIAN_POINT ( 'NONE',  ( -8.538937818508475885, 8.856515631215026829, 1.040834085586084257E-14 ) ) ;
#182930 = CARTESIAN_POINT ( 'NONE',  ( 5.881320641815353412, -0.05461762546566179682, 2.069818975884097689 ) ) ;
#182931 = CARTESIAN_POINT ( 'NONE',  ( 7.467843683028853263, 7.606905806488803101, 0.7998128361456341429 ) ) ;
#182932 = CARTESIAN_POINT ( 'NONE',  ( -6.204827856548512877, 10.39071626594860476, -0.7998128361456291469 ) ) ;
#182933 = CARTESIAN_POINT ( 'NONE',  ( 6.539320575229278454, 2.035006821797652687, 2.408631514295301645 ) ) ;
#182934 = CARTESIAN_POINT ( 'NONE',  ( 5.062762828692743966, 0.5904309321736100902, 1.931528952932992427 ) ) ;
#182935 = CARTESIAN_POINT ( 'NONE',  ( -1.500000000000015099, -0.7979166659838445863, 0.8660254037844403729 ) ) ;
#182936 = CARTESIAN_POINT ( 'NONE',  ( 1.340767248851399307, -2.011434839998844204, -0.4557168523060088905 ) ) ;
#182937 = CARTESIAN_POINT ( 'NONE',  ( 9.083599731475992201, 9.699880562917908122, 0.7216878364870438212 ) ) ;
#182938 = CARTESIAN_POINT ( 'NONE',  ( 5.830888582329017744, 8.960397891762626799, -1.199719254218452047 ) ) ;
#182939 = CARTESIAN_POINT ( 'NONE',  ( 4.766573523656222555, 7.718696989977711809, 1.199719254218452047 ) ) ;
#182940 = CARTESIAN_POINT ( 'NONE',  ( -1.364683531250000748, 1.071875000341421247, 0.000000000000000000 ) ) ;
#182942 = CARTESIAN_POINT ( 'NONE',  ( 3.418706159394787836, 6.339871777953998588, 1.082712511304601000 ) ) ;
#182941 = CARTESIAN_POINT ( 'NONE',  ( 3.542423274920540432, 7.354853930707762721, -1.734723475976807094E-15 ) ) ;
#182943 = CARTESIAN_POINT ( 'NONE',  ( 6.602457619730767391, 7.765583980183128787, 1.082531754730558626 ) ) ;
#182945 = PRESENTATION_STYLE_ASSIGNMENT (( #119084 ) ) ;
#182944 = CARTESIAN_POINT ( 'NONE',  ( 2.858077868800662724, -0.6831540018236246237, 2.060947818793914532 ) ) ;
#182947 = CARTESIAN_POINT ( 'NONE',  ( 3.052128622409277181, -1.392423357299840792, 1.204796875372941667 ) ) ;
#182946 = CARTESIAN_POINT ( 'NONE',  ( -4.229780737783618072, 6.918199379847403740, 1.082531754730560403 ) ) ;
#182948 = EDGE_CURVE ( 'NONE', #40760, #43199, #136177, .T. ) ;
#182949 = CARTESIAN_POINT ( 'NONE',  ( 1.364683531249990311, 5.113541667008084879, 0.7879004041258500513 ) ) ;
#182950 = CARTESIAN_POINT ( 'NONE',  ( 4.282901435897610298, 1.957309562236182021, -0.9860176978964061423 ) ) ;
#182951 = CARTESIAN_POINT ( 'NONE',  ( 8.766148990750032510, 13.42095518280116906, 8.127564194100379780 ) ) ;
#182952 = CARTESIAN_POINT ( 'NONE',  ( 4.381858629716777642, 1.474804143916402355, 1.715883708886431158 ) ) ;
#182953 = CARTESIAN_POINT ( 'NONE',  ( -4.381256195510448315, 8.263215994737505454, 1.040834085586084257E-14 ) ) ;
#182954 = CARTESIAN_POINT ( 'NONE',  ( -5.642163961945882988, 6.318168449258962482, -1.169820551124676422 ) ) ;
#182955 = CARTESIAN_POINT ( 'NONE',  ( 4.708029738644283313, 8.352945002179891887, -0.6661931671527853149 ) ) ;
#182956 = CARTESIAN_POINT ( 'NONE',  ( -4.434925645001610128, 8.188180662561590495, 0.7216878364870338292 ) ) ;
#182957 = CARTESIAN_POINT ( 'NONE',  ( 3.919715808126649659, 7.587102519540811940, 0.000000000000000000 ) ) ;
#182958 = CARTESIAN_POINT ( 'NONE',  ( 0.2152203129428611750, -1.737008003653650157, 0.3383841826808623443 ) ) ;
#182959 = CARTESIAN_POINT ( 'NONE',  ( 3.985024600404694972, -1.879186454625543901, -0.7224040237710227519 ) ) ;
#182960 = CARTESIAN_POINT ( 'NONE',  ( 8.294891053462476904, 8.571794405328034827, 1.040834085586084257E-14 ) ) ;
#182961 = CARTESIAN_POINT ( 'NONE',  ( 3.241344266390119078, -1.858123463236575290, 0.9911517508872002002 ) ) ;
#182962 = CARTESIAN_POINT ( 'NONE',  ( 0.9486861286592045417, -1.732399544687371229, -0.8177760133930843667 ) ) ;
#182964 = CARTESIAN_POINT ( 'NONE',  ( -1.500000000000013101, 2.379166666666686414, -0.8660254037844313801 ) ) ;
#182963 = CARTESIAN_POINT ( 'NONE',  ( 1.364683531249997417, 11.48437500034139802, 2.602085213965210642E-15 ) ) ;
#182965 = CARTESIAN_POINT ( 'NONE',  ( 1.890998328602263800, 0.1897877418215961898, 1.960365536012158127 ) ) ;
#182966 = CARTESIAN_POINT ( 'NONE',  ( 0.8131078318618142342, -0.2785150557334699073, 1.849687307983488571 ) ) ;
#182967 = CARTESIAN_POINT ( 'NONE',  ( 0.5023040531197673353, 1.956348610274569744, 0.1481081594910879096 ) ) ;
#182969 = ORIENTED_EDGE ( 'NONE', *, *, #177848, .T. ) ;
#182968 = CARTESIAN_POINT ( 'NONE',  ( 6.533470331352867255, -0.1283082721124771952, 1.781802213622991404 ) ) ;
#182970 = CARTESIAN_POINT ( 'NONE',  ( 5.016153647376201619, 7.835634441038803466, 1.082531754730558626 ) ) ;
#182971 = CARTESIAN_POINT ( 'NONE',  ( -1.364683531250000748, 0.5718750003414208027, 0.000000000000000000 ) ) ;
#182972 = CARTESIAN_POINT ( 'NONE',  ( 6.139502064137229986, -1.356240498024411600, -1.288626068300227523 ) ) ;
#182973 = CARTESIAN_POINT ( 'NONE',  ( 2.205172540517054802, 5.724451730578533848, 1.040834085586084257E-14 ) ) ;
#182974 = DIRECTION ( 'NONE',  ( 0.6483454320283799088, 0.000000000000000000, -0.7613463080411786432 ) ) ;
#182975 = CARTESIAN_POINT ( 'NONE',  ( 6.807487347360918761, -1.659057770219806160, -1.238116672595261480 ) ) ;
#182976 = VECTOR ( 'NONE', #107777, 1000.000000000000000 ) ;
#182977 = CARTESIAN_POINT ( 'NONE',  ( -1.250000000000021982, 10.00000000000000178, 4.154462424328226433 ) ) ;
#182978 = EDGE_CURVE ( 'NONE', #168570, #179011, #146567, .T. ) ;
#182979 = CARTESIAN_POINT ( 'NONE',  ( 3.179715765502636682, 5.975770656120749535, 2.419999999999999485 ) ) ;
#182980 = CARTESIAN_POINT ( 'NONE',  ( -1.500000000000001332, 1.150000000000019007, 0.000000000000000000 ) ) ;
#182981 = CARTESIAN_POINT ( 'NONE',  ( 5.452350330990040739, 9.512825819463730070, 0.7998128361456462443 ) ) ;
#182982 = CARTESIAN_POINT ( 'NONE',  ( -7.153898609505128015, 11.49796547773133604, 0.7998128361456481317 ) ) ;
#182983 = CARTESIAN_POINT ( 'NONE',  ( 7.028976294042106332, 7.165170195996068969, 0.000000000000000000 ) ) ;
#182984 = CARTESIAN_POINT ( 'NONE',  ( 0.6823417656249899377, 0.8427083336747520637, 1.181850606188755259 ) ) ;
#182985 = CARTESIAN_POINT ( 'NONE',  ( -0.7500000000000006661, 2.608333333333358262, -1.299038105676652011 ) ) ;
#182987 = CARTESIAN_POINT ( 'NONE',  ( 3.147464216666835402, 6.823792019419957278, -0.7998128361456291469 ) ) ;
#182986 = CARTESIAN_POINT ( 'NONE',  ( 5.723093114104088386, -1.772945450647535948, -0.8403097561825512152 ) ) ;
#182988 = CARTESIAN_POINT ( 'NONE',  ( 3.005232341680406094, 2.000550758621592706, 0.2495690156183311137 ) ) ;
#182989 = CARTESIAN_POINT ( 'NONE',  ( 3.889770295363860431, -1.910208526776317806, 0.1464741861031873538 ) ) ;
#182990 = CARTESIAN_POINT ( 'NONE',  ( 11.91292854676703961, 9.985184703269753825, -1.446370920797349635 ) ) ;
#182991 = CARTESIAN_POINT ( 'NONE',  ( 1.013517375116283592, -2.137022957946862700, 0.4851717564131745597 ) ) ;
#182992 = CARTESIAN_POINT ( 'NONE',  ( 0.1331715793776574175, 0.2412765091673596263, -1.987739918565622821 ) ) ;
#182993 = CARTESIAN_POINT ( 'NONE',  ( 2.829206387438303327, -1.746784236434804072, 0.6695917499066756928 ) ) ;
#182994 = CARTESIAN_POINT ( 'NONE',  ( -1.500000000000015099, -0.8395833326505166561, -0.8660254037844383745 ) ) ;
#182995 = CARTESIAN_POINT ( 'NONE',  ( -6.170932472514347289, 10.35117165124207972, 0.000000000000000000 ) ) ;
#182997 = CARTESIAN_POINT ( 'NONE',  ( 5.027025340701954725, -1.815278874653761809, 1.089499710131608401 ) ) ;
#182996 = CARTESIAN_POINT ( 'NONE',  ( -4.961921032921567054, 4.891255414604337659, 0.7216878364870317197 ) ) ;
#182998 = CYLINDRICAL_SURFACE ( 'NONE', #132176, 0.2500000000000002220 ) ;
#182999 = CARTESIAN_POINT ( 'NONE',  ( 5.705552448923417508, -1.629793913574303588, -1.276656259598766940 ) ) ;
#183001 = DIRECTION ( 'NONE',  ( 0.000000000000000000, 0.000000000000000000, -1.000000000000000000 ) ) ;
#183000 = CARTESIAN_POINT ( 'NONE',  ( 2.542619699696859303, -1.736688010486141520, 1.163783427146478200 ) ) ;
#183003 = VERTEX_POINT ( 'NONE', #36961 ) ;
#183002 = CARTESIAN_POINT ( 'NONE',  ( 1.236830563851202491, -1.561790747969876714, 0.7321873917187391445 ) ) ;
#183004 = CARTESIAN_POINT ( 'NONE',  ( 5.774883364416965037, 8.824782127540085952, -1.199719254218440723 ) ) ;
#183005 = CARTESIAN_POINT ( 'NONE',  ( 8.030844283385320637, 15.33938070391476671, 8.918166425210744208 ) ) ;
#183006 = CARTESIAN_POINT ( 'NONE',  ( -8.064677165291197269, -5.223431457505076203, 7.446209719563364082 ) ) ;
#183007 = AXIS2_PLACEMENT_3D ( 'NONE', #36393, #102471, #136051 ) ;
#183008 = CARTESIAN_POINT ( 'NONE',  ( -9.949568243101348131, 5.483630524090502334, 6.039417671888569039 ) ) ;
#183009 = CARTESIAN_POINT ( 'NONE',  ( 6.982085920913413624, 8.208483664896217391, -1.082531754730543971 ) ) ;
#183010 = CARTESIAN_POINT ( 'NONE',  ( 8.917737905728806425, 3.447199233515649386, 8.029567276306217138 ) ) ;
#183012 = CARTESIAN_POINT ( 'NONE',  ( 0.4865836442241474602, -1.705128007267729506, -0.6119416708995157883 ) ) ;
#183011 = CARTESIAN_POINT ( 'NONE',  ( 7.340813827156391191, 7.528980651296110160, 0.7998128361456281477 ) ) ;
#183013 = CARTESIAN_POINT ( 'NONE',  ( -5.343885102080728977, 9.386283052402845328, 0.7998128361456481317 ) ) ;
#183014 = CARTESIAN_POINT ( 'NONE',  ( 5.217190183160311356, 4.981143389975473568, -0.7998128361456211532 ) ) ;
#183015 = CARTESIAN_POINT ( 'NONE',  ( -6.081925898509194184, 7.037820769655190212, 1.000852813763454252 ) ) ;
#183016 = CARTESIAN_POINT ( 'NONE',  ( 5.365994935958575240, 9.482354201918870018, 0.7998128361456341429 ) ) ;
#183017 = CARTESIAN_POINT ( 'NONE',  ( 6.639320575229254118, 2.070803455257670844, 2.204946390281757207 ) ) ;
#183018 = DIRECTION ( 'NONE',  ( 0.000000000000000000, 0.000000000000000000, -1.000000000000000000 ) ) ;
#183019 = CARTESIAN_POINT ( 'NONE',  ( -11.44779964734699540, 10.99810470129610529, 3.599999963171390593 ) ) ;
#183020 = CARTESIAN_POINT ( 'NONE',  ( 8.405692050792682224, 12.75046512599275772, -0.7216878364870328300 ) ) ;
#183021 = VERTEX_POINT ( 'NONE', #103041 ) ;
#183022 = CARTESIAN_POINT ( 'NONE',  ( 2.892830138475974255, 0.2247066616481566970, 1.847348555264594960 ) ) ;
#183023 = AXIS2_PLACEMENT_3D ( 'NONE', #4705, #187752, #39381 ) ;
#183024 = CARTESIAN_POINT ( 'NONE',  ( 0.5443723441289443077, -1.386745921179835417, 1.321778134454040687 ) ) ;
#183025 = CARTESIAN_POINT ( 'NONE',  ( 0.5750489506927083383, -1.533040007955801753, 1.465245631482834821 ) ) ;
#183026 = CARTESIAN_POINT ( 'NONE',  ( 0.07680821025393774759, 7.629137130509076492, -2.410791881123967251 ) ) ;
#183027 = CARTESIAN_POINT ( 'NONE',  ( -0.1399997263889663501, 0.2375346743129815030, -2.034463206964792548 ) ) ;
#183028 = CARTESIAN_POINT ( 'NONE',  ( -1.518728846951488354, 8.688592980705449165, -2.528358009378028903 ) ) ;
#183029 = CARTESIAN_POINT ( 'NONE',  ( -2.819732761962332024, 6.233512622357263666, -0.7216878364870267237 ) ) ;
#183030 = CARTESIAN_POINT ( 'NONE',  ( 8.839552966430002101, 11.33589776563360019, -1.443375672974052559 ) ) ;
#183031 = CARTESIAN_POINT ( 'NONE',  ( 5.067230186376567858, 1.711625542863755012, 0.9741009975822639833 ) ) ;
#183032 = CARTESIAN_POINT ( 'NONE',  ( 1.049659257133638945, -1.915429643647760249, 0.9100379840868354497 ) ) ;
#183033 = CARTESIAN_POINT ( 'NONE',  ( -5.717788096661253761, 7.693838750903348789, 1.599625672291269396 ) ) ;
#183034 = CARTESIAN_POINT ( 'NONE',  ( -11.90624282132911382, 8.910973456084862576, -1.225840489975523306 ) ) ;
#183035 = CARTESIAN_POINT ( 'NONE',  ( 1.464175926609780964E-14, -2.537500000000001865, -3.475000000000000533 ) ) ;
#183036 = CARTESIAN_POINT ( 'NONE',  ( 5.437503290160631941, 0.8905978969957989433, -2.002497223260243153 ) ) ;
#183037 = CYLINDRICAL_SURFACE ( 'NONE', #1607, 0.08000000000000004330 ) ;
#183038 = CARTESIAN_POINT ( 'NONE',  ( 4.190394698586521471, -1.905300493120251515, -0.2835615876582204820 ) ) ;
#183039 = CARTESIAN_POINT ( 'NONE',  ( -8.505042434474312074, 8.816971016508505343, -0.7998128361456291469 ) ) ;
#183040 = CARTESIAN_POINT ( 'NONE',  ( 0.4283665542385572955, 1.745377284433462295, 0.5351633580037706839 ) ) ;
#183041 = CARTESIAN_POINT ( 'NONE',  ( 1.084930333755677045, -2.153824616689365978, -0.4803136671489223741 ) ) ;
#183042 = CARTESIAN_POINT ( 'NONE',  ( 5.462746646817801199, 6.412201880991806213, -1.228565393760511215 ) ) ;
#183043 = ORIENTED_EDGE ( 'NONE', *, *, #27140, .T. ) ;
#183044 = CARTESIAN_POINT ( 'NONE',  ( 2.943528747942701695, 6.448217615992859919, 0.000000000000000000 ) ) ;
#183045 = VERTEX_POINT ( 'NONE', #191730 ) ;
#183046 = CARTESIAN_POINT ( 'NONE',  ( 6.385607329849364078, -1.855618941174362879, 0.6602924305801564087 ) ) ;
#183047 = CARTESIAN_POINT ( 'NONE',  ( 0.8197486350577835035, 1.155594189952107609, -1.560708653158059622 ) ) ;
#183048 = CARTESIAN_POINT ( 'NONE',  ( 0.2630457479233569984, -2.015603748724136945, -0.05229424383911692592 ) ) ;
#183050 = CARTESIAN_POINT ( 'NONE',  ( 4.662867571641106323, 1.440366211568647303, -1.178370841985799888 ) ) ;
#183049 = CARTESIAN_POINT ( 'NONE',  ( -5.932574734431526942, 9.079031735882207244, 1.199719254218454489 ) ) ;
#183051 = CARTESIAN_POINT ( 'NONE',  ( 5.013482942003290255, 9.071090208970993274, -0.7998128361456481317 ) ) ;
#183052 = CARTESIAN_POINT ( 'NONE',  ( -0.7500000000000179856, 11.54166666666666607, 1.299038105676658228 ) ) ;
#183053 = PRESENTATION_STYLE_ASSIGNMENT (( #35732 ) ) ;
#183054 = CARTESIAN_POINT ( 'NONE',  ( -6.552668314106420588, 6.539201209412602189, -0.7998128361456291469 ) ) ;
#183055 = CARTESIAN_POINT ( 'NONE',  ( 6.720655732516647163, 0.005566325962592238996, 1.826293863978686982 ) ) ;
#183056 = CARTESIAN_POINT ( 'NONE',  ( 0.2752733618501881363, 2.042644424557562122, -0.7945232813236638991 ) ) ;
#183057 = CARTESIAN_POINT ( 'NONE',  ( 5.395781948558860286, 6.357795697149212444, -1.082531754730542195 ) ) ;
#183058 = AXIS2_PLACEMENT_3D ( 'NONE', #33213, #46291, #99297 ) ;
#183059 = CARTESIAN_POINT ( 'NONE',  ( 0.2999999999999927169, 3.999999999999974243, -1.007084189318427025 ) ) ;
#183060 = DIRECTION ( 'NONE',  ( 0.000000000000000000, -1.000000000000000000, 0.000000000000000000 ) ) ;
#183061 = CARTESIAN_POINT ( 'NONE',  ( 1.752308680507021155, 0.5713779359179693706, 1.734036872924920702 ) ) ;
#183062 = CARTESIAN_POINT ( 'NONE',  ( -2.923754682041362241, 6.562797562356882608, 0.7998128361456341429 ) ) ;
#183063 = CARTESIAN_POINT ( 'NONE',  ( 4.008270194328780178, -1.657810326508919685, 0.5087727743269004899 ) ) ;
#183064 = DIRECTION ( 'NONE',  ( 3.491481338843133355E-15, 0.000000000000000000, 1.000000000000000000 ) ) ;
#183065 = CARTESIAN_POINT ( 'NONE',  ( 6.509000000000010999, 0.007656933339201045172, 1.900274884395843245 ) ) ;
#183066 = CARTESIAN_POINT ( 'NONE',  ( 6.105879690743165926E-15, -11.10000000000000675, -0.2598076211376263434 ) ) ;
#183067 = CARTESIAN_POINT ( 'NONE',  ( 6.721331454403435934, -0.1262074967819451221, 1.796610827203233063 ) ) ;
#183068 = CARTESIAN_POINT ( 'NONE',  ( 4.698074428120575519, 0.8425069249109422564, -1.771795133841249203 ) ) ;
#183069 = AXIS2_PLACEMENT_3D ( 'NONE', #165737, #70331, #133269 ) ;
#183070 = CARTESIAN_POINT ( 'NONE',  ( -6.842061076390810292, 11.13415502243129218, 0.000000000000000000 ) ) ;
#183071 = CARTESIAN_POINT ( 'NONE',  ( 6.745345117998789775, 7.828323044875442172, 1.199719254218462483 ) ) ;
#183072 = EDGE_CURVE ( 'NONE', #133821, #62106, #175514, .T. ) ;
#183073 = CARTESIAN_POINT ( 'NONE',  ( 4.301511568767760529, 1.893648340000140040, -0.9544086401246790752 ) ) ;
#183074 = CARTESIAN_POINT ( 'NONE',  ( 7.530627977747744062, 7.750430493652658015, -0.7998128361456341429 ) ) ;
#183075 = CARTESIAN_POINT ( 'NONE',  ( -10.45741655484220267, 11.09474082360439873, -0.7998128361456221525 ) ) ;
#183076 = CARTESIAN_POINT ( 'NONE',  ( -6.484567079770452658, -6.583980363594976737, -7.100579091573040458 ) ) ;
#183077 = CARTESIAN_POINT ( 'NONE',  ( 3.045825399726838079, 1.460771095745692527, 1.467265538693182991 ) ) ;
#183079 = CARTESIAN_POINT ( 'NONE',  ( -1.364683531250014514, 0.09270833367475767028, 0.7879004041258379498 ) ) ;
#183078 = DIRECTION ( 'NONE',  ( 0.000000000000000000, -1.000000000000000000, 0.000000000000000000 ) ) ;
#183080 = ORIENTED_EDGE ( 'NONE', *, *, #73755, .F. ) ;
#183081 = CARTESIAN_POINT ( 'NONE',  ( 2.971610153692927803, -2.265147269936502727, -0.3905154627303064618 ) ) ;
#183082 = CARTESIAN_POINT ( 'NONE',  ( 9.097157885089661278, 9.715698408800516717, 1.040834085586084257E-14 ) ) ;
#183084 = CARTESIAN_POINT ( 'NONE',  ( 1.642778471875001811, -2.442708332855377140, 2.845375778867859751 ) ) ;
#183083 = CARTESIAN_POINT ( 'NONE',  ( 4.927462483923885195, 4.713404084191450849, -0.7998128361456481317 ) ) ;
#183085 = B_SPLINE_CURVE_WITH_KNOTS ( 'NONE', 3,
 ( #57324, #10684, #41094, #75704, #126669, #124546 ),
 .UNSPECIFIED., .F., .F.,
 ( 4, 2, 4 ),
 ( 0.000000000000000000, 0.0003767643964918269734, 0.0007535287929836536214 ),
 .UNSPECIFIED. ) ;
#183086 = CARTESIAN_POINT ( 'NONE',  ( 0.000000000000000000, 13.79999999999998295, 0.000000000000000000 ) ) ;
#183087 = ORIENTED_EDGE ( 'NONE', *, *, #149314, .T. ) ;
#183088 = CARTESIAN_POINT ( 'NONE',  ( -0.3999999999999854228, -6.938893903907228378E-15, -0.5000000000000368594 ) ) ;
#183089 = CARTESIAN_POINT ( 'NONE',  ( 3.515784362865181478, -0.5505564139345071606, 1.831456330389509501 ) ) ;
#183090 = CARTESIAN_POINT ( 'NONE',  ( -0.4866249300619188145, 6.869159268903599624, -3.677787980130352352 ) ) ;
#183091 = CARTESIAN_POINT ( 'NONE',  ( 4.787984082328099689, -0.8109719804370466578, 1.522229471167990233 ) ) ;
#183092 = CARTESIAN_POINT ( 'NONE',  ( 3.046111529846948329, 0.9110102549910354952, 1.799122713138465279 ) ) ;
#183093 = CARTESIAN_POINT ( 'NONE',  ( 4.729243902325204196, 2.292384926013335988, 0.1706581203582517303 ) ) ;
#183094 = CARTESIAN_POINT ( 'NONE',  ( -11.52901446936791352, 12.30574472532448205, -3.330874149801263062 ) ) ;
#183095 = CARTESIAN_POINT ( 'NONE',  ( 0.9442952520863318044, 0.8911936224933308948, -2.019119535841918278 ) ) ;
#183096 = CARTESIAN_POINT ( 'NONE',  ( -4.665414256878301025, 6.536345614481700927, -1.443375672974066548 ) ) ;
#183097 = ORIENTED_EDGE ( 'NONE', *, *, #139883, .T. ) ;
#183098 = CARTESIAN_POINT ( 'NONE',  ( 5.395664931544272847, -0.6364340197690997458, 1.651504472441939875 ) ) ;
#183100 = CARTESIAN_POINT ( 'NONE',  ( 2.431904175345489083, 1.079062523900159221, -2.022394142706671616 ) ) ;
#183099 = CARTESIAN_POINT ( 'NONE',  ( 5.091969210384201361, 8.098325291160362482, 1.199719254218452047 ) ) ;
#183101 = B_SPLINE_CURVE_WITH_KNOTS ( 'NONE', 3,
 ( #147472, #94467, #129171, #78186 ),
 .UNSPECIFIED., .F., .F.,
 ( 4, 4 ),
 ( 1.908185967165630741E-16, 0.0001045641765545072172 ),
 .UNSPECIFIED. ) ;
#183102 = CARTESIAN_POINT ( 'NONE',  ( 0.4975142532120572225, -0.5819891871022980778, -1.640261313346396133 ) ) ;
#183103 = CARTESIAN_POINT ( 'NONE',  ( -2.286521462199063492, 5.819358805874190743, 1.040834085586084257E-14 ) ) ;
#183104 = FILL_AREA_STYLE_COLOUR ( '', #159370 ) ;
#183105 = CARTESIAN_POINT ( 'NONE',  ( -8.072954122294394352, 8.383144328957069291, -0.7998128361456362523 ) ) ;
#183106 = CARTESIAN_POINT ( 'NONE',  ( 1.360316468749971364, -0.7031249996586053097, -3.469446951953614189E-14 ) ) ;
#183107 = CARTESIAN_POINT ( 'NONE',  ( 1.408343819019454993E-15, 4.000000000000003553, 11.49999999999998934 ) ) ;
#183108 = CARTESIAN_POINT ( 'NONE',  ( 6.584440175795505112, 1.195396180001909059, -1.690200020538407566 ) ) ;
#183109 = CARTESIAN_POINT ( 'NONE',  ( 0.6554828803995507158, 1.942095732595986890, -0.5424746339172461518 ) ) ;
#183110 = STYLED_ITEM ( 'NONE', ( #184954 ), #88981 ) ;
#183111 = CARTESIAN_POINT ( 'NONE',  ( -1.500000000000001332, 0.6812500006828161592, 0.000000000000000000 ) ) ;
#183112 = CARTESIAN_POINT ( 'NONE',  ( 5.215425455482871619, -0.2808245750387359796, 1.905809792320038998 ) ) ;
#183113 = CARTESIAN_POINT ( 'NONE',  ( -1.364683531250014514, 11.08854166700806410, -0.7879004041258335089 ) ) ;
#183114 = CARTESIAN_POINT ( 'NONE',  ( 1.916566064170255324, -2.220770990188126959, 0.06023022952456217466 ) ) ;
#183115 = VERTEX_POINT ( 'NONE', #108439 ) ;
#183117 = CARTESIAN_POINT ( 'NONE',  ( -8.673617379884035472E-15, 3.975067388631681187, -1.561251128379126385E-14 ) ) ;
#183116 = PRESENTATION_STYLE_ASSIGNMENT (( #144544 ) ) ;
#183118 = CARTESIAN_POINT ( 'NONE',  ( -0.2255463540285773671, 2.565807686639169471, -1.988980584585362754 ) ) ;
#183120 = EDGE_CURVE ( 'NONE', #88193, #94956, #169593, .T. ) ;
#183119 = CARTESIAN_POINT ( 'NONE',  ( 9.348510611822643313, 10.86534945433664134, 1.199719254218453823 ) ) ;
#183121 = DIRECTION ( 'NONE',  ( -0.9999753971658824625, 0.000000000000000000, 0.007014632059889242682 ) ) ;
#183122 = FILL_AREA_STYLE ('',( #70407 ) ) ;
#183123 = CARTESIAN_POINT ( 'NONE',  ( 4.405614404729386813, -0.7493292006620960732, -1.571029527175720863 ) ) ;
#183124 = CARTESIAN_POINT ( 'NONE',  ( 2.629291921057617554, 0.09916324773191761976, -1.959495597191794225 ) ) ;
#183126 = CARTESIAN_POINT ( 'NONE',  ( -7.212574532790100079, 9.437756259720353924, -1.443375672974059665 ) ) ;
#183125 = CARTESIAN_POINT ( 'NONE',  ( 4.847203612085560387, 5.613824621309978724, -1.199719254218452047 ) ) ;
#183127 = SURFACE_STYLE_FILL_AREA ( #84560 ) ;
#183128 = CARTESIAN_POINT ( 'NONE',  ( 4.367824458345868521, 3.990216711025275753, 0.1168690382639416964 ) ) ;
#183129 = CARTESIAN_POINT ( 'NONE',  ( 1.240767406152184282, -2.011986688465472906, -0.4537849334574247107 ) ) ;
#183130 = CARTESIAN_POINT ( 'NONE',  ( -8.193204901359996128, 8.453160561208463264, 1.040834085586084257E-14 ) ) ;
#183131 = CARTESIAN_POINT ( 'NONE',  ( -3.104453987404957260, 6.565687385373657925, -0.7216878364870257245 ) ) ;
#183132 = CARTESIAN_POINT ( 'NONE',  ( 0.9544393508495727652, 2.259765469927646375, -0.1136819296270324686 ) ) ;
#183133 = VERTEX_POINT ( 'NONE', #161397 ) ;
#183135 = EDGE_CURVE ( 'NONE', #182367, #84148, #74483, .T. ) ;
#183134 = CARTESIAN_POINT ( 'NONE',  ( 1.499999999999987121, 0.3270833340161527492, -0.8660254037844323793 ) ) ;
#183136 = CARTESIAN_POINT ( 'NONE',  ( 2.073319367481298858, 1.791407343212477077, -0.5384048943791116537 ) ) ;
#183137 = CARTESIAN_POINT ( 'NONE',  ( 1.002125825150332883, -1.692058386710117990, 0.3787823561424672469 ) ) ;
#183138 = CARTESIAN_POINT ( 'NONE',  ( 4.950807510372833065, -1.851323926424643274, -1.172527737679923465 ) ) ;
#183139 = CARTESIAN_POINT ( 'NONE',  ( 5.227664224568670193, -2.193190438267843323, 0.7177837189984050958 ) ) ;
#183140 = CARTESIAN_POINT ( 'NONE',  ( 1.129840139894950246, -1.306895429219852467, -1.593522927358894004 ) ) ;
#183141 = CARTESIAN_POINT ( 'NONE',  ( 3.345582828684705134, 1.942124712213384452, -0.0007862604347076693808 ) ) ;
#183142 = CARTESIAN_POINT ( 'NONE',  ( -4.650083499362882122, 6.448183387388563226, 1.443375672974064550 ) ) ;
#183143 = EDGE_CURVE ( 'NONE', #175731, #34023, #161387, .T. ) ;
#183144 = CARTESIAN_POINT ( 'NONE',  ( 5.887941446147332947, -0.8415115861447747259, 1.670666529855535654 ) ) ;
#183145 = CARTESIAN_POINT ( 'NONE',  ( 1.375000000000000888, 2.052068128417951609, -7.865587939079325464E-14 ) ) ;
#183146 = CARTESIAN_POINT ( 'NONE',  ( 4.016016189339381981, 7.573203028563332495, -0.3002613606930375489 ) ) ;
#183147 = CARTESIAN_POINT ( 'NONE',  ( 0.3679294144470013905, -0.4713284034136792644, 1.668465712161566916 ) ) ;
#183148 = CARTESIAN_POINT ( 'NONE',  ( 4.258669648468281110, 6.061810238003387141, 1.443375672974058777 ) ) ;
#183149 = CARTESIAN_POINT ( 'NONE',  ( -1.360316468750023544, 0.8906250003414064587, -2.602085213965210642E-14 ) ) ;
#183150 = CARTESIAN_POINT ( 'NONE',  ( 4.676407821165474488, 1.496050514612049742, 1.352155788975975437 ) ) ;
#183151 = CARTESIAN_POINT ( 'NONE',  ( -2.765500147063310266, 6.170241238308400433, 1.040834085586084257E-14 ) ) ;
#183152 = CARTESIAN_POINT ( 'NONE',  ( 7.411503528164766763, 11.79850454950093841, 1.040834085586084257E-14 ) ) ;
#183153 = CARTESIAN_POINT ( 'NONE',  ( 3.366167277942881064, 7.149221934233827014, -0.7998128361456362523 ) ) ;
#183155 = CYLINDRICAL_SURFACE ( 'NONE', #136735, 0.3999999999999997446 ) ;
#183154 = CARTESIAN_POINT ( 'NONE',  ( 2.279681363911123970, 1.122676072794186908, 1.439608767588994365 ) ) ;
#183156 = CARTESIAN_POINT ( 'NONE',  ( -5.285699784481336927, 7.260012063351913625, 1.599625672291263179 ) ) ;
#183157 = DIRECTION ( 'NONE',  ( 0.6743504407188151140, 0.000000000000000000, 0.7384114592165670343 ) ) ;
#183158 = CARTESIAN_POINT ( 'NONE',  ( -1.743066579297358008E-15, 1.875000000682791379, 1.224999999999958566 ) ) ;
#183159 = ORIENTED_EDGE ( 'NONE', *, *, #71839, .T. ) ;
#183160 = CARTESIAN_POINT ( 'NONE',  ( -6.414416072596849538, 7.616478518518682073, -1.082531754730549967 ) ) ;
#183161 = CARTESIAN_POINT ( 'NONE',  ( 1.620863580070950549, 0.4000000000000010214, -1.903365770102946941 ) ) ;
#183162 = CARTESIAN_POINT ( 'NONE',  ( -9.345647958521597687, 9.797677461230342999, 0.7998128361456462443 ) ) ;
#183163 = CARTESIAN_POINT ( 'NONE',  ( 6.358070640981934751, 0.7709996861101749976, -1.866924874111668853 ) ) ;
#183165 = VERTEX_POINT ( 'NONE', #209038 ) ;
#183164 = CARTESIAN_POINT ( 'NONE',  ( 6.533822986070857652, -2.155494434802426973, 0.5362405526610786177 ) ) ;
#183166 = CARTESIAN_POINT ( 'NONE',  ( -6.587282531393266360, 8.778525268082516320, 1.599625672291269396 ) ) ;
#183167 = CARTESIAN_POINT ( 'NONE',  ( 5.355634372598031767, 6.206993841907870291, -1.199719254218445830 ) ) ;
#183168 = AXIS2_PLACEMENT_3D ( 'NONE', #130822, #213047, #98260 ) ;
#183169 = CARTESIAN_POINT ( 'NONE',  ( 5.418845456765190249, 1.903306360667684993, 0.7908678518537788360 ) ) ;
#183170 = CARTESIAN_POINT ( 'NONE',  ( 4.887342357109404567, -0.6819942819097267739, -1.897698409216505011 ) ) ;
#183171 = ORIENTED_EDGE ( 'NONE', *, *, #13102, .F. ) ;
#183172 = CARTESIAN_POINT ( 'NONE',  ( 9.871989323747737188, 3.235871879154604169, 6.146221223954385415 ) ) ;
#183173 = LINE ( 'NONE', #16386, #2981 ) ;
#183175 = EDGE_LOOP ( 'NONE', ( #35362, #179326, #142067, #64236 ) ) ;
#183174 = CARTESIAN_POINT ( 'NONE',  ( -6.967964602780620353, 7.093989889524320525, 0.000000000000000000 ) ) ;
#183176 = CARTESIAN_POINT ( 'NONE',  ( 5.043764445095213489, 7.992138250556588552, 1.161813593947092382 ) ) ;
#183177 = CARTESIAN_POINT ( 'NONE',  ( 5.378279760196133630, -0.2985789616767355326, 1.993766414912321316 ) ) ;
#183178 = CARTESIAN_POINT ( 'NONE',  ( 4.628748294741646951, -1.682209325509572473, 0.7487199040775437409 ) ) ;
#183179 = CARTESIAN_POINT ( 'NONE',  ( -0.02338929933906607611, 7.629137130509112907, -2.310989781590186976 ) ) ;
#183180 = CARTESIAN_POINT ( 'NONE',  ( 2.807580367715529324, 1.950013211217585196, 1.233794411958085036 ) ) ;
#183181 = CARTESIAN_POINT ( 'NONE',  ( 6.855582950365507244, 8.027210192628430718, -1.199719254218452047 ) ) ;
#183182 = CARTESIAN_POINT ( 'NONE',  ( 5.061884429210019576, 2.138887713127162638, -0.3115965683029159883 ) ) ;
#183183 = CARTESIAN_POINT ( 'NONE',  ( 7.283754839039659146, 9.520799950344851936, -1.599625672291262513 ) ) ;
#183184 = CARTESIAN_POINT ( 'NONE',  ( -0.006442494416806704600, -1.941642170872309281, -0.04679624317607820189 ) ) ;
#183185 = CARTESIAN_POINT ( 'NONE',  ( -5.610376637956639101, 5.439860920571172542, 0.000000000000000000 ) ) ;
#183186 = CARTESIAN_POINT ( 'NONE',  ( -9.383668910029371091, 15.40608514343435509, -7.388226147498031082 ) ) ;
#183187 = CARTESIAN_POINT ( 'NONE',  ( -4.034433228518296666, 6.864533312316751790, -1.199719254218450271 ) ) ;
#183188 = CARTESIAN_POINT ( 'NONE',  ( 3.291731440620565330, -0.7593194595177065187, 1.709801165022284408 ) ) ;
#183191 = CARTESIAN_POINT ( 'NONE',  ( -6.934069218746458318, 7.054445274817795486, -0.7998128361456362523 ) ) ;
#183190 = CARTESIAN_POINT ( 'NONE',  ( 0.7499999999999867883, -0.9020833326505162120, -1.299038105676652011 ) ) ;
#183189 = CARTESIAN_POINT ( 'NONE',  ( 1.318461241437279607, -0.6911404020932455650, -1.783297644634279200 ) ) ;
#183192 = CARTESIAN_POINT ( 'NONE',  ( 2.420803835572300500, 1.440536793087299205, -1.671967039616916617 ) ) ;
#183193 = CARTESIAN_POINT ( 'NONE',  ( 3.785751206713845018, 5.439795712631356750, 1.599625672291267398 ) ) ;
#183194 = CARTESIAN_POINT ( 'NONE',  ( 7.797347741190739256, 8.269529584243604958, 0.7216878364870267237 ) ) ;
#183195 = CARTESIAN_POINT ( 'NONE',  ( -3.598799709423620374, 6.286017863381107240, 1.199719254218464037 ) ) ;
#183196 = CARTESIAN_POINT ( 'NONE',  ( -6.956742217143487395, 8.249192353823097790, 1.082531754730549078 ) ) ;
#183197 = CARTESIAN_POINT ( 'NONE',  ( 0.2101411907093185261, -0.8379918008738492796, -1.782380744178988285 ) ) ;
#183198 = CARTESIAN_POINT ( 'NONE',  ( 6.463506322211490129, 0.4017315814064837953, -2.272322137143814480 ) ) ;
#183199 = CARTESIAN_POINT ( 'NONE',  ( 1.258172656280614365, -1.962046632281065461, -0.003472340283867945618 ) ) ;
#183200 = CARTESIAN_POINT ( 'NONE',  ( 4.504768599022889397, 0.5450402360923761735, 1.989220403428487938 ) ) ;
#183201 = CARTESIAN_POINT ( 'NONE',  ( 5.748293942514166588, 7.729428904398431222, -1.443375672974057666 ) ) ;
#183202 = CARTESIAN_POINT ( 'NONE',  ( 6.343235766347262938, 8.493804042195527870, -1.599625672291281386 ) ) ;
#183203 = ORIENTED_EDGE ( 'NONE', *, *, #204199, .F. ) ;
#183204 = CARTESIAN_POINT ( 'NONE',  ( 8.717529583462654941, 9.272798723569005475, 0.7216878364870458196 ) ) ;
#183205 = CARTESIAN_POINT ( 'NONE',  ( 0.6823417656249899377, 4.238541667008085767, -1.181850606188754593 ) ) ;
#183206 = CARTESIAN_POINT ( 'NONE',  ( 11.84100621633422179, 12.48958425776664072, -1.444132586618106728 ) ) ;
#183207 = CARTESIAN_POINT ( 'NONE',  ( 3.185802909086937973, 6.660594460669327255, 0.7216878364870317197 ) ) ;
#183208 = CARTESIAN_POINT ( 'NONE',  ( 6.338351057450786641, -1.166998422550720393, 1.830725944502207048 ) ) ;
#183210 = CARTESIAN_POINT ( 'NONE',  ( 6.427308110136687347, -1.208249125052461181, -1.389453836245766016 ) ) ;
#183209 = CARTESIAN_POINT ( 'NONE',  ( 9.481348452320355946, -9.199999999999983302, -0.5950054837414361364 ) ) ;
#183211 = EDGE_CURVE ( 'NONE', #161745, #166496, #28181, .T. ) ;
#183212 = CYLINDRICAL_SURFACE ( 'NONE', #110178, 2.000000000000000000 ) ;
#183213 = FACE_OUTER_BOUND ( 'NONE', #192864, .T. ) ;
#183214 = CARTESIAN_POINT ( 'NONE',  ( 1.739302498465819191, -1.351291084634953066, -1.293660915597586003 ) ) ;
#183215 = CARTESIAN_POINT ( 'NONE',  ( -6.025499844618653178, 6.066343344509915525, -0.6079853925319089747 ) ) ;
#183216 = CARTESIAN_POINT ( 'NONE',  ( 6.304162555737000240, 6.968127521147626346, -0.9177210060461529206 ) ) ;
#183217 = CARTESIAN_POINT ( 'NONE',  ( -1.364683531249997417, 5.321875000341417916, 1.214306433183764966E-14 ) ) ;
#183218 = CARTESIAN_POINT ( 'NONE',  ( 1.365713085969634477, 0.5541664655046051324, -1.830235057661818487 ) ) ;
#183219 = CARTESIAN_POINT ( 'NONE',  ( 3.502600007508451352, 1.395586194379776712, -1.088321832170894288 ) ) ;
#183220 = CARTESIAN_POINT ( 'NONE',  ( 0.6977377480232997975, 1.284608138224270002, 1.416691289136004395 ) ) ;
#183222 = CARTESIAN_POINT ( 'NONE',  ( 3.831564657165886789, 0.6421465917123435618, -1.804920456748728474 ) ) ;
#183221 = CARTESIAN_POINT ( 'NONE',  ( 5.591005849568446706, 5.791977450266268868, -0.7139200525481930182 ) ) ;
#183223 = CARTESIAN_POINT ( 'NONE',  ( -1.500000000000015099, -1.079166666666641961, 0.8660254037844403729 ) ) ;
#183224 = CARTESIAN_POINT ( 'NONE',  ( 5.916450756658795385, 0.7966118609284984498, 1.801439653064011548 ) ) ;
#183225 = CARTESIAN_POINT ( 'NONE',  ( 1.459403507577087700, -1.788631592985808538, 1.138920039206146928 ) ) ;
#183226 = CARTESIAN_POINT ( 'NONE',  ( 0.1747071867222109443, -7.850481869465713913, -10.96497182194659281 ) ) ;
#183227 = CARTESIAN_POINT ( 'NONE',  ( 3.836663719693265584, 0.2738035037005565053, 1.850374562403465983 ) ) ;
#183229 = ORIENTED_EDGE ( 'NONE', *, *, #14569, .T. ) ;
#183228 = CARTESIAN_POINT ( 'NONE',  ( 0.09986456629675066754, -1.825204794925545881, -0.04862044751281074939 ) ) ;
#183231 = CARTESIAN_POINT ( 'NONE',  ( 9.994890815243271831, 3.870538056096196833, 5.945519334325363836 ) ) ;
#183230 = CARTESIAN_POINT ( 'NONE',  ( 3.791807063958370971, 1.597966631936774684, 1.522356218736670153 ) ) ;
#183232 = AXIS2_PLACEMENT_3D ( 'NONE', #50321, #116439, #132670 ) ;
#183233 = CARTESIAN_POINT ( 'NONE',  ( -0.6823417656250212460, 5.363541667008087543, 1.181850606188767472 ) ) ;
#183234 = EDGE_CURVE ( 'NONE', #88615, #102537, #194945, .T. ) ;
#183235 = CARTESIAN_POINT ( 'NONE',  ( 0.8364713509731898089, -1.147405136530167624, 1.713900253247694350 ) ) ;
#183236 = CARTESIAN_POINT ( 'NONE',  ( 7.233438648090761980, 8.397765496649418182, 1.199719254218462483 ) ) ;
#183237 = CARTESIAN_POINT ( 'NONE',  ( -7.506410603460441422, 11.90922947067921278, -0.7998128361456291469 ) ) ;
#183238 = CARTESIAN_POINT ( 'NONE',  ( 4.909461021924244051, 6.821066840368686712, 1.443375672974065660 ) ) ;
#183239 = CARTESIAN_POINT ( 'NONE',  ( 11.94980361490495291, 11.00332124735860617, -1.099999952232860512 ) ) ;
#183240 = CARTESIAN_POINT ( 'NONE',  ( 8.167861197590044142, 8.493869250135347215, 0.000000000000000000 ) ) ;
#183241 = ORIENTED_EDGE ( 'NONE', *, *, #45284, .T. ) ;
#183242 = CARTESIAN_POINT ( 'NONE',  ( 3.965334771736851671, 1.774175476309115984, 1.066894043611272824 ) ) ;
#183243 = CARTESIAN_POINT ( 'NONE',  ( 1.499999999999989120, 4.004166666666685970, 0.8660254037844524744 ) ) ;
#183244 = CARTESIAN_POINT ( 'NONE',  ( 1.669428131952359839, 0.1607934374257547205, -2.155692497560882437 ) ) ;
#183245 = CARTESIAN_POINT ( 'NONE',  ( -6.320392545075788959, 6.875563024200552320, -0.7000339101758262794 ) ) ;
#183246 = CARTESIAN_POINT ( 'NONE',  ( 1.506516584307997730, -2.010164795747824140, -0.1955670033209846170 ) ) ;
#183247 = CARTESIAN_POINT ( 'NONE',  ( 5.788968402910781741, 5.856144012925177833, 0.7216878364870568108 ) ) ;
#183248 = ORIENTED_EDGE ( 'NONE', *, *, #119616, .T. ) ;
#183250 = CARTESIAN_POINT ( 'NONE',  ( 7.456621297836067086, 10.68284669990868174, 1.082531754730558626 ) ) ;
#183249 = CARTESIAN_POINT ( 'NONE',  ( -3.475000000000000533, -3.879166666666665986, -2.006292185433948827 ) ) ;
#183251 = CARTESIAN_POINT ( 'NONE',  ( 6.819686488043297246, -1.560180513003786462, 1.276622200526676743 ) ) ;
#183252 = CARTESIAN_POINT ( 'NONE',  ( 6.473869786608328347, -0.8128310455158479497, 1.733272608194774689 ) ) ;
#183253 = FACE_OUTER_BOUND ( 'NONE', #204602, .T. ) ;
#183254 = CARTESIAN_POINT ( 'NONE',  ( 4.370767597569780172, -0.0006098066561242150270, -2.191739723162715592 ) ) ;
#183255 = CARTESIAN_POINT ( 'NONE',  ( 1.499999999999987121, 3.577083334016152527, -0.8660254037844262731 ) ) ;
#183256 = CARTESIAN_POINT ( 'NONE',  ( 3.216961742616857745, 1.504763323797538410, -1.180078671740567131 ) ) ;
#183257 = CARTESIAN_POINT ( 'NONE',  ( -5.915435094264120508, 5.795762452929912101, 0.000000000000000000 ) ) ;
#183258 = CARTESIAN_POINT ( 'NONE',  ( 3.348500752450929596, 6.850408611260650815, 0.7216878364870317197 ) ) ;
#183260 = CARTESIAN_POINT ( 'NONE',  ( 0.8433753223025289847, 0.3905737783656983431, -1.978056610397058712 ) ) ;
#183259 = CARTESIAN_POINT ( 'NONE',  ( -10.15469386651127515, 11.90985960142705657, 1.082531754730558626 ) ) ;
#183261 = CARTESIAN_POINT ( 'NONE',  ( 1.364683531250000303, 12.06770833367473195, -0.7879004041258355073 ) ) ;
#183263 = CARTESIAN_POINT ( 'NONE',  ( -6.317173229324657413, 6.334733287159020954, 0.000000000000000000 ) ) ;
#183262 = CARTESIAN_POINT ( 'NONE',  ( 0.1172542576415449567, -0.1040641125494116137, 2.290134469065004730 ) ) ;
#183264 = CARTESIAN_POINT ( 'NONE',  ( 3.750762392430748271, -1.410035727865316613, 0.9929894849482110430 ) ) ;
#183265 = CARTESIAN_POINT ( 'NONE',  ( -0.1399997263889836974, 2.022132088033218533, -2.415689637818136948 ) ) ;
#183266 = CARTESIAN_POINT ( 'NONE',  ( 5.332434488876471868, 5.115595079977664383, 0.7998128361456341429 ) ) ;
#183267 = DIRECTION ( 'NONE',  ( -0.000000000000000000, -1.000000000000000000, 0.000000000000000000 ) ) ;
#183268 = CARTESIAN_POINT ( 'NONE',  ( 1.732786548908150870, -1.861864252656076912, -0.6185235971247133868 ) ) ;
#183269 = DIRECTION ( 'NONE',  ( 0.000000000000000000, 1.000000000000000000, 0.000000000000000000 ) ) ;
#183270 = CARTESIAN_POINT ( 'NONE',  ( 3.344057444064992168, 7.053150784717805877, 1.040834085586084257E-14 ) ) ;
#183271 = CARTESIAN_POINT ( 'NONE',  ( 0.1753634416057741896, 2.865130778691078905, -2.632309609290182095 ) ) ;
#183272 = VERTEX_POINT ( 'NONE', #124704 ) ;
#183273 = FACE_OUTER_BOUND ( 'NONE', #44351, .T. ) ;
#183274 = ORIENTED_EDGE ( 'NONE', *, *, #152161, .T. ) ;
#183275 = CARTESIAN_POINT ( 'NONE',  ( 3.686021078551263930, 1.009145865423091815, 1.504116352017518476 ) ) ;
#183276 = VERTEX_POINT ( 'NONE', #46581 ) ;
#183277 = CARTESIAN_POINT ( 'NONE',  ( 7.530627977747744062, 7.750430493652658015, -0.7998128361456341429 ) ) ;
#183278 = CARTESIAN_POINT ( 'NONE',  ( 4.934241560730721510, 4.721313007132757811, 0.000000000000000000 ) ) ;
#183279 = CARTESIAN_POINT ( 'NONE',  ( 5.022017691244989201, -1.802217576119311770, 0.1829344734397136685 ) ) ;
#183280 = CARTESIAN_POINT ( 'NONE',  ( 6.387299765369506055, 7.584842826753462219, -1.082531754730548412 ) ) ;
#183281 = CARTESIAN_POINT ( 'NONE',  ( 5.538030394937467626, 6.199453712711876285, -0.9301498999644899346 ) ) ;
#183282 = ORIENTED_EDGE ( 'NONE', *, *, #195251, .F. ) ;
#183283 = EDGE_CURVE ( 'NONE', #142732, #196836, #211421, .T. ) ;
#183285 = CARTESIAN_POINT ( 'NONE',  ( 10.53876547652418338, 11.18964789890005918, 0.7998128361456462443 ) ) ;
#183284 = CARTESIAN_POINT ( 'NONE',  ( 6.004338076955692216, 1.858996105215251493, 0.09048898905416635774 ) ) ;
#183286 = CARTESIAN_POINT ( 'NONE',  ( 3.603066768525709396, -0.1374138116273740384, 1.910719597520103896 ) ) ;
#183287 = DIRECTION ( 'NONE',  ( -1.568190022283037360E-15, 0.8656921114426511243, -0.5005768354468317360 ) ) ;
#183288 = CARTESIAN_POINT ( 'NONE',  ( -12.46228870304231329, 8.331136472732479703, -2.451782011337487965 ) ) ;
#183289 = DIRECTION ( 'NONE',  ( 0.000000000000000000, 1.000000000000000000, 0.000000000000000000 ) ) ;
#183290 = FACE_OUTER_BOUND ( 'NONE', #120256, .T. ) ;
#183291 = CARTESIAN_POINT ( 'NONE',  ( 6.209271165378815738, 7.306866450105836464, -1.082531754730543083 ) ) ;
#183292 = CARTESIAN_POINT ( 'NONE',  ( -3.277320446201389181, 4.846626492033466072, 1.599625672291267398 ) ) ;
#183293 = CARTESIAN_POINT ( 'NONE',  ( 0.7960496800812134621, -0.7770375076890515542, 2.017388685454111652 ) ) ;
#183294 = CARTESIAN_POINT ( 'NONE',  ( -3.949167883330528372, 7.829389307186077396, 1.214306433183764966E-14 ) ) ;
#183295 = CARTESIAN_POINT ( 'NONE',  ( 4.529305835417093640, 7.441884687032027657, -1.199719254218450271 ) ) ;
#183296 = CARTESIAN_POINT ( 'NONE',  ( 1.043660158496478196, 0.7440559408637310579, -1.667260813828251642 ) ) ;
#183297 = CARTESIAN_POINT ( 'NONE',  ( -3.307299406729781399, 5.945934176904983381, -1.199719254218452935 ) ) ;
#183298 = CARTESIAN_POINT ( 'NONE',  ( 3.065264358586119009, 0.2694654384877669395, -1.805464241506696155 ) ) ;
#183299 = CARTESIAN_POINT ( 'NONE',  ( 1.634869402278725348, 1.785593253932623803, 0.6852637533772619749 ) ) ;
#183300 = ORIENTED_EDGE ( 'NONE', *, *, #150437, .T. ) ;
#183301 = CARTESIAN_POINT ( 'NONE',  ( 2.998452255303164726, 1.954363348466476857, 0.2436675063324095225 ) ) ;
#183302 = CARTESIAN_POINT ( 'NONE',  ( 5.249535210367334948, 1.939651965044559390, -0.09935550175556999430 ) ) ;
#183303 = CARTESIAN_POINT ( 'NONE',  ( -6.050681693448748177, 10.28115541899069463, 0.7998128361456291469 ) ) ;
#183305 = CARTESIAN_POINT ( 'NONE',  ( 4.306960158517386894, -0.4675538901007176285, -2.068242682749166672 ) ) ;
#183304 = CARTESIAN_POINT ( 'NONE',  ( 3.464990776744291345, 6.200183785247111778, 1.199719254218452047 ) ) ;
#183306 = CARTESIAN_POINT ( 'NONE',  ( -9.911098634504678095E-13, -7.246166700193024113, 9.500331257164617682 ) ) ;
#183307 = CARTESIAN_POINT ( 'NONE',  ( 9.585778300061798873, 11.14216175728232550, -1.199719254218440723 ) ) ;
#183308 = CARTESIAN_POINT ( 'NONE',  ( 5.639836874842681702, 6.325236607244836051, 1.140081021588116084 ) ) ;
#183309 = DIRECTION ( 'NONE',  ( 0.000000000000000000, 0.7071067811865469066, 0.7071067811865481278 ) ) ;
#183310 = ORIENTED_EDGE ( 'NONE', *, *, #30821, .T. ) ;
#183311 = CARTESIAN_POINT ( 'NONE',  ( -1.402160292154681736E-14, 13.17187500034139980, 1.575800808251682339 ) ) ;
#183312 = CARTESIAN_POINT ( 'NONE',  ( 5.011674058906918638, 5.875983152593414971, 1.199719254218452047 ) ) ;
#183313 = CARTESIAN_POINT ( 'NONE',  ( 5.009901455449552010, 5.803638771901306725, -1.199719254218452047 ) ) ;
#183314 = AXIS2_PLACEMENT_3D ( 'NONE', #69980, #53768, #3910 ) ;
#183315 = CARTESIAN_POINT ( 'NONE',  ( 5.712781623311797397, 7.758274208654143855, -1.599625672291283607 ) ) ;
#183317 =( BOUNDED_CURVE ( )  B_SPLINE_CURVE ( 2, ( #173550, #190818, #156222, #25124, #123801, #170308, #189761, #40336, #141066 ),
 .UNSPECIFIED., .F., .T. ) 
 B_SPLINE_CURVE_WITH_KNOTS ( ( 3, 2, 2, 2, 3 ),
 ( 0.5156250000000002220, 0.5208333333333333703, 0.5312500000000000000, 0.5416666666666666297, 0.5468749999999997780 ),
 .UNSPECIFIED. ) 
 CURVE ( )  GEOMETRIC_REPRESENTATION_ITEM ( )  RATIONAL_B_SPLINE_CURVE ( ( 0.9330127018922194093, 0.9330127018922221849, 1.000000000000000000, 0.8660254037844387076, 1.000000000000000000, 0.8660254037844387076, 1.000000000000000000, 0.9330127018922221849, 0.9330127018922194093 ) ) 
 REPRESENTATION_ITEM ( '' )  );
#183316 = DIRECTION ( 'NONE',  ( 0.000000000000000000, 1.804652791718263484E-16, -1.000000000000000000 ) ) ;
#183318 = CARTESIAN_POINT ( 'NONE',  ( 4.459475772512963232, 0.3974328844052883447, -1.781742007231662983 ) ) ;
#183319 = CARTESIAN_POINT ( 'NONE',  ( -5.974412749747273210, 4.760129193867236097, 2.438793960827106311 ) ) ;
#183320 = CARTESIAN_POINT ( 'NONE',  ( -7.971831135155409420, 11.28392484344787405, 1.082531754730549967 ) ) ;
#183321 = CARTESIAN_POINT ( 'NONE',  ( -6.612840081267999714, 6.759580388257274919, -0.1161152146933758927 ) ) ;
#183322 = FACE_OUTER_BOUND ( 'NONE', #96707, .T. ) ;
#183323 = CARTESIAN_POINT ( 'NONE',  ( 5.506679003988666388, 1.415762158562785533, -1.222804595763474333 ) ) ;
#183324 = CARTESIAN_POINT ( 'NONE',  ( 6.076025397218672630, 10.24044673006381245, -0.7998128361456291469 ) ) ;
#183325 = CARTESIAN_POINT ( 'NONE',  ( -5.786632634934295361, 5.645492917045106473, 0.7998128361456341429 ) ) ;
#183326 = EDGE_CURVE ( 'NONE', #175615, #139393, #212695, .T. ) ;
#183327 = CARTESIAN_POINT ( 'NONE',  ( 2.869522067586683711, 6.499526178826442013, 0.7998128361456362523 ) ) ;
#183328 = CARTESIAN_POINT ( 'NONE',  ( 0.6823417656249969321, 9.838541667008065872, -1.181850606188757036 ) ) ;
#183329 = CARTESIAN_POINT ( 'NONE',  ( -5.545448523189368650, 6.428443684264421698, -1.199719254218446718 ) ) ;
#183330 = CARTESIAN_POINT ( 'NONE',  ( 4.695201269034174452, 4.372156323494968966, 1.214306433183764966E-14 ) ) ;
#183331 = COLOUR_RGB ( '', 0.66274510, 0.83137255, 0.94901961) ;
#183332 = EDGE_CURVE ( 'NONE', #179865, #102987, #126837, .T. ) ;
#183333 = CARTESIAN_POINT ( 'NONE',  ( -3.973948422136981407, 5.729635473950147606, -1.443375672974066548 ) ) ;
#183334 = CARTESIAN_POINT ( 'NONE',  ( 1.476322311366547124, -2.107388574805735271, -0.2037450385454323831 ) ) ;
#183335 = CARTESIAN_POINT ( 'NONE',  ( 7.703003830858588863, 12.13858823597705872, -0.7998128361456291469 ) ) ;
#183336 = CARTESIAN_POINT ( 'NONE',  ( -1.499999999999981126, 3.629166666666691743, -0.8660254037844499209 ) ) ;
#183337 = CARTESIAN_POINT ( 'NONE',  ( 6.491088764554701740, 0.1969099459505334604, 2.060843999385448821 ) ) ;
#183339 = CARTESIAN_POINT ( 'NONE',  ( 4.003607682157598546, 7.822813005323850710, -0.1595685970469905290 ) ) ;
#183338 = CARTESIAN_POINT ( 'NONE',  ( 1.962219809069129184, -1.683971100191889336, -0.7449956418128443891 ) ) ;
#183340 = CARTESIAN_POINT ( 'NONE',  ( 4.365362273920230685, 8.036747052974847705, 0.7216878364870298324 ) ) ;
#183342 = CARTESIAN_POINT ( 'NONE',  ( 11.92619526913699879, 10.89999999999998259, 1.328859060402684644 ) ) ;
#183341 = CARTESIAN_POINT ( 'NONE',  ( -3.475000000000000533, -3.149999999999999911, 0.000000000000000000 ) ) ;
#183343 = CARTESIAN_POINT ( 'NONE',  ( 1.746416057278064482, 0.7220573502318957670, 2.175635376676859689 ) ) ;
#183345 = DIRECTION ( 'NONE',  ( 1.000000000000000000, 0.000000000000000000, 0.000000000000000000 ) ) ;
#183344 = CARTESIAN_POINT ( 'NONE',  ( -1.123270288249905713, 3.300000000000025135, 0.7750000000000117906 ) ) ;
#183346 = EDGE_LOOP ( 'NONE', ( #22251, #166284, #116239, #49982 ) ) ;
#183348 = EDGE_CURVE ( 'NONE', #179696, #33385, #111635, .T. ) ;
#183347 = CARTESIAN_POINT ( 'NONE',  ( 8.771762197917315262, 10.29643932140079166, -1.082531754730543083 ) ) ;
#183349 = CARTESIAN_POINT ( 'NONE',  ( 0.1232915322694717181, 1.753566389086946398, 0.9887636377800024245 ) ) ;
#183350 = CARTESIAN_POINT ( 'NONE',  ( 0.6198768371072012062, 1.941228818809427104, -0.2821078022595123747 ) ) ;
#183351 = CARTESIAN_POINT ( 'NONE',  ( 6.473846665049121540, -0.8576149079453172508, 1.823233050095712349 ) ) ;
#183353 = CARTESIAN_POINT ( 'NONE',  ( 6.471393748265519719, 5.229711127717882491, -2.419999999999995044 ) ) ;
#183352 = CARTESIAN_POINT ( 'NONE',  ( -8.202846631467911820, 9.528741477256060577, 1.199719254218462483 ) ) ;
#183354 = CARTESIAN_POINT ( 'NONE',  ( 1.154700538379228147, -2.500000000000002220, -1.734723475976807094E-15 ) ) ;
#183356 = CARTESIAN_POINT ( 'NONE',  ( 1.850134630017237880, 0.5516246727584225296, 1.681758779177483287 ) ) ;
#183355 = CARTESIAN_POINT ( 'NONE',  ( 4.207035958355084482, -0.3574298538902004885, 2.059684413417623094 ) ) ;
#183357 = DIRECTION ( 'NONE',  ( -0.000000000000000000, 1.000000000000000000, -0.000000000000000000 ) ) ;
#183359 = CARTESIAN_POINT ( 'NONE',  ( 5.630919443038269634, -2.074398886797897301, 0.9756724061340553700 ) ) ;
#183358 = CARTESIAN_POINT ( 'NONE',  ( -10.91033920341459051, 4.885615726745599297, 4.996448585388897357 ) ) ;
#183360 = CARTESIAN_POINT ( 'NONE',  ( 3.837644434229481316, 1.732183052659850286, 0.1680905250187741673 ) ) ;
#183361 = B_SPLINE_CURVE_WITH_KNOTS ( 'NONE', 3,
 ( #174180, #30037, #93994, #208764, #12693, #96123 ),
 .UNSPECIFIED., .F., .F.,
 ( 4, 2, 4 ),
 ( 0.000000000000000000, 0.002110194456903486965, 0.004220388913806973931 ),
 .UNSPECIFIED. ) ;
#183362 = CARTESIAN_POINT ( 'NONE',  ( 3.216308754939877446, 4.775446185561722956, -1.599625672291262513 ) ) ;
#183363 = CARTESIAN_POINT ( 'NONE',  ( 5.520104819419390907, 6.469152373191302985, 1.199719254218452935 ) ) ;
#183364 = CARTESIAN_POINT ( 'NONE',  ( 2.793977985172685141, -1.619072854944574313, 0.6208489642184951141 ) ) ;
#183365 = CARTESIAN_POINT ( 'NONE',  ( 3.051421578680337809, 1.863438581370242986, -1.114033871086346217 ) ) ;
#183366 = CARTESIAN_POINT ( 'NONE',  ( 4.847203612085560387, 5.613824621309978724, -1.199719254218452047 ) ) ;
#183367 = CARTESIAN_POINT ( 'NONE',  ( 4.276577519141481432, -0.4465006364167342645, -1.966305148836451577 ) ) ;
#183368 = CARTESIAN_POINT ( 'NONE',  ( 1.093750000000000666, -1.895863743164112547, -0.7852924748299294766 ) ) ;
#183369 = CARTESIAN_POINT ( 'NONE',  ( -1.499999999999997780, 4.181250000682819490, 1.214306433183764966E-14 ) ) ;
#183370 = CARTESIAN_POINT ( 'NONE',  ( 2.274328125206574569, -1.186679513062695257, 1.517402005686524280 ) ) ;
#183371 = CARTESIAN_POINT ( 'NONE',  ( -1.364683531250000748, 15.35937500034140157, 0.000000000000000000 ) ) ;
#183372 = CARTESIAN_POINT ( 'NONE',  ( 5.150715375432683985, 2.188637957643671417, 0.3792565894785212000 ) ) ;
#183373 = ORIENTED_EDGE ( 'NONE', *, *, #196923, .F. ) ;
#183374 = CARTESIAN_POINT ( 'NONE',  ( -0.1110810684432622653, 5.724789179085956192, -2.391029204513066553 ) ) ;
#183375 = CARTESIAN_POINT ( 'NONE',  ( -0.7500000000000215383, 1.191666666666688190, 1.299038105676659116 ) ) ;
#183376 = CARTESIAN_POINT ( 'NONE',  ( 5.289652487626049115, 9.323011668872403845, 0.7998128361456462443 ) ) ;
#183377 = CARTESIAN_POINT ( 'NONE',  ( 5.788968402910816380, 5.856144012925152076, 0.7216878364870317197 ) ) ;
#183378 = CARTESIAN_POINT ( 'NONE',  ( 1.642778471875001811, -2.092708332855373943, 2.845375778867859751 ) ) ;
#183380 = CARTESIAN_POINT ( 'NONE',  ( 6.144970055084349347, -0.2864424343173576082, -1.940704187532462432 ) ) ;
#183379 =( GEOMETRIC_REPRESENTATION_CONTEXT ( 3 ) GLOBAL_UNCERTAINTY_ASSIGNED_CONTEXT ( ( #68058 ) ) GLOBAL_UNIT_ASSIGNED_CONTEXT ( ( #89298, #5862, #41624 ) ) REPRESENTATION_CONTEXT ( 'NONE', 'WORKASPACE' ) );
#183381 = CARTESIAN_POINT ( 'NONE',  ( 6.941411460516762943, 11.04213777067082702, -0.7216878364870267237 ) ) ;
#183382 = CARTESIAN_POINT ( 'NONE',  ( 0.3985414750882500523, 3.110725714686441989, 2.025316624788002340 ) ) ;
#183383 = CARTESIAN_POINT ( 'NONE',  ( 6.925078400183534377, -0.01048729610059369148, 2.244148362790527429 ) ) ;
#183384 = CARTESIAN_POINT ( 'NONE',  ( 4.030516805012513082, 7.924296382481737844, 0.000000000000000000 ) ) ;
#183385 = CARTESIAN_POINT ( 'NONE',  ( -4.340018570150318666, 6.156717313299049366, -1.443375672974066548 ) ) ;
#183386 = CARTESIAN_POINT ( 'NONE',  ( 4.158677964895734824, -0.6440432224011168882, -1.959637643944433849 ) ) ;
#183387 = CARTESIAN_POINT ( 'NONE',  ( -4.120788623549732854, 6.895004929861607401, -1.199719254218452047 ) ) ;
#183389 = EDGE_CURVE ( 'NONE', #203057, #60914, #177624, .T. ) ;
#183388 = CARTESIAN_POINT ( 'NONE',  ( -1.499999999999997780, 4.181250000682819490, 1.214306433183764966E-14 ) ) ;
#183390 = CARTESIAN_POINT ( 'NONE',  ( 1.364683531249986537, -0.3447916663252443836, -0.7879004041258309554 ) ) ;
#183391 = CARTESIAN_POINT ( 'NONE',  ( 6.344977084850584426, -1.580176071495458023, 1.000667393836668362 ) ) ;
#183392 = CARTESIAN_POINT ( 'NONE',  ( 4.482897354602959794, -1.733954122632981099, -0.03610910148283198728 ) ) ;
#183393 = CARTESIAN_POINT ( 'NONE',  ( 4.722041168748464912, 1.667336974042502584, 0.4991589302964939412 ) ) ;
#183394 = CARTESIAN_POINT ( 'NONE',  ( 5.196852952739813070, 4.957416621151553571, -0.7998128361456221525 ) ) ;
#183395 = CARTESIAN_POINT ( 'NONE',  ( 1.998001414424467104, -2.291734237260790952, 0.06083037064899367297 ) ) ;
#183396 = CARTESIAN_POINT ( 'NONE',  ( -1.364683531250010295, 4.092708333674751842, 0.7879004041258379498 ) ) ;
#183397 = CARTESIAN_POINT ( 'NONE',  ( 5.935123052105460317, -1.514893180500265002, -1.441204661170019108 ) ) ;
#183398 = CARTESIAN_POINT ( 'NONE',  ( 6.527294062531273866, -1.270327234845580078, -1.468905576289506909 ) ) ;
#183399 = EDGE_CURVE ( 'NONE', #5628, #26543, #119391, .T. ) ;
#183400 = CARTESIAN_POINT ( 'NONE',  ( -11.48243876534946040, 13.79999999999999893, -3.200000000000001510 ) ) ;
#183401 = CARTESIAN_POINT ( 'NONE',  ( 1.160779977835691312, 1.203355533934968635, 1.617816888933524710 ) ) ;
#183402 = CARTESIAN_POINT ( 'NONE',  ( -5.219525951136856357, 6.152163700156858539, -1.082531754730543971 ) ) ;
#183403 = CARTESIAN_POINT ( 'NONE',  ( 7.836497216431498103, 13.95913530938479497, -9.964358386139231527 ) ) ;
#183404 = CARTESIAN_POINT ( 'NONE',  ( -8.015895134177625891, 10.37496362800581018, 1.599625672291295375 ) ) ;
#183405 = CARTESIAN_POINT ( 'NONE',  ( 6.667912619822566000, 6.673652899414787676, 1.040834085586084257E-14 ) ) ;
#183406 = CARTESIAN_POINT ( 'NONE',  ( 3.475340844119987782, -1.870931441966826148, -0.9980012987173058070 ) ) ;
#183407 = CARTESIAN_POINT ( 'NONE',  ( -1.364683531250014514, -0.7197916663252461600, 0.7879004041258379498 ) ) ;
#183408 = CARTESIAN_POINT ( 'NONE',  ( 6.024025069106937913, -1.018266858664597763, -1.515143308444939274 ) ) ;
#183409 = ORIENTED_EDGE ( 'NONE', *, *, #182170, .T. ) ;
#183410 = CARTESIAN_POINT ( 'NONE',  ( -6.414942957921379474, 7.513130201443591005, -1.199719254218452047 ) ) ;
#183411 = B_SPLINE_CURVE_WITH_KNOTS ( 'NONE', 3,
 ( #101933, #167999, #147500, #66196, #85677, #151765, #3334, #119310 ),
 .UNSPECIFIED., .F., .F.,
 ( 4, 2, 2, 4 ),
 ( 0.000000000000000000, 0.003005455498261385902, 0.004508183247392079721, 0.006010910996522773539 ),
 .UNSPECIFIED. ) ;
#183412 = CARTESIAN_POINT ( 'NONE',  ( -0.006768871532359390167, 8.210909518262125673, -2.038649385027042626 ) ) ;
#183413 = CARTESIAN_POINT ( 'NONE',  ( 5.844973620822823790, 9.833236634353070826, 0.7216878364870317197 ) ) ;
#183414 = CARTESIAN_POINT ( 'NONE',  ( 1.642778471875000035, -0.3135416661887088785, -2.845375778867859751 ) ) ;
#183415 = CARTESIAN_POINT ( 'NONE',  ( -7.067878151425722955, 7.140279352951794500, 0.7998128361456341429 ) ) ;
#183416 = CARTESIAN_POINT ( 'NONE',  ( 3.252217677095782911, 0.9042450522839510230, -1.806111763424333105 ) ) ;
#183417 = CARTESIAN_POINT ( 'NONE',  ( 6.756857042228312515, -1.710155547305733492, 1.394389531264042414 ) ) ;
#183418 = CARTESIAN_POINT ( 'NONE',  ( -4.496464221587651799, 5.274905009054215554, 1.199719254218452935 ) ) ;
#183419 = CARTESIAN_POINT ( 'NONE',  ( 4.293699386915854177, -1.280875055806574236, -1.350249269484518955 ) ) ;
#183420 = CARTESIAN_POINT ( 'NONE',  ( 9.589694723567584234, 10.08239868711733855, -0.7998128361456281477 ) ) ;
#183421 = CARTESIAN_POINT ( 'NONE',  ( 2.911969131885072670, 6.619324097166378706, 0.000000000000000000 ) ) ;
#183422 = VERTEX_POINT ( 'NONE', #43386 ) ;
#183423 = CARTESIAN_POINT ( 'NONE',  ( -4.386226389220933441, 5.076017861301227008, -1.199719254218446718 ) ) ;
#183424 = PRESENTATION_LAYER_ASSIGNMENT (  '', '', ( #79679 ) ) ;
#183425 = CARTESIAN_POINT ( 'NONE',  ( -8.019811557683421910, 9.315200557840817908, 1.199719254218462483 ) ) ;
#183427 = CARTESIAN_POINT ( 'NONE',  ( -4.390790479118549250, 7.352160220884910835, 1.215098293768980930 ) ) ;
#183426 = CARTESIAN_POINT ( 'NONE',  ( -7.910256278930404505, 8.193330178365746619, -0.7998128361456362523 ) ) ;
#183428 = CARTESIAN_POINT ( 'NONE',  ( -1.364683531250000748, -0.7406249996585803075, 0.000000000000000000 ) ) ;
#183429 = CARTESIAN_POINT ( 'NONE',  ( 2.055574482508758738, 1.511248224151232167, -0.8496982089122394610 ) ) ;
#183430 = CARTESIAN_POINT ( 'NONE',  ( 1.024908375165583863, -1.101351337790077212, -1.347483777630980040 ) ) ;
#183432 = CARTESIAN_POINT ( 'NONE',  ( 8.432808358020029260, 8.940623960552603222, 0.7216878364870438212 ) ) ;
#183431 = CARTESIAN_POINT ( 'NONE',  ( 6.604155123031994812, -2.307348207032692944, 0.04906353339812623282 ) ) ;
#183433 = CARTESIAN_POINT ( 'NONE',  ( 4.309512724297349884, 6.121127159803966933, 1.599625672291261402 ) ) ;
#183434 = CARTESIAN_POINT ( 'NONE',  ( 0.8958617733694884677, -0.7443198534227279950, 1.921839338364476513 ) ) ;
#183435 = CARTESIAN_POINT ( 'NONE',  ( 0.4564073884281876214, 1.492024165150519055, 1.356095248386236074 ) ) ;
#183436 = CYLINDRICAL_SURFACE ( 'NONE', #13448, 0.07999999999999972411 ) ;
#183437 = CARTESIAN_POINT ( 'NONE',  ( -5.743814354044916470, 6.730146830254374990, -1.199719254218453823 ) ) ;
#183438 = CARTESIAN_POINT ( 'NONE',  ( 6.649288223980674317, -1.503899034092892162, -1.112267350887645945 ) ) ;
#183440 = CARTESIAN_POINT ( 'NONE',  ( -5.614485009834902840, 9.564333254867113610, 0.7216878364870267237 ) ) ;
#183439 = CARTESIAN_POINT ( 'NONE',  ( 4.482611839828003930, -1.244964735940889522, 1.451779576051547282 ) ) ;
#183441 = CARTESIAN_POINT ( 'NONE',  ( 6.639307388351803674, -1.973492857608965423, 0.9879489342229507143 ) ) ;
#183442 = CARTESIAN_POINT ( 'NONE',  ( 1.224999999999971001, 2.187500000682782275, -4.683753385137379155E-14 ) ) ;
#183443 = CARTESIAN_POINT ( 'NONE',  ( -7.390603132780795725, 8.755363422066633206, -1.082531754730549967 ) ) ;
#183444 = CARTESIAN_POINT ( 'NONE',  ( 4.760321331729593375, 5.686701320840210627, -1.082531754730548412 ) ) ;
#183445 = CARTESIAN_POINT ( 'NONE',  ( -4.462041952228954500, 6.299077925724123617, -1.443375672974066548 ) ) ;
#183446 = CARTESIAN_POINT ( 'NONE',  ( 6.445950376775947177, -1.384621037358444662, -1.606076714075025613 ) ) ;
#183447 = ORIENTED_EDGE ( 'NONE', *, *, #47479, .F. ) ;
#183448 = CARTESIAN_POINT ( 'NONE',  ( 3.171242727813221585, -2.131442559959194849, -0.8847066026466602340 ) ) ;
#183449 = CARTESIAN_POINT ( 'NONE',  ( 5.283633159863808437, -1.863482887291990409, 0.6137318589548645953 ) ) ;
#183450 = CARTESIAN_POINT ( 'NONE',  ( 0.4792544977638459880, -0.1021076105021078151, 1.959249876678282209 ) ) ;
#183451 = CARTESIAN_POINT ( 'NONE',  ( -5.204170427930421283E-15, -1.000000000000000888, -12.26547674076639716 ) ) ;
#183452 = CARTESIAN_POINT ( 'NONE',  ( -0.5000000000000299760, 3.299999999999955858, -0.5000000000000403011 ) ) ;
#183453 = CARTESIAN_POINT ( 'NONE',  ( -0.04742653102243841318, -1.377616979729365809, 1.608019283586498371 ) ) ;
#183454 = CARTESIAN_POINT ( 'NONE',  ( -3.924195396151603177, 6.665646164563756138, 1.199719254218464037 ) ) ;
#183455 = DIRECTION ( 'NONE',  ( 1.000000000000000000, -0.000000000000000000, -0.000000000000000000 ) ) ;
#183456 = CARTESIAN_POINT ( 'NONE',  ( 3.696278757040452057, 0.9809249153905131857, -1.936940462344426628 ) ) ;
#183457 = CARTESIAN_POINT ( 'NONE',  ( -0.001670575542712476836, 2.503868101192739282, 2.003409546593375890 ) ) ;
#183458 = CARTESIAN_POINT ( 'NONE',  ( 1.283610819548046011, 0.1505422781087061845, -2.115291873224629082 ) ) ;
#183459 = CARTESIAN_POINT ( 'NONE',  ( -0.7500000000000006661, 2.389583334016155636, -1.299038105676652011 ) ) ;
#183460 = CARTESIAN_POINT ( 'NONE',  ( 9.297140650669039275, 11.86975006391249643, 1.599625672291281386 ) ) ;
#183461 = CARTESIAN_POINT ( 'NONE',  ( -1.833030277982322875, 2.526412122984485364, -2.500000000000015987 ) ) ;
#183462 = CARTESIAN_POINT ( 'NONE',  ( 6.567098404289990476, 6.791591158854626720, -0.3517435911668670423 ) ) ;
#183463 = CARTESIAN_POINT ( 'NONE',  ( 2.372404410299948196, -1.270453386316850342, 1.622462496149602140 ) ) ;
#183465 = CARTESIAN_POINT ( 'NONE',  ( 11.84668730067608600, 13.40000000000000036, -1.400000000000001910 ) ) ;
#183464 = CARTESIAN_POINT ( 'NONE',  ( -9.352427035328430449, 9.805586384171650849, 1.040834085586084257E-14 ) ) ;
#183466 = CARTESIAN_POINT ( 'NONE',  ( 0.6823417656249899377, 2.592708333674753618, 1.181850606188767472 ) ) ;
#183467 = CARTESIAN_POINT ( 'NONE',  ( 0.07755575628183573877, 5.720052600789671260, -2.782970829007725744 ) ) ;
#183468 = CARTESIAN_POINT ( 'NONE',  ( 10.50000000000000178, 10.89999999999998259, 3.599999999999999201 ) ) ;
#183469 = ORIENTED_EDGE ( 'NONE', *, *, #106403, .F. ) ;
#183470 = CARTESIAN_POINT ( 'NONE',  ( 4.775979982822478931, 1.890921987351320777, -0.2842533987747336566 ) ) ;
#183471 = CARTESIAN_POINT ( 'NONE',  ( -11.91826848330638455, 11.00729645956977798, 1.400000080589927753 ) ) ;
#183472 = CARTESIAN_POINT ( 'NONE',  ( 1.933286576697599513, 0.2207578219815004572, 2.251582216785783075 ) ) ;
#183473 = CARTESIAN_POINT ( 'NONE',  ( -2.927671105547157371, 5.503034492191895666, 1.199719254218462483 ) ) ;
#183474 = CARTESIAN_POINT ( 'NONE',  ( 1.494102799026775008, -0.9672467274632718937, 1.531528279607297094 ) ) ;
#183475 = CARTESIAN_POINT ( 'NONE',  ( 1.006889752881213296, -0.04349654304135543159, 1.915380135637449799 ) ) ;
#183476 = CARTESIAN_POINT ( 'NONE',  ( 2.348173244826061268, -0.8873571809006628452, 1.870714752860686447 ) ) ;
#183477 = CARTESIAN_POINT ( 'NONE',  ( 0.6823417656249899377, 1.655208333674752730, 1.181850606188755259 ) ) ;
#183478 = CARTESIAN_POINT ( 'NONE',  ( 0.1101414390347132816, -0.8398613168552993002, -1.781629259513841657 ) ) ;
#183479 = CARTESIAN_POINT ( 'NONE',  ( 5.654890666209754002, -1.517393486936137403, 1.186882646050735346 ) ) ;
#183481 = CARTESIAN_POINT ( 'NONE',  ( 5.726091835933811325, 7.283405380927965744, -1.209259067671350163 ) ) ;
#183480 = CARTESIAN_POINT ( 'NONE',  ( 0.4171991508139940574, 1.586773611656131289, -1.675818712001175381 ) ) ;
#183482 = CARTESIAN_POINT ( 'NONE',  ( 1.364683531249986537, 1.155208333674754728, -0.7879004041258239610 ) ) ;
#183483 = CARTESIAN_POINT ( 'NONE',  ( 4.721170020219593866, -1.840989660556498597, -0.9304453918272929114 ) ) ;
#183484 = CARTESIAN_POINT ( 'NONE',  ( -6.925517538482230506, 6.974191971184389160, 0.7998128361456341429 ) ) ;
#183485 = CARTESIAN_POINT ( 'NONE',  ( 8.263858322729371153, 9.599921783727809910, -1.199719254218446718 ) ) ;
#183486 = DIRECTION ( 'NONE',  ( -5.176899690512889973E-31, 0.6004703560067666812, -0.7996470168500017239 ) ) ;
#183487 = CARTESIAN_POINT ( 'NONE',  ( 5.494078562035752178, 7.432844293840273231, -1.599625672291262513 ) ) ;
#183489 = CARTESIAN_POINT ( 'NONE',  ( 1.499999999999989120, 3.525000000000021227, 1.214306433183764966E-14 ) ) ;
#183488 = CARTESIAN_POINT ( 'NONE',  ( 5.385806172021708527, 1.412131043145675280, 1.562536384088798691 ) ) ;
#183490 = CARTESIAN_POINT ( 'NONE',  ( 0.5905675304203241716, 1.115885162268255293, -1.862360684160404123 ) ) ;
#183491 = CARTESIAN_POINT ( 'NONE',  ( -1.364683531250000748, 1.071875000341421247, 0.000000000000000000 ) ) ;
#183492 = CARTESIAN_POINT ( 'NONE',  ( 5.413408226029433834, -0.3230527293765028118, 2.137217106551466905 ) ) ;
#183493 = CARTESIAN_POINT ( 'NONE',  ( 4.863928438619278261, 0.6316314618598058983, -1.918449035972718431 ) ) ;
#183494 = LINE ( 'NONE', #146773, #180786 ) ;
#183495 = EDGE_CURVE ( 'NONE', #183546, #113976, #174236, .T. ) ;
#183498 = CARTESIAN_POINT ( 'NONE',  ( 6.643132081016125845, 6.852668304048034287, 0.7216878364870317197 ) ) ;
#183497 = CARTESIAN_POINT ( 'NONE',  ( -3.285556943749998737, -1.830208332855373987, 1.896917185911908499 ) ) ;
#183496 = CARTESIAN_POINT ( 'NONE',  ( 6.502017186205484300, 9.743381262951846367, -1.199719254218452047 ) ) ;
#183499 =( BOUNDED_SURFACE ( )  B_SPLINE_SURFACE ( 3, 2, ( 
 ( #40684, #138182, #153353 ),
 ( #69934, #168532, #120931 ),
 ( #204192, #202058, #53718 ),
 ( #41759, #139247, #119851 ) ),
 .UNSPECIFIED., .F., .F., .T. ) 
 B_SPLINE_SURFACE_WITH_KNOTS ( ( 4, 4 ),
 ( 3, 3 ),
 ( 0.005239860189960142932, 0.008266248133684681726 ),
 ( 0.000000000000000000, 1.000000000000000000 ),
 .UNSPECIFIED. ) 
 GEOMETRIC_REPRESENTATION_ITEM ( )  RATIONAL_B_SPLINE_SURFACE ( (
 ( 1.000000000000000000, 0.7187737999613679207, 1.000000000000000000),
 ( 1.000000000000000000, 0.7186585579881036301, 1.000000000000000000),
 ( 1.000000000000000000, 0.7185467277397536989, 1.000000000000000000),
 ( 1.000000000000000000, 0.7184380228464066764, 1.000000000000000000) ) ) 
 REPRESENTATION_ITEM ( '' )  SURFACE ( )  );
#183500 = CARTESIAN_POINT ( 'NONE',  ( -5.119085517611572378, 8.129960982925583224, 1.199719254218452935 ) ) ;
#183501 = CARTESIAN_POINT ( 'NONE',  ( 3.907435596788138010, -1.928258004016227378, 0.5899861904685861358 ) ) ;
#183502 = CARTESIAN_POINT ( 'NONE',  ( -8.585337585951595685, 11.03931315507545108, -1.599625672291263179 ) ) ;
#183504 =( LENGTH_UNIT ( ) NAMED_UNIT ( * ) SI_UNIT ( .MILLI., .METRE. ) );
#183503 = CARTESIAN_POINT ( 'NONE',  ( -4.451154503988200339, 4.087435097607984957, 1.214306433183764966E-14 ) ) ;
#183506 = CARTESIAN_POINT ( 'NONE',  ( -11.86687215968023601, 12.49057787694210653, -1.056395335932043045 ) ) ;
#183505 = CARTESIAN_POINT ( 'NONE',  ( 4.592742373648754040, -0.4705147408641910944, -2.109722102427157964 ) ) ;
#183507 = CARTESIAN_POINT ( 'NONE',  ( -11.12459591588106811, 5.815451121142331203, -4.514238076378977560 ) ) ;
#183509 = CARTESIAN_POINT ( 'NONE',  ( 6.046499952770106212, -1.423952032562772807, 1.427948417171531759 ) ) ;
#183508 = CARTESIAN_POINT ( 'NONE',  ( -6.344852701071109102, 10.34615255131755163, 0.000000000000000000 ) ) ;
#183510 = CARTESIAN_POINT ( 'NONE',  ( -1.001543065824772872E-14, 4.962500000000019007, 1.732050807568877637 ) ) ;
#183511 = CARTESIAN_POINT ( 'NONE',  ( 0.4336905314940731060, 0.8911838752851186651, -1.476660275499335873 ) ) ;
#183512 = CARTESIAN_POINT ( 'NONE',  ( 5.143339171537801846, 7.093924681584509173, 1.599625672291269396 ) ) ;
#183514 = CARTESIAN_POINT ( 'NONE',  ( 6.373214726875630731, 9.593111727067046957, 1.199719254218452047 ) ) ;
#183513 = CARTESIAN_POINT ( 'NONE',  ( 7.131225611108085616, 10.30321839872603462, 1.082531754730558626 ) ) ;
#183515 = STYLED_ITEM ( 'NONE', ( #165200 ), #169296 ) ;
#183516 = CARTESIAN_POINT ( 'NONE',  ( -11.32461466721508181, 7.705894113993029038, 3.976347498773577183 ) ) ;
#183517 = CARTESIAN_POINT ( 'NONE',  ( 5.466025653875023593, 0.9211120992074215419, 1.627924866423650530 ) ) ;
#183518 = CARTESIAN_POINT ( 'NONE',  ( 6.451439527836500432, -1.796305863176387518, 0.9092463195026576628 ) ) ;
#183519 = CARTESIAN_POINT ( 'NONE',  ( 4.487385655998888723, 4.337630808194552934, 0.7216878364870317197 ) ) ;
#183520 = CARTESIAN_POINT ( 'NONE',  ( -6.631346530415505036, 7.869564052640446228, 1.082531754730549078 ) ) ;
#183521 = ORIENTED_EDGE ( 'NONE', *, *, #80739, .T. ) ;
#183522 = CARTESIAN_POINT ( 'NONE',  ( 10.01911233037457905, 11.75168114260095109, 1.082531754730548412 ) ) ;
#183524 = CARTESIAN_POINT ( 'NONE',  ( 1.335564786618839817, 0.5826355126458090394, -1.930425043884367087 ) ) ;
#183523 = CARTESIAN_POINT ( 'NONE',  ( 2.596466591541984226, -1.087938976695131066, 1.819974527870950265 ) ) ;
#183525 = CARTESIAN_POINT ( 'NONE',  ( 1.283166710957379220, 0.1313358247177751625, -1.806845861898898953 ) ) ;
#183526 = CARTESIAN_POINT ( 'NONE',  ( 7.526711554241970248, 8.810193563817646734, -1.199719254218452047 ) ) ;
#183527 = CARTESIAN_POINT ( 'NONE',  ( 6.684453901184132185, -2.118919246787358102, -0.4271090584619871566 ) ) ;
#183528 = COLOUR_RGB ( '', 0.40784314, 0.44705882, 0.49803922) ;
#183529 = ADVANCED_FACE ( 'NONE', ( #127917 ), #21524, .T. ) ;
#183530 = CARTESIAN_POINT ( 'NONE',  ( 7.100719765255169236, 9.307259030929609267, -1.599625672291262513 ) ) ;
#183532 = CARTESIAN_POINT ( 'NONE',  ( 0.7432033230480495911, 0.3705163548812146490, -1.879356322977752347 ) ) ;
#183531 = CARTESIAN_POINT ( 'NONE',  ( -4.367698041896780126, 8.247398148854895084, 0.7998128361456481317 ) ) ;
#183533 = CARTESIAN_POINT ( 'NONE',  ( 1.905110947044305725, 8.996536036952683446, 0.7750000000000004663 ) ) ;
#183534 =( NAMED_UNIT ( * ) SI_UNIT ( $, .STERADIAN. ) SOLID_ANGLE_UNIT ( ) );
#183535 = CARTESIAN_POINT ( 'NONE',  ( 6.277061933002785032, 7.385955679000473673, 1.082531754730558626 ) ) ;
#183536 = CARTESIAN_POINT ( 'NONE',  ( 5.484430959185961463, 6.043327615839654499, 0.8208683321978844649 ) ) ;
#183537 = CARTESIAN_POINT ( 'NONE',  ( 3.226477370372302644, 5.747678784534228313, 1.082531754730546636 ) ) ;
#183538 = CARTESIAN_POINT ( 'NONE',  ( -3.002240950422295995, 5.590032644546251817, -1.199719254218452935 ) ) ;
#183539 = CARTESIAN_POINT ( 'NONE',  ( 4.241217004700631676, -1.882188537963986219, 1.063020064016991117 ) ) ;
#183540 = CARTESIAN_POINT ( 'NONE',  ( -7.132998214565509087, 7.494455136514109661, 0.7216878364870317197 ) ) ;
#183541 = CARTESIAN_POINT ( 'NONE',  ( 7.038091139269835317, 7.383730215335837954, 0.000000000000000000 ) ) ;
#183542 = CARTESIAN_POINT ( 'NONE',  ( 1.494549364340029163, -1.129948290531690658, 1.794289463044356436 ) ) ;
#183543 = CARTESIAN_POINT ( 'NONE',  ( 6.743450862738472829, 15.00041888085534758, 9.536679667281278583 ) ) ;
#183544 = CARTESIAN_POINT ( 'NONE',  ( 1.651575284419577461, 0.5759676520707255332, -1.885319811257283096 ) ) ;
#183545 = CARTESIAN_POINT ( 'NONE',  ( 5.115449499555525747, 1.566912803841558732, 1.096118974231160781 ) ) ;
#183546 = VERTEX_POINT ( 'NONE', #50825 ) ;
#183547 = CARTESIAN_POINT ( 'NONE',  ( 9.611175950047698535, -6.604184692106344734, -0.3106162252735243934 ) ) ;
#183548 = CARTESIAN_POINT ( 'NONE',  ( 6.426221551499647688, 1.011104814135417751, 1.690039303870519705 ) ) ;
#183549 = CARTESIAN_POINT ( 'NONE',  ( 1.429522090333503304, 0.9575595492820774268, -1.689375863068052430 ) ) ;
#183550 = VERTEX_POINT ( 'NONE', #212244 ) ;
#183551 = CARTESIAN_POINT ( 'NONE',  ( -5.646044625448194410, 5.551749915969804938, 0.000000000000000000 ) ) ;
#183553 = CARTESIAN_POINT ( 'NONE',  ( 2.535011536075336913, 5.133042487381361596, -2.419999999999995044 ) ) ;
#183552 = CARTESIAN_POINT ( 'NONE',  ( -6.400857919427531684, 9.521399101757175742, 1.082531754730549967 ) ) ;
#183554 = CARTESIAN_POINT ( 'NONE',  ( 6.174848896020108668, 9.291408581077091000, 1.199719254218460707 ) ) ;
#183556 = CARTESIAN_POINT ( 'NONE',  ( 4.651856102820254968, 7.480896982382013505, -1.082531754730548412 ) ) ;
#183555 = CARTESIAN_POINT ( 'NONE',  ( 7.481401836642521452, 7.622723652371411696, 1.040834085586084257E-14 ) ) ;
#183558 = EDGE_LOOP ( 'NONE', ( #65198, #208909, #157106, #208635 ) ) ;
#183557 = CARTESIAN_POINT ( 'NONE',  ( 6.076807558263135789, -1.348954070496380941, 1.355674883165632227 ) ) ;
#183559 = CARTESIAN_POINT ( 'NONE',  ( 3.721466898765386500, -0.1629207441977159609, 2.200919931280575170 ) ) ;
#183560 = CARTESIAN_POINT ( 'NONE',  ( 1.694636308673210801, -2.196210861363355082, -0.2157497520150277182 ) ) ;
#183561 = EDGE_CURVE ( 'NONE', #7171, #205917, #22028, .T. ) ;
#183562 = DIRECTION ( 'NONE',  ( 0.000000000000000000, 1.000000000000000000, 0.000000000000000000 ) ) ;
#183563 = CARTESIAN_POINT ( 'NONE',  ( 0.2934254677693093338, 1.784247535656303230, -0.6883866973072181317 ) ) ;
#183564 = CARTESIAN_POINT ( 'NONE',  ( -10.56514123924917392, 13.75891954478806234, -3.404988257269842222 ) ) ;
#183565 = CARTESIAN_POINT ( 'NONE',  ( -6.447678837262236229, -6.532648880268781433, -6.949550370341204264 ) ) ;
#183566 = CARTESIAN_POINT ( 'NONE',  ( 3.279797552538410876, -1.996039814156633785, 0.5495672325947635883 ) ) ;
#183567 = CARTESIAN_POINT ( 'NONE',  ( -6.586563698140583512, 6.578745824119123675, 1.040834085586084257E-14 ) ) ;
#183568 = CARTESIAN_POINT ( 'NONE',  ( -5.050372967203840879, 7.883769262350217133, 1.105620360010154402 ) ) ;
#183570 = CARTESIAN_POINT ( 'NONE',  ( 1.622176833581047806, -1.201014165160016356, -1.797165035535647659 ) ) ;
#183569 = CARTESIAN_POINT ( 'NONE',  ( -5.088387723830502196, 4.830873854090670605, -0.7998128361456221525 ) ) ;
#183571 = CARTESIAN_POINT ( 'NONE',  ( 3.896163805485418852, -0.6886730243073329039, -2.080591098665984795 ) ) ;
#183572 = MECHANICAL_DESIGN_GEOMETRIC_PRESENTATION_REPRESENTATION (  '', ( #17652 ), #190523 ) ;
#183573 = CARTESIAN_POINT ( 'NONE',  ( -1.288108131580338211, -0.9841229182759280159, 3.227445187970915619 ) ) ;
#183574 = CARTESIAN_POINT ( 'NONE',  ( -11.84668730067608600, 12.69999999999998153, 1.399999999999998579 ) ) ;
#183575 = CARTESIAN_POINT ( 'NONE',  ( -0.6823417656250039265, 13.88020833367473195, -1.181850606188755259 ) ) ;
#183576 = CARTESIAN_POINT ( 'NONE',  ( -4.145761110728687804, 8.058748072483927771, -0.7998128361456481317 ) ) ;
#183577 = CARTESIAN_POINT ( 'NONE',  ( 6.240799290569317925, 1.728800370330787928, -0.1372766232172056844 ) ) ;
#183578 = CARTESIAN_POINT ( 'NONE',  ( -7.998947442382709383, 12.27592974951444660, 0.7216878364870478180 ) ) ;
#183579 = CARTESIAN_POINT ( 'NONE',  ( 3.836834752522141567, -1.993853832596056197, -0.5568897355931883286 ) ) ;
#183580 = CARTESIAN_POINT ( 'NONE',  ( 4.657876698301413043, 1.220176935102987636, 1.730081886799080593 ) ) ;
#183581 = CARTESIAN_POINT ( 'NONE',  ( 5.503720292143644777, 8.508425209887878538, 1.199719254218462483 ) ) ;
#183582 = CARTESIAN_POINT ( 'NONE',  ( 0.6823417656249899377, 4.676041667008086655, -1.181850606188754593 ) ) ;
#183583 = CARTESIAN_POINT ( 'NONE',  ( 3.291813281336749331, -1.319317765291039946, -1.462433841519056532 ) ) ;
#183584 = CARTESIAN_POINT ( 'NONE',  ( 0.3867804997886997720, -1.801505969789623629, -0.6421655129100201087 ) ) ;
#183585 = CARTESIAN_POINT ( 'NONE',  ( 5.314510991623739855, 2.116275055252315074, 0.8812819573641057502 ) ) ;
#183586 = CARTESIAN_POINT ( 'NONE',  ( 2.789462663364688844, 1.291185895303394116, 1.290987730777813702 ) ) ;
#183587 = CARTESIAN_POINT ( 'NONE',  ( 3.393283585170187688, 7.180857625999046867, 0.7998128361456271485 ) ) ;
#183589 = EDGE_CURVE ( 'NONE', #126491, #212596, #18304, .T. ) ;
#183588 = CARTESIAN_POINT ( 'NONE',  ( 5.382223794500827552, 7.302347065049529462, -1.443375672974051449 ) ) ;
#183590 = CARTESIAN_POINT ( 'NONE',  ( -6.287230548435221777, 8.358188277972981695, -1.599625672291263179 ) ) ;
#183591 = ORIENTED_EDGE ( 'NONE', *, *, #194941, .T. ) ;
#183592 = ORIENTED_EDGE ( 'NONE', *, *, #125545, .F. ) ;
#183593 = CARTESIAN_POINT ( 'NONE',  ( 3.779544948098710666, 0.2423517821111692006, -1.998478243804775900 ) ) ;
#183594 = CARTESIAN_POINT ( 'NONE',  ( 4.575024454672827368, 1.791946274209740952, 0.7988320279663924106 ) ) ;
#183595 = CARTESIAN_POINT ( 'NONE',  ( -7.263417608619167076, 9.497073181520933716, -1.599625672291263179 ) ) ;
#183596 = CARTESIAN_POINT ( 'NONE',  ( -6.762819695118240659, 6.784377820593065600, 0.7998128361456341429 ) ) ;
#183597 = DIRECTION ( 'NONE',  ( -0.6507913734559641616, -0.7592566023653004592, 0.000000000000000000 ) ) ;
#183599 = CARTESIAN_POINT ( 'NONE',  ( 5.172599881030584434, -1.667270648082047835, -0.5941068299562983768 ) ) ;
#183598 = CARTESIAN_POINT ( 'NONE',  ( 0.6793770918060678676, 1.407085465964125204, 1.546551842177671166 ) ) ;
#183600 = DIRECTION ( 'NONE',  ( -0.000000000000000000, 1.000000000000000000, 0.000000000000000000 ) ) ;
#183601 = CARTESIAN_POINT ( 'NONE',  ( 1.904481915951491189, 1.622449043516610123, -1.473309109067892697 ) ) ;
#183602 = CARTESIAN_POINT ( 'NONE',  ( 6.685563754570789996, -0.7372397036040450047, 1.575249959525576005 ) ) ;
#183603 = CARTESIAN_POINT ( 'NONE',  ( 7.884230021546724920, 9.157022099014721306, 1.199719254218462483 ) ) ;
#183604 = CARTESIAN_POINT ( 'NONE',  ( 0.2335667940002320309, 7.629137130509054288, -2.753349444758381281 ) ) ;
#183605 = CARTESIAN_POINT ( 'NONE',  ( 0.9962403866136140262, -0.4152203131645367806, -1.674012925115143213 ) ) ;
#183606 = CARTESIAN_POINT ( 'NONE',  ( 0.9666848095895408388, 1.880238891319021111, 1.321614243928259880 ) ) ;
#183608 = EDGE_CURVE ( 'NONE', #101488, #142386, #65969, .T. ) ;
#183607 = CARTESIAN_POINT ( 'NONE',  ( 0.5565083568685527116, -1.583368386835169783, 1.515454571103365344 ) ) ;
#183609 = CARTESIAN_POINT ( 'NONE',  ( 6.626334403847231158, 0.2915952204957816263, -1.708955668912811587 ) ) ;
#183610 = CARTESIAN_POINT ( 'NONE',  ( 2.543839704335303153, -1.636039663378138886, -1.481301067789652537 ) ) ;
#183611 = CARTESIAN_POINT ( 'NONE',  ( 6.473846665049121540, -0.8576149079453172508, 1.823233050095712349 ) ) ;
#183612 = CARTESIAN_POINT ( 'NONE',  ( 0.2862954470153349362, -1.335216113735339105, -1.712835229902017531 ) ) ;
#183613 = CARTESIAN_POINT ( 'NONE',  ( -1.432341765624997709, 5.860937500170720682, 1.214306433183764966E-14 ) ) ;
#183614 = CARTESIAN_POINT ( 'NONE',  ( 2.360703550434081421, -2.027734997378250359, -0.6095688489828243739 ) ) ;
#183615 = CARTESIAN_POINT ( 'NONE',  ( 1.873515663034551304, 3.299988112486747394, 0.3999999999999681033 ) ) ;
#183616 = CARTESIAN_POINT ( 'NONE',  ( 5.596683124612600757, -0.4680951147424931569, -1.868546797846575513 ) ) ;
#183617 = ORIENTED_EDGE ( 'NONE', *, *, #49896, .F. ) ;
#183619 = CARTESIAN_POINT ( 'NONE',  ( -1.364683531250014514, -0.9489583329919112353, -0.7879004041258359514 ) ) ;
#183618 = CARTESIAN_POINT ( 'NONE',  ( 1.980407754855911140, -2.249062817636026779, -0.4427264618648701910 ) ) ;
#183620 = CARTESIAN_POINT ( 'NONE',  ( 4.467575310902914154, 5.170924936596891008, 1.199719254218464037 ) ) ;
#183621 = CARTESIAN_POINT ( 'NONE',  ( 4.710568305744190276, 7.583081225755162968, 1.199719254218462483 ) ) ;
#183622 = CARTESIAN_POINT ( 'NONE',  ( 4.723389051577030706, 1.932298245749045629, 1.095468883668549553 ) ) ;
#183623 = CARTESIAN_POINT ( 'NONE',  ( -8.514157279702036618, 9.035531035848267223, -0.7216878364870278340 ) ) ;
#183624 = CARTESIAN_POINT ( 'NONE',  ( 5.511726693494604312, 6.000014001146780629, -0.7850539801177413013 ) ) ;
#183625 = CARTESIAN_POINT ( 'NONE',  ( 6.317736394288147039, 6.473040002865377396, 0.7216878364870317197 ) ) ;
#183626 = CARTESIAN_POINT ( 'NONE',  ( -9.151390499099978371, 9.778969791812544443, 0.7216878364870438212 ) ) ;
#183627 = CIRCLE ( 'NONE', #41888, 12.00000000000000178 ) ;
#183628 = CARTESIAN_POINT ( 'NONE',  ( 4.570507181582611267, 8.346359121906111511, 0.000000000000000000 ) ) ;
#183629 = ORIENTED_EDGE ( 'NONE', *, *, #46704, .F. ) ;
#183630 = CARTESIAN_POINT ( 'NONE',  ( 3.270157880292836605, 1.821742160604752137, -0.8647241845514613834 ) ) ;
#183632 = CARTESIAN_POINT ( 'NONE',  ( 1.498963261266316183, 0.3983865470186908064, 2.023570823014529729 ) ) ;
#183631 = CARTESIAN_POINT ( 'NONE',  ( 6.751070424600909448, 9.963667031088037973, -1.199719254218441611 ) ) ;
#183633 = CARTESIAN_POINT ( 'NONE',  ( 4.789477563416786765, 4.879958555012922083, 0.4526585511122512284 ) ) ;
#183634 = CARTESIAN_POINT ( 'NONE',  ( 5.194182247366868843, 8.113610817686430110, 1.082531754730548412 ) ) ;
#183636 = EDGE_CURVE ( 'NONE', #51191, #183133, #108562, .T. ) ;
#183635 =( LENGTH_UNIT ( ) NAMED_UNIT ( * ) SI_UNIT ( .MILLI., .METRE. ) );
#183637 = CARTESIAN_POINT ( 'NONE',  ( -1.201851678989727383E-14, 3.071875000341420137, 1.575800808251672791 ) ) ;
#183638 = CARTESIAN_POINT ( 'NONE',  ( 4.330150130892728377, 2.148942519667027984, 0.4286813238914553570 ) ) ;
#183639 = CARTESIAN_POINT ( 'NONE',  ( 0.8443752267504719411, 0.3905955241953715795, -1.978051186352240309 ) ) ;
#183640 = CARTESIAN_POINT ( 'NONE',  ( 1.241482983173985533, 1.839155304979672501, 0.08999620058360720265 ) ) ;
#183641 = CARTESIAN_POINT ( 'NONE',  ( 4.757543194620796889, 2.267657608012829673, -0.3350592807548398722 ) ) ;
#183642 = CARTESIAN_POINT ( 'NONE',  ( 3.029072736150268952, -1.236975958831527445, -1.363863411116640334 ) ) ;
#183643 = EDGE_CURVE ( 'NONE', #143658, #187130, #163866, .T. ) ;
#183644 = CARTESIAN_POINT ( 'NONE',  ( 8.934986926605834157, 10.38290515491702770, -1.199719254218446718 ) ) ;
#183645 = SURFACE_SIDE_STYLE ('',( #149017 ) ) ;
#183646 = CARTESIAN_POINT ( 'NONE',  ( 4.664971680594516279, -1.631047870213175432, -0.8201845326444437978 ) ) ;
#183647 = CARTESIAN_POINT ( 'NONE',  ( 5.397111353752316987, -0.9091427841607623295, -1.799923777076550824 ) ) ;
#183648 = CARTESIAN_POINT ( 'NONE',  ( -7.883176251342026042, 11.28445716228600126, -1.199719254218446718 ) ) ;
#183650 = CARTESIAN_POINT ( 'NONE',  ( -7.767895665986912057, 8.027242796598338614, -0.7998128361456362523 ) ) ;
#183649 = CARTESIAN_POINT ( 'NONE',  ( 4.961948105735218384, 2.238643107264228327, -0.3270478844536877649 ) ) ;
#183651 = CARTESIAN_POINT ( 'NONE',  ( 6.598663424749101836, -0.5579900645847408747, -2.030628608299019700 ) ) ;
#183652 = CARTESIAN_POINT ( 'NONE',  ( 3.701679681979888503, -1.565833156357125278, -1.354537944502069102 ) ) ;
#183653 = CARTESIAN_POINT ( 'NONE',  ( 8.920375002787457319, 12.49452237230570084, 1.199719254218450271 ) ) ;
#183654 = CARTESIAN_POINT ( 'NONE',  ( 0.6801582343749900117, 2.005208333674748822, 1.178068619123818994 ) ) ;
#183655 = APPLICATION_PROTOCOL_DEFINITION ( 'draft international standard', 'automotive_design', 1998, #90556 ) ;
#183657 = CARTESIAN_POINT ( 'NONE',  ( 1.840333348128117885, 1.905464876828693921, 0.2831333259317326823 ) ) ;
#183656 = CARTESIAN_POINT ( 'NONE',  ( -8.015895134177625891, 10.37496362800581018, 1.599625672291295375 ) ) ;
#183658 = UNCERTAINTY_MEASURE_WITH_UNIT (LENGTH_MEASURE( 1.000000000000000082E-05 ), #205447, 'distance_accuracy_value', 'NONE');
#183659 = CARTESIAN_POINT ( 'NONE',  ( -4.625266680917477835, 5.425174544939014964, -1.199719254218453823 ) ) ;
#183660 = CARTESIAN_POINT ( 'NONE',  ( 6.754754220498722539, -0.5220956727660872598, -1.898933868174660589 ) ) ;
#183661 = CARTESIAN_POINT ( 'NONE',  ( 4.217995187182920880, 6.974725914138481642, 1.082531754730549078 ) ) ;
#183662 = CARTESIAN_POINT ( 'NONE',  ( 5.892675752748299800, 5.976886221469982274, -0.004604801460011270775 ) ) ;
#183663 = CARTESIAN_POINT ( 'NONE',  ( -3.684065054611367351, 5.321161868511784299, -1.599625672291256295 ) ) ;
#183665 = CARTESIAN_POINT ( 'NONE',  ( 1.688022500292500228, 2.124017718264622268, -0.6504838024826449239 ) ) ;
#183664 = CARTESIAN_POINT ( 'NONE',  ( 1.213308285724056690, 1.730450836393576886, -1.225479750871574458 ) ) ;
#183666 = CARTESIAN_POINT ( 'NONE',  ( 3.047987177024631844, 0.7594498649067694673, -1.964434322149722245 ) ) ;
#183668 = CARTESIAN_POINT ( 'NONE',  ( -6.261886844665283114, 8.398896966899865646, 1.599625672291269396 ) ) ;
#183667 = VECTOR ( 'NONE', #159836, 1000.000000000000000 ) ;
#183669 = CARTESIAN_POINT ( 'NONE',  ( 8.125414133291656071, 8.374071331795406081, -0.7998128361456291469 ) ) ;
#183670 = CARTESIAN_POINT ( 'NONE',  ( 0.3439184179485414439, -0.8825062887024995861, 1.638522830676287789 ) ) ;
#183671 = CARTESIAN_POINT ( 'NONE',  ( 7.287671262545424966, 8.461036880179857889, -1.199719254218451159 ) ) ;
#183672 = CARTESIAN_POINT ( 'NONE',  ( -4.328009424535094851, 7.229878788426305825, -0.9977569098220413490 ) ) ;
#183673 = CARTESIAN_POINT ( 'NONE',  ( 3.323720213644492993, 7.029424015893889433, 1.040834085586084257E-14 ) ) ;
#183674 = CARTESIAN_POINT ( 'NONE',  ( -5.641601317062247212, 7.675230518029648508, -1.443375672974066548 ) ) ;
#183675 = CARTESIAN_POINT ( 'NONE',  ( -8.188761592974051595, 9.616271948966963024, -1.082531754730543971 ) ) ;
#183676 = CARTESIAN_POINT ( 'NONE',  ( 1.547299434221154124, 0.2130619955753136618, 2.109896976817266179 ) ) ;
#183677 = CARTESIAN_POINT ( 'NONE',  ( -7.286581212701773502, 7.465709267765667789, 0.7998128361456341429 ) ) ;
#183679 = CARTESIAN_POINT ( 'NONE',  ( 4.299235682465595509, -1.708000122724560477, 0.9650500775852040025 ) ) ;
#183678 = CARTESIAN_POINT ( 'NONE',  ( -3.555477883677943599E-14, 0.5624999999999785727, 1.414508159514563435 ) ) ;
#183680 = CARTESIAN_POINT ( 'NONE',  ( 3.098656953246520906, -0.6260995091542166380, -2.069055637940686143 ) ) ;
#183681 = CARTESIAN_POINT ( 'NONE',  ( 1.698526806778306586, 1.531337151408303621, 1.022036240780115346 ) ) ;
#183682 = CARTESIAN_POINT ( 'NONE',  ( -4.356251871828045630, 7.199010410547511007, -1.027643995846918790 ) ) ;
#183683 = CARTESIAN_POINT ( 'NONE',  ( 0.07755575628181146652, 7.629137130509076492, -2.788902932953696290 ) ) ;
#183684 = CARTESIAN_POINT ( 'NONE',  ( 4.118918040174416539, -1.664481161445837687, 0.5081549729096886958 ) ) ;
#183685 = CARTESIAN_POINT ( 'NONE',  ( -8.065673753977488758, 14.99999996918362832, -8.613976771944329869 ) ) ;
#183686 = CARTESIAN_POINT ( 'NONE',  ( 4.012850279964918165, 7.625483060026979842, -0.7216878364870197293 ) ) ;
#183687 = CARTESIAN_POINT ( 'NONE',  ( -9.986127180934126102, 5.615481227002261377, 5.966285604742011195 ) ) ;
#183688 = CARTESIAN_POINT ( 'NONE',  ( 2.114359756454447847, -1.018641858927371135, -1.906637348776268004 ) ) ;
#183689 = CARTESIAN_POINT ( 'NONE',  ( 3.022814370378481552, 2.006652721595225675, -0.1948103792988181704 ) ) ;
#183690 = CARTESIAN_POINT ( 'NONE',  ( -9.991996023147281747, 11.72004545083573568, 1.082531754730558626 ) ) ;
#183691 = CARTESIAN_POINT ( 'NONE',  ( 0.8487565004985967443, 0.6285140637429244004, 2.068326486519965979 ) ) ;
#183692 = CARTESIAN_POINT ( 'NONE',  ( 3.871915168923282913, 1.094167467933440108, 1.639771958457488132 ) ) ;
#183693 = CARTESIAN_POINT ( 'NONE',  ( 6.508999999999981689, 4.698440520552249922, 2.462686878797680556 ) ) ;
#183694 = CARTESIAN_POINT ( 'NONE',  ( 2.981904208038600679, -1.913756795454506721, -0.3294587723015156011 ) ) ;
#183697 = ORIENTED_EDGE ( 'NONE', *, *, #57726, .F. ) ;
#183696 = CARTESIAN_POINT ( 'NONE',  ( -4.340018570150322219, 5.196348098997705556, -1.082531754730551743 ) ) ;
#183695 = CARTESIAN_POINT ( 'NONE',  ( -9.205623113554631587, 11.76297960394566466, 1.443375672974076540 ) ) ;
#183698 = CARTESIAN_POINT ( 'NONE',  ( -4.462041952228954500, 6.299077925724123617, -1.443375672974066548 ) ) ;
#183699 = CARTESIAN_POINT ( 'NONE',  ( 4.085803189671889157, 5.860132702740892263, -1.599625672291273171 ) ) ;
#183700 = CARTESIAN_POINT ( 'NONE',  ( -3.806807270387036368, 7.663301925418665839, 0.000000000000000000 ) ) ;
#183701 = CARTESIAN_POINT ( 'NONE',  ( -6.330731382938325602, 6.350551133041632212, 0.7998128361456281477 ) ) ;
#183702 = CARTESIAN_POINT ( 'NONE',  ( -9.205623113554631587, 11.76297960394566466, 1.443375672974076540 ) ) ;
#183703 = CARTESIAN_POINT ( 'NONE',  ( 0.1302870565101400258, -1.360178740744298675, -1.738515015553928622 ) ) ;
#183704 = CARTESIAN_POINT ( 'NONE',  ( 0.000000000000000000, -2.646874999522040639, -3.793834371823813001 ) ) ;
#183705 = CARTESIAN_POINT ( 'NONE',  ( 4.610177715184628155, 1.961415711727178213, -0.04403062578262756377 ) ) ;
#183706 = CARTESIAN_POINT ( 'NONE',  ( 1.318982659667154334, 0.9913977828604101372, -1.755770081111128977 ) ) ;
#183707 = VERTEX_POINT ( 'NONE', #149394 ) ;
#183708 = CARTESIAN_POINT ( 'NONE',  ( 3.942653875399897423, -1.566338124119817987, 1.424821879184964946 ) ) ;
#183709 = CARTESIAN_POINT ( 'NONE',  ( -0.7500000000000006661, 2.889583334016148974, -1.299038105676652011 ) ) ;
#183711 = CARTESIAN_POINT ( 'NONE',  ( -5.555090253297260361, 7.504024600312024340, 1.599625672291269396 ) ) ;
#183710 = CARTESIAN_POINT ( 'NONE',  ( 0.1745949693968693039, 6.948552162806741705, -2.350360486623141121 ) ) ;
#183712 = CARTESIAN_POINT ( 'NONE',  ( 3.275182144284937369, 1.168729223632531733, 1.422615900182722770 ) ) ;
#183713 = VERTEX_POINT ( 'NONE', #976 ) ;
#183714 = CARTESIAN_POINT ( 'NONE',  ( -9.267161690140662600, 10.77044237904097734, -1.199719254218441611 ) ) ;
#183715 = CARTESIAN_POINT ( 'NONE',  ( 0.3999999999999511169, 3.372708439410156522, 0.4999999999999558686 ) ) ;
#183716 = CARTESIAN_POINT ( 'NONE',  ( 5.748313822965784858, 1.043546352714582071, -1.845953426139717246 ) ) ;
#183717 = CARTESIAN_POINT ( 'NONE',  ( 1.499999999999990896, 4.306250000682819490, 1.214306433183764966E-14 ) ) ;
#183718 = CARTESIAN_POINT ( 'NONE',  ( 5.750629710490689384, 9.860818428881154674, -0.7998128361456291469 ) ) ;
#183719 = CARTESIAN_POINT ( 'NONE',  ( 4.938775350723108026, 0.3481798140595788738, 2.030979325763365928 ) ) ;
#183722 = CARTESIAN_POINT ( 'NONE',  ( 3.052128622409277181, -1.392423357299840792, 1.204796875372941667 ) ) ;
#183721 = CARTESIAN_POINT ( 'NONE',  ( 0.4669691663035968054, 1.616376026143636624, 0.9223025969757200349 ) ) ;
#183720 = CARTESIAN_POINT ( 'NONE',  ( 0.3999999999999681033, 3.372708439410100567, 0.4999999999999501510 ) ) ;
#183723 = CARTESIAN_POINT ( 'NONE',  ( 7.913155211870404493, 12.38376484715752213, 0.7998128361456462443 ) ) ;
#183724 = PRODUCT_DEFINITION_FORMATION_WITH_SPECIFIED_SOURCE ( 'ANY', '', #29899, .NOT_KNOWN. ) ;
#183725 = DIRECTION ( 'NONE',  ( -0.6483454320283799088, 0.000000000000000000, 0.7613463080411786432 ) ) ;
#183726 = DIRECTION ( 'NONE',  ( 0.6507913734559658270, 0.7592566023652989049, 0.000000000000000000 ) ) ;
#183727 = AXIS2_PLACEMENT_3D ( 'NONE', #178668, #179733, #81153 ) ;
#183728 = CARTESIAN_POINT ( 'NONE',  ( 1.823171247573553311, 2.059948494222668014, 0.7922594597074559264 ) ) ;
#183729 = CARTESIAN_POINT ( 'NONE',  ( 5.431070396044226811, 0.1588226897794122738, 2.256881284257936215 ) ) ;
#183730 = CARTESIAN_POINT ( 'NONE',  ( 3.555875268649951959, 1.124244472066991518, 1.673854899288424347 ) ) ;
#183731 = AXIS2_PLACEMENT_3D ( 'NONE', #185064, #33501, #199173 ) ;
#183732 = CARTESIAN_POINT ( 'NONE',  ( -7.700668062882078502, 9.046829497192987901, -1.082531754730543971 ) ) ;
#183733 = CARTESIAN_POINT ( 'NONE',  ( 4.605596613081209156, 1.347055988495224232, 1.211539923951672648 ) ) ;
#183734 = CARTESIAN_POINT ( 'NONE',  ( 4.856599191889834799, -1.806003080954875495, -0.6394761690226327122 ) ) ;
#183735 = CARTESIAN_POINT ( 'NONE',  ( 0.6823417656249899377, 5.738541667008087543, -1.181850606188754593 ) ) ;
#183736 = CARTESIAN_POINT ( 'NONE',  ( 4.047701786889636111, 0.6652045265579300537, -1.855968581334372702 ) ) ;
#183737 = CARTESIAN_POINT ( 'NONE',  ( 5.014452206985246185, 1.289541220462528504, -1.355370375751355105 ) ) ;
#183738 = CARTESIAN_POINT ( 'NONE',  ( 4.387043322907993925, 0.09000376980121749249, 1.858987348747977331 ) ) ;
#183739 = CARTESIAN_POINT ( 'NONE',  ( 0.6823417656249917140, 5.592708333674749177, 1.181850606188765695 ) ) ;
#183740 = CARTESIAN_POINT ( 'NONE',  ( 0.3566581422463632189, -1.900417414521380133, -0.6748426577906708745 ) ) ;
#183742 = CARTESIAN_POINT ( 'NONE',  ( 1.278104297367024467, 1.255928009607910623, 1.690453460462447044 ) ) ;
#183741 = CARTESIAN_POINT ( 'NONE',  ( -3.755245360860931303, 5.404205559136275205, -1.443375672974051449 ) ) ;
#183743 = CARTESIAN_POINT ( 'NONE',  ( 10.07387183015377197, 11.71160420905630062, -1.199719254218440723 ) ) ;
#183745 = CARTESIAN_POINT ( 'NONE',  ( -10.34217224912604571, 10.96028913360221502, 0.7998128361456462443 ) ) ;
#183744 = CARTESIAN_POINT ( 'NONE',  ( 0.7500000000000006661, 11.86458333401613174, 1.299038105676657340 ) ) ;
#183746 = CARTESIAN_POINT ( 'NONE',  ( 2.848016566918720294, -1.427295477286108394, -1.568503593382633454 ) ) ;
#183747 = DIRECTION ( 'NONE',  ( 0.000000000000000000, -1.000000000000000000, 0.000000000000000000 ) ) ;
#183748 = CARTESIAN_POINT ( 'NONE',  ( 1.881123716185427286, -1.848401041775033171, -0.8146170886813360879 ) ) ;
#183749 = CARTESIAN_POINT ( 'NONE',  ( 0.6823417656249882723, 2.676041667008084879, -1.181850606188749264 ) ) ;
#183750 = CARTESIAN_POINT ( 'NONE',  ( 6.720655732516647163, 0.005566325962592238996, 1.826293863978686982 ) ) ;
#183751 = CARTESIAN_POINT ( 'NONE',  ( 4.359110081993588182, 5.044382169536003602, -1.199719254218452047 ) ) ;
#183752 = VERTEX_POINT ( 'NONE', #133179 ) ;
#183753 = CARTESIAN_POINT ( 'NONE',  ( 1.722176697685766200, -1.199285583244277253, -1.798187405066300038 ) ) ;
#183754 = CARTESIAN_POINT ( 'NONE',  ( 6.890000000000005898, 7.052460701731090076, 2.598152593539102551 ) ) ;
#183755 = EDGE_CURVE ( 'NONE', #172895, #24495, #116952, .T. ) ;
#183758 = CYLINDRICAL_SURFACE ( 'NONE', #211743, 1.500000000000000222 ) ;
#183757 = CARTESIAN_POINT ( 'NONE',  ( -15.75000000000000000, 10.90000000000000036, -0.7000000000000009548 ) ) ;
#183756 = CARTESIAN_POINT ( 'NONE',  ( 5.083381250481017410, 4.895309311841474553, 0.7998128361456352531 ) ) ;
#183759 = CARTESIAN_POINT ( 'NONE',  ( 10.07334494482924292, 11.81495252613139257, -1.082531754730537088 ) ) ;
#183760 = CARTESIAN_POINT ( 'NONE',  ( 1.499999999999990896, 4.056250000682819490, 1.214306433183764966E-14 ) ) ;
#183761 = CARTESIAN_POINT ( 'NONE',  ( -6.344852701515500293, 9.385783337534627790, 1.082531754730548412 ) ) ;
#183762 = CARTESIAN_POINT ( 'NONE',  ( 1.488088480104592826, -2.181432686776756391, -0.2102995727721947705 ) ) ;
#183763 = DIRECTION ( 'NONE',  ( 5.551115123125765446E-17, 0.000000000000000000, -1.000000000000000000 ) ) ;
#183765 = CARTESIAN_POINT ( 'NONE',  ( -0.6823417656250039265, 12.06770833367473017, -1.181850606188755259 ) ) ;
#183764 = CARTESIAN_POINT ( 'NONE',  ( 1.218052960884225433, -2.206959832567402469, 0.4976822367108637013 ) ) ;
#183766 = CARTESIAN_POINT ( 'NONE',  ( -9.671043645249580933, 10.17730576241299900, 0.7998128361456462443 ) ) ;
#183767 = CARTESIAN_POINT ( 'NONE',  ( -3.701012746406287413, 6.301303389907177532, 1.082531754730560403 ) ) ;
#183768 = CARTESIAN_POINT ( 'NONE',  ( -1.364683531250012516, 2.092708333674750953, 0.7879004041258379498 ) ) ;
#183769 = CARTESIAN_POINT ( 'NONE',  ( 4.607663176575717223, 8.357619647684677133, 0.2284409323990380658 ) ) ;
#183770 = EDGE_CURVE ( 'NONE', #203495, #116100, #119089, .T. ) ;
#183771 = CARTESIAN_POINT ( 'NONE',  ( -1.500000000000008216, 9.250000000000001776, 3.469446951953614189E-15 ) ) ;
#183772 = CARTESIAN_POINT ( 'NONE',  ( 4.441862337843591746, 0.7341043403586414717, -1.561010781705338912 ) ) ;
#183773 = CARTESIAN_POINT ( 'NONE',  ( 7.024532985656128936, 9.288650798055913427, 1.443375672974065660 ) ) ;
#183774 = CARTESIAN_POINT ( 'NONE',  ( 1.809446860903692444, -1.757098282301880365, 0.2103932681993408993 ) ) ;
#183775 = CARTESIAN_POINT ( 'NONE',  ( 5.350674426004140116, 0.6359874849255696683, 2.113150234885258438 ) ) ;
#183776 = ORIENTED_EDGE ( 'NONE', *, *, #70214, .F. ) ;
#183777 = CARTESIAN_POINT ( 'NONE',  ( -4.925354943514475003, 8.968274210734028529, 0.000000000000000000 ) ) ;
#183778 = CARTESIAN_POINT ( 'NONE',  ( 5.097279880301520905, -0.2930512725940071506, 1.994873791649566463 ) ) ;
#183779 = ORIENTED_EDGE ( 'NONE', *, *, #94104, .F. ) ;
#183780 = EDGE_CURVE ( 'NONE', #25151, #185939, #126357, .T. ) ;
#183781 = CARTESIAN_POINT ( 'NONE',  ( 3.115926070338378207, -0.9207206926411042325, -1.628290677324291780 ) ) ;
#183782 = EDGE_CURVE ( 'NONE', #118779, #130707, #167398, .T. ) ;
#183783 = CIRCLE ( 'NONE', #173473, 0.5000000000000008882 ) ;
#183784 = CARTESIAN_POINT ( 'NONE',  ( -5.899206235277530297, 9.896508017883515862, 0.7216878364870267237 ) ) ;
#183785 = CARTESIAN_POINT ( 'NONE',  ( 2.214975196874233720, 1.533708969217022933, -1.142120075431733994 ) ) ;
#183786 = FACE_OUTER_BOUND ( 'NONE', #143278, .T. ) ;
#183787 = CARTESIAN_POINT ( 'NONE',  ( -10.47097306639366820, 4.046871294038967726, -7.151610515452683003 ) ) ;
#183788 = LINE ( 'NONE', #101473, #3815 ) ;
#183789 = CARTESIAN_POINT ( 'NONE',  ( -1.201851678989727383E-14, 4.759375000341419693, -1.575800808251660134 ) ) ;
#183790 = CARTESIAN_POINT ( 'NONE',  ( 0.3340484552533556917, -1.024938778295768849, -1.614363347046356978 ) ) ;
#183791 = CARTESIAN_POINT ( 'NONE',  ( 4.882344714696929877, 8.710169577206153591, -0.7216878364870458196 ) ) ;
#183792 = CARTESIAN_POINT ( 'NONE',  ( 1.539427311113782837, 1.813978416018032558, -0.7477436361984082236 ) ) ;
#183793 = CARTESIAN_POINT ( 'NONE',  ( 0.1927366488196740335, -1.238295061544148812, -1.591656064170659191 ) ) ;
#183794 = CARTESIAN_POINT ( 'NONE',  ( -5.469788628470539926, 5.346117919495872783, -0.7998128361456362523 ) ) ;
#183795 = CARTESIAN_POINT ( 'NONE',  ( 5.308877466510794285, -0.5174029350529658622, -2.056363676157816123 ) ) ;
#183796 = CARTESIAN_POINT ( 'NONE',  ( 9.582915646760733708, 10.07448976417602893, 0.7998128361456462443 ) ) ;
#183797 = CARTESIAN_POINT ( 'NONE',  ( 0.2978465640060874997, -1.869987984933557890, -0.05268733258671080832 ) ) ;
#183798 = CARTESIAN_POINT ( 'NONE',  ( -1.402160292154681736E-14, 2.196875000341423689, -1.575800808251660134 ) ) ;
#183799 = CARTESIAN_POINT ( 'NONE',  ( 2.056891478215248981, 0.4451058530966587323, 1.963224067645082949 ) ) ;
#183800 = ORIENTED_EDGE ( 'NONE', *, *, #143084, .F. ) ;
#183802 = CARTESIAN_POINT ( 'NONE',  ( 0.6677574575255783573, 1.425215384571768551, 1.565850431965072787 ) ) ;
#183801 = CARTESIAN_POINT ( 'NONE',  ( -8.703971430293361067, 9.256980878204810637, 0.7216878364870438212 ) ) ;
#183803 = CARTESIAN_POINT ( 'NONE',  ( 11.70317096822030400, 7.060310916292978689, -2.662588479640240813 ) ) ;
#183804 = CARTESIAN_POINT ( 'NONE',  ( 2.980987059868035693, 1.948563265827065960, 0.6999735360200682877 ) ) ;
#183805 = CARTESIAN_POINT ( 'NONE',  ( 5.391302360089590628, 6.318882837306503575, -1.199719254218452047 ) ) ;
#183806 = CARTESIAN_POINT ( 'NONE',  ( 4.411198876399872404, 6.239761003923544713, -1.599625672291273171 ) ) ;
#183807 = EDGE_LOOP ( 'NONE', ( #8278, #86921, #116095, #201438 ) ) ;
#183809 = CARTESIAN_POINT ( 'NONE',  ( 3.517450787741589036, 6.191110788085444128, -1.199719254218446718 ) ) ;
#183808 = CARTESIAN_POINT ( 'NONE',  ( 4.716787809154822320, -0.1028738300157816532, 2.088225860312553195 ) ) ;
#183812 = ORIENTED_EDGE ( 'NONE', *, *, #18617, .T. ) ;
#183811 = CARTESIAN_POINT ( 'NONE',  ( 2.226969132303910470, 1.618658205268191930, 0.8133494039403755815 ) ) ;
#183810 = CARTESIAN_POINT ( 'NONE',  ( 3.557459645987316232, 0.4443818804308434789, -1.770531947851671006 ) ) ;
#183813 = CARTESIAN_POINT ( 'NONE',  ( 6.358075476802443227, 2.201304964888863402, -0.1578768562689457922 ) ) ;
#183814 = CARTESIAN_POINT ( 'NONE',  ( 6.890000000000008562, 1.260399741928097672, 2.114076522472335462 ) ) ;
#183815 = CARTESIAN_POINT ( 'NONE',  ( 9.285099613924293394, 13.38408970557267175, 6.770650828121584475 ) ) ;
#183816 = CARTESIAN_POINT ( 'NONE',  ( 5.456176519787153012, 2.204477245749701719, -0.1032804940204190558 ) ) ;
#183817 = CARTESIAN_POINT ( 'NONE',  ( 0.6823417656249934904, 9.255208333674728394, 1.181850606188764807 ) ) ;
#183818 = ORIENTED_EDGE ( 'NONE', *, *, #156042, .T. ) ;
#183819 = CARTESIAN_POINT ( 'NONE',  ( 3.545477442914763078, -1.765841875850767906, 0.7343832577718923948 ) ) ;
#183820 = CARTESIAN_POINT ( 'NONE',  ( -5.108724954250998707, 4.854600622914589714, -0.7998128361456221525 ) ) ;
#183821 = CARTESIAN_POINT ( 'NONE',  ( 7.099665995050449041, 11.43469409420089455, 0.7998128361456462443 ) ) ;
#183822 = CARTESIAN_POINT ( 'NONE',  ( 0.6801582343749813520, 0.005208333674754095366, 1.178068619123793015 ) ) ;
#183823 = CARTESIAN_POINT ( 'NONE',  ( 3.972175818679561043, 7.578029521860726092, -0.7216878364870197293 ) ) ;
#183824 = CARTESIAN_POINT ( 'NONE',  ( 4.905139262582266291, 4.827437033166341429, 0.6004564335717228474 ) ) ;
#183825 = CARTESIAN_POINT ( 'NONE',  ( 6.902720183911292828, 14.55305236562704074, -9.761920501353824164 ) ) ;
#183826 = CARTESIAN_POINT ( 'NONE',  ( 5.133413704082500385E-17, 15.44694763437295748, -11.95586206896552106 ) ) ;
#183827 = VERTEX_POINT ( 'NONE', #57232 ) ;
#183828 = AXIS2_PLACEMENT_3D ( 'NONE', #92762, #93829, #73264 ) ;
#183829 = CARTESIAN_POINT ( 'NONE',  ( 0.000000000000000000, 7.849261790823902629, 0.000000000000000000 ) ) ;
#183830 = CARTESIAN_POINT ( 'NONE',  ( 3.813614929637609841, -1.843318686535613926, 0.3169883347873063695 ) ) ;
#183831 = CARTESIAN_POINT ( 'NONE',  ( 8.167861197590044142, 8.493869250135347215, 0.000000000000000000 ) ) ;
#183832 = CARTESIAN_POINT ( 'NONE',  ( -0.2409995289980003397, 4.087843961663322645, -2.555282842491034323 ) ) ;
#183833 = CARTESIAN_POINT ( 'NONE',  ( -5.910991785878165317, 8.879612269291090598, -1.082531754730538864 ) ) ;
#183834 = CARTESIAN_POINT ( 'NONE',  ( 4.435452530326143616, 5.203724702582467998, -1.199719254218452047 ) ) ;
#183835 = CARTESIAN_POINT ( 'NONE',  ( 4.147904930777053245, 6.926640621626830807, -1.199719254218452047 ) ) ;
#183836 = CARTESIAN_POINT ( 'NONE',  ( 0.3210686601547476093, -1.756690599571947065, -0.8905566435374636658 ) ) ;
#183837 = CARTESIAN_POINT ( 'NONE',  ( 2.636342400811112707, 0.6820146075395253638, 1.897692325672148073 ) ) ;
#183838 = CARTESIAN_POINT ( 'NONE',  ( -7.995557903757128493, 10.35123685918189729, 1.599625672291295375 ) ) ;
#183839 = CARTESIAN_POINT ( 'NONE',  ( 7.028976294042106332, 7.165170195996068969, 0.000000000000000000 ) ) ;
#183840 = CARTESIAN_POINT ( 'NONE',  ( 2.484552680892829546, -0.3758780662847274190, -2.158817762932266682 ) ) ;
#183841 = CARTESIAN_POINT ( 'NONE',  ( 6.322862864304120478, 1.705426906915354035, 0.6521430802832667295 ) ) ;
#183842 = CARTESIAN_POINT ( 'NONE',  ( -3.460355519985875983, 5.060167411448709629, 1.599625672291267398 ) ) ;
#183843 = CARTESIAN_POINT ( 'NONE',  ( 5.573810548993915148, 5.675402860013913475, 0.000000000000000000 ) ) ;
#183845 = EDGE_CURVE ( 'NONE', #129573, #175025, #19373, .T. ) ;
#183844 = CARTESIAN_POINT ( 'NONE',  ( 7.425061681778431399, 11.81432239538354345, 0.7998128361456462443 ) ) ;
#183846 = CARTESIAN_POINT ( 'NONE',  ( 4.566398809704347528, 4.221886787610169556, -0.7998128361456211532 ) ) ;
#183847 = CARTESIAN_POINT ( 'NONE',  ( 6.536439455564150514, 9.679577560583279450, 1.082531754730549078 ) ) ;
#183848 = ORIENTED_EDGE ( 'NONE', *, *, #134782, .T. ) ;
#183850 = CARTESIAN_POINT ( 'NONE',  ( 0.7506400166778016692, 1.983664654656223991, 0.3420602577784581655 ) ) ;
#183849 = CARTESIAN_POINT ( 'NONE',  ( 3.509164994824386596, -1.813400730843343966, 0.3181347684400454012 ) ) ;
#183851 = CARTESIAN_POINT ( 'NONE',  ( 3.585630231873372598, 1.460649136416993121, -1.774545834528557409 ) ) ;
#183853 = CARTESIAN_POINT ( 'NONE',  ( 0.5318007479364270651, 1.064995724915913433, 1.525891442952797439 ) ) ;
#183852 = CARTESIAN_POINT ( 'NONE',  ( 2.901081683644319842, 5.368050483351580304, 1.082531754730548412 ) ) ;
#183854 = CARTESIAN_POINT ( 'NONE',  ( 1.642778471875000035, -3.726041666188707691, -2.845375778867859751 ) ) ;
#183855 = CARTESIAN_POINT ( 'NONE',  ( -3.730464822054482710, 7.503959392372201442, 1.040834085586084257E-14 ) ) ;
#183856 = CARTESIAN_POINT ( 'NONE',  ( 4.588094604188536429, 1.105678411722615051, 1.560157546714964871 ) ) ;
#183857 = CARTESIAN_POINT ( 'NONE',  ( -10.14557902172788495, 10.73093036830436553, 1.040834085586084257E-14 ) ) ;
#183858 = CARTESIAN_POINT ( 'NONE',  ( 6.039396378094620488, 7.052381734106362821, -1.030794243266313082 ) ) ;
#183859 = CARTESIAN_POINT ( 'NONE',  ( -6.780486220610186798, 8.043560357867583832, -1.082531754730549967 ) ) ;
#183861 = CARTESIAN_POINT ( 'NONE',  ( 1.973319494866377699, 1.790917844098998124, -0.5403536831049270406 ) ) ;
#183860 = CARTESIAN_POINT ( 'NONE',  ( 3.896100387133538234, -0.6578992572023834029, -1.984587938432079257 ) ) ;
#183862 = CARTESIAN_POINT ( 'NONE',  ( 6.304178240674458422, 10.29869901418813782, 1.040834085586084257E-14 ) ) ;
#183863 = CARTESIAN_POINT ( 'NONE',  ( 3.491524089112467699, -1.738650433694358233, -0.08144215361822156052 ) ) ;
#183864 = CARTESIAN_POINT ( 'NONE',  ( 3.310162060030825248, 7.013606170011280838, -0.7998128361456291469 ) ) ;
#183866 = CARTESIAN_POINT ( 'NONE',  ( 4.436542580169809291, 6.199052314996659874, 1.599625672291267398 ) ) ;
#183865 = DIRECTION ( 'NONE',  ( 0.7592566023653044560, -0.6507913734559596097, 8.231876577584280507E-15 ) ) ;
#183867 = CARTESIAN_POINT ( 'NONE',  ( 4.178129962880992920, -0.9906059873891288614, 1.411843326160647782 ) ) ;
#183868 = CARTESIAN_POINT ( 'NONE',  ( -6.527360889975461156, 9.702672574024962415, 1.199719254218452047 ) ) ;
#183869 = CARTESIAN_POINT ( 'NONE',  ( 0.2109833617158912156, 1.658496975328831891, 0.5066527762955413960 ) ) ;
#183870 = CARTESIAN_POINT ( 'NONE',  ( 6.235036409211808461, 0.2120174297785166195, 2.196685143856290878 ) ) ;
#183871 = FACE_OUTER_BOUND ( 'NONE', #48326, .T. ) ;
#183872 = PRESENTATION_LAYER_ASSIGNMENT (  '', '', ( #14408 ) ) ;
#183873 = DIRECTION ( 'NONE',  ( -1.000000000000000000, 8.673617379884035472E-16, 0.000000000000000000 ) ) ;
#183874 = CARTESIAN_POINT ( 'NONE',  ( 3.678747780723041760, 1.381198535464265520, -1.675025177318607783 ) ) ;
#183875 = CARTESIAN_POINT ( 'NONE',  ( 2.543341688579534576, -1.352695106659363766, -1.226303905950577366 ) ) ;
#183876 = CARTESIAN_POINT ( 'NONE',  ( 5.120359440597627376, 2.086519121862129289, 0.3590335527714014763 ) ) ;
#183877 =( GEOMETRIC_REPRESENTATION_CONTEXT ( 3 ) GLOBAL_UNCERTAINTY_ASSIGNED_CONTEXT ( ( #103484 ) ) GLOBAL_UNIT_ASSIGNED_CONTEXT ( ( #172642, #108764, #192056 ) ) REPRESENTATION_CONTEXT ( 'NONE', 'WORKASPACE' ) );
#183878 = ORIENTED_EDGE ( 'NONE', *, *, #96921, .T. ) ;
#183880 = CARTESIAN_POINT ( 'NONE',  ( 1.364683531249990311, 2.946875000341416140, 1.214306433183764966E-14 ) ) ;
#183879 = CARTESIAN_POINT ( 'NONE',  ( 5.513300880735551246, -2.237181406077014323, 0.4993042908148867531 ) ) ;
#183881 = CARTESIAN_POINT ( 'NONE',  ( 2.191614386903386613, 5.708633884695917260, -0.7998128361456281477 ) ) ;
#183882 = CARTESIAN_POINT ( 'NONE',  ( 1.840644454891388282, 1.218392294859267144, -1.735325642819862013 ) ) ;
#183883 = CARTESIAN_POINT ( 'NONE',  ( -4.067082894419624672, 6.728385229256075739, 1.082531754730560403 ) ) ;
#183884 = CARTESIAN_POINT ( 'NONE',  ( 2.901081683644319842, 5.368050483351580304, 1.082531754730548412 ) ) ;
#183885 = CARTESIAN_POINT ( 'NONE',  ( -5.327991180046197428, 8.199444895820425572, 1.082531754730548412 ) ) ;
#183886 =( BOUNDED_SURFACE ( )  B_SPLINE_SURFACE ( 3, 2, ( 
 ( #97036, #130650, #159875 ),
 ( #44010, #209667, #94897 ),
 ( #98097, #47217, #142593 ),
 ( #110130, #29885, #179340 ),
 ( #11480, #210748, #61309 ),
 ( #144737, #30962, #48282 ),
 ( #78613, #95969, #114395 ),
 ( #162023, #14670, #10410 ),
 ( #146853, #76482, #178275 ),
 ( #127471, #193441, #62371 ),
 ( #208602, #45085, #32014 ),
 ( #128533, #212873, #13613 ),
 ( #79687, #111194, #145799 ),
 ( #211805, #28813, #60233 ) ),
 .UNSPECIFIED., .F., .F., .T. ) 
 B_SPLINE_SURFACE_WITH_KNOTS ( ( 4, 2, 2, 2, 2, 2, 4 ),
 ( 3, 3 ),
 ( 0.001912008033049055660, 0.002390010041311319087, 0.002629011045442450692, 0.002868012049573582731, 0.003346014057835845941, 0.003585015061966977980, 0.003824016066098109585 ),
 ( 0.000000000000000000, 1.000000000000000000 ),
 .UNSPECIFIED. ) 
 GEOMETRIC_REPRESENTATION_ITEM ( )  RATIONAL_B_SPLINE_SURFACE ( (
 ( 1.000000000000000000, 0.8708456909032173954, 1.000000000000000000),
 ( 1.000000000000000000, 0.8699862225466781229, 1.000000000000000000),
 ( 1.000000000000000000, 0.8740515128124174415, 1.000000000000000000),
 ( 1.000000000000000000, 0.8627336009020736274, 1.000000000000000000),
 ( 1.000000000000000000, 0.8557431983334260472, 1.000000000000000000),
 ( 1.000000000000000000, 0.8314605231444136546, 1.000000000000000000),
 ( 1.000000000000000000, 0.8141324793652144898, 1.000000000000000000),
 ( 1.000000000000000000, 0.7486317046916625140, 1.000000000000000000),
 ( 1.000000000000000000, 0.6849789572270683635, 1.000000000000000000),
 ( 1.000000000000000000, 0.5903265755406649218, 1.000000000000000000),
 ( 1.000000000000000000, 0.5583523351999168938, 1.000000000000000000),
 ( 1.000000000000000000, 0.5090820572709163772, 1.000000000000000000),
 ( 1.000000000000000000, 0.4920791080019514263, 1.000000000000000000),
 ( 1.000000000000000000, 0.4915962107220576138, 1.000000000000000000) ) ) 
 REPRESENTATION_ITEM ( '' )  SURFACE ( )  );
#183888 = CARTESIAN_POINT ( 'NONE',  ( 1.500000000000001332, 12.15625000068279427, 0.000000000000000000 ) ) ;
#183887 = CARTESIAN_POINT ( 'NONE',  ( -10.91962425643211532, -9.999999999999998224, 0.09058751758334862569 ) ) ;
#183890 = VERTEX_POINT ( 'NONE', #7387 ) ;
#183889 = CARTESIAN_POINT ( 'NONE',  ( 1.102519259163890153, -0.9942956747860592914, 1.986404433118430291 ) ) ;
#183891 = CARTESIAN_POINT ( 'NONE',  ( 6.205703963786828758, 1.882472927010571118, 0.7231429968634556227 ) ) ;
#183893 = CARTESIAN_POINT ( 'NONE',  ( 3.977431857364383205, -0.1567958407116451236, 2.056696387209145716 ) ) ;
#183892 = CARTESIAN_POINT ( 'NONE',  ( 2.822068529938852155, 6.444163718237301275, -0.7998128361456291469 ) ) ;
#183895 = FACE_OUTER_BOUND ( 'NONE', #214395, .T. ) ;
#183894 = CARTESIAN_POINT ( 'NONE',  ( 7.028976294042106332, 7.165170195996068969, 0.000000000000000000 ) ) ;
#183896 = CARTESIAN_POINT ( 'NONE',  ( 5.176180785367283654, 9.260904359562321275, -0.7998128361456481317 ) ) ;
#183898 = ADVANCED_FACE ( 'NONE', ( #37777 ), #43731, .F. ) ;
#183897 = CARTESIAN_POINT ( 'NONE',  ( 3.285556943750000070, -2.034374999522043481, 0.000000000000000000 ) ) ;
#183899 = CARTESIAN_POINT ( 'NONE',  ( 0.8848510708264365476, 1.842997052242268508, -0.9869714196348714497 ) ) ;
#183900 = CARTESIAN_POINT ( 'NONE',  ( 4.992814645674492624, -2.006446365708704160, 0.2004330516618065550 ) ) ;
#183901 = CARTESIAN_POINT ( 'NONE',  ( 4.651808992177354440, 0.7092673950449077669, 1.699362209096597187 ) ) ;
#183902 = CARTESIAN_POINT ( 'NONE',  ( 3.818592820543298405, 7.606775390609172405, -0.7998128361456221525 ) ) ;
#183903 =( NAMED_UNIT ( * ) PLANE_ANGLE_UNIT ( ) SI_UNIT ( $, .RADIAN. ) );
#183904 = CARTESIAN_POINT ( 'NONE',  ( 1.184105695005283287, -1.681391461502951046, -0.3836232258775870152 ) ) ;
#183905 = CARTESIAN_POINT ( 'NONE',  ( -0.2234322562767385167, -0.4468160588090731022, -1.973564571300358228 ) ) ;
#183906 = CARTESIAN_POINT ( 'NONE',  ( 0.7745980011552360267, 2.023606461939434720, -1.090472508649400263 ) ) ;
#183907 = CARTESIAN_POINT ( 'NONE',  ( -5.738125327081750271, 7.717565519727259904, 1.599625672291269396 ) ) ;
#183908 = CARTESIAN_POINT ( 'NONE',  ( 1.704739465036476442, -0.8136145326368517949, -2.111227425349770481 ) ) ;
#183909 = CARTESIAN_POINT ( 'NONE',  ( 2.930406704442231725, 1.169546373139153328, -1.751267329298618280 ) ) ;
#183910 = CARTESIAN_POINT ( 'NONE',  ( -4.125423880308188629, 8.035021303660014880, -0.7998128361456481317 ) ) ;
#183912 = EDGE_CURVE ( 'NONE', #169017, #85779, #27650, .T. ) ;
#183911 = CARTESIAN_POINT ( 'NONE',  ( 7.284808609244363353, 7.393364887073558656, 0.7998128361456341429 ) ) ;
#183913 = CARTESIAN_POINT ( 'NONE',  ( 5.844973620822830895, 8.872867420051733234, 1.082531754730549967 ) ) ;
#183914 = CARTESIAN_POINT ( 'NONE',  ( 5.906250000000004441, 1.895863743163945125, -0.7852924748303062863 ) ) ;
#183915 = CARTESIAN_POINT ( 'NONE',  ( -6.261168011412601153, 6.199117522936475666, 1.040834085586084257E-14 ) ) ;
#183916 = CARTESIAN_POINT ( 'NONE',  ( 5.626270559546804328, 9.507806719539201978, 0.7216878364870438212 ) ) ;
#183917 = CARTESIAN_POINT ( 'NONE',  ( 5.344703475446304530, 6.534489784648752853, 1.338571508491542383 ) ) ;
#183918 = CARTESIAN_POINT ( 'NONE',  ( -4.783329267523015460, 4.474972321731942593, -0.7998128361456221525 ) ) ;
#183919 = CARTESIAN_POINT ( 'NONE',  ( 5.537407084817251857, -0.05464564937080264306, 2.220880467482534204 ) ) ;
#183920 = CARTESIAN_POINT ( 'NONE',  ( 3.855584222106961612, 2.174980185927982923, -0.2676557845137442215 ) ) ;
#183921 = CARTESIAN_POINT ( 'NONE',  ( -4.252453736180621391, 8.112946458852704268, -0.7998128361456281477 ) ) ;
#183922 = CARTESIAN_POINT ( 'NONE',  ( -11.97297122925985136, 9.801250793269115746, 0.8121202983519364427 ) ) ;
#183923 = CARTESIAN_POINT ( 'NONE',  ( 5.687936657224680559, -1.243353266631580523, -1.517579924814119074 ) ) ;
#183924 = CARTESIAN_POINT ( 'NONE',  ( 0.6823417656249882723, 2.676041667008084879, -1.181850606188749264 ) ) ;
#183925 = CARTESIAN_POINT ( 'NONE',  ( 6.610000000000028741, 4.695285100415147461, 2.562642482393460597 ) ) ;
#183926 = CARTESIAN_POINT ( 'NONE',  ( -5.802526556968872207, 6.832331073627524454, 1.082531754730548412 ) ) ;
#183927 = CARTESIAN_POINT ( 'NONE',  ( 4.974906307097914926, -1.534222593358970821, 1.464151343314526121 ) ) ;
#183928 = CARTESIAN_POINT ( 'NONE',  ( -5.939880696562884310, 9.943961556049767836, 0.7216878364870267237 ) ) ;
#183929 = ORIENTED_EDGE ( 'NONE', *, *, #2092, .T. ) ;
#183931 = CARTESIAN_POINT ( 'NONE',  ( 6.192270064542984898, -2.150811787302907785, -0.2168040374768212541 ) ) ;
#183930 = CARTESIAN_POINT ( 'NONE',  ( -6.292392690518214593, 7.474117906093608710, -1.082531754730549967 ) ) ;
#183932 = CARTESIAN_POINT ( 'NONE',  ( 5.789495288235341874, 6.713164910151406595, 1.199719254218462483 ) ) ;
#183933 = CARTESIAN_POINT ( 'NONE',  ( 5.390138975101268493, -0.4531076923771395482, -1.784498753146485539 ) ) ;
#183934 = CARTESIAN_POINT ( 'NONE',  ( -1.364683531249997417, 3.321875000341423245, 1.214306433183764966E-14 ) ) ;
#183935 = CARTESIAN_POINT ( 'NONE',  ( 0.6259951400321401849, 0.1256764613348868298, 1.735981902797034238 ) ) ;
#183936 = CARTESIAN_POINT ( 'NONE',  ( 11.48784849554594345, 12.26950472818075077, 3.469614872287801521 ) ) ;
#183937 = CARTESIAN_POINT ( 'NONE',  ( -0.6823417656250003738, -0.7197916663252492686, -1.181850606188749264 ) ) ;
#183938 = DIRECTION ( 'NONE',  ( 0.6743504407188133376, -1.091556109765015220E-14, 0.7384114592165688107 ) ) ;
#183939 = CARTESIAN_POINT ( 'NONE',  ( 5.559502693676295237, 0.4258712887980077300, -2.119171757835013548 ) ) ;
#183940 = CARTESIAN_POINT ( 'NONE',  ( -3.972702704004144714, 4.593573561881607148, 1.199719254218462483 ) ) ;
#183942 = ADVANCED_FACE ( 'NONE', ( #9540 ), #26850, .F. ) ;
#183941 = AXIS2_PLACEMENT_3D ( 'NONE', #5389, #42216, #175410 ) ;
#183943 = CARTESIAN_POINT ( 'NONE',  ( -8.012505595552038784, 8.450270737673262644, 0.7216878364870578100 ) ) ;
#183944 = CARTESIAN_POINT ( 'NONE',  ( 4.469695567000064429, 2.097540297429688838, -0.5223010940857697459 ) ) ;
#183945 = CARTESIAN_POINT ( 'NONE',  ( -1.364683531249997417, 3.259375000341423245, 1.214306433183764966E-14 ) ) ;
#183946 = CARTESIAN_POINT ( 'NONE',  ( 4.885985806860754010, -0.9320292603649924512, 1.737142539612034353 ) ) ;
#183947 = CARTESIAN_POINT ( 'NONE',  ( 4.534371549175888028, 1.681635666518576988, -0.4216726850935527127 ) ) ;
#183948 = CARTESIAN_POINT ( 'NONE',  ( 1.505704256594592838, -2.174480876681058827, 0.2726767719730335826 ) ) ;
#183949 = CARTESIAN_POINT ( 'NONE',  ( 2.310004868091195540, -0.5052997711322243513, 2.251431844744283151 ) ) ;
#183950 = CARTESIAN_POINT ( 'NONE',  ( 5.132131416026131987, 1.062877790662479116, -1.765404227961290484 ) ) ;
#183951 = CARTESIAN_POINT ( 'NONE',  ( 6.550339418841141459, -1.498220820903242601, 1.235316290203094081 ) ) ;
#183952 = CARTESIAN_POINT ( 'NONE',  ( -6.182154857707119255, 10.15633840072622363, 0.000000000000000000 ) ) ;
#183953 = CARTESIAN_POINT ( 'NONE',  ( -4.980641328173854632, 6.904110530993182948, 1.599625672291263179 ) ) ;
#183954 = LINE ( 'NONE', #129968, #33363 ) ;
#183955 = FILL_AREA_STYLE ('',( #19316 ) ) ;
#183956 = CARTESIAN_POINT ( 'NONE',  ( 1.688125190044654556, 1.678006053171029688, 1.117831401076685660 ) ) ;
#183957 = CARTESIAN_POINT ( 'NONE',  ( -6.195713011320790109, 9.211787032307496403, -1.082531754730537976 ) ) ;
#183958 = CARTESIAN_POINT ( 'NONE',  ( 2.889901548669851383, 1.559680528474843841, 1.561422205034967314 ) ) ;
#183959 = CARTESIAN_POINT ( 'NONE',  ( 3.285556943750000070, -1.771874999522041083, 0.000000000000000000 ) ) ;
#183960 = CARTESIAN_POINT ( 'NONE',  ( 1.358004595412452664, -1.861131634099476573, -0.006961619045023344915 ) ) ;
#183961 = CARTESIAN_POINT ( 'NONE',  ( -0.1290005225502398323, 0.2247172878383028038, -2.207197350255707402 ) ) ;
#183962 = CARTESIAN_POINT ( 'NONE',  ( -11.84100621633422179, 12.48958425776662118, 1.444132586618105174 ) ) ;
#183963 = CYLINDRICAL_SURFACE ( 'NONE', #134203, 1.500000000000000222 ) ;
#183965 = CARTESIAN_POINT ( 'NONE',  ( 6.825078400183579141, 1.241995729952071637, 2.258014901253778461 ) ) ;
#183964 = CARTESIAN_POINT ( 'NONE',  ( -4.588266729941921973, 8.494429388143421633, -0.1275441020149002680 ) ) ;
#183966 = CARTESIAN_POINT ( 'NONE',  ( -1.360316468749997565, 2.890625000341401574, 1.734723475976807094E-15 ) ) ;
#183967 = ORIENTED_EDGE ( 'NONE', *, *, #100257, .F. ) ;
#183968 = CARTESIAN_POINT ( 'NONE',  ( 3.467699783257427004, 2.010999201309400686, -0.4499753609362132090 ) ) ;
#183969 = CARTESIAN_POINT ( 'NONE',  ( -4.757329562667670667E-14, 1.953125000341451312, 1.570758158831762286 ) ) ;
#183970 = CARTESIAN_POINT ( 'NONE',  ( -6.403528624356093601, 6.365204904703887223, 1.040834085586084257E-14 ) ) ;
#183971 = CARTESIAN_POINT ( 'NONE',  ( 1.875654870896212190, 0.3429857902390308078, -1.990162865174507800 ) ) ;
#183972 = CARTESIAN_POINT ( 'NONE',  ( -1.402160292154681736E-14, -0.7874999999999764411, 1.732050807568877637 ) ) ;
#183973 = CARTESIAN_POINT ( 'NONE',  ( 3.011882680530176604, 6.665613560593854459, 0.7998128361456341429 ) ) ;
#183974 = AXIS2_PLACEMENT_3D ( 'NONE', #212415, #159421, #194045 ) ;
#183975 = CARTESIAN_POINT ( 'NONE',  ( 2.325137485922982084, -0.001238304602014379070, 2.061077815622249343 ) ) ;
#183977 = CARTESIAN_POINT ( 'NONE',  ( -1.364683531250010295, 13.63020833367473017, 0.7879004041258445001 ) ) ;
#183976 = CARTESIAN_POINT ( 'NONE',  ( -5.233084104750526322, 5.207612331738130429, 0.000000000000000000 ) ) ;
#183978 = CARTESIAN_POINT ( 'NONE',  ( 5.632522751473472589, 8.658694745772667289, -1.199719254218440723 ) ) ;
#183979 =( BOUNDED_CURVE ( )  B_SPLINE_CURVE ( 3, ( #68378, #121507, #134509, #39109 ),
 .UNSPECIFIED., .F., .T. ) 
 B_SPLINE_CURVE_WITH_KNOTS ( ( 4, 4 ),
 ( 4.683789229004536203, 4.706575325518645769 ),
 .UNSPECIFIED. ) 
 CURVE ( )  GEOMETRIC_REPRESENTATION_ITEM ( )  RATIONAL_B_SPLINE_CURVE ( ( 1.000000000000000000, 0.9999567332851475587, 0.9999567332851475587, 1.000000000000000000 ) ) 
 REPRESENTATION_ITEM ( '' )  );
#183980 = CARTESIAN_POINT ( 'NONE',  ( -0.1408020194050172424, 4.085453189724971956, -2.655103234342595986 ) ) ;
#183981 = CARTESIAN_POINT ( 'NONE',  ( 5.127635347277352373, -2.096377701570474539, 0.6897739467496829535 ) ) ;
#183982 = CARTESIAN_POINT ( 'NONE',  ( 4.877901405866606588, 8.912911750144889567, 0.7998128361456341429 ) ) ;
#183983 = CARTESIAN_POINT ( 'NONE',  ( 1.458524589769864210, 0.8745999688587955401, 1.976921506453344080 ) ) ;
#183984 = CARTESIAN_POINT ( 'NONE',  ( -5.260200412422220140, 5.239248024021764039, -0.7216878364870207285 ) ) ;
#183985 = CARTESIAN_POINT ( 'NONE',  ( 1.587125413319636635, 1.679225032509903404, 1.116207499648947943 ) ) ;
#183986 = FACE_OUTER_BOUND ( 'NONE', #1330, .T. ) ;
#183987 =( NAMED_UNIT ( * ) PLANE_ANGLE_UNIT ( ) SI_UNIT ( $, .RADIAN. ) );
#183988 = CARTESIAN_POINT ( 'NONE',  ( 2.272138710904994863, -1.152746988206950096, 1.473173409640892162 ) ) ;
#183989 = CARTESIAN_POINT ( 'NONE',  ( 4.083220446344194343, 1.622485107653489633, 1.197306254465977826 ) ) ;
#183991 = FACE_OUTER_BOUND ( 'NONE', #153529, .T. ) ;
#183990 = CARTESIAN_POINT ( 'NONE',  ( -0.6823417656250212460, 2.301041667008084435, 1.181850606188767472 ) ) ;
#183993 = CARTESIAN_POINT ( 'NONE',  ( 5.373694187740483130, 2.029982003570539817, -0.5606972681787207868 ) ) ;
#183992 = CARTESIAN_POINT ( 'NONE',  ( -7.609150525767646833, 9.900428251527500834, -1.599625672291263179 ) ) ;
#183994 = CARTESIAN_POINT ( 'NONE',  ( 6.982612806237943559, 8.105135347821125436, -1.199719254218446718 ) ) ;
#183995 = CARTESIAN_POINT ( 'NONE',  ( -5.879432169820529630, 10.01108796476595764, -0.7998128361456221525 ) ) ;
#183996 = CARTESIAN_POINT ( 'NONE',  ( 1.772826578343118742, 3.950000000000034373, -0.4000000000000274447 ) ) ;
#183997 = CARTESIAN_POINT ( 'NONE',  ( 5.133071871609922177, 1.867805937340912159, 0.7691607467245373808 ) ) ;
#183998 = CARTESIAN_POINT ( 'NONE',  ( 1.364683531249992088, 5.634375000341417916, 1.214306433183764966E-14 ) ) ;
#183999 = CARTESIAN_POINT ( 'NONE',  ( 0.6024794235527919373, 2.056786662827071233, 0.1555941968269194953 ) ) ;
#184000 = CARTESIAN_POINT ( 'NONE',  ( 7.944714827928043732, 10.29191993738131927, 1.443375672974076540 ) ) ;
#184001 = CARTESIAN_POINT ( 'NONE',  ( 5.773793314573267388, 7.829454515125894964, 1.599625672291268286 ) ) ;
#184002 = CARTESIAN_POINT ( 'NONE',  ( 5.631432701629774051, 7.663367133358481631, 1.599625672291269396 ) ) ;
#184003 = CARTESIAN_POINT ( 'NONE',  ( -1.402160292154681736E-14, 0.1343750003414218575, 1.575800808251672791 ) ) ;
#184005 = CARTESIAN_POINT ( 'NONE',  ( -3.511198596259319960, 6.271927390929313617, 1.082471891955974153 ) ) ;
#184004 = CARTESIAN_POINT ( 'NONE',  ( 5.285699784481295183, 7.260012063351913625, 1.599625672291268286 ) ) ;
#184006 = CARTESIAN_POINT ( 'NONE',  ( 7.578644679914706472, 9.864838098032418401, 1.443375672974076540 ) ) ;
#184008 = CARTESIAN_POINT ( 'NONE',  ( -4.057819647168310340, 3.809089625685526226, -2.500000000000000888 ) ) ;
#184007 = CARTESIAN_POINT ( 'NONE',  ( 3.490846471615864921, 2.117612208401131735, 0.4786232489656114253 ) ) ;
#184010 = CARTESIAN_POINT ( 'NONE',  ( 3.210337823311388394, 1.665856106666419034, 0.7845605768846477535 ) ) ;
#184009 = CARTESIAN_POINT ( 'NONE',  ( -3.945059511896602089, 7.546393830613923548, 1.040834085586084257E-14 ) ) ;
#184011 = CARTESIAN_POINT ( 'NONE',  ( -0.6823417656249969321, 3.467708333674754506, -1.181850606188749264 ) ) ;
#184012 = CARTESIAN_POINT ( 'NONE',  ( 4.124703146219878214, 0.1084699374758208573, 2.189010777610411740 ) ) ;
#184013 = CARTESIAN_POINT ( 'NONE',  ( 4.663087558633967511, -2.018941045467276929, -1.021363250454855764 ) ) ;
#184014 = CARTESIAN_POINT ( 'NONE',  ( -4.855791571988752331, 8.816840600628864877, 0.7998128361456481317 ) ) ;
#184015 = CARTESIAN_POINT ( 'NONE',  ( 4.601768607255383614, 8.481659704624913587, -0.1707596084408805059 ) ) ;
#184016 = CARTESIAN_POINT ( 'NONE',  ( -5.980555156959541208, 7.110307450275150210, 1.082531754730549078 ) ) ;
#184017 = CARTESIAN_POINT ( 'NONE',  ( 3.770576118376306241, 6.452737000530752276, 1.082531754730549078 ) ) ;
#184018 = CARTESIAN_POINT ( 'NONE',  ( 6.081276588353502710, 1.634447734625959825, -0.6791225938206167934 ) ) ;
#184019 = AXIS2_PLACEMENT_3D ( 'NONE', #132282, #200418, #119254 ) ;
#184020 = CARTESIAN_POINT ( 'NONE',  ( 6.771407655021410399, 9.987393799911945536, -1.199719254218441611 ) ) ;
#184021 = CARTESIAN_POINT ( 'NONE',  ( 1.835132634908468452, 0.2055991040930336133, 2.095883127255711464 ) ) ;
#184022 = CARTESIAN_POINT ( 'NONE',  ( 1.212342387966048651, 1.846533033048233463, 0.5095510818057205071 ) ) ;
#184023 = VECTOR ( 'NONE', #33868, 1000.000000000000000 ) ;
#184025 = CARTESIAN_POINT ( 'NONE',  ( -1.500000000000013101, 2.170833333333357373, 0.8660254037844403729 ) ) ;
#184024 = CARTESIAN_POINT ( 'NONE',  ( -1.402160292154681736E-14, 11.42187500034140157, 1.575800808251682339 ) ) ;
#184026 = CARTESIAN_POINT ( 'NONE',  ( 1.996483073472170133, 1.947676829468534265, 0.2919340086137369727 ) ) ;
#184027 = CARTESIAN_POINT ( 'NONE',  ( 1.111929834214450796, -0.8377583890188080584, -1.672643128629976772 ) ) ;
#184028 = CARTESIAN_POINT ( 'NONE',  ( 0.4847190467827041105, 1.876267867961832980, 0.5731238010058882226 ) ) ;
#184030 = ORIENTED_EDGE ( 'NONE', *, *, #138240, .T. ) ;
#184029 = CARTESIAN_POINT ( 'NONE',  ( 0.1406777020166137260, 1.830675540527426648, 0.5531436448603862521 ) ) ;
#184031 = CARTESIAN_POINT ( 'NONE',  ( 6.995644074971448134, 7.263932296995902149, -0.7216878364870257245 ) ) ;
#184032 = EDGE_CURVE ( 'NONE', #114840, #21185, #4845, .T. ) ;
#184033 = CARTESIAN_POINT ( 'NONE',  ( 1.364683531249986537, 0.9677083336747538400, -0.7879004041258239610 ) ) ;
#184034 = CARTESIAN_POINT ( 'NONE',  ( 6.385618529757402406, 1.291587659170100766, 1.353439767483602285 ) ) ;
#184035 = CARTESIAN_POINT ( 'NONE',  ( 1.123270288250308280, 2.860197346350005887, 0.7749999999993786304 ) ) ;
#184036 = CARTESIAN_POINT ( 'NONE',  ( 5.963751281166302043, -0.5086355806236466659, 2.006660534352236347 ) ) ;
#184037 = CARTESIAN_POINT ( 'NONE',  ( -3.755786496842897795E-14, 2.812499999999973355, 1.414508159514537455 ) ) ;
#184038 = CARTESIAN_POINT ( 'NONE',  ( -5.289089322662584358, 5.343228095960675716, 0.000000000000000000 ) ) ;
#184039 = SURFACE_STYLE_USAGE ( .BOTH. , #52979 ) ;
#184040 = CARTESIAN_POINT ( 'NONE',  ( 1.499999999999989120, 0.7750000000000187850, 0.000000000000000000 ) ) ;
#184041 = CARTESIAN_POINT ( 'NONE',  ( 8.372323551638698902, 9.726464550788689323, 1.199719254218462483 ) ) ;
#184042 = CARTESIAN_POINT ( 'NONE',  ( -10.01677656239806247, 10.58066083241955901, 0.7998128361456462443 ) ) ;
#184043 = CARTESIAN_POINT ( 'NONE',  ( 6.343235766347262938, 8.493804042195527870, -1.599625672291281386 ) ) ;
#184044 = CARTESIAN_POINT ( 'NONE',  ( -1.364683531250014514, 1.238541667008091096, -0.7879004041258289570 ) ) ;
#184045 = CARTESIAN_POINT ( 'NONE',  ( 1.499999999999989120, 3.025000000000020783, 1.214306433183764966E-14 ) ) ;
#184047 = CARTESIAN_POINT ( 'NONE',  ( 2.835626683552519012, 6.459981564119914310, 0.000000000000000000 ) ) ;
#184046 = CARTESIAN_POINT ( 'NONE',  ( 5.142999638377217408, -0.2383176028181442918, -1.947251298587366231 ) ) ;
#184048 = CARTESIAN_POINT ( 'NONE',  ( 3.075545897833771747, 1.462222457232667416, -1.388272539953112839 ) ) ;
#184049 = CARTESIAN_POINT ( 'NONE',  ( 2.290125521308879808, -0.7372973962519657753, -1.768360312244516841 ) ) ;
#184050 = EDGE_CURVE ( 'NONE', #157333, #166319, #185315, .T. ) ;
#184051 = CARTESIAN_POINT ( 'NONE',  ( 2.547265342226494947E-16, 0.08000000000000020983, -2.080000000000000071 ) ) ;
#184052 = CARTESIAN_POINT ( 'NONE',  ( 0.3983070667218471805, -0.7439898890007863308, -2.061537379893277677 ) ) ;
#184053 = CARTESIAN_POINT ( 'NONE',  ( 0.1333692844072767447, 1.351132181276387678, -2.308013766563504987 ) ) ;
#184054 = CARTESIAN_POINT ( 'NONE',  ( 3.075316773429651818, 1.777364689479765003, -0.5833007003755164011 ) ) ;
#184055 = CARTESIAN_POINT ( 'NONE',  ( -0.7500000000000249800, -0.5270833326505158789, 1.299038105676659116 ) ) ;
#184056 = ADVANCED_BREP_SHAPE_REPRESENTATION ( '', ( #88722, #200407 ), #3714 ) ;
#184057 = CARTESIAN_POINT ( 'NONE',  ( -8.694856585065634746, 9.038420858865048757, 0.7998128361456462443 ) ) ;
#184059 = CARTESIAN_POINT ( 'NONE',  ( 3.919616530476960126, -1.461442364795034976, -1.532149496301576486 ) ) ;
#184058 = CARTESIAN_POINT ( 'NONE',  ( -5.748293942514186128, 6.769059690097084747, -1.082531754730544860 ) ) ;
#184060 = DIRECTION ( 'NONE',  ( 1.000000000000000000, -0.000000000000000000, -0.000000000000000000 ) ) ;
#184061 = CARTESIAN_POINT ( 'NONE',  ( 6.391088794356012848, 0.1989163192229244648, 2.060770550043041993 ) ) ;
#184063 = CARTESIAN_POINT ( 'NONE',  ( 6.620655732516650183, -0.005281389526671976913, 2.273887028200880511 ) ) ;
#184062 = CARTESIAN_POINT ( 'NONE',  ( 1.241864343681793548, 2.088520813897582151, 0.09894013698169208670 ) ) ;
#184065 = ORIENTED_EDGE ( 'NONE', *, *, #9722, .T. ) ;
#184064 = CARTESIAN_POINT ( 'NONE',  ( 0.5160737793865723955, 1.194803229551535173, -1.244154219207161960 ) ) ;
#184066 = CARTESIAN_POINT ( 'NONE',  ( 6.805303039055573322, 10.02693841461847057, 1.199719254218460707 ) ) ;
#184068 = TOROIDAL_SURFACE ( 'NONE', #204774, 1.600000000000000311, 0.1000000000000000056 ) ;
#184067 = CARTESIAN_POINT ( 'NONE',  ( -0.08228926980218694009, -9.910743320677065427, -9.499643698783447832 ) ) ;
#184069 = CARTESIAN_POINT ( 'NONE',  ( -9.915825940873133959, 4.173851563286998356, 6.175246223022227809 ) ) ;
#184070 = CARTESIAN_POINT ( 'NONE',  ( 7.605760987142057061, 7.975735361194951523, -0.7216878364870267237 ) ) ;
#184071 = CARTESIAN_POINT ( 'NONE',  ( -1.896367326442750745, 3.293421909012280047, 0.4056650308922222781 ) ) ;
#184073 = CARTESIAN_POINT ( 'NONE',  ( 0.3986853379376364415, -0.2198743563824180347, -1.798016573952045283 ) ) ;
#184072 = CARTESIAN_POINT ( 'NONE',  ( 7.842465510862060896, 8.114240948952696542, 0.000000000000000000 ) ) ;
#184074 = CARTESIAN_POINT ( 'NONE',  ( -8.667740277838301921, 9.006785167099828016, -0.7998128361456291469 ) ) ;
#184075 = CARTESIAN_POINT ( 'NONE',  ( 4.650610384687404952, 5.384465856012134566, 1.199719254218462483 ) ) ;
#184076 = CARTESIAN_POINT ( 'NONE',  ( -5.116488771863230589, 7.819496687688390679, 1.149033069458482270 ) ) ;
#184077 = CARTESIAN_POINT ( 'NONE',  ( 5.851225812749518695, 8.984124660586543243, -1.199719254218452047 ) ) ;
#184078 = B_SPLINE_CURVE_WITH_KNOTS ( 'NONE', 3,
 ( #88598, #19296, #138414, #69100, #20364, #21415, #117945 ),
 .UNSPECIFIED., .F., .F.,
 ( 4, 3, 4 ),
 ( 0.000000000000000000, 2.617081137853276995E-05, 3.552777339496689108E-05 ),
 .UNSPECIFIED. ) ;
#184079 = CARTESIAN_POINT ( 'NONE',  ( 0.000000000000000000, 11.37999999999999901, 0.000000000000000000 ) ) ;
#184080 = CARTESIAN_POINT ( 'NONE',  ( 4.063008298707909027, 7.508743736771079647, -0.5217633019904341918 ) ) ;
#184081 = CARTESIAN_POINT ( 'NONE',  ( 9.734391104931951588, 11.41950637958454706, 1.082531754730548412 ) ) ;
#184082 = ORIENTED_EDGE ( 'NONE', *, *, #85262, .T. ) ;
#184083 = CARTESIAN_POINT ( 'NONE',  ( 6.275017575846199236, 1.753023089329442064, -0.9963169848806670004 ) ) ;
#184084 = CARTESIAN_POINT ( 'NONE',  ( 0.8738735914427526730, 0.4098651554323496926, -2.080331290949386513 ) ) ;
#184085 = CARTESIAN_POINT ( 'NONE',  ( -0.4800000000000000933, 2.999999999999999112, -2.420000000000000373 ) ) ;
#184086 = CIRCLE ( 'NONE', #80834, 7.426656976154414558 ) ;
#184087 = PLANE ( 'NONE',  #123121 ) ;
#184088 = CARTESIAN_POINT ( 'NONE',  ( -3.470524135418294520, 6.992769224722559684, -0.7216878364870267237 ) ) ;
#184089 = CARTESIAN_POINT ( 'NONE',  ( 9.002250809793993724, 11.52571191622492464, -1.443375672974057666 ) ) ;
#184090 = CARTESIAN_POINT ( 'NONE',  ( 3.520317136570957128, 0.8812775084000439296, 1.761307543597267822 ) ) ;
#184091 = CARTESIAN_POINT ( 'NONE',  ( 1.647299267346370444, 0.2110521635003380359, 2.109970702148834754 ) ) ;
#184092 = CARTESIAN_POINT ( 'NONE',  ( -5.392392409933270514, 7.314210449720692786, 1.599625672291269396 ) ) ;
#184093 = CARTESIAN_POINT ( 'NONE',  ( -11.29577547002741866, 7.647201583078615528, -3.921964478061291004 ) ) ;
#184094 = CARTESIAN_POINT ( 'NONE',  ( -5.398914348987512213, 6.259949555863199677, 2.420000000000001261 ) ) ;
#184095 = CARTESIAN_POINT ( 'NONE',  ( 5.666036703420031628, -1.392593631063457682, 1.692088878451535106 ) ) ;
#184096 = DIRECTION ( 'NONE',  ( -0.6483454320283799088, 0.000000000000000000, 0.7613463080411786432 ) ) ;
#184097 = CARTESIAN_POINT ( 'NONE',  ( 4.313445203237777470, -0.3300861979738233254, 1.897755268844825816 ) ) ;
#184098 = CARTESIAN_POINT ( 'NONE',  ( -6.821723845970312894, 11.11042825360738284, 0.000000000000000000 ) ) ;
#184099 = CARTESIAN_POINT ( 'NONE',  ( -0.1294898018152304819, 0.2484418290887774605, -1.961697698124951650 ) ) ;
#184100 = CARTESIAN_POINT ( 'NONE',  ( 1.225528936851564499, -0.05108506852482053856, 2.206457870188943016 ) ) ;
#184101 = CARTESIAN_POINT ( 'NONE',  ( -0.4417779905600746071, 7.383047307301207951, 2.041823008714554355 ) ) ;
#184102 = ORIENTED_EDGE ( 'NONE', *, *, #168972, .F. ) ;
#184103 = CARTESIAN_POINT ( 'NONE',  ( 4.475600106286968582, 5.354526557823810151, -1.082531754730548412 ) ) ;
#184104 = CARTESIAN_POINT ( 'NONE',  ( 6.719592862238788378, 0.3399973502477529608, -1.939713583613829728 ) ) ;
#184105 = CARTESIAN_POINT ( 'NONE',  ( 0.4681772292557941917, -1.829107974901639899, -0.6530565061142034056 ) ) ;
#184106 = CARTESIAN_POINT ( 'NONE',  ( 6.116662973727256869, 0.6756443950356945116, -2.196842021360578823 ) ) ;
#184108 = CARTESIAN_POINT ( 'NONE',  ( 4.170637490619288457, 1.318561355513592215, -1.313476238859044409 ) ) ;
#184107 = CARTESIAN_POINT ( 'NONE',  ( -7.944151662964566540, 8.232874793072271657, 0.000000000000000000 ) ) ;
#184109 = CARTESIAN_POINT ( 'NONE',  ( 7.361151057576892143, 7.552707420120024828, 0.7998128361456291469 ) ) ;
#184110 = DIRECTION ( 'NONE',  ( -0.01745240643728004568, 0.000000000000000000, -0.9998476951563913806 ) ) ;
#184111 =( NAMED_UNIT ( * ) PLANE_ANGLE_UNIT ( ) SI_UNIT ( $, .RADIAN. ) );
#184112 = CARTESIAN_POINT ( 'NONE',  ( -4.381256195510448315, 8.263215994737505454, 1.040834085586084257E-14 ) ) ;
#184113 = CARTESIAN_POINT ( 'NONE',  ( 6.720655732516650716, 2.984497329163855905, 2.280179935440066252 ) ) ;
#184114 = CARTESIAN_POINT ( 'NONE',  ( 6.585487052573138378, -0.8941505307449393314, 1.888277625537030380 ) ) ;
#184115 = CARTESIAN_POINT ( 'NONE',  ( 3.538314903486612817, 7.071858454135611538, 1.040834085586084257E-14 ) ) ;
#184116 = ORIENTED_EDGE ( 'NONE', *, *, #36292, .F. ) ;
#184117 = CIRCLE ( 'NONE', #90773, 0.08000000000000044575 ) ;
#184118 = CARTESIAN_POINT ( 'NONE',  ( -3.337985173046072340, 6.383183490859034137, 0.8077998227833966816 ) ) ;
#184119 =( NAMED_UNIT ( * ) SI_UNIT ( $, .STERADIAN. ) SOLID_ANGLE_UNIT ( ) );
#184120 = CARTESIAN_POINT ( 'NONE',  ( 0.6096330727367264002, -1.817201089070449971, 0.1759225495863714350 ) ) ;
#184121 = CARTESIAN_POINT ( 'NONE',  ( -3.978428010606240850, 6.728917548094202949, -1.199719254218452047 ) ) ;
#184122 = CARTESIAN_POINT ( 'NONE',  ( 2.074501327421875096, -0.7402772072304538709, 1.568325542203717227 ) ) ;
#184123 = DIRECTION ( 'NONE',  ( -2.126226658603517140E-31, 1.665334536937738015E-16, 1.000000000000000000 ) ) ;
#184124 = CARTESIAN_POINT ( 'NONE',  ( -3.960390268523300339, 7.634556056670224855, 1.214306433183764966E-14 ) ) ;
#184125 = CARTESIAN_POINT ( 'NONE',  ( 6.322862864304120478, 1.705426906915354035, 0.6521430802832667295 ) ) ;
#184126 = CARTESIAN_POINT ( 'NONE',  ( 3.397265449134680981, -1.732261247800225279, 0.9206733083975682241 ) ) ;
#184127 = CARTESIAN_POINT ( 'NONE',  ( 1.224999999999988320, -0.06249999931720595647, -6.938893903907228378E-15 ) ) ;
#184128 = CARTESIAN_POINT ( 'NONE',  ( -9.501566725078754772, 9.979582688880366703, -0.7998128361456291469 ) ) ;
#184129 = CARTESIAN_POINT ( 'NONE',  ( 7.474622759835693131, 7.614814729430110951, -0.7998128361456281477 ) ) ;
#184130 = CARTESIAN_POINT ( 'NONE',  ( 4.811248821985151913, 1.762591750878339081, -1.178568461981117643 ) ) ;
#184131 = CARTESIAN_POINT ( 'NONE',  ( 6.912678218121202534, 9.158153569265168770, 1.599625672291268286 ) ) ;
#184132 = CARTESIAN_POINT ( 'NONE',  ( -9.972185678051314284, 11.59297036493672017, 1.199719254218462483 ) ) ;
#184133 = CARTESIAN_POINT ( 'NONE',  ( 2.764580022184208730, -0.7881864689132519475, -1.914544693583389634 ) ) ;
#184135 = CARTESIAN_POINT ( 'NONE',  ( 0.6823417656249882723, -0.2614583329919109578, -1.181850606188749264 ) ) ;
#184134 = CARTESIAN_POINT ( 'NONE',  ( 6.827182134110196365, 4.700652535171166768, 2.373648650996477372 ) ) ;
#184137 = ORIENTED_EDGE ( 'NONE', *, *, #176248, .T. ) ;
#184136 = CARTESIAN_POINT ( 'NONE',  ( 4.881579437514656838, 0.2187098293420664807, -2.210487333941961285 ) ) ;
#184138 = CARTESIAN_POINT ( 'NONE',  ( 2.725512391864647999, 2.281683302435618010, 0.2785734649361614745 ) ) ;
#184139 = CARTESIAN_POINT ( 'NONE',  ( 8.026063749610047537, 10.38682701267698150, -1.443375672974057666 ) ) ;
#184141 = CARTESIAN_POINT ( 'NONE',  ( -3.285556943750000514, -2.238541666188709200, -1.896917185911906500 ) ) ;
#184140 = CARTESIAN_POINT ( 'NONE',  ( 6.536439455564155843, 8.719208346281938304, 1.443375672974065660 ) ) ;
#184142 = ADVANCED_FACE ( 'NONE', ( #8465 ), #13334, .T. ) ;
#184143 = FACE_OUTER_BOUND ( 'NONE', #15712, .T. ) ;
#184144 = CARTESIAN_POINT ( 'NONE',  ( -10.47222688565958926, 3.889612458557746510, 5.860485223248574016 ) ) ;
#184145 = LINE ( 'NONE', #67180, #115148 ) ;
#184146 = CARTESIAN_POINT ( 'NONE',  ( 4.183787391381143195, 1.853651273288700718, -0.4697857328580385960 ) ) ;
#184147 = CARTESIAN_POINT ( 'NONE',  ( -11.84100621633422179, 13.61041574223336248, -1.444132586618106728 ) ) ;
#184148 = CARTESIAN_POINT ( 'NONE',  ( 4.418794198169028853, 1.577559062085803765, 0.6976772398503274797 ) ) ;
#184149 = CARTESIAN_POINT ( 'NONE',  ( 3.450407915430803385, -1.350735839785843773, 1.497501794165828626 ) ) ;
#184150 =( BOUNDED_SURFACE ( )  B_SPLINE_SURFACE ( 3, 2, ( 
 ( #128071, #180977, #111794 ),
 ( #96568, #13142, #98674 ),
 ( #145337, #177799, #28337 ),
 ( #29416, #211338, #147431 ),
 ( #64039, #94434, #130184 ),
 ( #196177, #47819, #179926 ) ),
 .UNSPECIFIED., .F., .F., .F. ) 
 B_SPLINE_SURFACE_WITH_KNOTS ( ( 4, 2, 4 ),
 ( 3, 3 ),
 ( 0.000000000000000000, 0.0003831327362561326704, 0.0007662654725122653408 ),
 ( 0.000000000000000000, 1.000000000000000000 ),
 .UNSPECIFIED. ) 
 GEOMETRIC_REPRESENTATION_ITEM ( )  RATIONAL_B_SPLINE_SURFACE ( (
 ( 1.000000000000000000, 0.5879095031487664436, 1.000000000000000000),
 ( 1.000000000000000000, 0.5873691247578739505, 1.000000000000000000),
 ( 1.000000000000000000, 0.6054349545497327290, 1.000000000000000000),
 ( 1.000000000000000000, 0.6533334602766750487, 1.000000000000000000),
 ( 1.000000000000000000, 0.6828746263150841100, 1.000000000000000000),
 ( 1.000000000000000000, 0.7071067811865475727, 1.000000000000000000) ) ) 
 REPRESENTATION_ITEM ( '' )  SURFACE ( )  );
#184151 = CARTESIAN_POINT ( 'NONE',  ( 4.184446765594143081, 1.846410498051667348, 1.369081834291352218 ) ) ;
#184152 = CARTESIAN_POINT ( 'NONE',  ( -11.52483635780544624, 12.22000008642464941, -3.345866325258089358 ) ) ;
#184153 = CARTESIAN_POINT ( 'NONE',  ( 0.08304785351339466493, -2.141800023564765620, -0.5316218738360134477 ) ) ;
#184154 = CARTESIAN_POINT ( 'NONE',  ( -5.234856708652269042, 7.200695141551334721, 1.443375672974058777 ) ) ;
#184155 = VERTEX_POINT ( 'NONE', #14849 ) ;
#184156 = CARTESIAN_POINT ( 'NONE',  ( 5.167173303313960631, 0.1731176489731758861, -1.761265287352784314 ) ) ;
#184157 = ADVANCED_FACE ( 'NONE', ( #18044 ), #177769, .T. ) ;
#184159 = CARTESIAN_POINT ( 'NONE',  ( 0.8324521645294904459, 2.259258938120102922, 0.3867697638584958186 ) ) ;
#184158 = CARTESIAN_POINT ( 'NONE',  ( 5.363132282657546490, 8.414682208812571673, -1.199719254218452047 ) ) ;
#184160 = CARTESIAN_POINT ( 'NONE',  ( 6.456982894382444549, 0.3095715517048603371, -1.814770079682447967 ) ) ;
#184161 = CARTESIAN_POINT ( 'NONE',  ( 0.6499422464084809725, 4.349924920312916221, -0.06926476342541491860 ) ) ;
#184162 = CARTESIAN_POINT ( 'NONE',  ( 6.720655732516647163, -0.004400176169771369272, 2.173773060281408931 ) ) ;
#184163 = CARTESIAN_POINT ( 'NONE',  ( -2.979759899953417612, 6.698413326579433225, 0.7998128361456352531 ) ) ;
#184164 = CARTESIAN_POINT ( 'NONE',  ( -0.6801582343750265380, -0.2864583329919220822, 1.178068619123820771 ) ) ;
#184165 = FACE_OUTER_BOUND ( 'NONE', #197287, .T. ) ;
#184166 = CARTESIAN_POINT ( 'NONE',  ( 0.4499840099862363330, 1.609255455985519445, 1.457649523623653298 ) ) ;
#184167 = CARTESIAN_POINT ( 'NONE',  ( 1.446500318503377125, -1.422605717829699801, 1.429450658469958668 ) ) ;
#184168 = CIRCLE ( 'NONE', #97787, 0.09999999999999982514 ) ;
#184169 = CARTESIAN_POINT ( 'NONE',  ( 1.499999999999985123, -0.4229166659838508036, -0.8660254037844323793 ) ) ;
#184170 = CARTESIAN_POINT ( 'NONE',  ( 5.795520199677122619, 1.460474902364042649, 1.256451531516086684 ) ) ;
#184171 = CARTESIAN_POINT ( 'NONE',  ( -0.6823417656250003738, 11.90104166700806054, 1.181850606188754593 ) ) ;
#184172 = CARTESIAN_POINT ( 'NONE',  ( 1.020144049103311801, -0.5328101295089396894, 2.156480530197317780 ) ) ;
#184173 = ORIENTED_EDGE ( 'NONE', *, *, #162394, .T. ) ;
#184176 = COLOUR_RGB ( '', 0.72549020, 0.75294118, 0.79215686) ;
#184175 = CARTESIAN_POINT ( 'NONE',  ( 0.4206437366318451221, 7.996079560418730026, -1.998769755887081834 ) ) ;
#184174 =( NAMED_UNIT ( * ) SI_UNIT ( $, .STERADIAN. ) SOLID_ANGLE_UNIT ( ) );
#184177 = CARTESIAN_POINT ( 'NONE',  ( -0.1128749944181871995, 2.519999999999980034, -2.000000000000003553 ) ) ;
#184178 = CARTESIAN_POINT ( 'NONE',  ( 8.106885785967500979, 11.54545161934907682, 1.199719254218460707 ) ) ;
#184179 =( LENGTH_UNIT ( ) NAMED_UNIT ( * ) SI_UNIT ( .MILLI., .METRE. ) );
#184180 = CARTESIAN_POINT ( 'NONE',  ( 4.458407330353141518, -1.557363759602323761, -0.7771466779550126880 ) ) ;
#184181 = CARTESIAN_POINT ( 'NONE',  ( 2.787496613063783713, -1.831585881375777713, 0.7034878451678548972 ) ) ;
#184183 = CARTESIAN_POINT ( 'NONE',  ( 1.364683531249990311, 2.696875000341415696, 1.214306433183764966E-14 ) ) ;
#184182 = CARTESIAN_POINT ( 'NONE',  ( 3.985207087413062066, 6.736826471035503694, -1.199719254218452047 ) ) ;
#184184 = CARTESIAN_POINT ( 'NONE',  ( -5.889415777131212337, 6.013640170854067435, 0.2549476635474844932 ) ) ;
#184185 = CARTESIAN_POINT ( 'NONE',  ( 0.9419289695592079070, 1.383825781391546883, 1.529776408950918265 ) ) ;
#184186 = CARTESIAN_POINT ( 'NONE',  ( -7.965578943228732278, 9.251929174310385307, -1.199719254218446718 ) ) ;
#184187 = EDGE_CURVE ( 'NONE', #80885, #209385, #164324, .T. ) ;
#184188 = CARTESIAN_POINT ( 'NONE',  ( -3.592547517496935683, 6.174760622846296343, -1.082531754730548412 ) ) ;
#184189 = CARTESIAN_POINT ( 'NONE',  ( 1.358695222972395422, 0.9186288065576648787, 2.067797507578944760 ) ) ;
#184190 = VERTEX_POINT ( 'NONE', #84131 ) ;
#184191 = CARTESIAN_POINT ( 'NONE',  ( -0.7500000000000249800, -0.2770833326505156569, 1.299038105676659116 ) ) ;
#184192 = CARTESIAN_POINT ( 'NONE',  ( 2.055717040066493695, 1.865871300129381183, -0.1328275987748789300 ) ) ;
#184193 = CARTESIAN_POINT ( 'NONE',  ( 0.9845302160453218709, -1.734343004718540637, -0.001328871039332768294 ) ) ;
#184194 = CARTESIAN_POINT ( 'NONE',  ( 5.618738332679400038, -0.05485954975367920983, 2.191026952110195491 ) ) ;
#184195 = CARTESIAN_POINT ( 'NONE',  ( 5.315557996638371918, -0.3450676865139382099, 2.281540517825955128 ) ) ;
#184196 = CARTESIAN_POINT ( 'NONE',  ( 1.006794875882726314, 1.561001636543899673, -1.345678083183374341 ) ) ;
#184197 = CARTESIAN_POINT ( 'NONE',  ( 3.433474178283620670, 0.8725410082476585671, -1.734956227438133158 ) ) ;
#184198 = CARTESIAN_POINT ( 'NONE',  ( -5.246642258364192735, 5.223430177620739023, 0.7216878364870317197 ) ) ;
#184199 = CARTESIAN_POINT ( 'NONE',  ( 5.835183367072669824, -1.691281831231405963, 0.7993005984755219284 ) ) ;
#184200 = CARTESIAN_POINT ( 'NONE',  ( 4.003835517601626925, 7.590433450137844318, -0.2001945245787856709 ) ) ;
#184201 = CARTESIAN_POINT ( 'NONE',  ( 6.661482485103542572, -0.5350097378542042481, -1.943772860543022230 ) ) ;
#184202 = CARTESIAN_POINT ( 'NONE',  ( 0.6801582343749796866, 1.473958333674751930, 1.178068619123789462 ) ) ;
#184203 = CARTESIAN_POINT ( 'NONE',  ( 4.992814645674492624, -2.006446365708704160, 0.2004330516618065550 ) ) ;
#184204 = CARTESIAN_POINT ( 'NONE',  ( -2.914639836813632812, 6.344237543017112735, 0.7216878364870317197 ) ) ;
#184205 = CARTESIAN_POINT ( 'NONE',  ( 7.574201371528760163, 11.98831870009225931, 1.040834085586084257E-14 ) ) ;
#184206 = CARTESIAN_POINT ( 'NONE',  ( 4.686278372178935392, 5.496354851410763409, 1.199719254218452047 ) ) ;
#184208 = CARTESIAN_POINT ( 'NONE',  ( -7.057683771862373945, -6.583723166013941253, 6.531918710723850552 ) ) ;
#184207 = CARTESIAN_POINT ( 'NONE',  ( 1.963248404482214049, 0.3131683437365209710, -1.798463397695612809 ) ) ;
#184209 = CARTESIAN_POINT ( 'NONE',  ( -4.716257332707368910, 6.595662536282280719, -1.599625672291271394 ) ) ;
#184210 = CARTESIAN_POINT ( 'NONE',  ( -15.75000000000000000, 12.69999999999999929, -1.100000000000000311 ) ) ;
#184211 = CARTESIAN_POINT ( 'NONE',  ( -7.460470246983022413, -6.805008568744149500, -7.900729602272508423 ) ) ;
#184212 = VERTEX_POINT ( 'NONE', #149131 ) ;
#184213 = CARTESIAN_POINT ( 'NONE',  ( -4.611181641979265500, 8.393812659035525314, 0.000000000000000000 ) ) ;
#184214 = DIRECTION ( 'NONE',  ( 0.000000000000000000, 0.000000000000000000, -1.000000000000000000 ) ) ;
#184215 = CARTESIAN_POINT ( 'NONE',  ( -9.318531651294266638, 9.766041769465124034, -0.7998128361456291469 ) ) ;
#184216 = CARTESIAN_POINT ( 'NONE',  ( 5.180334445267184229, 0.9972254788270168424, 1.756242667785257172 ) ) ;
#184217 = CARTESIAN_POINT ( 'NONE',  ( 0.4871770963560326240, -1.998059126451703138, -0.7104936405118513765 ) ) ;
#184218 = CARTESIAN_POINT ( 'NONE',  ( -7.110325215724114578, 7.260077271291732082, 0.000000000000000000 ) ) ;
#184219 = AXIS2_PLACEMENT_3D ( 'NONE', #81285, #147361, #213388 ) ;
#184220 = CARTESIAN_POINT ( 'NONE',  ( 3.818592820543298405, 7.606775390609172405, -0.7998128361456221525 ) ) ;
#184221 = CARTESIAN_POINT ( 'NONE',  ( 4.768464766973178115, -1.347833537202504317, 1.559116658007191347 ) ) ;
#184222 = CARTESIAN_POINT ( 'NONE',  ( 5.080704010962952211, -0.7231418808758652839, 1.882473355234378865 ) ) ;
#184223 = ORIENTED_EDGE ( 'NONE', *, *, #198065, .T. ) ;
#184224 = CARTESIAN_POINT ( 'NONE',  ( 10.59754597632703899, 11.29999999999999893, -3.303592501912006263 ) ) ;
#184225 = CARTESIAN_POINT ( 'NONE',  ( 2.544126380858701797, 6.119897877643793116, 0.7998128361456462443 ) ) ;
#184227 = ORIENTED_EDGE ( 'NONE', *, *, #122849, .T. ) ;
#184226 = CARTESIAN_POINT ( 'NONE',  ( -5.094831863685302942, 9.165997284266655498, 0.7998128361456291469 ) ) ;
#184228 = CARTESIAN_POINT ( 'NONE',  ( 4.597876849858236525, 8.486543085689454813, -0.1053875944492469602 ) ) ;
#184229 = CARTESIAN_POINT ( 'NONE',  ( 5.571638683613604037, 1.528505562557905595, -1.314797328242120367 ) ) ;
#184230 = CARTESIAN_POINT ( 'NONE',  ( 4.013478867934616723, -0.9481684062532383939, -1.578073411074693899 ) ) ;
#184231 = DIRECTION ( 'NONE',  ( 0.000000000000000000, 0.000000000000000000, -1.000000000000000000 ) ) ;
#184232 = CARTESIAN_POINT ( 'NONE',  ( 1.788135723919834774, 1.593634496655076171, 1.669289477041531633 ) ) ;
#184233 = CARTESIAN_POINT ( 'NONE',  ( 6.749980374757213575, 8.968339418673846097, 1.599625672291268286 ) ) ;
#184234 = CARTESIAN_POINT ( 'NONE',  ( 4.833375328034618335, -1.978455579520097762, 0.8711445904842631816 ) ) ;
#184235 = CARTESIAN_POINT ( 'NONE',  ( 7.425061681778431399, 11.81432239538354345, 0.7998128361456462443 ) ) ;
#184236 = CARTESIAN_POINT ( 'NONE',  ( 0.5033352851749985923, -1.932590057610440226, 0.1917435184634954937 ) ) ;
#184237 = CARTESIAN_POINT ( 'NONE',  ( -3.737243898861318137, 7.511868315313511069, 0.7998128361456341429 ) ) ;
#184238 = CARTESIAN_POINT ( 'NONE',  ( 3.831692444270826226, -1.546495240224911250, 1.700404426133800939 ) ) ;
#184239 = CARTESIAN_POINT ( 'NONE',  ( 11.88237951145550220, 9.843193473787149372, 0.9087114598430685586 ) ) ;
#184240 = CARTESIAN_POINT ( 'NONE',  ( -6.143779885648060102, 7.196773283791382703, 1.199719254218452047 ) ) ;
#184241 = AXIS2_PLACEMENT_3D ( 'NONE', #57203, #173101, #9515 ) ;
#184242 = CARTESIAN_POINT ( 'NONE',  ( 3.643291952642300213, -1.415932857957047375, -1.222571138756740838 ) ) ;
#184243 = VECTOR ( 'NONE', #101966, 1000.000000000000000 ) ;
#184245 = CARTESIAN_POINT ( 'NONE',  ( -6.882699257592852504, 8.058845884393651460, -1.199719254218452047 ) ) ;
#184244 = CARTESIAN_POINT ( 'NONE',  ( 0.6823417656249899377, 5.426041667008087543, -1.181850606188754593 ) ) ;
#184246 = CARTESIAN_POINT ( 'NONE',  ( 1.383733252933561086, 2.037972573443189717, -0.8472329510355591786 ) ) ;
#184247 = CARTESIAN_POINT ( 'NONE',  ( -11.97181073603049661, 9.719999999999998863, 0.8318477717169566743 ) ) ;
#184248 = CARTESIAN_POINT ( 'NONE',  ( 3.506755287428983792, 7.242964935309132990, 1.040834085586084257E-14 ) ) ;
#184249 = CARTESIAN_POINT ( 'NONE',  ( -4.623494077460110319, 5.352830164246910272, 1.199719254218462483 ) ) ;
#184250 = CARTESIAN_POINT ( 'NONE',  ( -7.607533590599451223, 9.008448956188397361, 1.082531754730549078 ) ) ;
#184251 = CARTESIAN_POINT ( 'NONE',  ( 6.819227947992137828, -0.1355634432321853045, 1.940828160714276995 ) ) ;
#184252 = CARTESIAN_POINT ( 'NONE',  ( 0.3062966595402705217, -0.6107984557060777142, 2.225206381879496487 ) ) ;
#184253 = CARTESIAN_POINT ( 'NONE',  ( 0.9944974185457016169, 1.932217576897478528, 0.3389098420027157332 ) ) ;
#184254 = CARTESIAN_POINT ( 'NONE',  ( 4.030177592043080459, 1.141696479982070578, 1.717582018908659025 ) ) ;
#184255 = CARTESIAN_POINT ( 'NONE',  ( 5.992340707560160240, 7.053780915984068756, 1.082531754730558626 ) ) ;
#184256 = PRESENTATION_LAYER_ASSIGNMENT (  '', '', ( #73555 ) ) ;
#184257 = CARTESIAN_POINT ( 'NONE',  ( 5.722423353419669567, 8.833855124701747386, 1.199719254218451159 ) ) ;
#184258 = VERTEX_POINT ( 'NONE', #115624 ) ;
#184259 = CARTESIAN_POINT ( 'NONE',  ( 8.242994206984347372, 8.719174117677642499, 1.040834085586084257E-14 ) ) ;
#184260 = CARTESIAN_POINT ( 'NONE',  ( -1.201851678989727383E-14, 4.134375000341417028, 1.575800808251672791 ) ) ;
#184261 = CARTESIAN_POINT ( 'NONE',  ( 10.95308175811721085, 9.799999999999982947, 1.799999999999999600 ) ) ;
#184262 = CARTESIAN_POINT ( 'NONE',  ( 3.673896439178923057, 5.309298483840612093, 1.443375672974066548 ) ) ;
#184263 = CARTESIAN_POINT ( 'NONE',  ( 6.689883316565048865, -1.412897867115006978, -1.648663827357793155 ) ) ;
#184265 = CARTESIAN_POINT ( 'NONE',  ( 5.970224376651540155, -1.750504005202535796, -0.5711807346103907612 ) ) ;
#184264 = CARTESIAN_POINT ( 'NONE',  ( 1.499999999999990896, 4.806250000682819490, 1.214306433183764966E-14 ) ) ;
#184266 = CARTESIAN_POINT ( 'NONE',  ( 1.214306433183764966E-14, 2.428612866367529932E-14, 1.500000000000001332 ) ) ;
#184267 = CARTESIAN_POINT ( 'NONE',  ( -11.81911962874442068, 12.34289426515883648, -1.591749704452499303 ) ) ;
#184268 = CARTESIAN_POINT ( 'NONE',  ( 0.8955150854165813135, -0.6789544621725839280, 1.743152336062703256 ) ) ;
#184270 = CARTESIAN_POINT ( 'NONE',  ( -5.710256234166866562, 6.271970132040741497, 1.104226958479601173 ) ) ;
#184269 = CIRCLE ( 'NONE', #101243, 11.99999999999999112 ) ;
#184271 = CYLINDRICAL_SURFACE ( 'NONE', #175996, 3.150000000000000799 ) ;
#184272 = CARTESIAN_POINT ( 'NONE',  ( 5.120401779693986910, 7.917229619699595489, -1.217862772375446712 ) ) ;
#184273 = CARTESIAN_POINT ( 'NONE',  ( -1.364683531250010295, 5.301041667008085767, -0.7879004041258300672 ) ) ;
#184274 = CARTESIAN_POINT ( 'NONE',  ( 1.225099565173026761, 1.686864977381890451, 0.9006792851762451813 ) ) ;
#184275 = CARTESIAN_POINT ( 'NONE',  ( 3.484973364136711549, 1.600408865665205571, -0.7559459569618111052 ) ) ;
#184276 = CARTESIAN_POINT ( 'NONE',  ( 0.9614044138335111622, -1.507904615609249488, -1.175938229252027956 ) ) ;
#184278 = CARTESIAN_POINT ( 'NONE',  ( 4.605048111083247520, -0.08973289204975383460, 1.913620015931324581 ) ) ;
#184277 = CARTESIAN_POINT ( 'NONE',  ( -8.631737353394710155, 13.22211067893587533, 1.040834085586084257E-14 ) ) ;
#184279 = DIRECTION ( 'NONE',  ( -0.6483454320283799088, 0.000000000000000000, 0.7613463080411786432 ) ) ;
#184280 = CARTESIAN_POINT ( 'NONE',  ( 5.037540015474098354, 1.838441386810828693, -0.7070908002782918533 ) ) ;
#184281 = CARTESIAN_POINT ( 'NONE',  ( 0.7387272492362946252, 1.258454933865692293, -1.706699550108881080 ) ) ;
#184282 = CYLINDRICAL_SURFACE ( 'NONE', #34157, 0.08000000000000020983 ) ;
#184283 = CARTESIAN_POINT ( 'NONE',  ( 3.643291952642300213, -1.415932857957047375, -1.222571138756740838 ) ) ;
#184285 = ORIENTED_EDGE ( 'NONE', *, *, #6013, .T. ) ;
#184284 = CARTESIAN_POINT ( 'NONE',  ( 5.795441377679017236, 1.310440327830458385, 1.121692192092491380 ) ) ;
#184287 = CARTESIAN_POINT ( 'NONE',  ( 2.846849069189655967, 5.304779099821139710, -1.082531754730543083 ) ) ;
#184286 = CARTESIAN_POINT ( 'NONE',  ( 3.598431038176507002, -2.204323482753521635, -0.1086902067785888437 ) ) ;
#184288 = EDGE_CURVE ( 'NONE', #57016, #25036, #24948, .T. ) ;
#184289 = CARTESIAN_POINT ( 'NONE',  ( -0.6823417656250212460, 5.113541667008086655, 1.181850606188767472 ) ) ;
#184290 = CARTESIAN_POINT ( 'NONE',  ( 0.3794369086736723018, -0.1030016517138358095, 2.060237976199934984 ) ) ;
#184291 = CARTESIAN_POINT ( 'NONE',  ( 5.452350330990040739, 9.512825819463730070, 0.7998128361456462443 ) ) ;
#184292 = CARTESIAN_POINT ( 'NONE',  ( -7.980945979938748103, 12.46285407657057220, 0.000000000000000000 ) ) ;
#184293 = CARTESIAN_POINT ( 'NONE',  ( -9.043854491631282855, 2.018041202053908023, -8.143123160305936636 ) ) ;
#184294 = CARTESIAN_POINT ( 'NONE',  ( -3.423294271397314681, -0.02146400342267793318, -0.4188604460931010243 ) ) ;
#184295 = LINE ( 'NONE', #39132, #23301 ) ;
#184296 = ORIENTED_EDGE ( 'NONE', *, *, #147140, .F. ) ;
#184297 = CARTESIAN_POINT ( 'NONE',  ( 3.596198176508007105, 0.9334358170956689182, -1.848091447891623051 ) ) ;
#184298 = CARTESIAN_POINT ( 'NONE',  ( -0.7499999999999972244, 4.358333333333352932, -1.299038105676652011 ) ) ;
#184299 = CARTESIAN_POINT ( 'NONE',  ( 1.985828983967323325, 1.489073237690191398, 1.567133960648489976 ) ) ;
#184300 = CARTESIAN_POINT ( 'NONE',  ( -6.155278136343885542, 7.070130543739276519, 1.092798041965221900 ) ) ;
#184301 = CARTESIAN_POINT ( 'NONE',  ( 1.137374441040917672, -0.04723908312853628000, 2.019287564836816262 ) ) ;
#184302 = CARTESIAN_POINT ( 'NONE',  ( -1.665334536937735057E-16, -0.5000000000000004441, 3.000000000000010214 ) ) ;
#184303 = EDGE_LOOP ( 'NONE', ( #169297, #114874, #83957, #68241 ) ) ;
#184305 = CARTESIAN_POINT ( 'NONE',  ( 7.402388683381404988, 10.61957531637824204, -1.082531754730537976 ) ) ;
#184304 = CARTESIAN_POINT ( 'NONE',  ( 0.1747926744264452492, 5.725295659261265158, -2.449351454080525681 ) ) ;
#184306 = CARTESIAN_POINT ( 'NONE',  ( 6.591172692507557329, 1.163088239368128995, -1.646588791553056152 ) ) ;
#184307 = CARTESIAN_POINT ( 'NONE',  ( 6.139839150192680783, 1.910077931696544384, -0.1482136438759658337 ) ) ;
#184308 = CARTESIAN_POINT ( 'NONE',  ( 6.639320575229256782, 3.683803431435454190, 2.717262547424610375 ) ) ;
#184309 = CARTESIAN_POINT ( 'NONE',  ( 3.597391730528697540, -0.6346259394694170330, 2.097678010650514402 ) ) ;
#184310 = CARTESIAN_POINT ( 'NONE',  ( 0.7499999999999902300, 3.764583334016149863, 1.299038105676669330 ) ) ;
#184311 = CARTESIAN_POINT ( 'NONE',  ( 3.006014587165442453, -0.7710369221427433306, 1.750240277048662030 ) ) ;
#184312 = CARTESIAN_POINT ( 'NONE',  ( -4.391951695823077984, 7.211361847513815704, 1.199719254218464037 ) ) ;
#184313 = CARTESIAN_POINT ( 'NONE',  ( 4.663641652976547647, 4.543262804668490418, 1.214306433183764966E-14 ) ) ;
#184315 = CARTESIAN_POINT ( 'NONE',  ( 1.282827611874960416, 1.646826022920354848, -1.163289555428485667 ) ) ;
#184314 = CARTESIAN_POINT ( 'NONE',  ( -9.937763408692596556, 11.65677406730528887, -1.082531754730537976 ) ) ;
#184316 = CARTESIAN_POINT ( 'NONE',  ( -1.364683531250010295, 10.69270833367473372, 0.7879004041258445001 ) ) ;
#184318 = CARTESIAN_POINT ( 'NONE',  ( -5.981082042284069367, 7.006959133200059142, 1.199719254218452935 ) ) ;
#184317 = CARTESIAN_POINT ( 'NONE',  ( 0.4688447829373428855, -2.161134926827886549, -0.7649225765839831048 ) ) ;
#184320 = ORIENTED_EDGE ( 'NONE', *, *, #45609, .T. ) ;
#184319 = CARTESIAN_POINT ( 'NONE',  ( 3.803458131734431813, -0.5007765277059565978, 1.650448229862747196 ) ) ;
#184321 = CARTESIAN_POINT ( 'NONE',  ( 0.1394461523057474728, 0.7845381482947767493, -1.808261586923729736 ) ) ;
#184322 = CARTESIAN_POINT ( 'NONE',  ( 8.633844893804129228, 8.967240552393299424, -0.7998128361456211532 ) ) ;
#184323 = CARTESIAN_POINT ( 'NONE',  ( 4.033714395265605823, 4.664753868353354704, -1.199719254218446718 ) ) ;
#184324 = CARTESIAN_POINT ( 'NONE',  ( -1.177110729581199999, 2.960371626218858410, -0.7749999999999944711 ) ) ;
#184325 = CARTESIAN_POINT ( 'NONE',  ( 1.398799877119625501, 0.3793605821263335565, 1.924665094374561791 ) ) ;
#184326 = CARTESIAN_POINT ( 'NONE',  ( 11.33772467203874612, 10.09267152018149361, -3.600000000000000977 ) ) ;
#184327 = CARTESIAN_POINT ( 'NONE',  ( 3.981290663907289140, 7.796589541200495965, -0.7998128361456221525 ) ) ;
#184328 = CARTESIAN_POINT ( 'NONE',  ( 0.07536363704235481131, 0.6997989235110781969, -2.226667633679416447 ) ) ;
#184329 = VERTEX_POINT ( 'NONE', #162204 ) ;
#184331 = COLOUR_RGB ( '', 0.09019608, 0.27058824, 0.51372549) ;
#184330 = SURFACE_STYLE_FILL_AREA ( #150799 ) ;
#184332 = ORIENTED_EDGE ( 'NONE', *, *, #118861, .F. ) ;
#184333 = CARTESIAN_POINT ( 'NONE',  ( 4.002463340116116264, -1.792309675113772371, -0.2618007260343068743 ) ) ;
#184334 = VERTEX_POINT ( 'NONE', #13791 ) ;
#184336 = CARTESIAN_POINT ( 'NONE',  ( 4.694866332082116678, 8.699370830729650450, 0.7998128361456341429 ) ) ;
#184335 = VECTOR ( 'NONE', #18848, 1000.000000000000000 ) ;
#184338 = EDGE_CURVE ( 'NONE', #179385, #16492, #179953, .T. ) ;
#184337 = DIRECTION ( 'NONE',  ( 1.779758311459930245E-16, 0.000000000000000000, -1.000000000000000000 ) ) ;
#184339 = CARTESIAN_POINT ( 'NONE',  ( 5.268131585227527225, 1.809134041791292002, -0.09470131462574123138 ) ) ;
#184340 = CARTESIAN_POINT ( 'NONE',  ( 5.844973620822835336, 7.912498205750389424, 1.443375672974064550 ) ) ;
#184341 = CARTESIAN_POINT ( 'NONE',  ( 2.275391796764376640, 5.643962577969389827, -0.5307291018262025872 ) ) ;
#184342 = CARTESIAN_POINT ( 'NONE',  ( 5.328689024754546644, 6.340921230984883472, -1.104828203510083373 ) ) ;
#184344 = CARTESIAN_POINT ( 'NONE',  ( 8.055515824813896941, 12.54985222892493368, 0.7998128361456462443 ) ) ;
#184343 = CARTESIAN_POINT ( 'NONE',  ( 6.285601362909060796, -1.752004058920811902, 0.6281230767469258014 ) ) ;
#184345 = CARTESIAN_POINT ( 'NONE',  ( 4.358935675595962955, -0.003970376728411328937, -1.915793142021319007 ) ) ;
#184346 = CARTESIAN_POINT ( 'NONE',  ( -6.326802395788107880, 6.950450678040672514, 0.9045734915664763731 ) ) ;
#184347 = CARTESIAN_POINT ( 'NONE',  ( -11.91006458477769314, 5.204012295529565790, -4.700227299318338936 ) ) ;
#184348 = ADVANCED_FACE ( 'NONE', ( #170715, #21234 ), #88412, .T. ) ;
#184349 = DIRECTION ( 'NONE',  ( 0.9632918427306595976, 0.000000000000000000, 0.2684563758389253985 ) ) ;
#184350 =( NAMED_UNIT ( * ) SI_UNIT ( $, .STERADIAN. ) SOLID_ANGLE_UNIT ( ) );
#184351 = CARTESIAN_POINT ( 'NONE',  ( 6.317736394288135493, 8.393778431468064127, 1.443375672974076540 ) ) ;
#184352 = CARTESIAN_POINT ( 'NONE',  ( -9.083599731475995753, 11.62061899152058686, 1.443375672974064550 ) ) ;
#184353 = CARTESIAN_POINT ( 'NONE',  ( 1.129994055010040022, -1.371941552271437770, -1.670562328977095445 ) ) ;
#184354 = CARTESIAN_POINT ( 'NONE',  ( -4.111865726694519552, 8.019203457777400956, 0.000000000000000000 ) ) ;
#184355 = CARTESIAN_POINT ( 'NONE',  ( 4.746236293235721604, 7.694970221153795364, 1.199719254218451159 ) ) ;
#184356 = CARTESIAN_POINT ( 'NONE',  ( 0.6393319655835437709, -1.287349573739982933, -1.294668131371433661 ) ) ;
#184357 = CARTESIAN_POINT ( 'NONE',  ( -4.717347382551060342, 7.590990148696470818, 1.199719254218464037 ) ) ;
#184358 = CARTESIAN_POINT ( 'NONE',  ( 3.715676801689533626, -1.798647723735953496, 0.3114480851732701061 ) ) ;
#184359 = CARTESIAN_POINT ( 'NONE',  ( 12.12244102266335233, 8.055895858565015999, 3.199560920820632148 ) ) ;
#184360 = CARTESIAN_POINT ( 'NONE',  ( 1.617294888471169312, 1.591762500684265946, 1.059657513450793953 ) ) ;
#184361 = CARTESIAN_POINT ( 'NONE',  ( 3.068762047175084717, 1.428394590129605346, -1.356294421569247177 ) ) ;
#184362 = CARTESIAN_POINT ( 'NONE',  ( 3.315898775378321339, 1.229719374647167296, -1.503149361444736876 ) ) ;
#184363 = CARTESIAN_POINT ( 'NONE',  ( -4.167152111353897403, 5.955039778036558040, 1.599625672291270506 ) ) ;
#184365 = CARTESIAN_POINT ( 'NONE',  ( 4.447591161967184625, -1.937652164471121763, 0.8620916771790232414 ) ) ;
#184364 = CARTESIAN_POINT ( 'NONE',  ( 5.246079093845007257, 5.085123462432798114, 0.7998128361456352531 ) ) ;
#184366 = CARTESIAN_POINT ( 'NONE',  ( 6.484567079770445552, -6.583980363594983842, 7.100579091573057333 ) ) ;
#184367 = CARTESIAN_POINT ( 'NONE',  ( 7.248805684800777804, 11.60869039890961218, 1.040834085586084257E-14 ) ) ;
#184368 = CARTESIAN_POINT ( 'NONE',  ( 6.114657076318319007, 6.015903114251479167, -0.04046911893108330605 ) ) ;
#184369 = CARTESIAN_POINT ( 'NONE',  ( 0.2331563151865451988, 4.092570554693980789, -2.500672995626152861 ) ) ;
#184370 = ORIENTED_EDGE ( 'NONE', *, *, #10253, .T. ) ;
#184371 = CARTESIAN_POINT ( 'NONE',  ( 6.308621549060418054, 6.254479983525607523, 0.7998128361456341429 ) ) ;
#184372 = CARTESIAN_POINT ( 'NONE',  ( 6.008198349511364000, 7.038594824965278995, 1.199719254218453823 ) ) ;
#184373 = CARTESIAN_POINT ( 'NONE',  ( 11.89197816957260478, 12.30000000000000071, -0.8055420615339534685 ) ) ;
#184375 = CARTESIAN_POINT ( 'NONE',  ( 6.034388706570055660, 0.6371486477873434806, 1.913263546360920220 ) ) ;
#184374 = CARTESIAN_POINT ( 'NONE',  ( 3.686012862905340803, -0.8985999850123352894, 1.589152278004740237 ) ) ;
#184376 = CARTESIAN_POINT ( 'NONE',  ( 0.1132184859782718600, 3.829867255648774726, -11.66962136008044304 ) ) ;
#184377 = CARTESIAN_POINT ( 'NONE',  ( -8.731087737520713432, 10.24898578427137963, 1.082531754730558626 ) ) ;
#184378 = CARTESIAN_POINT ( 'NONE',  ( -4.725015201957559086, 8.329469486225510977, 0.7380969479929339050 ) ) ;
#184379 = CARTESIAN_POINT ( 'NONE',  ( 7.100579091573050228, -6.583980363594990948, -6.484567079770450881 ) ) ;
#184380 = CARTESIAN_POINT ( 'NONE',  ( 4.487079325084206260, 1.670935625628103605, -0.8411387520786617333 ) ) ;
#184381 = CARTESIAN_POINT ( 'NONE',  ( 7.344766530301147789, 9.591980256816594164, 1.599625672291281386 ) ) ;
#184382 = CARTESIAN_POINT ( 'NONE',  ( 3.352094138168077553, 1.926676517159428670, -0.0006976933946620245131 ) ) ;
#184383 = CARTESIAN_POINT ( 'NONE',  ( 2.972313222866368676, 6.545497292499366182, 0.5012468031770876964 ) ) ;
#184384 = CARTESIAN_POINT ( 'NONE',  ( 5.040934186182656873, 4.775511393501539636, 1.040834085586084257E-14 ) ) ;
#184385 = CARTESIAN_POINT ( 'NONE',  ( -0.6823417656250003738, 9.713541667008065872, 1.181850606188754593 ) ) ;
#184386 = CARTESIAN_POINT ( 'NONE',  ( -7.549192604710863286, 7.701812881784464437, -0.7998128361456291469 ) ) ;
#184387 = CARTESIAN_POINT ( 'NONE',  ( 3.195971524519376494, 4.751719416737803847, -1.599625672291262513 ) ) ;
#184388 = CARTESIAN_POINT ( 'NONE',  ( -4.462041952228957165, 5.338708711422782471, -1.082531754730549967 ) ) ;
#184389 = CIRCLE ( 'NONE', #7972, 0.05000000000000057176 ) ;
#184390 = CARTESIAN_POINT ( 'NONE',  ( 1.493934562436026292, -2.100767169153750391, 0.2631679424494152153 ) ) ;
#184391 = CARTESIAN_POINT ( 'NONE',  ( 9.752392566931574081, 10.27221283770866300, -0.7998128361456281477 ) ) ;
#184392 = CARTESIAN_POINT ( 'NONE',  ( 1.499999999999995115, 3.545833333333354709, -0.8660254037844217212 ) ) ;
#184393 = CARTESIAN_POINT ( 'NONE',  ( 6.578973861349465935, 1.929489650308688464, 0.7507879531711419974 ) ) ;
#184395 = CARTESIAN_POINT ( 'NONE',  ( 4.007874524826865681, 7.816931064126571016, 0.2151701594551927443 ) ) ;
#184394 = CARTESIAN_POINT ( 'NONE',  ( 1.382094229771430705, -0.2707140722739818650, -1.821126350552772610 ) ) ;
#184396 = CARTESIAN_POINT ( 'NONE',  ( 6.065094409921147900, -1.233312222785312384, 1.939673083280533783 ) ) ;
#184397 = CARTESIAN_POINT ( 'NONE',  ( 6.643132081016125845, 6.852668304048034287, 0.7216878364870317197 ) ) ;
#184399 = SURFACE_STYLE_USAGE ( .BOTH. , #119480 ) ;
#184398 = CARTESIAN_POINT ( 'NONE',  ( 3.770576118376306241, 6.452737000530752276, 1.082531754730549078 ) ) ;
#184400 = CARTESIAN_POINT ( 'NONE',  ( 1.851946410329910808, 2.285883199777267283, -0.1717553002464344836 ) ) ;
#184401 = CARTESIAN_POINT ( 'NONE',  ( -3.853900823548995991, 8.531065964593981477, 2.447540105570293001 ) ) ;
#184402 = CARTESIAN_POINT ( 'NONE',  ( -6.445975688654487001, 6.485002823043819475, -0.7998128361456362523 ) ) ;
#184403 = CARTESIAN_POINT ( 'NONE',  ( 5.490160960519338218, -0.4736594950825470107, -1.883182239726274076 ) ) ;
#184404 = EDGE_LOOP ( 'NONE', ( #28311, #136428 ) ) ;
#184405 = CARTESIAN_POINT ( 'NONE',  ( 7.226132685959389512, 11.37431253368722750, -0.7216878364870267237 ) ) ;
#184406 = VECTOR ( 'NONE', #75762, 1000.000000000000000 ) ;
#184407 = CARTESIAN_POINT ( 'NONE',  ( 0.3342400628787962624, -1.080556536492575770, -1.698484060877824886 ) ) ;
#184408 = CARTESIAN_POINT ( 'NONE',  ( -5.823017895876262173, 7.308274721394978357, -1.333157625313810879 ) ) ;
#184410 = SURFACE_STYLE_FILL_AREA ( #89080 ) ;
#184409 = CARTESIAN_POINT ( 'NONE',  ( -8.528242318195895066, 9.908369778438709474, 1.199719254218462483 ) ) ;
#184411 = CARTESIAN_POINT ( 'NONE',  ( 0.000000000000000000, 9.719999999999998863, 0.000000000000000000 ) ) ;
#184413 = CARTESIAN_POINT ( 'NONE',  ( 2.781836775232096048, -0.9115585761545975663, 1.516887842838773759 ) ) ;
#184412 = CARTESIAN_POINT ( 'NONE',  ( 3.257844248621785788, 0.9402718649541740303, 1.867333078124802315 ) ) ;
#184414 = DIRECTION ( 'NONE',  ( 0.000000000000000000, 0.000000000000000000, -1.000000000000000000 ) ) ;
#184415 = EDGE_CURVE ( 'NONE', #190459, #85365, #161940, .T. ) ;
#184417 = CARTESIAN_POINT ( 'NONE',  ( 4.962941676929116142, 0.2283445767556212536, -2.280853557871139525 ) ) ;
#184416 = CARTESIAN_POINT ( 'NONE',  ( -0.3282377607281419252, 2.051335450315354691, 1.224999999999995870 ) ) ;
#184418 = CARTESIAN_POINT ( 'NONE',  ( 3.784860527941535491, 1.262060850391345523, 1.198560274591720098 ) ) ;
#184419 = AXIS2_PLACEMENT_3D ( 'NONE', #209232, #110763, #192996 ) ;
#184420 = CARTESIAN_POINT ( 'NONE',  ( 9.028840231696797503, 12.62106513936658203, -1.199719254218446718 ) ) ;
#184421 = CARTESIAN_POINT ( 'NONE',  ( 4.278479993564246797, 7.149254538203735798, 1.199719254218452047 ) ) ;
#184422 = CARTESIAN_POINT ( 'NONE',  ( 3.128000772048340927, 0.2569867100842055940, -1.714543959099825710 ) ) ;
#184423 = CARTESIAN_POINT ( 'NONE',  ( 3.420551359632235222, 0.9736478647841840806, 1.940675715818460878 ) ) ;
#184424 = CARTESIAN_POINT ( 'NONE',  ( 5.983225862332436584, 5.874851682342960402, 0.7998128361456341429 ) ) ;
#184425 = CARTESIAN_POINT ( 'NONE',  ( 4.223842396274177347, 0.8578445224393380641, -1.825075645057252505 ) ) ;
#184426 = CARTESIAN_POINT ( 'NONE',  ( 0.7812500000000006661, 0.7852924748300293967, 1.895863743164072357 ) ) ;
#184427 = CARTESIAN_POINT ( 'NONE',  ( -1.001543065824772872E-14, 4.743750000682822154, 1.732050807568877637 ) ) ;
#184428 = CARTESIAN_POINT ( 'NONE',  ( 1.922754896507544720, 1.796626380246616028, 0.6955005520668521291 ) ) ;
#184429 = CARTESIAN_POINT ( 'NONE',  ( -1.364683531250000748, 15.10937500034140157, 0.000000000000000000 ) ) ;
#184430 = CARTESIAN_POINT ( 'NONE',  ( 5.642908736356011978, 2.140874091242400912, 0.5926086046802480078 ) ) ;
#184431 = VERTEX_POINT ( 'NONE', #53773 ) ;
#184432 = CARTESIAN_POINT ( 'NONE',  ( -0.1108833634136767998, 2.883350581177961391, -2.385667623150728556 ) ) ;
#184433 = CARTESIAN_POINT ( 'NONE',  ( -1.499999999999997780, 1.650000000000019451, 0.000000000000000000 ) ) ;
#184434 = CARTESIAN_POINT ( 'NONE',  ( 6.043183783389218355, 8.073467052085995022, 1.599625672291267398 ) ) ;
#184435 = CARTESIAN_POINT ( 'NONE',  ( 3.497640442201256139, 7.024404915969360452, 1.040834085586084257E-14 ) ) ;
#184436 = CARTESIAN_POINT ( 'NONE',  ( 1.642778471875001811, -1.742708332855374298, 2.845375778867859751 ) ) ;
#184437 = CARTESIAN_POINT ( 'NONE',  ( 0.2236696677372449760, 1.935810370009845460, 1.089285801332658732 ) ) ;
#184438 = CARTESIAN_POINT ( 'NONE',  ( 6.250445965835445428, -1.952298026214387416, -0.1936728439068043650 ) ) ;
#184439 = CARTESIAN_POINT ( 'NONE',  ( 9.083599731475992201, 9.699880562917908122, 0.7216878364870438212 ) ) ;
#184440 = CARTESIAN_POINT ( 'NONE',  ( 0.1939103488286992305, 3.363703174398338547, 1.993194580354152867 ) ) ;
#184441 = CARTESIAN_POINT ( 'NONE',  ( 6.345044588916532113, -1.916324442970654962, 1.202328811479462578 ) ) ;
#184442 = CARTESIAN_POINT ( 'NONE',  ( 6.066347387471824781, 6.042103138330730872, -0.7998128361456481317 ) ) ;
#184443 = CARTESIAN_POINT ( 'NONE',  ( -4.502716413514301408, 7.306900678191715848, -1.082531754730549967 ) ) ;
#184444 = CARTESIAN_POINT ( 'NONE',  ( 4.914538883754228316, 0.7863694667932183968, 1.907089347224044884 ) ) ;
#184445 = CARTESIAN_POINT ( 'NONE',  ( -6.240830780992103755, 6.175390754112560110, 1.040834085586084257E-14 ) ) ;
#184446 = CARTESIAN_POINT ( 'NONE',  ( -0.7500000000000215383, 4.222916667349481123, 1.299038105676671107 ) ) ;
#184447 = CARTESIAN_POINT ( 'NONE',  ( 1.364683531249990311, 5.426041667008086655, 0.7879004041258500513 ) ) ;
#184448 = CARTESIAN_POINT ( 'NONE',  ( 5.729731410239141454, -1.186140735684092284, -1.446405967604667886 ) ) ;
#184449 = CARTESIAN_POINT ( 'NONE',  ( 4.588316246536889409, -0.4565669943805070186, 1.672893389497135841 ) ) ;
#184450 = CARTESIAN_POINT ( 'NONE',  ( 3.227794649281841011, 1.698692639566254936, 0.3781252810216747529 ) ) ;
#184451 = CARTESIAN_POINT ( 'NONE',  ( 10.53432216769390095, 11.39239007183880581, -0.7216878364870257245 ) ) ;
#184452 = CARTESIAN_POINT ( 'NONE',  ( 1.417954980037740009, -1.278267931767061771, -1.902717450791486353 ) ) ;
#184453 = CARTESIAN_POINT ( 'NONE',  ( 0.6823417656249899377, 3.488541667008085323, -1.181850606188754593 ) ) ;
#184454 = CARTESIAN_POINT ( 'NONE',  ( 5.425362623596053702, -1.327343567673059166, -1.615326566546205767 ) ) ;
#184455 = CARTESIAN_POINT ( 'NONE',  ( 0.5504183687293667804, -1.553892155338543191, -0.9872222399871022347 ) ) ;
#184456 = FACE_OUTER_BOUND ( 'NONE', #145304, .T. ) ;
#184457 = CARTESIAN_POINT ( 'NONE',  ( 2.110000207431836472, 0.002812218110825881467, 2.016597019944998959 ) ) ;
#184458 = CARTESIAN_POINT ( 'NONE',  ( 0.1116237293282626442, -2.148295633857814746, 0.4319020730012904097 ) ) ;
#184459 = CARTESIAN_POINT ( 'NONE',  ( 7.449797558097145611, 15.00000000000000000, -10.26196259744787653 ) ) ;
#184460 = CARTESIAN_POINT ( 'NONE',  ( -6.665805079413154921, 10.92852302595736447, 0.7998128361456481317 ) ) ;
#184461 = CARTESIAN_POINT ( 'NONE',  ( 6.602984505055297326, 7.662235663108029726, 1.199719254218462483 ) ) ;
#184462 = CARTESIAN_POINT ( 'NONE',  ( 2.719513590175401063, 1.792643918890064247, 1.132349250948051500 ) ) ;
#184463 = CARTESIAN_POINT ( 'NONE',  ( -1.364683531250014514, -1.011458332991911568, -0.7879004041258359514 ) ) ;
#184464 = CARTESIAN_POINT ( 'NONE',  ( 6.041596546049881944, -1.325759876995153075, -1.255439798616593716 ) ) ;
#184465 = ORIENTED_EDGE ( 'NONE', *, *, #82581, .F. ) ;
#184466 = CARTESIAN_POINT ( 'NONE',  ( -7.279802135894939852, 7.457800344824362604, -0.7998128361456362523 ) ) ;
#184467 = SURFACE_STYLE_USAGE ( .BOTH. , #149866 ) ;
#184468 = CARTESIAN_POINT ( 'NONE',  ( -3.475000000000000533, -4.156249999044084653, 0.000000000000000000 ) ) ;
#184469 = CARTESIAN_POINT ( 'NONE',  ( -7.366157530926372488, 7.488271962369228874, -0.7998128361456291469 ) ) ;
#184470 = CARTESIAN_POINT ( 'NONE',  ( 2.496358458697241378, -1.034576831241553307, 1.734530517449877740 ) ) ;
#184471 = CARTESIAN_POINT ( 'NONE',  ( 0.3058767667667975365, -0.5614299121656821656, 2.029657625958045664 ) ) ;
#184472 = CARTESIAN_POINT ( 'NONE',  ( 9.622536337397022521, 12.24937836509514710, 1.599625672291281386 ) ) ;
#184473 = CARTESIAN_POINT ( 'NONE',  ( 3.942128412476927135, -0.9204884114761485714, 1.617296529409748773 ) ) ;
#184474 = CARTESIAN_POINT ( 'NONE',  ( 8.432281472695482449, 11.92507992053172572, 1.199719254218450271 ) ) ;
#184475 = DIRECTION ( 'NONE',  ( 1.000000000000000000, -7.387867266669436732E-31, 0.000000000000000000 ) ) ;
#184476 = CARTESIAN_POINT ( 'NONE',  ( -4.437596350374534815, 4.071617251725375475, -0.7998128361456221525 ) ) ;
#184477 = CARTESIAN_POINT ( 'NONE',  ( -8.453672473320708036, 9.821371626084353323, -1.199719254218446718 ) ) ;
#184478 = MECHANICAL_DESIGN_GEOMETRIC_PRESENTATION_REPRESENTATION (  '', ( #156843 ), #60024 ) ;
#184480 = CARTESIAN_POINT ( 'NONE',  ( -4.074449998555902397, 7.717048951691181102, 0.6760625908293280695 ) ) ;
#184479 = CARTESIAN_POINT ( 'NONE',  ( -5.912237504011027767, 9.055304967058290799, 1.199719254218454489 ) ) ;
#184481 = CARTESIAN_POINT ( 'NONE',  ( 0.6823417656249864960, -0.8239583329919114574, -1.181850606188749264 ) ) ;
#184482 = CARTESIAN_POINT ( 'NONE',  ( 1.440355836138224932, 1.027696236922505557, 1.396268056379332378 ) ) ;
#184483 = CARTESIAN_POINT ( 'NONE',  ( 1.640152974701726496, -1.471428658003028911, 0.9289965205148569272 ) ) ;
#184485 = CARTESIAN_POINT ( 'NONE',  ( 7.117667457494414762, 11.24776976714476184, 1.040834085586084257E-14 ) ) ;
#184484 = CARTESIAN_POINT ( 'NONE',  ( 5.145303760848274344, -1.981494167013456709, 1.182657305203537401 ) ) ;
#184486 = CARTESIAN_POINT ( 'NONE',  ( 3.715816618597135523, 6.492813934075403637, -1.199719254218453823 ) ) ;
#184487 = CARTESIAN_POINT ( 'NONE',  ( 1.792332366127664223, -2.050593157767267805, -0.2048568651325937962 ) ) ;
#184488 = CARTESIAN_POINT ( 'NONE',  ( 5.900823170445728572, 7.907379670318584353, 1.599625672291267398 ) ) ;
#184489 = CARTESIAN_POINT ( 'NONE',  ( 6.890000000000009450, -0.01081285896028030651, 2.279840171838908525 ) ) ;
#184490 = DIRECTION ( 'NONE',  ( 0.000000000000000000, 0.000000000000000000, -1.000000000000000000 ) ) ;
#184491 = CARTESIAN_POINT ( 'NONE',  ( -5.773793314573309132, 7.829454515125894964, 1.599625672291263179 ) ) ;
#184492 = CARTESIAN_POINT ( 'NONE',  ( 0.5320225927652595388, 1.015637564890453426, -1.689598002260852772 ) ) ;
#184493 = B_SPLINE_CURVE_WITH_KNOTS ( 'NONE', 3,
 ( #174280, #141799, #206743, #207803, #56243, #188360 ),
 .UNSPECIFIED., .F., .F.,
 ( 4, 2, 4 ),
 ( 0.000000000000000000, 0.0003473417695167276627, 0.0006946835390334553254 ),
 .UNSPECIFIED. ) ;
#184495 = CARTESIAN_POINT ( 'NONE',  ( -6.455090533882193782, 9.584670485287619002, -1.082531754730549967 ) ) ;
#184494 = CARTESIAN_POINT ( 'NONE',  ( 4.095896644567202038, 1.253117935160457552, 1.444681106026260320 ) ) ;
#184496 = CARTESIAN_POINT ( 'NONE',  ( 6.604147088760183415, -2.206502607372296421, 0.04933187264975073122 ) ) ;
#184497 = CARTESIAN_POINT ( 'NONE',  ( 1.224999999999996980, 1.687500000682823353, -2.602085213965210642E-14 ) ) ;
#184498 = CARTESIAN_POINT ( 'NONE',  ( -7.905812970100109638, 8.396072351304486148, 0.7216878364870317197 ) ) ;
#184499 = CARTESIAN_POINT ( 'NONE',  ( 5.221298554594243413, 5.264138866547622975, -0.7216878364870458196 ) ) ;
#184500 = CARTESIAN_POINT ( 'NONE',  ( -4.543390873910949423, 6.393985001019784953, 1.443375672974058777 ) ) ;
#184501 = CARTESIAN_POINT ( 'NONE',  ( 0.4694063198951373694, -1.707435420315214003, -1.078448885650341582 ) ) ;
#184502 = ORIENTED_EDGE ( 'NONE', *, *, #81818, .T. ) ;
#184503 = CARTESIAN_POINT ( 'NONE',  ( 3.557953228543974777, 0.5631008447647236625, -2.237707790512387440 ) ) ;
#184504 = CARTESIAN_POINT ( 'NONE',  ( 4.791432466842788784, -1.794507165602466037, 0.7932701521168731285 ) ) ;
#184505 = CARTESIAN_POINT ( 'NONE',  ( 0.5847188370675902025, 1.875566754216885013, 0.5750099747552291918 ) ) ;
#184506 = CARTESIAN_POINT ( 'NONE',  ( 2.223174002961016082, 5.537527403522402025, -0.7216878364870267237 ) ) ;
#184507 = CARTESIAN_POINT ( 'NONE',  ( 6.500815859342971237, -6.554751161430536932, 6.901817408925775332 ) ) ;
#184508 = ORIENTED_EDGE ( 'NONE', *, *, #35190, .F. ) ;
#184509 = CARTESIAN_POINT ( 'NONE',  ( 0.2513570338038995100, 0.2008850299538050832, -2.107768975555255331 ) ) ;
#184510 = CARTESIAN_POINT ( 'NONE',  ( -9.318531651294266638, 9.766041769465124034, -0.7998128361456291469 ) ) ;
#184511 = CARTESIAN_POINT ( 'NONE',  ( -0.007072395215936694290, 7.009756401597622144, 2.079987976222394952 ) ) ;
#184512 = CARTESIAN_POINT ( 'NONE',  ( 3.643588050499571018, 1.964860050422628124, -0.9237357390106512023 ) ) ;
#184513 = CARTESIAN_POINT ( 'NONE',  ( 0.9496594531581278309, -1.914679731917130479, 0.9119059213342151082 ) ) ;
#184514 = CARTESIAN_POINT ( 'NONE',  ( 1.499999999999987121, 1.285416667349485120, 0.8660254037844524744 ) ) ;
#184515 = CARTESIAN_POINT ( 'NONE',  ( 9.728138913005292210, 11.30824913904973705, -1.199719254218440723 ) ) ;
#184516 = CARTESIAN_POINT ( 'NONE',  ( 11.89204169242350950, 13.79999999999999893, -0.8046421800350563869 ) ) ;
#184517 = CARTESIAN_POINT ( 'NONE',  ( 6.597622414017595638, 6.771646741010207471, 0.1687998040609314243 ) ) ;
#184518 = CARTESIAN_POINT ( 'NONE',  ( 2.056002787803516973, 2.055476740694470728, -0.1483529063488266686 ) ) ;
#184520 = CARTESIAN_POINT ( 'NONE',  ( 6.902720183911290164, 14.55305236562705318, -9.761920501353818835 ) ) ;
#184519 = CARTESIAN_POINT ( 'NONE',  ( -9.992522908471816123, 11.61669713376064372, 1.199719254218462483 ) ) ;
#184521 = CARTESIAN_POINT ( 'NONE',  ( 1.364683531249988535, 2.613541667008089764, 0.7879004041258500513 ) ) ;
#184522 = CARTESIAN_POINT ( 'NONE',  ( -3.188928480291423728, 8.980740528189222971, 2.451733079074398969 ) ) ;
#184523 = CARTESIAN_POINT ( 'NONE',  ( 10.62873463776380056, 11.29999999999998117, 3.199999999999997957 ) ) ;
#184524 = ORIENTED_EDGE ( 'NONE', *, *, #208497, .F. ) ;
#184525 = CARTESIAN_POINT ( 'NONE',  ( 4.986922676292999235, -1.801926769106906745, -0.6406197933803285949 ) ) ;
#184526 = DIRECTION ( 'NONE',  ( 0.000000000000000000, 0.000000000000000000, 1.000000000000000000 ) ) ;
#184527 = CARTESIAN_POINT ( 'NONE',  ( 0.7204656808509112276, -1.211343046821738101, -1.910610397963452112 ) ) ;
#184528 = CARTESIAN_POINT ( 'NONE',  ( -4.060830702492950195, 4.696389560118578999, -1.199719254218452047 ) ) ;
#184529 = CARTESIAN_POINT ( 'NONE',  ( 0.9315677820061087910, -1.767094751418090803, 0.3981412331970111684 ) ) ;
#184530 = CARTESIAN_POINT ( 'NONE',  ( 0.6904808011564408377, 1.448434100015457693, -1.253846941973751683 ) ) ;
#184531 = CARTESIAN_POINT ( 'NONE',  ( 1.451716722110554025, 1.566445173006292935, 1.353826630019476562 ) ) ;
#184532 = CARTESIAN_POINT ( 'NONE',  ( 0.6823417656249882723, 0.1552083336747514530, 1.181850606188755259 ) ) ;
#184533 = CARTESIAN_POINT ( 'NONE',  ( 6.772336237553374438, -1.148929780121176414, 1.476827877338216854 ) ) ;
#184534 = CARTESIAN_POINT ( 'NONE',  ( 5.479104952107777926, -0.04952074540257554031, -1.926025958231538882 ) ) ;
#184536 = CARTESIAN_POINT ( 'NONE',  ( 6.170003545802125622, 6.961323287618347955, -0.9016653442153206299 ) ) ;
#184535 = CARTESIAN_POINT ( 'NONE',  ( 0.5402173299829955422, -1.636151841282366126, -1.627667753820499330 ) ) ;
#184537 = EDGE_CURVE ( 'NONE', #213528, #31261, #91360, .T. ) ;
#184538 = CARTESIAN_POINT ( 'NONE',  ( -1.364683531250012516, 2.238541667008087988, -0.7879004041258289570 ) ) ;
#184539 = CARTESIAN_POINT ( 'NONE',  ( 3.701677541426426910, -1.560128098810292130, -1.349382831327667454 ) ) ;
#184540 = AXIS2_PLACEMENT_3D ( 'NONE', #212651, #175922, #160725 ) ;
#184542 = CARTESIAN_POINT ( 'NONE',  ( -5.876569516519495551, 8.943415971659659292, 1.199719254218452047 ) ) ;
#184541 = AXIS2_PLACEMENT_3D ( 'NONE', #112028, #29648, #147665 ) ;
#184543 = CARTESIAN_POINT ( 'NONE',  ( 7.884230021546724920, 9.157022099014721306, 1.199719254218462483 ) ) ;
#184544 = CARTESIAN_POINT ( 'NONE',  ( 3.734381245560244089, 6.444196322207211836, 1.199719254218462483 ) ) ;
#184545 = CARTESIAN_POINT ( 'NONE',  ( 4.306686350635271054, 8.176217842383143974, -0.7998128361456221525 ) ) ;
#184547 = CARTESIAN_POINT ( 'NONE',  ( -1.500000000000011324, 4.379166666666688634, -0.8660254037844313801 ) ) ;
#184546 = CARTESIAN_POINT ( 'NONE',  ( 5.315496758875870142, -0.3119175628578441661, 2.082610458907033557 ) ) ;
#184548 = CARTESIAN_POINT ( 'NONE',  ( 6.039524589772497620, 1.914416561877980261, -0.7887839105886890190 ) ) ;
#184550 = CARTESIAN_POINT ( 'NONE',  ( -0.6823417656250212460, 1.113541667008083325, 1.181850606188755259 ) ) ;
#184549 = CIRCLE ( 'NONE', #77415, 0.08000000000000020983 ) ;
#184551 = CARTESIAN_POINT ( 'NONE',  ( 4.446650332099550518, 0.5718123500428309303, 2.084546224624775679 ) ) ;
#184552 = CARTESIAN_POINT ( 'NONE',  ( 4.529947673531667718, -1.980263497020241292, 0.3961197999026391248 ) ) ;
#184553 = CARTESIAN_POINT ( 'NONE',  ( 3.104453987849314700, 4.644948957289396496, 0.000000000000000000 ) ) ;
#184554 = AXIS2_PLACEMENT_3D ( 'NONE', #146587, #130386, #81549 ) ;
#184557 = CARTESIAN_POINT ( 'NONE',  ( 5.450014563013511726, 8.341805509282339770, -1.082531754730543083 ) ) ;
#184556 = CARTESIAN_POINT ( 'NONE',  ( -3.285556943750000070, -1.859374999522041882, 0.000000000000000000 ) ) ;
#184555 = CARTESIAN_POINT ( 'NONE',  ( 5.826972158823246595, 10.02016096192762085, -0.7998128361456481317 ) ) ;
#184558 = CARTESIAN_POINT ( 'NONE',  ( -6.119526231721793330, 8.232809585132461194, 1.599625672291263179 ) ) ;
#184559 = CARTESIAN_POINT ( 'NONE',  ( 3.854704076794239764, -1.883312302057647880, -0.7212934815618715634 ) ) ;
#184560 = CARTESIAN_POINT ( 'NONE',  ( -9.854078719034067291, 10.39084668182823634, 0.7998128361456462443 ) ) ;
#184562 = CARTESIAN_POINT ( 'NONE',  ( -10.99462479582586738, -5.166863022246599435, 0.3540227772641256210 ) ) ;
#184561 = CARTESIAN_POINT ( 'NONE',  ( -5.427341564172148303, 5.226320001155936090, 0.000000000000000000 ) ) ;
#184563 = B_SPLINE_CURVE_WITH_KNOTS ( 'NONE', 3,
 ( #70824, #116467, #182459, #168360, #86040, #66554 ),
 .UNSPECIFIED., .F., .F.,
 ( 4, 2, 4 ),
 ( 0.000000000000000000, 0.0003767643964918268649, 0.0007535287929836534046 ),
 .UNSPECIFIED. ) ;
#184564 = CARTESIAN_POINT ( 'NONE',  ( -11.96535697748089078, 12.34737332935553944, -0.9148528286454110647 ) ) ;
#184565 = FACE_OUTER_BOUND ( 'NONE', #112241, .T. ) ;
#184567 = CARTESIAN_POINT ( 'NONE',  ( 4.183220377109976518, 1.621195451842275315, 1.198844725951081047 ) ) ;
#184566 = CARTESIAN_POINT ( 'NONE',  ( -8.473482818416682605, 8.988077497682020578, -0.7216878364870267237 ) ) ;
#184568 = CARTESIAN_POINT ( 'NONE',  ( 1.499999999999989120, 5.045833333333354709, -0.8660254037844323793 ) ) ;
#184569 = CARTESIAN_POINT ( 'NONE',  ( 0.1875851866701295223, -0.8181552731707610882, 1.518483014795414032 ) ) ;
#184570 = CARTESIAN_POINT ( 'NONE',  ( 4.552505719138623341, 8.533283448962240669, 0.7998128361456341429 ) ) ;
#184572 = CARTESIAN_POINT ( 'NONE',  ( 0.000000000000000000, 13.49999999999999822, 0.000000000000000000 ) ) ;
#184571 = CARTESIAN_POINT ( 'NONE',  ( 8.785320351975350661, 9.351887953500479966, -0.7216878364870197293 ) ) ;
#184573 = CARTESIAN_POINT ( 'NONE',  ( 10.99943592164172657, -9.900000000000005684, -0.1113975120798811613 ) ) ;
#184574 = CARTESIAN_POINT ( 'NONE',  ( 4.938664768831325880, 0.3182328507864223277, 1.843102042236575588 ) ) ;
#184575 =( BOUNDED_CURVE ( )  B_SPLINE_CURVE ( 3, ( #201858, #187760, #104399, #154211 ),
 .UNSPECIFIED., .F., .T. ) 
 B_SPLINE_CURVE_WITH_KNOTS ( ( 4, 4 ),
 ( 0.000000000000000000, 1.570796326794816844 ),
 .UNSPECIFIED. ) 
 CURVE ( )  GEOMETRIC_REPRESENTATION_ITEM ( )  RATIONAL_B_SPLINE_CURVE ( ( 1.000000000000000000, 0.8047378541243839223, 0.8047378541243839223, 1.000000000000000000 ) ) 
 REPRESENTATION_ITEM ( '' )  );
#184576 = CARTESIAN_POINT ( 'NONE',  ( 6.504166875733549347, -0.8557802559411722410, 1.820156917002911712 ) ) ;
#184577 = FILL_AREA_STYLE ('',( #135855 ) ) ;
#184578 = CARTESIAN_POINT ( 'NONE',  ( -6.251718229232856139, 8.387033582228697881, -1.443375672974066548 ) ) ;
#184579 = VERTEX_POINT ( 'NONE', #171786 ) ;
#184580 = CARTESIAN_POINT ( 'NONE',  ( 9.910647101465253073, 11.62513837554007168, -1.082531754730537088 ) ) ;
#184582 = EDGE_CURVE ( 'NONE', #49028, #49203, #72129, .T. ) ;
#184581 = CARTESIAN_POINT ( 'NONE',  ( 0.4918148228068714989, -2.006445053647107013, 0.2004575690456936732 ) ) ;
#184583 = CARTESIAN_POINT ( 'NONE',  ( 1.441375510584298913, -1.705046834049932292, 0.6123784311264174329 ) ) ;
#184584 = CARTESIAN_POINT ( 'NONE',  ( 5.365994935958575240, 9.482354201918870018, 0.7998128361456341429 ) ) ;
#184585 = CARTESIAN_POINT ( 'NONE',  ( 6.649309733611729278, -1.732918351142084035, -1.292073167451508686 ) ) ;
#184586 = CARTESIAN_POINT ( 'NONE',  ( 5.764187864104357573, 9.876636274763768597, 1.040834085586084257E-14 ) ) ;
#184588 = CARTESIAN_POINT ( 'NONE',  ( -0.1884536309573183466, -1.180508991428173671, -1.509157985239983679 ) ) ;
#184587 = CARTESIAN_POINT ( 'NONE',  ( -5.362413449404877852, 6.214902764849178141, -1.199719254218446718 ) ) ;
#184589 = CARTESIAN_POINT ( 'NONE',  ( -0.7499999999999972244, 5.108333333333353821, -1.299038105676652011 ) ) ;
#184590 = CARTESIAN_POINT ( 'NONE',  ( 6.559000000000036579, 7.629137130509070275, 2.600000000000001421 ) ) ;
#184591 = EDGE_CURVE ( 'NONE', #94238, #69637, #143329, .T. ) ;
#184592 = CARTESIAN_POINT ( 'NONE',  ( 0.6823417656249882723, -0.8447916663252494907, 1.181850606188755259 ) ) ;
#184594 = EDGE_LOOP ( 'NONE', ( #57403, #188495, #33431, #140526 ) ) ;
#184593 = CARTESIAN_POINT ( 'NONE',  ( 2.236732156574683827, 5.553345249405011508, 1.040834085586084257E-14 ) ) ;
#184595 = CARTESIAN_POINT ( 'NONE',  ( -4.308793891044708779, 3.921347715840572956, 1.214306433183764966E-14 ) ) ;
#184596 = CARTESIAN_POINT ( 'NONE',  ( 4.135729569369491543, -1.488772398488471094, -1.567562023322838671 ) ) ;
#184597 = EDGE_CURVE ( 'NONE', #81793, #167113, #63650, .T. ) ;
#184598 = CARTESIAN_POINT ( 'NONE',  ( -6.644904684473536882, 6.925012684740138980, 0.7216878364870317197 ) ) ;
#184599 = CARTESIAN_POINT ( 'NONE',  ( 4.746763178560241769, 8.551991118380046331, 0.7216878364870328300 ) ) ;
#184600 = CARTESIAN_POINT ( 'NONE',  ( 1.195735321641926197, 1.957225868588155837, -0.8166992996602241428 ) ) ;
#184601 = DIRECTION ( 'NONE',  ( 0.000000000000000000, 0.000000000000000000, -1.000000000000000000 ) ) ;
#184602 = CARTESIAN_POINT ( 'NONE',  ( 2.477749938138404051, 1.209727786519874559, 1.556487202666415604 ) ) ;
#184603 = CARTESIAN_POINT ( 'NONE',  ( 4.306835718904429733, -0.4242474483713705169, -1.864571660543254961 ) ) ;
#184604 = ORIENTED_EDGE ( 'NONE', *, *, #175858, .F. ) ;
#184605 = CARTESIAN_POINT ( 'NONE',  ( 1.123270288250308280, 2.860197346350005887, 0.7749999999993786304 ) ) ;
#184606 = CARTESIAN_POINT ( 'NONE',  ( 6.338338845641732888, -1.054863691225367939, 1.663055945198953278 ) ) ;
#184607 = CARTESIAN_POINT ( 'NONE',  ( 0.8318532965871343610, 1.913089267318631270, 0.3326846900589939815 ) ) ;
#184608 = ORIENTED_EDGE ( 'NONE', *, *, #86821, .F. ) ;
#184609 = CARTESIAN_POINT ( 'NONE',  ( -4.472210567661380587, 6.310941310395290493, 1.599625672291270506 ) ) ;
#184610 = CARTESIAN_POINT ( 'NONE',  ( -4.767627293860968507, 5.591261926706423857, -1.199719254218453823 ) ) ;
#184612 = CARTESIAN_POINT ( 'NONE',  ( 7.010974831598141499, 7.352094523052197239, -0.7216878364870317197 ) ) ;
#184611 = CARTESIAN_POINT ( 'NONE',  ( 6.470265622219697477, 8.571729197388226140, -1.599625672291262513 ) ) ;
#184614 = EDGE_LOOP ( 'NONE', ( #153991, #52105, #126110, #10430 ) ) ;
#184613 = CARTESIAN_POINT ( 'NONE',  ( 4.600206319907148789, -0.8982956317880007591, 1.688143452400918454 ) ) ;
#184615 = CARTESIAN_POINT ( 'NONE',  ( 3.703933201646680828, -0.6411959742554216302, 2.111683309420588905 ) ) ;
#184616 = B_SPLINE_CURVE_WITH_KNOTS ( 'NONE', 3,
 ( #23618, #124429, #109231, #106004, #126556, #173104 ),
 .UNSPECIFIED., .F., .F.,
 ( 4, 2, 4 ),
 ( 0.000000000000000000, 0.0003239988925529259205, 0.0006479977851058518409 ),
 .UNSPECIFIED. ) ;
#184617 = CARTESIAN_POINT ( 'NONE',  ( 2.362605853119781774, 0.9431403173822919817, 1.995201469058570432 ) ) ;
#184618 = CARTESIAN_POINT ( 'NONE',  ( 0.4516138619287948797, 3.070015318549077943, -0.4124855346668246381 ) ) ;
#184619 = CARTESIAN_POINT ( 'NONE',  ( 0.4340482808194641162, -1.023182136338888659, -1.615339470012015166 ) ) ;
#184621 = CIRCLE ( 'NONE', #163940, 0.04999999999999991257 ) ;
#184620 = CARTESIAN_POINT ( 'NONE',  ( -10.50060100873255031, 5.377693802073529206, 5.808388628131297970 ) ) ;
#184622 = CARTESIAN_POINT ( 'NONE',  ( 0.1263921868141488214, 7.050106634747087320, 4.033475512996062662 ) ) ;
#184623 = CARTESIAN_POINT ( 'NONE',  ( 3.437997351728830697, 1.311287738946330439, 1.602184970737066338 ) ) ;
#184624 = CARTESIAN_POINT ( 'NONE',  ( -5.436983294280064882, 6.301900917203534291, 1.199719254218450271 ) ) ;
#184625 = CARTESIAN_POINT ( 'NONE',  ( -4.627894000755552462, 8.353582960325299567, 0.3099817540855500653 ) ) ;
#184627 = CARTESIAN_POINT ( 'NONE',  ( 1.165152350680317195, -1.954565670758709128, -0.9236901323337529668 ) ) ;
#184626 = CARTESIAN_POINT ( 'NONE',  ( -3.228813138348844536, 6.918699094715619502, 0.7998128361456341429 ) ) ;
#184628 = CARTESIAN_POINT ( 'NONE',  ( 2.577880719133851084, -1.123996537731044354, 1.881222605751430521 ) ) ;
#184629 = CARTESIAN_POINT ( 'NONE',  ( -0.1018178655972588748, 3.468664187816145716, -1.997505796056266547 ) ) ;
#184630 = PLANE ( 'NONE',  #97124 ) ;
#184631 = CARTESIAN_POINT ( 'NONE',  ( -1.225000000000038058, 1.041666667349488984, -0.7072540797573257931 ) ) ;
#184632 = CARTESIAN_POINT ( 'NONE',  ( -1.402160292154681736E-14, 12.98437500034139980, 1.575800808251682339 ) ) ;
#184633 = CARTESIAN_POINT ( 'NONE',  ( -4.956387674247580755, 7.940146832334256111, 1.199719254218452935 ) ) ;
#184634 = PRODUCT_DEFINITION_CONTEXT ( 'detailed design', #126667, 'design' ) ;
#184635 = CARTESIAN_POINT ( 'NONE',  ( 6.275961099261262000, 1.503942705979001593, -0.8632642021696999013 ) ) ;
#184636 = CARTESIAN_POINT ( 'NONE',  ( -3.440018289565379028, 5.036440642624797626, 1.599625672291267398 ) ) ;
#184637 = CARTESIAN_POINT ( 'NONE',  ( 3.713788242813487184, 0.5077267127921447631, -2.006887321594638784 ) ) ;
#184638 = CARTESIAN_POINT ( 'NONE',  ( 4.429392955138825805, -1.637772332673973485, -1.341807030983455773 ) ) ;
#184639 = CARTESIAN_POINT ( 'NONE',  ( 4.964256800898067645, 8.943383367689749619, 0.7998128361456462443 ) ) ;
#184640 = CARTESIAN_POINT ( 'NONE',  ( 0.6823417656249917140, 4.842708333674755394, 1.181850606188765695 ) ) ;
#184641 = CARTESIAN_POINT ( 'NONE',  ( 2.395301122324170695, -1.761490415372953589, 0.8809153588016715997 ) ) ;
#184642 = CARTESIAN_POINT ( 'NONE',  ( 0.6856317642073318508, 1.842354612247762091, -0.5124485439033445999 ) ) ;
#184643 = CARTESIAN_POINT ( 'NONE',  ( 5.244168061255013669, 0.6613091839676830119, 2.194790591360805898 ) ) ;
#184644 = CARTESIAN_POINT ( 'NONE',  ( 2.613660848560445782, -1.805822647967848971, 0.2677728182119283318 ) ) ;
#184645 = CARTESIAN_POINT ( 'NONE',  ( 7.512626515748109135, 8.897724035528543851, 1.082531754730549967 ) ) ;
#184646 = CARTESIAN_POINT ( 'NONE',  ( 5.517805330637495231, 6.500156309574290248, -1.082531754730543083 ) ) ;
#184647 = CARTESIAN_POINT ( 'NONE',  ( -7.206322340863467346, 8.366129804884193888, 1.199719254218450271 ) ) ;
#184648 = CARTESIAN_POINT ( 'NONE',  ( 4.552993993533384298, 0.3484205210483002357, 1.982688671860346252 ) ) ;
#184649 = CARTESIAN_POINT ( 'NONE',  ( 4.891432378139471737, -1.795214109662087942, 0.7913882323652280393 ) ) ;
#184650 = CARTESIAN_POINT ( 'NONE',  ( -7.588813295347149435, 9.876701482703580837, -1.599625672291263179 ) ) ;
#184651 = CARTESIAN_POINT ( 'NONE',  ( -6.274726165026268454, 6.214935368819085149, 0.7998128361456341429 ) ) ;
#184652 = CARTESIAN_POINT ( 'NONE',  ( 0.1753634416057739953, 5.721028741045294908, -2.738064866945366660 ) ) ;
#184654 = CARTESIAN_POINT ( 'NONE',  ( 5.348444421042818142, 0.5165251424982686412, 1.692803071163173634 ) ) ;
#184653 = CARTESIAN_POINT ( 'NONE',  ( -0.1291982275798781443, -0.004298614154785855221, -2.073875112923003083 ) ) ;
#184655 = PLANE ( 'NONE',  #43479 ) ;
#184656 = EDGE_CURVE ( 'NONE', #82080, #50087, #181306, .T. ) ;
#184657 = CARTESIAN_POINT ( 'NONE',  ( 1.429895766826321690, 1.077743243251317429, -1.908043295719801025 ) ) ;
#184658 = CARTESIAN_POINT ( 'NONE',  ( 6.210887288261135453, -0.2055507460125911567, 1.728089712739445671 ) ) ;
#184659 = CARTESIAN_POINT ( 'NONE',  ( 5.615048174354031474, 9.702639970055050966, 0.7998128361456462443 ) ) ;
#184660 = PRESENTATION_STYLE_ASSIGNMENT (( #118676 ) ) ;
#184661 = CARTESIAN_POINT ( 'NONE',  ( 0.04690384546136848465, -1.329360633743952746, -1.098954345569080893 ) ) ;
#184662 = CARTESIAN_POINT ( 'NONE',  ( 1.283028839759347894, -2.242172747002548316, 0.5046827817699239827 ) ) ;
#184663 = CARTESIAN_POINT ( 'NONE',  ( 0.2401087780563165297, 2.186128513634697512, 0.1550312349237955856 ) ) ;
#184664 = CARTESIAN_POINT ( 'NONE',  ( 6.608738931450677256, 0.6592670866186548517, -1.603827835538347291 ) ) ;
#184665 = CARTESIAN_POINT ( 'NONE',  ( 3.528125218122651230, -1.314342534882004809, -1.772652456903674567 ) ) ;
#184666 = CARTESIAN_POINT ( 'NONE',  ( 0.3566018059198462486, -2.170557273582163216, -0.05455199461934338162 ) ) ;
#184667 = CARTESIAN_POINT ( 'NONE',  ( 0.000000000000000000, 11.29999999999999893, 0.000000000000000000 ) ) ;
#184668 = CARTESIAN_POINT ( 'NONE',  ( 1.692723046232265105, 1.565162839624185898, -1.426121385913220019 ) ) ;
#184669 = CARTESIAN_POINT ( 'NONE',  ( 6.727182134110167411, 4.685720203848058318, 2.851561905840187983 ) ) ;
#184670 = CARTESIAN_POINT ( 'NONE',  ( 5.877940811483009398, 1.147681995895684315, 1.547064007116766060 ) ) ;
#184671 = EDGE_LOOP ( 'NONE', ( #203510, #50922, #142165, #81268 ) ) ;
#184673 = CARTESIAN_POINT ( 'NONE',  ( -1.402160292154681736E-14, -0.8656249996585829720, 1.575800808251672791 ) ) ;
#184672 = CARTESIAN_POINT ( 'NONE',  ( 1.716775041481681585, 2.140780187006920077, 0.8202503203454788450 ) ) ;
#184674 = CARTESIAN_POINT ( 'NONE',  ( 2.900554798319789906, 5.471398800426671372, 1.199719254218452047 ) ) ;
#184675 = CARTESIAN_POINT ( 'NONE',  ( 6.356075086708249167, 6.309842444114747373, -0.7998128361456281477 ) ) ;
#184676 = CARTESIAN_POINT ( 'NONE',  ( 3.264521566599550173, 2.221473416772083098, -0.001674386450213962828 ) ) ;
#184677 = CARTESIAN_POINT ( 'NONE',  ( -7.700668062882072284, 10.00719871149432549, -1.443375672974059665 ) ) ;
#184678 =( NAMED_UNIT ( * ) PLANE_ANGLE_UNIT ( ) SI_UNIT ( $, .RADIAN. ) );
#184679 = CARTESIAN_POINT ( 'NONE',  ( 6.046573322014824114, 7.117052299514516456, -1.082531754730543083 ) ) ;
#184680 = CARTESIAN_POINT ( 'NONE',  ( -7.470179451005382276, 11.65903375957422128, 0.7216878364870458196 ) ) ;
#184681 = AXIS2_PLACEMENT_3D ( 'NONE', #27005, #93111, #39011 ) ;
#184682 = CARTESIAN_POINT ( 'NONE',  ( 6.400857919427532572, 6.640291458853147866, -0.7216878364870458196 ) ) ;
#184683 = ORIENTED_EDGE ( 'NONE', *, *, #91921, .F. ) ;
#184684 = CARTESIAN_POINT ( 'NONE',  ( 2.022111496571117772, -1.799922141918413487, 0.9091460122201827643 ) ) ;
#184686 = CARTESIAN_POINT ( 'NONE',  ( 1.393505825229651052, -1.866293207157668776, 0.8783701326641482066 ) ) ;
#184685 = CARTESIAN_POINT ( 'NONE',  ( 6.591235234537977661, 10.84152487360300299, 0.7998128361456462443 ) ) ;
#184687 = CARTESIAN_POINT ( 'NONE',  ( 5.031484404002867450, 8.884165881396448583, 0.7216878364870317197 ) ) ;
#184688 = AXIS2_PLACEMENT_3D ( 'NONE', #174792, #110896, #26368 ) ;
#184689 = DIRECTION ( 'NONE',  ( 0.000000000000000000, 0.000000000000000000, -1.000000000000000000 ) ) ;
#184690 = CARTESIAN_POINT ( 'NONE',  ( -0.6823417656249969321, 4.217708333674755394, -1.181850606188749264 ) ) ;
#184691 = CARTESIAN_POINT ( 'NONE',  ( 4.154361996720875361, -1.624486827992781990, 1.471056368041193219 ) ) ;
#184692 = CARTESIAN_POINT ( 'NONE',  ( 0.7740648250077889481, 1.777010169924503558, -0.9530137779002674225 ) ) ;
#184693 = CARTESIAN_POINT ( 'NONE',  ( 0.7316835000789992938, 1.813914744281470925, 0.3150931809976220133 ) ) ;
#184694 = CARTESIAN_POINT ( 'NONE',  ( 5.759400667030329934, 2.259083744078540956, -0.3884743064591251738 ) ) ;
#184695 = CARTESIAN_POINT ( 'NONE',  ( 3.398233898566359823, 1.450718870894672330, -1.133551952132209717 ) ) ;
#184696 = CARTESIAN_POINT ( 'NONE',  ( 8.748035429315576650, 11.22912730566677553, -1.599625672291255185 ) ) ;
#184697 = CARTESIAN_POINT ( 'NONE',  ( 4.401258566127845384, 1.466438172381477445, 1.087111955044787859 ) ) ;
#184698 = CARTESIAN_POINT ( 'NONE',  ( 5.168592345394213972, 1.356298078840772803, 1.492257005506092193 ) ) ;
#184699 = CARTESIAN_POINT ( 'NONE',  ( -8.422639742587602285, 10.84949900448412841, -1.599625672291263179 ) ) ;
#184701 = CARTESIAN_POINT ( 'NONE',  ( -7.282664789195997912, 8.525472337930658284, 1.199719254218452047 ) ) ;
#184700 = CARTESIAN_POINT ( 'NONE',  ( 4.346707190358800155, 0.5996197433882300976, 2.181559591530066289 ) ) ;
#184702 = CARTESIAN_POINT ( 'NONE',  ( 6.721705546354253435, -2.043712959172855115, 0.5078683761520035311 ) ) ;
#184703 = CARTESIAN_POINT ( 'NONE',  ( 3.086448098943677998, 1.152334561581969785, -1.719836228861029603 ) ) ;
#184704 = CARTESIAN_POINT ( 'NONE',  ( 8.530051201292206287, 13.10347683481629488, 0.000000000000000000 ) ) ;
#184705 = CARTESIAN_POINT ( 'NONE',  ( 0.6801582343749900117, 1.588541667008100511, -1.178068619123890270 ) ) ;
#184706 = APPLICATION_PROTOCOL_DEFINITION ( 'draft international standard', 'automotive_design', 1998, #86421 ) ;
#184708 = CARTESIAN_POINT ( 'NONE',  ( 1.559075672363739118, -1.651969382833524902, -0.9909376787137593734 ) ) ;
#184707 = CARTESIAN_POINT ( 'NONE',  ( -9.664264568442742842, 10.16939683947169115, -0.7998128361456291469 ) ) ;
#184709 = CARTESIAN_POINT ( 'NONE',  ( 6.860212146170862724, -1.969081375482661267, 0.04489377202578949400 ) ) ;
#184710 = CARTESIAN_POINT ( 'NONE',  ( 5.031484404002891431, 5.042689024191078673, 0.7216878364870328300 ) ) ;
#184711 = CARTESIAN_POINT ( 'NONE',  ( 5.731063993565963521, 6.075950606329157289, 0.6577720730673256577 ) ) ;
#184712 = DIRECTION ( 'NONE',  ( -0.9486832980505139901, -0.3162277660168373861, 3.312310031615527941E-15 ) ) ;
#184713 = CARTESIAN_POINT ( 'NONE',  ( -8.649738815838677652, 13.03518635187974262, 0.7216878364870357165 ) ) ;
#184714 = CARTESIAN_POINT ( 'NONE',  ( 2.057158355326561772, 0.4919409011131297138, 2.166103627455501890 ) ) ;
#184715 = CARTESIAN_POINT ( 'NONE',  ( 3.065558131891146676, 0.3103791954156452371, -2.082839965623133782 ) ) ;
#184716 = CARTESIAN_POINT ( 'NONE',  ( -7.259464905474441565, 7.434073576000447048, -0.7998128361456362523 ) ) ;
#184717 = CARTESIAN_POINT ( 'NONE',  ( 8.260995669428309540, 8.532249790621511565, 0.7998128361456481317 ) ) ;
#184718 = CARTESIAN_POINT ( 'NONE',  ( 0.6251817401201573698, 0.1879592460329523318, -1.851551742960926727 ) ) ;
#184719 = CARTESIAN_POINT ( 'NONE',  ( 6.799577732453452761, 7.891594428405881878, -1.199719254218446718 ) ) ;
#184720 = CARTESIAN_POINT ( 'NONE',  ( 3.310162060030825248, 7.013606170011280838, -0.7998128361456291469 ) ) ;
#184721 = CARTESIAN_POINT ( 'NONE',  ( -6.794044374223859428, 7.099008989448849505, 0.000000000000000000 ) ) ;
#184722 = CARTESIAN_POINT ( 'NONE',  ( -7.212574532790100079, 9.437756259720353924, -1.443375672974059665 ) ) ;
#184723 = CARTESIAN_POINT ( 'NONE',  ( 1.336355901170083849, -1.182550835430173919, -1.760063440837428272 ) ) ;
#184724 = CARTESIAN_POINT ( 'NONE',  ( -7.435720902452096936, 7.639705572474380091, 0.000000000000000000 ) ) ;
#184726 = CARTESIAN_POINT ( 'NONE',  ( 4.545333077707183200, 1.753367681936630840, -0.8802267832125689750 ) ) ;
#184725 = CARTESIAN_POINT ( 'NONE',  ( -1.225000000000060263, 1.270833333333358128, 0.7072540797572717253 ) ) ;
#184727 = CARTESIAN_POINT ( 'NONE',  ( 3.028364643526501698, 1.202066397148596977, -1.796461956351296019 ) ) ;
#184728 = CARTESIAN_POINT ( 'NONE',  ( 1.751249726499287673, 1.836263021919124050, -0.1365115386888632321 ) ) ;
#184729 = CARTESIAN_POINT ( 'NONE',  ( -4.014638704412293535, 7.626288086010478473, 0.05010440672792437766 ) ) ;
#184730 = CARTESIAN_POINT ( 'NONE',  ( 5.156098626313831090, -1.256936769724174674, 1.203943403725541206 ) ) ;
#184731 = CARTESIAN_POINT ( 'NONE',  ( 1.000000047849771034, 16.00000000000000711, -11.64874984998672680 ) ) ;
#184732 = CARTESIAN_POINT ( 'NONE',  ( 4.690757960648221037, 7.456006139856155457, 1.082531754730558626 ) ) ;
#184733 = CARTESIAN_POINT ( 'NONE',  ( -11.52570357830391323, 8.091488070261075194, -2.173620758456770830 ) ) ;
#184734 = CARTESIAN_POINT ( 'NONE',  ( 2.008865009297224447, 1.601992838228694316, -1.451600824242594845 ) ) ;
#184735 = EDGE_CURVE ( 'NONE', #41100, #15288, #164016, .T. ) ;
#184736 = CARTESIAN_POINT ( 'NONE',  ( 3.602888598310006074, 0.9090057795711030675, -1.799647124144133858 ) ) ;
#184737 = CARTESIAN_POINT ( 'NONE',  ( -9.693716643646601128, 12.33242205571964512, 1.443375672974076540 ) ) ;
#184738 = CARTESIAN_POINT ( 'NONE',  ( 1.129994055010040022, -1.371941552271437770, -1.670562328977095445 ) ) ;
#184739 = CARTESIAN_POINT ( 'NONE',  ( 2.905103271286565647, 1.664600965932877319, 1.056039161509576108 ) ) ;
#184740 = AXIS2_PLACEMENT_3D ( 'NONE', #105155, #170122, #122547 ) ;
#184741 = CARTESIAN_POINT ( 'NONE',  ( -1.249999999999964695, 8.500000000000000000, -11.02939254900287303 ) ) ;
#184742 = CARTESIAN_POINT ( 'NONE',  ( 3.333474266508968054, 0.8707927262202612706, -1.735945723835415677 ) ) ;
#184745 = ORIENTED_EDGE ( 'NONE', *, *, #139330, .T. ) ;
#184744 = CARTESIAN_POINT ( 'NONE',  ( -3.797692425603673705, 6.484372692295976570, 1.082531754730549967 ) ) ;
#184743 = CARTESIAN_POINT ( 'NONE',  ( -10.45297324601190425, 11.29748299654313470, 0.7216878364870438212 ) ) ;
#184746 = CARTESIAN_POINT ( 'NONE',  ( -5.302647476276252547, 5.359045941843285199, 0.7216878364870257245 ) ) ;
#184747 = CARTESIAN_POINT ( 'NONE',  ( -0.1108833634137010304, 7.629137130509073828, -2.496956624467902675 ) ) ;
#184748 = CARTESIAN_POINT ( 'NONE',  ( 5.923986774528332333, 5.876015756563318426, -0.7998128361456481317 ) ) ;
#184749 = CARTESIAN_POINT ( 'NONE',  ( -3.980200614063634568, 6.801261928786307642, 1.199719254218452935 ) ) ;
#184750 = CARTESIAN_POINT ( 'NONE',  ( -5.582925393777276035, 9.735439736040634173, 0.7998128361456291469 ) ) ;
#184751 = CARTESIAN_POINT ( 'NONE',  ( -8.297226821439000588, 12.62392235841345389, 1.040834085586084257E-14 ) ) ;
#184752 = CARTESIAN_POINT ( 'NONE',  ( 0.5873203293235219613, -0.2722241568871349160, -2.189838084831654541 ) ) ;
#184753 = CARTESIAN_POINT ( 'NONE',  ( 0.000000000000000000, -3.696874999522040017, -3.793834371823813001 ) ) ;
#184754 = CARTESIAN_POINT ( 'NONE',  ( 4.135565103414404753, 1.848670044762780407, -0.6568835154602686854 ) ) ;
#184755 =( BOUNDED_CURVE ( )  B_SPLINE_CURVE ( 2, ( #181604, #33232, #67827, #148068, #114560, #133974, #183744, #165365, #49488 ),
 .UNSPECIFIED., .F., .T. ) 
 B_SPLINE_CURVE_WITH_KNOTS ( ( 3, 2, 2, 2, 3 ),
 ( 0.4732142857142856984, 0.4761904761904761640, 0.4821428571428571508, 0.4880952380952380820, 0.4910714285714285476 ),
 .UNSPECIFIED. ) 
 CURVE ( )  GEOMETRIC_REPRESENTATION_ITEM ( )  RATIONAL_B_SPLINE_CURVE ( ( 0.9330127018922194093, 0.9330127018922194093, 1.000000000000000000, 0.8660254037844387076, 1.000000000000000000, 0.8660254037844387076, 1.000000000000000000, 0.9330127018922199644, 0.9330127018922194093 ) ) 
 REPRESENTATION_ITEM ( '' )  );
#184756 = CARTESIAN_POINT ( 'NONE',  ( 8.945682426918439845, 9.331051007693339727, 1.040834085586084257E-14 ) ) ;
#184757 = CARTESIAN_POINT ( 'NONE',  ( 1.776017750421728270, 1.753029812786778940, -0.9963028777105963352 ) ) ;
#184758 = VERTEX_POINT ( 'NONE', #85196 ) ;
#184759 = CARTESIAN_POINT ( 'NONE',  ( 3.134099051248913970, 2.117513410275436936, -0.004568276605129357668 ) ) ;
#184760 = CARTESIAN_POINT ( 'NONE',  ( -0.7500000000000006661, 1.389583334016154748, -1.299038105676652011 ) ) ;
#184762 = CARTESIAN_POINT ( 'NONE',  ( -6.891622154448065807, 6.934647356477856128, 1.040834085586084257E-14 ) ) ;
#184761 = FILL_AREA_STYLE_COLOUR ( '', #114781 ) ;
#184763 = CARTESIAN_POINT ( 'NONE',  ( 2.607153984523866264, -1.821078476238715327, 0.2702138248509636242 ) ) ;
#184764 = VERTEX_POINT ( 'NONE', #204250 ) ;
#184765 =( REPRESENTATION_RELATIONSHIP ('NONE','NONE', #84563, #121983 ) REPRESENTATION_RELATIONSHIP_WITH_TRANSFORMATION ( #73091 )SHAPE_REPRESENTATION_RELATIONSHIP( ) );
#184766 = CARTESIAN_POINT ( 'NONE',  ( -7.621654909176601045, 12.04368116068139472, 0.7998128361456481317 ) ) ;
#184767 = CARTESIAN_POINT ( 'NONE',  ( -3.795919822146283540, 6.412028311603867436, -1.082531754730549967 ) ) ;
#184768 = CARTESIAN_POINT ( 'NONE',  ( 3.797228045176269440, -0.2112621354826669517, -2.110076569278092062 ) ) ;
#184769 = CARTESIAN_POINT ( 'NONE',  ( -1.500000000000011324, 5.160416667349487341, -0.8660254037844313801 ) ) ;
#184770 = CARTESIAN_POINT ( 'NONE',  ( 5.615048174354031474, 9.702639970055050966, 0.7998128361456462443 ) ) ;
#184771 = EDGE_CURVE ( 'NONE', #77260, #60029, #35373, .T. ) ;
#184772 = CARTESIAN_POINT ( 'NONE',  ( 5.677046966798700467, -0.04615325445976201785, -2.060428132270344381 ) ) ;
#184774 = CARTESIAN_POINT ( 'NONE',  ( 2.296224312773272658, 1.477747569344042278, -1.098160524033331642 ) ) ;
#184773 = CARTESIAN_POINT ( 'NONE',  ( 0.8361097980106885208, -1.038377568841988063, 1.544222109484013172 ) ) ;
#184775 = CARTESIAN_POINT ( 'NONE',  ( 8.880754312151170282, 10.31963377138658089, 1.199719254218453823 ) ) ;
#184776 = CARTESIAN_POINT ( 'NONE',  ( 6.095638044316721960, 6.027669342855261014, -0.2934597938374111092 ) ) ;
#184777 =( NAMED_UNIT ( * ) SI_UNIT ( $, .STERADIAN. ) SOLID_ANGLE_UNIT ( ) );
#184778 = DIRECTION ( 'NONE',  ( 0.000000000000000000, 1.000000000000000000, 0.000000000000000000 ) ) ;
#184779 = CARTESIAN_POINT ( 'NONE',  ( 0.000000000000000000, 13.49999999999999822, -1.500000000000000222 ) ) ;
#184780 = CARTESIAN_POINT ( 'NONE',  ( 2.491098823239074278, -0.3784457004711218042, -2.174036671264235387 ) ) ;
#184781 = CARTESIAN_POINT ( 'NONE',  ( 5.114671183409561728, 1.565253227384774792, -1.633764300155052807 ) ) ;
#184782 = CARTESIAN_POINT ( 'NONE',  ( -6.385527162356466668, 10.39360608948380182, 0.000000000000000000 ) ) ;
#184783 = CARTESIAN_POINT ( 'NONE',  ( 4.482537919100934687, -1.178242479775050811, 1.376196796631526720 ) ) ;
#184784 = CARTESIAN_POINT ( 'NONE',  ( 4.065584057473277113, 1.255829935711678669, 1.446728075138058678 ) ) ;
#184785 = CARTESIAN_POINT ( 'NONE',  ( -0.6823417656250212460, 3.613541667008085767, 1.181850606188767472 ) ) ;
#184786 = CARTESIAN_POINT ( 'NONE',  ( 3.731288366010646396, -1.822051990069279315, 0.7533225318517923208 ) ) ;
#184787 = CARTESIAN_POINT ( 'NONE',  ( 4.873830839387755631, 1.077430855447782942, 1.529020332772989210 ) ) ;
#184788 = CARTESIAN_POINT ( 'NONE',  ( 4.738624546071780408, -1.804922690063763824, -0.4530168641722984169 ) ) ;
#184789 = CARTESIAN_POINT ( 'NONE',  ( 1.364683531249992088, 5.634375000341417916, 1.214306433183764966E-14 ) ) ;
#184790 = CLOSED_SHELL ( 'NONE', ( #207611, #59839, #67480, #24832, #48574, #205842, #152194, #107061 ) ) ;
#184791 = CARTESIAN_POINT ( 'NONE',  ( 0.2336117360935245635, 0.6279853779636718203, -1.916355031878452797 ) ) ;
#184793 = CARTESIAN_POINT ( 'NONE',  ( 1.928482936185798247, 1.211665229685221057, -1.722411974427066506 ) ) ;
#184792 = CARTESIAN_POINT ( 'NONE',  ( -4.731432421044888592, 4.622352034081546712, -0.7216878364870207285 ) ) ;
#184794 = CARTESIAN_POINT ( 'NONE',  ( 10.58621901417202515, 11.24501035948919991, -0.7998128361456281477 ) ) ;
#184796 = CARTESIAN_POINT ( 'NONE',  ( 0.07479286986305544449, 2.046156589154801253, -2.272744413733415403 ) ) ;
#184795 = CARTESIAN_POINT ( 'NONE',  ( -1.001543065824772872E-14, 5.134375000341421469, 1.575800808251672791 ) ) ;
#184797 = FACE_OUTER_BOUND ( 'NONE', #111552, .T. ) ;
#184798 = CARTESIAN_POINT ( 'NONE',  ( 1.336200995665462354, -1.125576746034629094, -1.676869184967361814 ) ) ;
#184799 = CARTESIAN_POINT ( 'NONE',  ( -1.364683531250012516, 2.488541667008088876, -0.7879004041258289570 ) ) ;
#184800 = CARTESIAN_POINT ( 'NONE',  ( -4.175548123328963079, 4.934189567714277302, 1.082531754730560403 ) ) ;
#184801 = CARTESIAN_POINT ( 'NONE',  ( 3.388648328411762556, 6.040841252200647382, 1.199719254218462483 ) ) ;
#184802 = ORIENTED_EDGE ( 'NONE', *, *, #149589, .F. ) ;
#184803 = ADVANCED_FACE ( 'NONE', ( #155547 ), #35457, .F. ) ;
#184804 = CARTESIAN_POINT ( 'NONE',  ( 2.601032539102793084, 1.737798908178284307, -1.285340053188685383 ) ) ;
#184805 = CARTESIAN_POINT ( 'NONE',  ( 6.610000000000006537, 0.002781820520842553934, 2.000159646111852929 ) ) ;
#184808 = CARTESIAN_POINT ( 'NONE',  ( -3.903294069008378830, 8.999999999999998224, -0.7749999999999979128 ) ) ;
#184807 = CARTESIAN_POINT ( 'NONE',  ( -1.420000000000021911, 6.280000000000042881, 2.500000000000011102 ) ) ;
#184806 = CARTESIAN_POINT ( 'NONE',  ( 4.760848217054122422, 5.583353003765119560, -1.199719254218452047 ) ) ;
#184809 = CARTESIAN_POINT ( 'NONE',  ( 11.96217875511317885, 9.771456334210231631, 0.9561995067075056420 ) ) ;
#184810 = CARTESIAN_POINT ( 'NONE',  ( 11.88235317400313917, 9.843357602269703577, -0.9089793033029952563 ) ) ;
#184811 = CARTESIAN_POINT ( 'NONE',  ( -6.873620692448438874, 10.96304854125777695, 0.000000000000000000 ) ) ;
#184812 = CARTESIAN_POINT ( 'NONE',  ( 0.9607770615731696662, -1.983481723135366304, -0.9323335341336475013 ) ) ;
#184813 = DIRECTION ( 'NONE',  ( 0.000000000000000000, 0.000000000000000000, 1.000000000000000000 ) ) ;
#184815 = CARTESIAN_POINT ( 'NONE',  ( -0.6823417656250039265, 11.56770833367473017, -1.181850606188755259 ) ) ;
#184814 = CARTESIAN_POINT ( 'NONE',  ( 1.604739632818411144, -0.8155265934593752819, -2.110601385940619412 ) ) ;
#184816 = CARTESIAN_POINT ( 'NONE',  ( -8.134002093194872884, 11.57708731111429401, 1.199719254218453823 ) ) ;
#184817 = CARTESIAN_POINT ( 'NONE',  ( -3.578989363883261277, 7.119311991265024453, 1.040834085586084257E-14 ) ) ;
#184818 = CARTESIAN_POINT ( 'NONE',  ( -1.402160292154681736E-14, 2.509375000341417028, -1.575800808251660134 ) ) ;
#184819 = CARTESIAN_POINT ( 'NONE',  ( 4.644395130292630292, 8.311692339142366492, -0.4369040224408097250 ) ) ;
#184820 = CARTESIAN_POINT ( 'NONE',  ( -1.500000000000015099, 9.479166666666669627, -0.8660254037844309360 ) ) ;
#184821 = CARTESIAN_POINT ( 'NONE',  ( 3.527714679269139619, -1.028799902082434992, -1.384306889003545926 ) ) ;
#184822 = CARTESIAN_POINT ( 'NONE',  ( 5.174371902270911150, 6.065797303184739420, 1.199719254218452047 ) ) ;
#184823 = EDGE_CURVE ( 'NONE', #146443, #35153, #98289, .T. ) ;
#184824 = CARTESIAN_POINT ( 'NONE',  ( 2.424752316626857862, -0.004995123648579914352, 1.769921776121333945 ) ) ;
#184825 = CARTESIAN_POINT ( 'NONE',  ( 5.737410212107617369, -1.997324651315037780, 0.9386623957203032997 ) ) ;
#184826 = VERTEX_POINT ( 'NONE', #137170 ) ;
#184827 = CARTESIAN_POINT ( 'NONE',  ( 4.183856667257361828, 1.958065582907195568, -0.4948979464895820191 ) ) ;
#184828 = CARTESIAN_POINT ( 'NONE',  ( -6.505933609711270549, 8.683618192786854095, -1.599625672291271394 ) ) ;
#184829 = CARTESIAN_POINT ( 'NONE',  ( 3.708611378246814638, 1.915606880664010747, 0.6298579873919087913 ) ) ;
#184831 = ORIENTED_EDGE ( 'NONE', *, *, #154049, .T. ) ;
#184830 = CARTESIAN_POINT ( 'NONE',  ( 4.130988372668517705, 1.658889437441883441, 0.7283703743019008803 ) ) ;
#184832 = CARTESIAN_POINT ( 'NONE',  ( 2.588565208901713266, -0.3177388942022137397, -1.843305967786903032 ) ) ;
#184833 = AXIS2_PLACEMENT_3D ( 'NONE', #44569, #176683, #28295 ) ;
#184834 = CARTESIAN_POINT ( 'NONE',  ( 1.499999999999821032, 7.240846818246208905, -4.154462424328212222 ) ) ;
#184835 = CARTESIAN_POINT ( 'NONE',  ( 2.127084423382288314, 1.709874882824816478, 0.8565708355050825062 ) ) ;
#184836 = DIRECTION ( 'NONE',  ( -0.000000000000000000, -1.000000000000000000, -0.000000000000000000 ) ) ;
#184837 = CARTESIAN_POINT ( 'NONE',  ( -10.57449672806501262, 3.061848070889987561, -7.008429158759065913 ) ) ;
#184838 = CARTESIAN_POINT ( 'NONE',  ( -7.037870247915956945, -8.233137084989836652, 6.381095703207982694 ) ) ;
#184839 = COLOUR_RGB ( '', 0.72549020, 0.75294118, 0.79215686) ;
#184840 = ADVANCED_FACE ( 'NONE', ( #120991 ), #186958, .F. ) ;
#184841 = CARTESIAN_POINT ( 'NONE',  ( 0.6823417656249882723, 2.738541667008084879, -1.181850606188749264 ) ) ;
#184842 = CARTESIAN_POINT ( 'NONE',  ( 0.4570967503451648373, -1.639016809899789040, 0.9851245988263114262 ) ) ;
#184843 = CARTESIAN_POINT ( 'NONE',  ( 4.171111447311355747, 1.799123655847803205, -0.9110083886025857058 ) ) ;
#184844 = CARTESIAN_POINT ( 'NONE',  ( 6.129694847154206983, 8.244672969803623630, -1.443375672974078761 ) ) ;
#184845 = CARTESIAN_POINT ( 'NONE',  ( 2.049198471137442912, 1.708465938063120637, -0.9642302061752603404 ) ) ;
#184846 = ADVANCED_FACE ( 'NONE', ( #91634, #208527 ), #127392, .F. ) ;
#184847 = CARTESIAN_POINT ( 'NONE',  ( -3.763755302173069861, 3.180306474485406820, -2.446972558850334600 ) ) ;
#184848 = CARTESIAN_POINT ( 'NONE',  ( -5.586841817283045408, 8.675676665875643678, 1.199719254218454489 ) ) ;
#184849 = CARTESIAN_POINT ( 'NONE',  ( 4.148766697842418694, 2.080301416381886703, 0.4105806053946169376 ) ) ;
#184851 = DIRECTION ( 'NONE',  ( -8.881784197001252323E-15, 0.000000000000000000, 1.000000000000000000 ) ) ;
#184850 = CARTESIAN_POINT ( 'NONE',  ( 8.224992744984721327, 12.74757530245756243, 1.040834085586084257E-14 ) ) ;
#184852 = CARTESIAN_POINT ( 'NONE',  ( 5.413337677306027551, -0.2920802625693446619, 1.949502277767001690 ) ) ;
#184853 = CARTESIAN_POINT ( 'NONE',  ( 1.364683531249986537, 1.405208333674755838, -0.7879004041258239610 ) ) ;
#184854 = CARTESIAN_POINT ( 'NONE',  ( 1.019790247428183472, -0.4849793317353002786, 1.953821064534920326 ) ) ;
#184855 = VERTEX_POINT ( 'NONE', #159798 ) ;
#184856 = CARTESIAN_POINT ( 'NONE',  ( 1.265409400557556907, 1.954659568096604350, -0.8140754496198910894 ) ) ;
#184857 = CARTESIAN_POINT ( 'NONE',  ( 11.75718816816947587, 6.923265086052656336, 2.447717586180979676 ) ) ;
#184858 = CARTESIAN_POINT ( 'NONE',  ( 2.576698201331685922, 1.354182300986291887, -1.566139152919379107 ) ) ;
#184859 = CARTESIAN_POINT ( 'NONE',  ( 5.578253857379852576, 5.472660686556754861, -0.7998128361456481317 ) ) ;
#184860 = CARTESIAN_POINT ( 'NONE',  ( 4.715203562502613188, 8.723097599553565118, 0.7998128361456341429 ) ) ;
#184861 = ORIENTED_EDGE ( 'NONE', *, *, #80428, .F. ) ;
#184863 = CARTESIAN_POINT ( 'NONE',  ( 4.487912541323413329, 5.194651705420806564, 1.199719254218462483 ) ) ;
#184862 = CARTESIAN_POINT ( 'NONE',  ( 4.576172254314175625, -2.027756842407653082, -0.5083681234262329429 ) ) ;
#184866 = ORIENTED_EDGE ( 'NONE', *, *, #150667, .T. ) ;
#184865 = CARTESIAN_POINT ( 'NONE',  ( 1.137045503269896285, -0.04498225810314023659, 1.811072777871777006 ) ) ;
#184864 = CARTESIAN_POINT ( 'NONE',  ( 2.696107482849848580, -1.820545782403935720, -0.1364615833806467338 ) ) ;
#184867 = CARTESIAN_POINT ( 'NONE',  ( 6.656857027519620829, -1.708965229049699053, 1.396003577074665714 ) ) ;
#184868 = CARTESIAN_POINT ( 'NONE',  ( 4.354158978451688533, 5.549389920478685845, 1.308530732453070833 ) ) ;
#184869 = CARTESIAN_POINT ( 'NONE',  ( 8.815910235490386881, 13.32329502132428267, -7.673832123164161523 ) ) ;
#184870 = CARTESIAN_POINT ( 'NONE',  ( 5.421004802376033993, 2.037064969303593820, 0.8491359902737596332 ) ) ;
#184871 = CARTESIAN_POINT ( 'NONE',  ( -0.6823417656250039265, 9.630208333674728394, -1.181850606188755259 ) ) ;
#184872 = ORIENTED_EDGE ( 'NONE', *, *, #124535, .F. ) ;
#184873 = CARTESIAN_POINT ( 'NONE',  ( 4.283787348595206268, 1.854039900284172315, -0.4678174759695231666 ) ) ;
#184874 = CARTESIAN_POINT ( 'NONE',  ( -4.647747731386360215, 4.316793862905830892, 0.7998128361456341429 ) ) ;
#184875 = CARTESIAN_POINT ( 'NONE',  ( 7.527801604085637699, 9.805521176231838609, 1.599625672291281386 ) ) ;
#184876 = CARTESIAN_POINT ( 'NONE',  ( 6.865700769154306826, -0.4580177224273937475, 2.026514595051785772 ) ) ;
#184877 = TOROIDAL_SURFACE ( 'NONE', #25793, 11.18000000000000149, 0.08000000000000000167 ) ;
#184878 = CARTESIAN_POINT ( 'NONE',  ( 1.360316468750004448, 0.2968750003413955785, -6.938893903907228378E-15 ) ) ;
#184879 = CARTESIAN_POINT ( 'NONE',  ( 3.348500752450929596, 6.850408611260650815, 0.7216878364870317197 ) ) ;
#184880 = CARTESIAN_POINT ( 'NONE',  ( 10.99970480893080627, -6.221252899067775566, 0.08058608058608524027 ) ) ;
#184881 = CARTESIAN_POINT ( 'NONE',  ( 5.348589505275513467, 7.707351500233518671, -1.315919829448284784 ) ) ;
#184882 = CARTESIAN_POINT ( 'NONE',  ( -4.795850263662800650, 15.51848109256882147, -11.00904932270169212 ) ) ;
#184883 = CARTESIAN_POINT ( 'NONE',  ( 3.286256049847174676, -1.842268013383094427, -0.3231441395407097517 ) ) ;
#184884 = CARTESIAN_POINT ( 'NONE',  ( 3.285556943750000514, -1.101041666188710355, 1.896917185911906722 ) ) ;
#184885 = CARTESIAN_POINT ( 'NONE',  ( 1.886825320689258012, 2.480000000000016858, -2.459652456995881753 ) ) ;
#184887 = CARTESIAN_POINT ( 'NONE',  ( -7.049876689426113785, 8.287572894827684777, -1.082531754730544860 ) ) ;
#184886 = MECHANICAL_DESIGN_GEOMETRIC_PRESENTATION_REPRESENTATION (  '', ( #178131 ), #81168 ) ;
#184888 = CARTESIAN_POINT ( 'NONE',  ( 4.869313445963426190, 5.709895770826003414, 1.199719254218452935 ) ) ;
#184889 = CARTESIAN_POINT ( 'NONE',  ( 6.661133543015731462, 6.665743976473484267, -0.7998128361456281477 ) ) ;
#184890 = CARTESIAN_POINT ( 'NONE',  ( 6.631696427350994405, 1.982895789845315671, -0.5951614246157420629 ) ) ;
#184891 = CARTESIAN_POINT ( 'NONE',  ( 0.7906389332529573100, 1.525030349845598820, -1.319245847334844735 ) ) ;
#184892 = CARTESIAN_POINT ( 'NONE',  ( -9.646789991323334590, 11.21334206375407305, 1.199719254218462483 ) ) ;
#184893 = CARTESIAN_POINT ( 'NONE',  ( 5.006703865196457492, 9.063181286029688977, 0.000000000000000000 ) ) ;
#184894 = CARTESIAN_POINT ( 'NONE',  ( 0.8850414913617115076, 1.931072968267994794, -1.036053359626129877 ) ) ;
#184895 = CARTESIAN_POINT ( 'NONE',  ( 6.656878040733529289, -1.407521694628325770, 1.162499734694094844 ) ) ;
#184896 = CARTESIAN_POINT ( 'NONE',  ( -2.462777459176719308, 6.024990802348131780, -0.7998128361456281477 ) ) ;
#184897 = VECTOR ( 'NONE', #106141, 1000.000000000000000 ) ;
#184898 = CARTESIAN_POINT ( 'NONE',  ( 4.258669648468268676, 7.982548666606070320, 0.7216878364870257245 ) ) ;
#184899 = CARTESIAN_POINT ( 'NONE',  ( 8.992082194361556091, 11.51384853155376220, 1.599625672291279388 ) ) ;
#184900 = CARTESIAN_POINT ( 'NONE',  ( 5.190073875932979419, 4.949507698210251938, 0.7998128361456341429 ) ) ;
#184901 = CARTESIAN_POINT ( 'NONE',  ( 3.390420931869152721, 6.113185632892752075, -1.199719254218452047 ) ) ;
#184902 = ORIENTED_EDGE ( 'NONE', *, *, #54063, .T. ) ;
#184904 = CARTESIAN_POINT ( 'NONE',  ( 1.049477475095396573, -1.818952357203638570, 0.8628315626280655959 ) ) ;
#184903 = CARTESIAN_POINT ( 'NONE',  ( 4.018977146631536712, -1.760761141180338774, 0.5383908109771737838 ) ) ;
#184905 = CARTESIAN_POINT ( 'NONE',  ( 1.968534425330380921, 1.910819170882430695, 1.277001204893423170 ) ) ;
#184907 = CARTESIAN_POINT ( 'NONE',  ( 0.4263013476871494456, -1.221759592413705908, 1.403788950402263369 ) ) ;
#184906 = CARTESIAN_POINT ( 'NONE',  ( 5.043269954603547767, 4.986162489899998995, -0.7216878364870197293 ) ) ;
#184908 = CARTESIAN_POINT ( 'NONE',  ( 3.475000000000000533, -0.1458333333333326765, -2.006292185433951047 ) ) ;
#184909 = CARTESIAN_POINT ( 'NONE',  ( -3.228813138348844536, 6.918699094715619502, 0.7998128361456341429 ) ) ;
#184910 = SURFACE_STYLE_FILL_AREA ( #120003 ) ;
#184911 = CARTESIAN_POINT ( 'NONE',  ( 4.183787391381143195, 1.853651273288700718, -0.4697857328580385960 ) ) ;
#184912 = CARTESIAN_POINT ( 'NONE',  ( -9.972185678051314284, 11.59297036493672017, 1.199719254218462483 ) ) ;
#184913 = CARTESIAN_POINT ( 'NONE',  ( 6.435429789636040177, 6.784273175954743884, -0.4071148367965071735 ) ) ;
#184914 = CARTESIAN_POINT ( 'NONE',  ( -6.238160076063538284, 9.331584951165851294, 1.082531754730549967 ) ) ;
#184916 = CARTESIAN_POINT ( 'NONE',  ( 2.606148294764852213, -0.7140300644919925777, -1.729217693616967644 ) ) ;
#184915 = CARTESIAN_POINT ( 'NONE',  ( 4.001575260567552306, -2.085028717228009310, 0.1556281442064103848 ) ) ;
#184917 = CARTESIAN_POINT ( 'NONE',  ( 9.097157885089661278, 9.715698408800516717, 1.040834085586084257E-14 ) ) ;
#184918 = CARTESIAN_POINT ( 'NONE',  ( -6.381095703207996905, -8.233137084989849086, -7.037870247915946287 ) ) ;
#184919 = CARTESIAN_POINT ( 'NONE',  ( 3.087183437724149826, -0.7025620359558025774, 1.592517242405028233 ) ) ;
#184920 = CARTESIAN_POINT ( 'NONE',  ( 4.202137545231717120, 6.989912005157271402, 1.199719254218462483 ) ) ;
#184922 = CARTESIAN_POINT ( 'NONE',  ( 11.86145016429273191, 13.40000000000000036, -1.100000000000002087 ) ) ;
#184921 = CARTESIAN_POINT ( 'NONE',  ( -5.548322005359108466, 5.928160571233643594, 0.7412397383242540494 ) ) ;
#184923 = CARTESIAN_POINT ( 'NONE',  ( 3.650762458506318087, -1.408968171862119423, 0.9946885059901353632 ) ) ;
#184924 = CARTESIAN_POINT ( 'NONE',  ( 3.878626735558046157, -0.2160506499642600997, -2.180900317982924275 ) ) ;
#184925 = CARTESIAN_POINT ( 'NONE',  ( 6.199877634063251541, -0.7475181258948644381, 2.076568058718592624 ) ) ;
#184926 = CARTESIAN_POINT ( 'NONE',  ( 0.4019237886466778820, 8.573664549684629321, 1.500000000000001554 ) ) ;
#184927 = CARTESIAN_POINT ( 'NONE',  ( 4.012681996134721096, 0.7761599038508348869, 2.027777647250021076 ) ) ;
#184928 = CARTESIAN_POINT ( 'NONE',  ( 1.857752496991037061, 1.820901040755190214, -0.1330985588276211995 ) ) ;
#184929 = CARTESIAN_POINT ( 'NONE',  ( 0.3210474040165818277, -1.749687966165301090, -0.8873976775175674847 ) ) ;
#184930 = CARTESIAN_POINT ( 'NONE',  ( 4.803976500543080341, -1.135498674831243227, -1.786957999583696610 ) ) ;
#184931 = ORIENTED_EDGE ( 'NONE', *, *, #165187, .F. ) ;
#184933 = CARTESIAN_POINT ( 'NONE',  ( -0.6823417656250003738, 2.530208333674753618, -1.181850606188749264 ) ) ;
#184932 = CARTESIAN_POINT ( 'NONE',  ( 4.634495141935854434, 0.3908333592176889137, 2.258673302944668837 ) ) ;
#184934 = CARTESIAN_POINT ( 'NONE',  ( 6.720655732516641834, 0.008434553976904584152, 1.726293928996263771 ) ) ;
#184935 = CARTESIAN_POINT ( 'NONE',  ( 4.390142812726693045, 4.016254791136236513, 1.214306433183764966E-14 ) ) ;
#184936 = CARTESIAN_POINT ( 'NONE',  ( 0.9090200710941964690, -0.5189423241485704441, -2.055877189782874481 ) ) ;
#184937 = CARTESIAN_POINT ( 'NONE',  ( -3.958617665510272943, 6.601842462195195438, -1.082531754730549967 ) ) ;
#184938 = CARTESIAN_POINT ( 'NONE',  ( -6.371969008298464132, 6.536311385877402458, 1.040834085586084257E-14 ) ) ;
#184940 = CARTESIAN_POINT ( 'NONE',  ( -1.500000000000008216, 12.03125000068279427, 3.469446951953614189E-15 ) ) ;
#184939 = CARTESIAN_POINT ( 'NONE',  ( -15.75000000000000000, 10.89999999999998259, 3.599999999999999201 ) ) ;
#184941 = ORIENTED_EDGE ( 'NONE', *, *, #199216, .T. ) ;
#184942 = CARTESIAN_POINT ( 'NONE',  ( 5.660779783930850684, 1.203351582566011047, 1.617819807990819481 ) ) ;
#184944 = CARTESIAN_POINT ( 'NONE',  ( 4.645415531332927728, 1.844630620182326153, -0.9228673458712335353 ) ) ;
#184943 = CARTESIAN_POINT ( 'NONE',  ( 3.974511587100456822, 7.788680618259193444, 1.040834085586084257E-14 ) ) ;
#184946 = CARTESIAN_POINT ( 'NONE',  ( -1.737499999999997824, -3.441666666666665986, 3.009438278150925683 ) ) ;
#184945 = CARTESIAN_POINT ( 'NONE',  ( 5.508355548902068577, 9.648441583686274470, 0.7998128361456331437 ) ) ;
#184947 = CARTESIAN_POINT ( 'NONE',  ( 6.282224075085741433, 8.422623735723785643, 1.599625672291268286 ) ) ;
#184948 = CARTESIAN_POINT ( 'NONE',  ( -3.285556943750000514, -0.8385416661887076240, -1.896917185911906500 ) ) ;
#184949 = CARTESIAN_POINT ( 'NONE',  ( 0.1331565106231571705, 4.092041177288479048, -2.500854978060399691 ) ) ;
#184950 = CARTESIAN_POINT ( 'NONE',  ( 0.2872076490801517279, 1.550519377178682268, 1.402564467939530823 ) ) ;
#184951 = CARTESIAN_POINT ( 'NONE',  ( 4.658827374183164949, 1.163267680695536876, 1.646840100852072997 ) ) ;
#184952 = CARTESIAN_POINT ( 'NONE',  ( 4.511176471348508521, -1.804767551675333204, 0.3638508048048467169 ) ) ;
#184953 = CARTESIAN_POINT ( 'NONE',  ( 6.491656622844908853, 6.468020902940851968, 0.7998128361456341429 ) ) ;
#184954 = PRESENTATION_STYLE_ASSIGNMENT (( #69065 ) ) ;
#184955 = CARTESIAN_POINT ( 'NONE',  ( 1.025878534523045449, 1.032422052977323590, -1.381481875464431797 ) ) ;
#184956 = CARTESIAN_POINT ( 'NONE',  ( 0.1457207355009884908, 1.993892511249679034, -0.3006540981884687214 ) ) ;
#184957 = CARTESIAN_POINT ( 'NONE',  ( 0.8976324851915818970, -1.040256531696292397, -2.049935236865876309 ) ) ;
#184958 = CARTESIAN_POINT ( 'NONE',  ( -5.442708600882160574, 8.437244903416123876, -1.199719254218446718 ) ) ;
#184959 = CARTESIAN_POINT ( 'NONE',  ( 0.8083708232014105155, -2.251370329867402376, 0.2228818479251652163 ) ) ;
#184960 = CARTESIAN_POINT ( 'NONE',  ( 2.789785578339375238, 1.489779160094312660, 1.488918557309417467 ) ) ;
#184961 = CARTESIAN_POINT ( 'NONE',  ( -6.310394152517827315, 6.326824364217716656, 0.7998128361456281477 ) ) ;
#184962 = CARTESIAN_POINT ( 'NONE',  ( 6.252281394196331554, 10.44607872653774372, 1.040834085586084257E-14 ) ) ;
#184963 = CARTESIAN_POINT ( 'NONE',  ( 5.600926855776875435, 7.627776979863398310, -1.443375672974078761 ) ) ;
#184964 = PRESENTATION_STYLE_ASSIGNMENT (( #186037 ) ) ;
#184965 = CARTESIAN_POINT ( 'NONE',  ( -4.076197739202962467, 7.907314462378773001, 1.040834085586084257E-14 ) ) ;
#184966 = CARTESIAN_POINT ( 'NONE',  ( 5.734735788456138295, 8.673980272298743799, -1.082531754730537976 ) ) ;
#184967 = CARTESIAN_POINT ( 'NONE',  ( 4.369547513234953939, 7.382648021784232739, 1.157447143386416188 ) ) ;
#184968 = EDGE_CURVE ( 'NONE', #97098, #207604, #97501, .T. ) ;
#184969 = CARTESIAN_POINT ( 'NONE',  ( -3.948449050077848632, 5.629609863222681199, 1.599625672291267398 ) ) ;
#184970 = CARTESIAN_POINT ( 'NONE',  ( 5.273765199871699672, 0.4330091245797212385, -2.178642023334904199 ) ) ;
#184971 = CARTESIAN_POINT ( 'NONE',  ( 2.238457302780196390, 0.4817095239468481283, 2.137691825660259948 ) ) ;
#184972 = CARTESIAN_POINT ( 'NONE',  ( -5.575427483717760424, 7.527751369135936343, 1.599625672291269396 ) ) ;
#184973 = CARTESIAN_POINT ( 'NONE',  ( -3.634467696915153034, 6.397906858779740524, 1.199719254218452935 ) ) ;
#184974 = CARTESIAN_POINT ( 'NONE',  ( 5.336364984333265227, -1.091323163865608459, 1.630109012322231266 ) ) ;
#184975 = CARTESIAN_POINT ( 'NONE',  ( -1.201851678989727383E-14, 1.571875000341420581, 1.575800808251672791 ) ) ;
#184976 = CARTESIAN_POINT ( 'NONE',  ( 6.890000000000039648, 4.701345932300413644, 2.282685536056531461 ) ) ;
#184978 = ORIENTED_EDGE ( 'NONE', *, *, #32633, .F. ) ;
#184977 = CARTESIAN_POINT ( 'NONE',  ( -4.419594888374909658, 8.100018436505289188, 0.7216878364870458196 ) ) ;
#184979 = CARTESIAN_POINT ( 'NONE',  ( 4.482752736079084421, -1.382999391253452615, 1.607682512923855445 ) ) ;
#184980 = CARTESIAN_POINT ( 'NONE',  ( -5.953438850176548947, 9.959779401932374654, 0.000000000000000000 ) ) ;
#184981 = ORIENTED_EDGE ( 'NONE', *, *, #77886, .T. ) ;
#184983 = CARTESIAN_POINT ( 'NONE',  ( 6.420800710400103917, 2.015122584031241004, 0.7829223626853940576 ) ) ;
#184982 = CARTESIAN_POINT ( 'NONE',  ( -4.963693636378939011, 8.805076652501815815, 0.7216878364870267237 ) ) ;
#184984 = CARTESIAN_POINT ( 'NONE',  ( 5.133733721068893807, 9.141106441222381918, 1.040834085586084257E-14 ) ) ;
#184985 = CARTESIAN_POINT ( 'NONE',  ( 4.845164456061270997, 0.5726227986864868003, -1.750029900461601340 ) ) ;
#184986 = UNCERTAINTY_MEASURE_WITH_UNIT (LENGTH_MEASURE( 1.000000000000000082E-05 ), #182006, 'distance_accuracy_value', 'NONE');
#184987 = CARTESIAN_POINT ( 'NONE',  ( -1.364683531249997417, 3.071875000341423245, 1.214306433183764966E-14 ) ) ;
#184988 = CARTESIAN_POINT ( 'NONE',  ( 0.8193799409778947940, 1.038239828973979373, -1.396697621350863505 ) ) ;
#184990 = EDGE_CURVE ( 'NONE', #184334, #197566, #146717, .T. ) ;
#184989 = CARTESIAN_POINT ( 'NONE',  ( 0.000000000000000000, -9.919999999999998153, 0.000000000000000000 ) ) ;
#184991 = CARTESIAN_POINT ( 'NONE',  ( -0.6823417656250246877, -0.8864583329919115684, 1.181850606188755259 ) ) ;
#184992 = CARTESIAN_POINT ( 'NONE',  ( 6.204464077730128757, 7.037555732820855781, 1.030856974308017149 ) ) ;
#184993 = CARTESIAN_POINT ( 'NONE',  ( 5.752838164830007983, -1.706859214253673152, 1.326403591387192771 ) ) ;
#184994 = EDGE_CURVE ( 'NONE', #160443, #65240, #82682, .T. ) ;
#184995 = CIRCLE ( 'NONE', #119372, 0.08000000000000040412 ) ;
#184996 = CARTESIAN_POINT ( 'NONE',  ( -2.923754682041362241, 6.562797562356882608, 0.7998128361456341429 ) ) ;
#184997 = CARTESIAN_POINT ( 'NONE',  ( -8.175203438916030407, 8.640084888264587093, 0.7216878364870578100 ) ) ;
#184998 = CARTESIAN_POINT ( 'NONE',  ( 5.190363053866647647, -2.144918610114197488, -0.2683968819863768451 ) ) ;
#184999 = CARTESIAN_POINT ( 'NONE',  ( -0.6823417656249969321, 3.717708333674754506, -1.181850606188749264 ) ) ;
#185000 = CARTESIAN_POINT ( 'NONE',  ( 5.096930449404251107, 1.640577245564038389, -1.092763768510503608 ) ) ;
#185001 = CARTESIAN_POINT ( 'NONE',  ( 4.059675810253587258, 1.465203325174119664, -0.9266335502581940498 ) ) ;
#185002 = TOROIDAL_SURFACE ( 'NONE', #39850, 1.829047314007947955, 0.05000000000000000278 ) ;
#185003 = CARTESIAN_POINT ( 'NONE',  ( 1.312353134292881141, 1.468346937154514364, -1.627112938194043235 ) ) ;
#185004 = CARTESIAN_POINT ( 'NONE',  ( 2.643975807074511408, -1.709602402607094396, -1.550068159870971574 ) ) ;
#185005 = CARTESIAN_POINT ( 'NONE',  ( 5.009085904467641015, 1.791045569760267631, 1.019200576588958240 ) ) ;
#185006 = CARTESIAN_POINT ( 'NONE',  ( 6.620655732516682157, 0.004685112605702904456, 1.926407831898164114 ) ) ;
#185007 = CARTESIAN_POINT ( 'NONE',  ( -7.985389288324710400, 8.418635045908049008, -0.7216878364870267237 ) ) ;
#185008 = CARTESIAN_POINT ( 'NONE',  ( -6.642568916052639771, 6.714361588341672515, 0.000000000000000000 ) ) ;
#185009 = DIRECTION ( 'NONE',  ( 0.000000000000000000, 0.000000000000000000, -1.000000000000000000 ) ) ;
#185010 = CARTESIAN_POINT ( 'NONE',  ( -6.195713011320795438, 8.251417818006149929, -1.443375672974058777 ) ) ;
#185011 = CARTESIAN_POINT ( 'NONE',  ( 3.417197246517459597, 1.994164043739574232, 0.9453733912969732867 ) ) ;
#185012 = CARTESIAN_POINT ( 'NONE',  ( 0.000000000000000000, -1.684374999522041172, -3.793834371823813001 ) ) ;
#185013 = CARTESIAN_POINT ( 'NONE',  ( 0.5669689972240202769, 1.615300940711749789, 0.9240007631576854230 ) ) ;
#185014 = AXIS2_PLACEMENT_3D ( 'NONE', #207113, #107557, #124891 ) ;
#185015 = CARTESIAN_POINT ( 'NONE',  ( 1.364853456228726225, 3.682974172409147595, -0.6233480900563427296 ) ) ;
#185016 = CARTESIAN_POINT ( 'NONE',  ( 0.7499999999999902300, 4.847916667349482012, -1.299038105676658228 ) ) ;
#185017 = CARTESIAN_POINT ( 'NONE',  ( 2.296870906627769049, 2.697687087511395632, -2.500000000000000444 ) ) ;
#185019 = DIRECTION ( 'NONE',  ( 1.276756478318932585E-15, -1.000000000000000000, 1.665334536937738262E-16 ) ) ;
#185018 = CARTESIAN_POINT ( 'NONE',  ( -4.780157383859068077, 8.266535928781179265, -0.8537241328121815132 ) ) ;
#185020 = CARTESIAN_POINT ( 'NONE',  ( 6.070224334863941529, -1.749758606415029449, -0.5730458292283467925 ) ) ;
#185021 = EDGE_LOOP ( 'NONE', ( #109677, #174157, #19703, #34835, #116629, #62322 ) ) ;
#185022 = CARTESIAN_POINT ( 'NONE',  ( 2.922786580453646366, 1.940006684909411971, 0.6957959148722169251 ) ) ;
#185023 = CARTESIAN_POINT ( 'NONE',  ( -0.6801582343750316451, 2.098958333674738608, -1.178068619123862515 ) ) ;
#185024 = UNCERTAINTY_MEASURE_WITH_UNIT (LENGTH_MEASURE( 1.000000000000000082E-05 ), #81896, 'distance_accuracy_value', 'NONE');
#185025 = CARTESIAN_POINT ( 'NONE',  ( -6.124532705071231931, 8.168374127381657246, -1.599625672291263179 ) ) ;
#185026 = CARTESIAN_POINT ( 'NONE',  ( 1.752609234595727816, 1.998021763388730720, 0.2939949305936078172 ) ) ;
#185027 = CARTESIAN_POINT ( 'NONE',  ( 1.499999999999987566, -0.7249999999999825473, 0.000000000000000000 ) ) ;
#185028 = CARTESIAN_POINT ( 'NONE',  ( 2.822068529938852155, 6.444163718237301275, -0.7998128361456291469 ) ) ;
#185029 = CARTESIAN_POINT ( 'NONE',  ( 1.762645127485995555, -1.458140857472267626, 1.456663342728149901 ) ) ;
#185031 = CARTESIAN_POINT ( 'NONE',  ( -1.364683531250000748, 13.60937500034139980, 0.000000000000000000 ) ) ;
#185030 = CARTESIAN_POINT ( 'NONE',  ( 0.000000000000000000, 2.499999999999998668, 0.000000000000000000 ) ) ;
#185032 = CARTESIAN_POINT ( 'NONE',  ( 7.481401836642521452, 7.622723652371411696, 1.040834085586084257E-14 ) ) ;
#185033 = FILL_AREA_STYLE ('',( #103816 ) ) ;
#185034 = CIRCLE ( 'NONE', #119415, 0.08000000000000020983 ) ;
#185035 = CARTESIAN_POINT ( 'NONE',  ( 5.057340365224886725, -1.863002784048470639, -1.182737378625432489 ) ) ;
#185036 = CARTESIAN_POINT ( 'NONE',  ( 1.599129061979026822, 1.768144091905754500, -1.243190488262067683 ) ) ;
#185037 = CARTESIAN_POINT ( 'NONE',  ( -5.477130870240893401, 6.452702772444876445, 1.082531754730548412 ) ) ;
#185038 = CARTESIAN_POINT ( 'NONE',  ( 0.3918150239524306189, -2.006371095615328226, 0.2024682584410575914 ) ) ;
#185039 = CARTESIAN_POINT ( 'NONE',  ( 2.003655084434956102, 2.273349380270474729, 0.3377564834418695927 ) ) ;
#185040 = DIRECTION ( 'NONE',  ( 0.000000000000000000, -1.000000000000000000, 0.000000000000000000 ) ) ;
#185041 = CARTESIAN_POINT ( 'NONE',  ( -0.4373225248172993851, -5.223431457505089526, -10.96785329849811497 ) ) ;
#185042 = CARTESIAN_POINT ( 'NONE',  ( 1.844607821789259638, 8.931289555339859021, -0.7749999999999996891 ) ) ;
#185043 = CARTESIAN_POINT ( 'NONE',  ( 1.762360912074714125, -1.325010844092512796, 1.320751239342173200 ) ) ;
#185044 = CARTESIAN_POINT ( 'NONE',  ( 3.573454097414618946, 1.463926983822515293, 1.387100322000796027 ) ) ;
#185046 = FACE_OUTER_BOUND ( 'NONE', #155631, .T. ) ;
#185045 = CARTESIAN_POINT ( 'NONE',  ( -0.6823417656250212460, 2.551041667008084435, 1.181850606188767472 ) ) ;
#185048 = CARTESIAN_POINT ( 'NONE',  ( 4.776057437618447921, 1.212020014983648863, 1.722159047642721541 ) ) ;
#185047 = CARTESIAN_POINT ( 'NONE',  ( -7.985916173649233230, 9.275655943134292869, -1.199719254218446718 ) ) ;
#185049 = CARTESIAN_POINT ( 'NONE',  ( 7.633404179693907388, 8.864391950186421454, -1.199719254218441611 ) ) ;
#185051 = CARTESIAN_POINT ( 'NONE',  ( -7.202405917357668663, 9.425892875049191488, 1.599625672291295375 ) ) ;
#185050 = CARTESIAN_POINT ( 'NONE',  ( 5.896870467300973750, 5.844380064798101237, 0.7998128361456352531 ) ) ;
#185052 = DIRECTION ( 'NONE',  ( 0.000000000000000000, 0.000000000000000000, -1.000000000000000000 ) ) ;
#185053 = CARTESIAN_POINT ( 'NONE',  ( 4.816668504955663899, -0.6845142050268312461, -1.900371106210005712 ) ) ;
#185054 = CARTESIAN_POINT ( 'NONE',  ( -1.500000000000001332, -1.068749999317178290, 0.000000000000000000 ) ) ;
#185055 = CARTESIAN_POINT ( 'NONE',  ( 1.252863987647494515, -0.4972004349026898362, -2.001653351804733028 ) ) ;
#185056 = CARTESIAN_POINT ( 'NONE',  ( 8.487040972474689582, 9.964264558384387627, -1.082531754730543083 ) ) ;
#185057 = EDGE_CURVE ( 'NONE', #24037, #10073, #111874, .T. ) ;
#185058 = CARTESIAN_POINT ( 'NONE',  ( 5.061990249855835344, 6.999017606288844284, -1.599625672291273171 ) ) ;
#185059 = CARTESIAN_POINT ( 'NONE',  ( -1.364683531250000748, -0.6781249996585803075, 0.000000000000000000 ) ) ;
#185061 = CARTESIAN_POINT ( 'NONE',  ( 8.832353407160718817, 3.956598013261175772, 7.432338980325266853 ) ) ;
#185060 = CARTESIAN_POINT ( 'NONE',  ( 4.044074958626150185, 7.940114228364351767, 0.7998128361456271485 ) ) ;
#185062 = CARTESIAN_POINT ( 'NONE',  ( 7.741342523278705201, 9.094283034322399928, 1.082531754730558626 ) ) ;
#185064 = CARTESIAN_POINT ( 'NONE',  ( -9.748756651352278979, 4.000007913748506283, -7.301653494139321410 ) ) ;
#185063 = CARTESIAN_POINT ( 'NONE',  ( 2.998652106967353514, 2.154486853421373027, 0.2683346083656880099 ) ) ;
#185066 = CARTESIAN_POINT ( 'NONE',  ( 2.331387312403776946, 0.8663521307504215008, -1.624669977836174839 ) ) ;
#185065 = CARTESIAN_POINT ( 'NONE',  ( -5.436456409399874623, 5.444880020495701523, 0.000000000000000000 ) ) ;
#185067 = CARTESIAN_POINT ( 'NONE',  ( 1.364683531249988535, 3.863541667008087543, 0.7879004041258500513 ) ) ;
#185068 = CARTESIAN_POINT ( 'NONE',  ( 4.318054327947466575, 1.347776305887092185, -1.728067674571641898 ) ) ;
#185069 = DIRECTION ( 'NONE',  ( 1.000000000000000000, 0.000000000000000000, -5.421010862427519212E-16 ) ) ;
#185070 = CARTESIAN_POINT ( 'NONE',  ( 4.557670991828286056, 0.4998169670675355336, -2.206472437794388952 ) ) ;
#185071 = CARTESIAN_POINT ( 'NONE',  ( -7.230575994789712801, 7.330093503543126054, 0.7998128361456341429 ) ) ;
#185072 = DIRECTION ( 'NONE',  ( -1.000000000000000000, 0.000000000000000000, 0.000000000000000000 ) ) ;
#185073 = CARTESIAN_POINT ( 'NONE',  ( 5.788239156490550208, 7.236076679697275083, -1.185412701995581797 ) ) ;
#185074 = CARTESIAN_POINT ( 'NONE',  ( -0.7500000000000179856, 13.54166666666666785, 1.299038105676658228 ) ) ;
#185075 = CARTESIAN_POINT ( 'NONE',  ( -4.950135482320914271, 8.789258806100786359, -0.7216878364870338292 ) ) ;
#185076 = CARTESIAN_POINT ( 'NONE',  ( 4.990809943606266508, 6.915973915664348937, -1.443375672974068769 ) ) ;
#185077 = EDGE_CURVE ( 'NONE', #59550, #155131, #67020, .T. ) ;
#185078 = CARTESIAN_POINT ( 'NONE',  ( 5.237463280334829996, -1.251769750873907849, -1.251277626909578222 ) ) ;
#185079 = CARTESIAN_POINT ( 'NONE',  ( 3.193996758133522018, 1.278685386795814560, 1.554813472153792286 ) ) ;
#185080 = CARTESIAN_POINT ( 'NONE',  ( 7.470706336329915764, 8.674577799595093452, -1.199719254218441611 ) ) ;
#185081 = CARTESIAN_POINT ( 'NONE',  ( 2.028482804581877019, 1.213238276247522895, -1.721163102310949045 ) ) ;
#185083 = CARTESIAN_POINT ( 'NONE',  ( 1.499999999999987121, 2.295833333333350268, -0.8660254037844262731 ) ) ;
#185082 = CARTESIAN_POINT ( 'NONE',  ( -1.364683531250010295, 11.63020833367472839, 0.7879004041258445001 ) ) ;
#185084 = CARTESIAN_POINT ( 'NONE',  ( 1.627339542692422869, 0.1479755015179542166, -1.964067387968527312 ) ) ;
#185085 = CARTESIAN_POINT ( 'NONE',  ( 0.7779422811538607707, -1.042605501850740080, 1.552959968518424771 ) ) ;
#185086 = CARTESIAN_POINT ( 'NONE',  ( 1.187862215860764126, -1.241893603568875903, -1.518774446641702580 ) ) ;
#185088 = ORIENTED_EDGE ( 'NONE', *, *, #200712, .T. ) ;
#185087 = CARTESIAN_POINT ( 'NONE',  ( 6.381129877538572970, -1.660329982341423705, -0.7251259014357125388 ) ) ;
#185089 = CARTESIAN_POINT ( 'NONE',  ( 6.656690234629796699, 6.868486149930637552, 1.040834085586084257E-14 ) ) ;
#185090 = CARTESIAN_POINT ( 'NONE',  ( -0.6823417656250003738, -0.2197916663252488800, -1.181850606188749264 ) ) ;
#185091 = CARTESIAN_POINT ( 'NONE',  ( 5.823093596695693819, -0.04436734784114480107, 1.870300906237104988 ) ) ;
#185092 = CARTESIAN_POINT ( 'NONE',  ( 5.664915734613278353, 1.571387620024040199, -1.347999112033698044 ) ) ;
#185093 = CARTESIAN_POINT ( 'NONE',  ( -4.285785955251283141, 8.014184357852876417, 0.000000000000000000 ) ) ;
#185094 = CARTESIAN_POINT ( 'NONE',  ( 0.07680821025393690105, 0.005952109439256307241, -1.810863387344714193 ) ) ;
#185095 = CARTESIAN_POINT ( 'NONE',  ( 0.7499999999999885647, 0.7333333333333567072, 1.299038105676657340 ) ) ;
#185096 = CARTESIAN_POINT ( 'NONE',  ( 6.564118927310645724, 10.80988918183778225, -0.7998128361456291469 ) ) ;
#185097 = CARTESIAN_POINT ( 'NONE',  ( -8.503988664269602538, 10.94440607977979063, 1.599625672291269396 ) ) ;
#185098 = CARTESIAN_POINT ( 'NONE',  ( 6.717138760927786834, 6.801359740696030443, -0.7998128361456481317 ) ) ;
#185099 = EDGE_CURVE ( 'NONE', #212450, #41218, #61236, .T. ) ;
#185100 = CARTESIAN_POINT ( 'NONE',  ( -1.364683531250000748, -0.4906249996585801409, 0.000000000000000000 ) ) ;
#185101 = CARTESIAN_POINT ( 'NONE',  ( -1.402160292154681736E-14, 0.5875000000000220046, -1.732050807568863648 ) ) ;
#185103 = CARTESIAN_POINT ( 'NONE',  ( 3.649115900372475796, 7.409052317076538330, 1.040834085586084257E-14 ) ) ;
#185102 = CARTESIAN_POINT ( 'NONE',  ( 4.896903505236655185, 0.3334610245491422265, 1.933150054703360432 ) ) ;
#185104 = EDGE_CURVE ( 'NONE', #22427, #129544, #77562, .T. ) ;
#185105 = CARTESIAN_POINT ( 'NONE',  ( 3.655624903986275154, -0.3905385215352343287, -1.977747697055858955 ) ) ;
#185106 = CARTESIAN_POINT ( 'NONE',  ( 2.307709453281155731, -1.106667911223922829, -1.563510803672981231 ) ) ;
#185107 = DIRECTION ( 'NONE',  ( 0.000000000000000000, 0.000000000000000000, 1.000000000000000000 ) ) ;
#185108 = CARTESIAN_POINT ( 'NONE',  ( 0.2928600448571065940, 1.818678932476354149, -1.222557900829209121 ) ) ;
#185109 = CARTESIAN_POINT ( 'NONE',  ( 0.2331713839410628208, 0.2432647426263275514, -1.987790486660771627 ) ) ;
#185110 = CARTESIAN_POINT ( 'NONE',  ( 2.213927045526514537, -0.8776910013945339317, -1.651823421649289081 ) ) ;
#185111 = CARTESIAN_POINT ( 'NONE',  ( -1.500000000000001332, -0.3187499993171846735, 0.000000000000000000 ) ) ;
#185112 = CARTESIAN_POINT ( 'NONE',  ( 3.744393049878576463, 1.073438034848249290, -1.702967747733853843 ) ) ;
#185113 = CARTESIAN_POINT ( 'NONE',  ( -7.531718027591449705, 8.745758106066849891, 1.199719254218462483 ) ) ;
#185115 = CARTESIAN_POINT ( 'NONE',  ( 4.587589571003643840, -0.5631140419127963481, 2.040926637660822163 ) ) ;
#185114 = CARTESIAN_POINT ( 'NONE',  ( -4.609409038966234995, 7.361099064560491456, -1.082531754730549967 ) ) ;
#185117 = AXIS2_PLACEMENT_3D ( 'NONE', #103053, #120440, #203715 ) ;
#185116 = DIRECTION ( 'NONE',  ( 0.7592566023653004592, 0.6507913734559639396, 0.000000000000000000 ) ) ;
#185118 = CARTESIAN_POINT ( 'NONE',  ( 5.740704066448026666, -2.019076491677873619, -0.4572469816465085657 ) ) ;
#185120 = CARTESIAN_POINT ( 'NONE',  ( 6.620655732516649294, 2.950034989283246478, 2.626075342966327497 ) ) ;
#185119 = CARTESIAN_POINT ( 'NONE',  ( 1.558266987246118562, -1.476132899515494534, 1.480894285863892934 ) ) ;
#185122 = VERTEX_POINT ( 'NONE', #175007 ) ;
#185121 = CARTESIAN_POINT ( 'NONE',  ( 6.440460073785046369, 1.806197173870389694, 0.2645596887278709453 ) ) ;
#185123 = CARTESIAN_POINT ( 'NONE',  ( 7.100719765255169236, 9.307259030929609267, -1.599625672291262513 ) ) ;
#185124 = CARTESIAN_POINT ( 'NONE',  ( 6.825078400183575589, -0.005632053428735600553, 2.144262460745151255 ) ) ;
#185125 = CARTESIAN_POINT ( 'NONE',  ( -0.07971467182326515133, -9.904506264776385294, -9.499665578938831345 ) ) ;
#185126 = CARTESIAN_POINT ( 'NONE',  ( -9.470186914265017464, 4.005096909781187264, 6.837150237413082365 ) ) ;
#185127 = CARTESIAN_POINT ( 'NONE',  ( 6.358410854684775515, 8.441231968597481483, -1.443375672974058777 ) ) ;
#185128 = CARTESIAN_POINT ( 'NONE',  ( -1.911175648939861693, 3.243131119507702387, 0.4542559028653238573 ) ) ;
#185130 = CARTESIAN_POINT ( 'NONE',  ( 0.9085206565882588681, -0.4392767353821840914, -1.757246876086359988 ) ) ;
#185129 = CARTESIAN_POINT ( 'NONE',  ( 7.856023664475727308, 8.130058794835305136, -0.7998128361456341429 ) ) ;
#185131 = CARTESIAN_POINT ( 'NONE',  ( -8.019811557683421910, 9.315200557840817908, 1.199719254218462483 ) ) ;
#185132 = CARTESIAN_POINT ( 'NONE',  ( 6.017121246366603060, 5.914396297049491658, 1.040834085586084257E-14 ) ) ;
#185133 = CARTESIAN_POINT ( 'NONE',  ( -6.875062624577635617, -8.049367966558001797, 6.605500049835224097 ) ) ;
#185134 = CARTESIAN_POINT ( 'NONE',  ( 4.029290343944737174, 7.554674111305462070, -0.3786771240106376890 ) ) ;
#185135 = CARTESIAN_POINT ( 'NONE',  ( 3.684065054611349144, 5.321161868511784299, -1.599625672291262513 ) ) ;
#185136 = ORIENTED_EDGE ( 'NONE', *, *, #207358, .T. ) ;
#185137 = CARTESIAN_POINT ( 'NONE',  ( 5.976185453469534892, -2.006962702346287930, -0.1948244327795861652 ) ) ;
#185138 = CARTESIAN_POINT ( 'NONE',  ( 0.8211285067932658777, 1.603129840700336928, -1.388046135824993366 ) ) ;
#185139 = MECHANICAL_DESIGN_GEOMETRIC_PRESENTATION_REPRESENTATION (  '', ( #164440 ), #1908 ) ;
#185140 = DIRECTION ( 'NONE',  ( 3.330669073875478989E-16, -3.540251991789410786E-16, -1.000000000000000000 ) ) ;
#185141 = CARTESIAN_POINT ( 'NONE',  ( 0.1405533004714097089, -0.003749010675423158478, -2.279853246149381452 ) ) ;
#185142 = CARTESIAN_POINT ( 'NONE',  ( 7.550983558724436051, -6.148216694138042726, 7.550983558724430722 ) ) ;
#185143 =( BOUNDED_CURVE ( )  B_SPLINE_CURVE ( 2, ( #209436, #63210, #127240, #212643, #64285, #128313, #147676 ),
 .UNSPECIFIED., .F., .T. ) 
 B_SPLINE_CURVE_WITH_KNOTS ( ( 3, 2, 2, 3 ),
 ( 0.2375000000000001832, 0.2416666666666668906, 0.2458333333333335702, 0.2500000000000002776 ),
 .UNSPECIFIED. ) 
 CURVE ( )  GEOMETRIC_REPRESENTATION_ITEM ( )  RATIONAL_B_SPLINE_CURVE ( ( 0.9999999999999937828, 0.8660254037844449249, 1.000000000000000000, 0.8660254037844387076, 1.000000000000000000, 0.8660254037844298258, 1.000000000000008882 ) ) 
 REPRESENTATION_ITEM ( '' )  );
#185144 = CARTESIAN_POINT ( 'NONE',  ( -4.934804725694231564, 5.819988937140460727, -1.082531754730544860 ) ) ;
#185145 = CIRCLE ( 'NONE', #39993, 11.09999999999999964 ) ;
#185146 = CARTESIAN_POINT ( 'NONE',  ( 9.571693261567961741, 11.22969222899322617, 1.082531754730548412 ) ) ;
#185147 = CARTESIAN_POINT ( 'NONE',  ( 3.432427499664345127, -1.176894005904068896, 1.578936197102176031 ) ) ;
#185148 = CARTESIAN_POINT ( 'NONE',  ( 4.218375177057286152, 1.978055892313890229, 0.3905773888849966013 ) ) ;
#185149 = CARTESIAN_POINT ( 'NONE',  ( -6.612626235163205024, 8.737816579155630592, -1.599625672291263179 ) ) ;
#185150 =( LENGTH_UNIT ( ) NAMED_UNIT ( * ) SI_UNIT ( .MILLI., .METRE. ) );
#185151 = CARTESIAN_POINT ( 'NONE',  ( -9.499562802171206854, -9.415754203682764611, 0.1226201807150902046 ) ) ;
#185152 = CARTESIAN_POINT ( 'NONE',  ( 4.295009486468337023, 1.759388067201245187, 1.306329983072423984 ) ) ;
#185153 = CARTESIAN_POINT ( 'NONE',  ( 0.6823417656249882723, 2.988541667008084879, -1.181850606188754593 ) ) ;
#185154 = CARTESIAN_POINT ( 'NONE',  ( 3.416937173653651794, 1.740928992956072952, 0.8250102540389223638 ) ) ;
#185155 = CARTESIAN_POINT ( 'NONE',  ( -8.355902744723985975, 8.642974711799791265, 1.040834085586084257E-14 ) ) ;
#185156 = CARTESIAN_POINT ( 'NONE',  ( -0.1296875068448159751, 0.001480089298542403009, -1.826395826379861864 ) ) ;
#185157 = CARTESIAN_POINT ( 'NONE',  ( 0.2939702064862387831, 1.638257335637434364, 1.478849500172851217 ) ) ;
#185158 = FACE_OUTER_BOUND ( 'NONE', #204272, .T. ) ;
#185159 = EDGE_LOOP ( 'NONE', ( #90021, #47579, #115221 ) ) ;
#185161 =( BOUNDED_SURFACE ( )  B_SPLINE_SURFACE ( 3, 2, ( 
 ( #166977, #183209, #103036 ),
 ( #36956, #18568, #200508 ),
 ( #168033, #66228, #48966 ),
 ( #133437, #182131, #67298 ),
 ( #83574, #149655, #199444 ),
 ( #70497, #69438, #201569 ),
 ( #84644, #150735, #115084 ),
 ( #51087, #53215, #148592 ) ),
 .UNSPECIFIED., .F., .F., .F. ) 
 B_SPLINE_SURFACE_WITH_KNOTS ( ( 4, 2, 2, 4 ),
 ( 3, 3 ),
 ( 0.000000000000000000, 0.0002469787127373868161, 0.0004939574254747736322, 0.0009879148509495472644 ),
 ( 0.000000000000000000, 1.000000000000000000 ),
 .UNSPECIFIED. ) 
 GEOMETRIC_REPRESENTATION_ITEM ( )  RATIONAL_B_SPLINE_SURFACE ( (
 ( 1.000000000000000000, 0.3826834323650769032, 1.000000000000000000),
 ( 1.000000000000000000, 0.3798541548344007701, 1.000000000000000000),
 ( 1.000000000000000000, 0.3995981355978897587, 1.000000000000000000),
 ( 1.000000000000000000, 0.4556299950042955182, 1.000000000000000000),
 ( 1.000000000000000000, 0.4903550589607370558, 1.000000000000000000),
 ( 1.000000000000000000, 0.5915489574622737612, 1.000000000000000000),
 ( 1.000000000000000000, 0.6554239218402749811, 1.000000000000000000),
 ( 1.000000000000000000, 0.7100530722070640399, 1.000000000000000000) ) ) 
 REPRESENTATION_ITEM ( '' )  SURFACE ( )  );
#185160 = CARTESIAN_POINT ( 'NONE',  ( 4.340018570150304456, 6.156717313299049366, -1.443375672974068769 ) ) ;
#185162 = CARTESIAN_POINT ( 'NONE',  ( 4.627768981117735159, 1.911305289405954344, -0.4745475857620209958 ) ) ;
#185164 = CARTESIAN_POINT ( 'NONE',  ( 4.547525146836687959, -1.839596654198237369, 0.8179813495266550216 ) ) ;
#185163 = CARTESIAN_POINT ( 'NONE',  ( 0.2044968316872765035, 1.690132753820037692, 0.9564217018903762302 ) ) ;
#185165 = CARTESIAN_POINT ( 'NONE',  ( 5.501416862357105586, 2.263058191380825424, 0.4008149593560642598 ) ) ;
#185167 = CARTESIAN_POINT ( 'NONE',  ( 3.977287768980780402, -0.1405865315737795385, 1.855722876009910038 ) ) ;
#185166 = CARTESIAN_POINT ( 'NONE',  ( -4.327421261425478782, 8.660439569662104375, -0.7750000000000001332 ) ) ;
#185168 = CARTESIAN_POINT ( 'NONE',  ( 7.550965208168244125, 7.774157262476569130, -0.7998128361456341429 ) ) ;
#185169 = CYLINDRICAL_SURFACE ( 'NONE', #188475, 1.224999999999996980 ) ;
#185170 = DIRECTION ( 'NONE',  ( -0.000000000000000000, 0.000000000000000000, -1.000000000000000000 ) ) ;
#185171 = CARTESIAN_POINT ( 'NONE',  ( -7.528855374290365887, 7.678086112960552434, -0.7998128361456291469 ) ) ;
#185172 = CARTESIAN_POINT ( 'NONE',  ( -3.472296738875691346, 6.104744391113324120, 1.082531754730549967 ) ) ;
#185173 = CARTESIAN_POINT ( 'NONE',  ( 0.4510473619779230003, -1.854578567552306767, -1.167393260480112493 ) ) ;
#185174 = CARTESIAN_POINT ( 'NONE',  ( 4.839897650398541806, 8.590371658866210680, 1.040834085586084257E-14 ) ) ;
#185175 = VERTEX_POINT ( 'NONE', #26593 ) ;
#185176 = CARTESIAN_POINT ( 'NONE',  ( -15.75000000000000000, 13.39999999999998259, 3.599999999999999201 ) ) ;
#185178 =( BOUNDED_SURFACE ( )  B_SPLINE_SURFACE ( 1, 2, ( 
 ( #22473, #153575, #141634, #9450, #55007, #71221, #24618, #173036, #154642, #53938, #186050, #7292, #124363, #41979, #21401, #23548, #88584, #138401, #140562, #90726, #75521, #190320, #204420, #73370, #108089, #25691, #187124, #120074, #171959, #37685, #169813, #6223, #104836, #205504, #188191, #139475, #189267, #170881, #72293, #56075, #39826, #76579, #113428, #159974, #61406, #92863, #210842, #62468, #11578, #77649, #143771, #94996, #63540, #29979, #128630, #111292, #80859, #109163, #209765, #28911, #27837, #127568, #158910, #43050, #78708, #110227, #207642, #176235, #193537, #96065, #161042, #31055, #194597, #45179, #12637, #79780, #144834, #195678, #177297, #46241, #112358, #162117, #178371, #13707, #145892, #211903, #129695, #47314, #26762, #191384, #208701, #179434, #59261, #97131, #10506, #163183, #142691, #14768, #125418, #175174, #60328, #126489, #192452, #44106, #93933, #36345, #150126, #147999, #1699, #146949, #98190, #32105, #151190, #212964, #65632, #134953, #115541, #117682, #130743, #67753, #133903, #199910, #164238, #197783, #15826, #81911, #64602, #180486, #33164, #2762, #50483, #17950, #166360, #149043, #34220, #183674, #131780, #618, #20091, #196736, #35278, #48377, #101355, #181536, #49421, #114489, #165294, #132833, #66686, #200961, #184721, #52608, #116603, #84037, #99245, #51556, #214009, #16888, #198837, #82970, #182597, #100293, #167433, #19025, #85105, #68831, #118737, #102423, #168491, #56879, #120893, #138144, #5961, #40649, #41725, #190073, #69893, #106752, #8120, #104575, #169559, #170620, #154384, #57945, #23286, #87244, #39560, #105662, #152248, #37422, #107835, #153310, #89398, #204154, #186867, #136005, #72032, #124110, #103498, #38497, #24353, #202018, #21141, #119809, #55809, #70963, #172779, #121963, #90462, #155446, #4885, #156529, #137073, #74207, #203098, #187930, #53677, #54743, #73107, #173860, #140302, #189008, #171689, #86178, #139207, #22207, #7030, #206320, #205238, #3821, #88320, #123054, #185788, #128381, #109973, #209507, #160789, #61147, #193280, #44925, #59012 ),
 ( #177039, #12381, #92614, #145651, #78461, #208443, #125169, #113174, #129445, #108903, #191128, #210593, #144579, #126235, #25436, #157601, #111033, #95811, #13457, #207392, #127309, #60077, #175984, #112111, #62223, #47057, #194348, #27577, #28656, #79533, #211647, #174926, #45990, #143511, #178114, #75267, #192195, #42794, #94742, #93676, #29729, #161867, #10256, #141382, #76330, #63283, #26506, #195427, #43859, #159718, #158657, #91542, #9196, #11316, #77395, #142436, #69380, #37978, #4371, #36896, #85653, #55295, #80603, #184209, #3310, #2239, #200450, #133379, #14511, #53158, #84591, #179177, #150678, #101910, #135488, #162930, #67244, #30801, #71515, #51030, #1180, #152791, #20633, #68316, #96880, #146698, #201510, #104051, #170097, #199384, #151740, #134447, #52096, #54230, #86722, #203644, #169036, #118223, #119287, #21683, #87793, #117153, #70441, #185273, #120368, #183156, #35832, #34759, #102978, #167975, #136557, #202578, #166918, #100833, #18512, #186343, #19581, #153867, #5436, #137627, #6515, #124647, #190604, #139768, #205794, #57424, #8663, #191665, #158139, #42262, #24906, #208979, #22760, #123586, #157074, #155997, #189549, #72591, #171170, #206859, #23839, #121445, #89947, #41197, #74743, #105130, #175454, #92082, #7584, #207925, #88877, #75805, #43329, #107304, #204709, #173328, #91012, #93147, #58491, #122522, #140847, #108375, #187414, #138692, #10785, #188485, #174398, #25976, #73669, #154930, #9730, #141913, #56359, #40115, #59547, #125706, #159184, #39045, #172252, #109447, #27038, #106226, #76860, #142979, #60616, #195964, #164523, #131025, #62742, #163466, #177581, #146167, #80065, #129977, #63819, #13981, #31334, #176509, #212182, #47599, #127858, #180765, #113713, #29195, #48652, #32393, #144055, #179717, #178651, #147224, #110509, #95284, #160255, #97411, #128902, #30262, #15046, #45457, #28121, #111573, #213249, #210050, #98459, #12916, #194883, #11856, #81139, #64879, #78996, #145112, #211118, #162403, #197016, #114769, #16108, #96348, #148286, #94215, #46520, #82192, #161332 ) ),
 .UNSPECIFIED., .F., .F., .F. ) 
 B_SPLINE_SURFACE_WITH_KNOTS ( ( 2, 2 ),
 ( 3, 2, 2, 2, 2, 2, 2, 2, 2, 2, 2, 2, 2, 2, 2, 2, 2, 2, 2, 2, 2, 2, 2, 2, 2, 2, 2, 2, 2, 2, 2, 2, 2, 2, 2, 2, 2, 2, 2, 2, 2, 2, 2, 2, 2, 2, 2, 2, 2, 2, 2, 2, 2, 2, 2, 2, 2, 2, 2, 2, 2, 2, 2, 2, 2, 2, 2, 2, 2, 2, 2, 2, 2, 2, 2, 2, 2, 2, 2, 2, 2, 2, 2, 2, 2, 2, 2, 2, 2, 2, 2, 2, 2, 2, 2, 2, 2, 2, 2, 2, 2, 2, 2, 2, 2, 2, 2, 2, 2, 2, 2, 2, 2, 2, 2, 2, 2, 2, 2, 2, 3 ),
 ( 0.000000000000000000, 1.000000000000000000 ),
 ( 0.000000000000000000, 0.008333333333333333218, 0.01666666666666666644, 0.02500000000000000139, 0.03333333333333333287, 0.04166666666666666435, 0.05000000000000000278, 0.05833333333333333426, 0.06666666666666666574, 0.07499999999999999722, 0.08333333333333332871, 0.09166666666666666019, 0.1000000000000000056, 0.1083333333333333370, 0.1166666666666666685, 0.1250000000000000000, 0.1333333333333333315, 0.1416666666666666630, 0.1499999999999999944, 0.1583333333333333259, 0.1666666666666666574, 0.1749999999999999889, 0.1833333333333333204, 0.1916666666666666796, 0.2000000000000000111, 0.2083333333333333426, 0.2166666666666666741, 0.2250000000000000056, 0.2333333333333333370, 0.2416666666666666685, 0.2500000000000000000, 0.2583333333333333592, 0.2666666666666666630, 0.2750000000000000222, 0.2833333333333333259, 0.2916666666666666852, 0.2999999999999999889, 0.3083333333333333481, 0.3166666666666666519, 0.3250000000000000111, 0.3333333333333333148, 0.3416666666666666741, 0.3499999999999999778, 0.3583333333333333370, 0.3666666666666666408, 0.3750000000000000000, 0.3833333333333333592, 0.3916666666666666630, 0.4000000000000000222, 0.4083333333333333259, 0.4166666666666666852, 0.4249999999999999889, 0.4333333333333333481, 0.4416666666666666519, 0.4500000000000000111, 0.4583333333333333148, 0.4666666666666666741, 0.4749999999999999778, 0.4833333333333333370, 0.4916666666666666408, 0.5000000000000000000, 0.5083333333333333037, 0.5166666666666667185, 0.5250000000000000222, 0.5333333333333333259, 0.5416666666666666297, 0.5500000000000000444, 0.5583333333333333481, 0.5666666666666666519, 0.5749999999999999556, 0.5833333333333333703, 0.5916666666666666741, 0.5999999999999999778, 0.6083333333333332815, 0.6166666666666666963, 0.6250000000000000000, 0.6333333333333333037, 0.6416666666666667185, 0.6500000000000000222, 0.6583333333333333259, 0.6666666666666666297, 0.6750000000000000444, 0.6833333333333333481, 0.6916666666666666519, 0.6999999999999999556, 0.7083333333333333703, 0.7166666666666666741, 0.7249999999999999778, 0.7333333333333332815, 0.7416666666666666963, 0.7500000000000000000, 0.7583333333333333037, 0.7666666666666667185, 0.7750000000000000222, 0.7833333333333333259, 0.7916666666666666297, 0.8000000000000000444, 0.8083333333333333481, 0.8166666666666666519, 0.8249999999999999556, 0.8333333333333333703, 0.8416666666666666741, 0.8499999999999999778, 0.8583333333333332815, 0.8666666666666666963, 0.8750000000000000000, 0.8833333333333333037, 0.8916666666666667185, 0.9000000000000000222, 0.9083333333333333259, 0.9166666666666666297, 0.9250000000000000444, 0.9333333333333333481, 0.9416666666666666519, 0.9499999999999999556, 0.9583333333333333703, 0.9666666666666666741, 0.9749999999999999778, 0.9833333333333332815, 0.9916666666666666963, 1.000000000000000000 ),
 .UNSPECIFIED. ) 
 GEOMETRIC_REPRESENTATION_ITEM ( )  RATIONAL_B_SPLINE_SURFACE ( (
 ( 1.000000000000000000, 0.8660254037844387076, 1.000000000000000000, 0.8660254037844387076, 1.000000000000000000, 0.8660254037844387076, 1.000000000000000000, 0.8660254037844387076, 1.000000000000000000, 0.8660254037844387076, 1.000000000000000000, 0.8660254037844387076, 1.000000000000000000, 0.8660254037844387076, 1.000000000000000000, 0.8660254037844387076, 1.000000000000000000, 0.8660254037844387076, 1.000000000000000000, 0.8660254037844387076, 1.000000000000000000, 0.8660254037844387076, 1.000000000000000000, 0.8660254037844387076, 1.000000000000000000, 0.8660254037844387076, 1.000000000000000000, 0.8660254037844387076, 1.000000000000000000, 0.8660254037844387076, 1.000000000000000000, 0.8660254037844387076, 1.000000000000000000, 0.8660254037844387076, 1.000000000000000000, 0.8660254037844387076, 1.000000000000000000, 0.8660254037844387076, 1.000000000000000000, 0.8660254037844387076, 1.000000000000000000, 0.8660254037844387076, 1.000000000000000000, 0.8660254037844387076, 1.000000000000000000, 0.8660254037844387076, 1.000000000000000000, 0.8660254037844387076, 1.000000000000000000, 0.8660254037844387076, 1.000000000000000000, 0.8660254037844387076, 1.000000000000000000, 0.8660254037844387076, 1.000000000000000000, 0.8660254037844387076, 1.000000000000000000, 0.8660254037844387076, 1.000000000000000000, 0.8660254037844387076, 1.000000000000000000, 0.8660254037844387076, 1.000000000000000000, 0.8660254037844387076, 1.000000000000000000, 0.8660254037844387076, 1.000000000000000000, 0.8660254037844387076, 1.000000000000000000, 0.8660254037844387076, 1.000000000000000000, 0.8660254037844387076, 1.000000000000000000, 0.8660254037844387076, 1.000000000000000000, 0.8660254037844387076, 1.000000000000000000, 0.8660254037844387076, 1.000000000000000000, 0.8660254037844387076, 1.000000000000000000, 0.8660254037844387076, 1.000000000000000000, 0.8660254037844387076, 1.000000000000000000, 0.8660254037844387076, 1.000000000000000000, 0.8660254037844387076, 1.000000000000000000, 0.8660254037844387076, 1.000000000000000000, 0.8660254037844387076, 1.000000000000000000, 0.8660254037844387076, 1.000000000000000000, 0.8660254037844387076, 1.000000000000000000, 0.8660254037844387076, 1.000000000000000000, 0.8660254037844387076, 1.000000000000000000, 0.8660254037844387076, 1.000000000000000000, 0.8660254037844387076, 1.000000000000000000, 0.8660254037844387076, 1.000000000000000000, 0.8660254037844387076, 1.000000000000000000, 0.8660254037844387076, 1.000000000000000000, 0.8660254037844387076, 1.000000000000000000, 0.8660254037844387076, 1.000000000000000000, 0.8660254037844387076, 1.000000000000000000, 0.8660254037844387076, 1.000000000000000000, 0.8660254037844387076, 1.000000000000000000, 0.8660254037844387076, 1.000000000000000000, 0.8660254037844387076, 1.000000000000000000, 0.8660254037844387076, 1.000000000000000000, 0.8660254037844387076, 1.000000000000000000, 0.8660254037844387076, 1.000000000000000000, 0.8660254037844387076, 1.000000000000000000, 0.8660254037844387076, 1.000000000000000000, 0.8660254037844387076, 1.000000000000000000, 0.8660254037844387076, 1.000000000000000000, 0.8660254037844387076, 1.000000000000000000, 0.8660254037844387076, 1.000000000000000000, 0.8660254037844387076, 1.000000000000000000, 0.8660254037844387076, 1.000000000000000000, 0.8660254037844387076, 1.000000000000000000, 0.8660254037844387076, 1.000000000000000000, 0.8660254037844387076, 1.000000000000000000, 0.8660254037844387076, 1.000000000000000000, 0.8660254037844387076, 1.000000000000000000, 0.8660254037844387076, 1.000000000000000000, 0.8660254037844387076, 1.000000000000000000, 0.8660254037844387076, 1.000000000000000000, 0.8660254037844387076, 1.000000000000000000, 0.8660254037844387076, 1.000000000000000000, 0.8660254037844387076, 1.000000000000000000, 0.8660254037844387076, 1.000000000000000000, 0.8660254037844387076, 1.000000000000000000, 0.8660254037844387076, 1.000000000000000000, 0.8660254037844387076, 1.000000000000000000, 0.8660254037844387076, 1.000000000000000000, 0.8660254037844387076, 1.000000000000000000, 0.8660254037844387076, 1.000000000000000000, 0.8660254037844387076, 1.000000000000000000, 0.8660254037844387076, 1.000000000000000000, 0.8660254037844387076, 1.000000000000000000, 0.8660254037844387076, 1.000000000000000000, 0.8660254037844387076, 1.000000000000000000, 0.8660254037844387076, 1.000000000000000000, 0.8660254037844387076, 1.000000000000000000, 0.8660254037844387076, 1.000000000000000000, 0.8660254037844387076, 1.000000000000000000, 0.8660254037844387076, 1.000000000000000000, 0.8660254037844387076, 1.000000000000000000, 0.8660254037844387076, 1.000000000000000000, 0.8660254037844387076, 1.000000000000000000, 0.8660254037844387076, 1.000000000000000000, 0.8660254037844387076, 1.000000000000000000, 0.8660254037844387076, 1.000000000000000000, 0.8660254037844387076, 1.000000000000000000, 0.8660254037844387076, 1.000000000000000000, 0.8660254037844387076, 1.000000000000000000, 0.8660254037844387076, 1.000000000000000000, 0.8660254037844387076, 1.000000000000000000, 0.8660254037844387076, 1.000000000000000000, 0.8660254037844387076, 1.000000000000000000, 0.8660254037844387076, 1.000000000000000000, 0.8660254037844387076, 1.000000000000000000, 0.8660254037844387076, 1.000000000000000000, 0.8660254037844387076, 1.000000000000000000, 0.8660254037844387076, 1.000000000000000000, 0.8660254037844387076, 1.000000000000000000),
 ( 1.000000000000000000, 0.8660254037844387076, 1.000000000000000000, 0.8660254037844387076, 1.000000000000000000, 0.8660254037844387076, 1.000000000000000000, 0.8660254037844387076, 1.000000000000000000, 0.8660254037844387076, 1.000000000000000000, 0.8660254037844387076, 1.000000000000000000, 0.8660254037844387076, 1.000000000000000000, 0.8660254037844387076, 1.000000000000000000, 0.8660254037844387076, 1.000000000000000000, 0.8660254037844387076, 1.000000000000000000, 0.8660254037844387076, 1.000000000000000000, 0.8660254037844387076, 1.000000000000000000, 0.8660254037844387076, 1.000000000000000000, 0.8660254037844387076, 1.000000000000000000, 0.8660254037844387076, 1.000000000000000000, 0.8660254037844387076, 1.000000000000000000, 0.8660254037844387076, 1.000000000000000000, 0.8660254037844387076, 1.000000000000000000, 0.8660254037844387076, 1.000000000000000000, 0.8660254037844387076, 1.000000000000000000, 0.8660254037844387076, 1.000000000000000000, 0.8660254037844387076, 1.000000000000000000, 0.8660254037844387076, 1.000000000000000000, 0.8660254037844387076, 1.000000000000000000, 0.8660254037844387076, 1.000000000000000000, 0.8660254037844387076, 1.000000000000000000, 0.8660254037844387076, 1.000000000000000000, 0.8660254037844387076, 1.000000000000000000, 0.8660254037844387076, 1.000000000000000000, 0.8660254037844387076, 1.000000000000000000, 0.8660254037844387076, 1.000000000000000000, 0.8660254037844387076, 1.000000000000000000, 0.8660254037844387076, 1.000000000000000000, 0.8660254037844387076, 1.000000000000000000, 0.8660254037844387076, 1.000000000000000000, 0.8660254037844387076, 1.000000000000000000, 0.8660254037844387076, 1.000000000000000000, 0.8660254037844387076, 1.000000000000000000, 0.8660254037844387076, 1.000000000000000000, 0.8660254037844387076, 1.000000000000000000, 0.8660254037844387076, 1.000000000000000000, 0.8660254037844387076, 1.000000000000000000, 0.8660254037844387076, 1.000000000000000000, 0.8660254037844387076, 1.000000000000000000, 0.8660254037844387076, 1.000000000000000000, 0.8660254037844387076, 1.000000000000000000, 0.8660254037844387076, 1.000000000000000000, 0.8660254037844387076, 1.000000000000000000, 0.8660254037844387076, 1.000000000000000000, 0.8660254037844387076, 1.000000000000000000, 0.8660254037844387076, 1.000000000000000000, 0.8660254037844387076, 1.000000000000000000, 0.8660254037844387076, 1.000000000000000000, 0.8660254037844387076, 1.000000000000000000, 0.8660254037844387076, 1.000000000000000000, 0.8660254037844387076, 1.000000000000000000, 0.8660254037844387076, 1.000000000000000000, 0.8660254037844387076, 1.000000000000000000, 0.8660254037844387076, 1.000000000000000000, 0.8660254037844387076, 1.000000000000000000, 0.8660254037844387076, 1.000000000000000000, 0.8660254037844387076, 1.000000000000000000, 0.8660254037844387076, 1.000000000000000000, 0.8660254037844387076, 1.000000000000000000, 0.8660254037844387076, 1.000000000000000000, 0.8660254037844387076, 1.000000000000000000, 0.8660254037844387076, 1.000000000000000000, 0.8660254037844387076, 1.000000000000000000, 0.8660254037844387076, 1.000000000000000000, 0.8660254037844387076, 1.000000000000000000, 0.8660254037844387076, 1.000000000000000000, 0.8660254037844387076, 1.000000000000000000, 0.8660254037844387076, 1.000000000000000000, 0.8660254037844387076, 1.000000000000000000, 0.8660254037844387076, 1.000000000000000000, 0.8660254037844387076, 1.000000000000000000, 0.8660254037844387076, 1.000000000000000000, 0.8660254037844387076, 1.000000000000000000, 0.8660254037844387076, 1.000000000000000000, 0.8660254037844387076, 1.000000000000000000, 0.8660254037844387076, 1.000000000000000000, 0.8660254037844387076, 1.000000000000000000, 0.8660254037844387076, 1.000000000000000000, 0.8660254037844387076, 1.000000000000000000, 0.8660254037844387076, 1.000000000000000000, 0.8660254037844387076, 1.000000000000000000, 0.8660254037844387076, 1.000000000000000000, 0.8660254037844387076, 1.000000000000000000, 0.8660254037844387076, 1.000000000000000000, 0.8660254037844387076, 1.000000000000000000, 0.8660254037844387076, 1.000000000000000000, 0.8660254037844387076, 1.000000000000000000, 0.8660254037844387076, 1.000000000000000000, 0.8660254037844387076, 1.000000000000000000, 0.8660254037844387076, 1.000000000000000000, 0.8660254037844387076, 1.000000000000000000, 0.8660254037844387076, 1.000000000000000000, 0.8660254037844387076, 1.000000000000000000, 0.8660254037844387076, 1.000000000000000000, 0.8660254037844387076, 1.000000000000000000, 0.8660254037844387076, 1.000000000000000000, 0.8660254037844387076, 1.000000000000000000, 0.8660254037844387076, 1.000000000000000000, 0.8660254037844387076, 1.000000000000000000, 0.8660254037844387076, 1.000000000000000000, 0.8660254037844387076, 1.000000000000000000, 0.8660254037844387076, 1.000000000000000000, 0.8660254037844387076, 1.000000000000000000, 0.8660254037844387076, 1.000000000000000000, 0.8660254037844387076, 1.000000000000000000, 0.8660254037844387076, 1.000000000000000000, 0.8660254037844387076, 1.000000000000000000, 0.8660254037844387076, 1.000000000000000000, 0.8660254037844387076, 1.000000000000000000, 0.8660254037844387076, 1.000000000000000000, 0.8660254037844387076, 1.000000000000000000, 0.8660254037844387076, 1.000000000000000000, 0.8660254037844387076, 1.000000000000000000, 0.8660254037844387076, 1.000000000000000000, 0.8660254037844387076, 1.000000000000000000) ) ) 
 REPRESENTATION_ITEM ( '' )  SURFACE ( )  );
#185177 = FACE_OUTER_BOUND ( 'NONE', #84888, .T. ) ;
#185179 = CARTESIAN_POINT ( 'NONE',  ( 0.3811277156573149583, 1.704729334087114578, -0.6539457117896373406 ) ) ;
#185180 = CARTESIAN_POINT ( 'NONE',  ( -3.327636637150278798, 5.969660945728899826, -1.199719254218452935 ) ) ;
#185181 = CARTESIAN_POINT ( 'NONE',  ( 2.390900936787855091, -0.6653014413638760338, -1.601662460290956380 ) ) ;
#185182 = CARTESIAN_POINT ( 'NONE',  ( -10.35569247086017697, 1.405922845961228962, -6.063183772476178568 ) ) ;
#185183 = EDGE_CURVE ( 'NONE', #162364, #84441, #124197, .T. ) ;
#185184 = MECHANICAL_DESIGN_GEOMETRIC_PRESENTATION_REPRESENTATION (  '', ( #64155 ), #91857 ) ;
#185185 = CARTESIAN_POINT ( 'NONE',  ( 5.197797600609998625, -0.6536857159176562293, 1.704833070275885598 ) ) ;
#185186 = CARTESIAN_POINT ( 'NONE',  ( 2.922649740298603138, -1.356309479035762378, 1.417576456850026867 ) ) ;
#185187 = CARTESIAN_POINT ( 'NONE',  ( 0.6124999999999967137, -0.5208333326505234506, -1.060881119635972647 ) ) ;
#185188 = CARTESIAN_POINT ( 'NONE',  ( -8.130085669689073313, 12.63685038127928806, 0.7998128361456481317 ) ) ;
#185189 = CARTESIAN_POINT ( 'NONE',  ( 6.531277313481192337, 8.642909503859968368, 1.599625672291281386 ) ) ;
#185190 = CARTESIAN_POINT ( 'NONE',  ( 4.442108405842562391, -1.305342523080333272, -1.670987904322115636 ) ) ;
#185191 = CARTESIAN_POINT ( 'NONE',  ( 7.517069824134078537, 7.734612647770044092, 0.000000000000000000 ) ) ;
#185192 = CARTESIAN_POINT ( 'NONE',  ( -9.134442807305063639, 11.67993591332117376, 1.599625672291281386 ) ) ;
#185193 = CARTESIAN_POINT ( 'NONE',  ( 2.887621454190898884, -1.933326653459125355, 0.7409182656877840722 ) ) ;
#185195 = CARTESIAN_POINT ( 'NONE',  ( -1.402160292154681736E-14, -0.3656249996585805295, 1.575800808251672791 ) ) ;
#185194 = CARTESIAN_POINT ( 'NONE',  ( 0.000000000000000000, 1.000000000000000888, 0.000000000000000000 ) ) ;
#185197 = ORIENTED_EDGE ( 'NONE', *, *, #175333, .F. ) ;
#185196 = CARTESIAN_POINT ( 'NONE',  ( 4.248835331960220785, 2.178490119157860061, 0.4332075398792554766 ) ) ;
#185198 = CARTESIAN_POINT ( 'NONE',  ( 3.235276958591898566, 2.298851035330526038, -0.002058992973525546142 ) ) ;
#185199 = CARTESIAN_POINT ( 'NONE',  ( 8.324343129110697959, 9.774450407793066731, -1.082531754730543083 ) ) ;
#185201 = CARTESIAN_POINT ( 'NONE',  ( -1.642778471875000035, -2.267708332855375541, -2.845375778867859751 ) ) ;
#185200 = CARTESIAN_POINT ( 'NONE',  ( 6.021229618244865023, 10.03886863134542828, -0.7216878364870458196 ) ) ;
#185202 = SURFACE_STYLE_USAGE ( .BOTH. , #132248 ) ;
#185203 = VERTEX_POINT ( 'NONE', #8209 ) ;
#185205 = FACE_OUTER_BOUND ( 'NONE', #158513, .T. ) ;
#185204 = CIRCLE ( 'NONE', #133315, 0.07999999999999951594 ) ;
#185206 = CARTESIAN_POINT ( 'NONE',  ( 2.742330423940505302, 1.058908597569432120, -1.592262909973440888 ) ) ;
#185207 = DIRECTION ( 'NONE',  ( -7.387867266669436732E-31, 1.000000000000000000, 8.546850786086424434E-32 ) ) ;
#185208 = CARTESIAN_POINT ( 'NONE',  ( 4.207791664195513093, -1.720086916870446236, 0.1276756817342617201 ) ) ;
#185209 = CARTESIAN_POINT ( 'NONE',  ( 3.995327539805045181, -0.3399590882401174463, 1.987497567597557468 ) ) ;
#185210 = CARTESIAN_POINT ( 'NONE',  ( 3.903220922379626145, -1.182460753651290775, -1.971142157236325243 ) ) ;
#185211 = CARTESIAN_POINT ( 'NONE',  ( -7.334597915313094241, 9.580116872663850813, 1.040834085586084257E-14 ) ) ;
#185212 = CARTESIAN_POINT ( 'NONE',  ( 5.936178820057578243, 1.039279821879979693, -1.831694563109196316 ) ) ;
#185213 = CARTESIAN_POINT ( 'NONE',  ( -5.261973015879593873, 8.192700047617899273, 1.082531754730549967 ) ) ;
#185214 = VERTEX_POINT ( 'NONE', #190161 ) ;
#185215 = CARTESIAN_POINT ( 'NONE',  ( 5.061649853805494814, 1.750434175623495348, -0.2595850195740417310 ) ) ;
#185217 = CARTESIAN_POINT ( 'NONE',  ( 1.306998621393583138, 2.023524796797530723, 1.076953482639223747 ) ) ;
#185216 = CARTESIAN_POINT ( 'NONE',  ( 5.688527969385528849, 8.794310509995222347, -1.199719254218452047 ) ) ;
#185218 = CARTESIAN_POINT ( 'NONE',  ( 0.2865101139537007402, 1.286042648715233216, 1.172746904078510122 ) ) ;
#185219 = CARTESIAN_POINT ( 'NONE',  ( -6.933015448541747006, 9.181880338089085214, 1.599625672291269396 ) ) ;
#185220 = CARTESIAN_POINT ( 'NONE',  ( 6.333935822332934507, 2.167035306593240840, 0.3253760364356065860 ) ) ;
#185221 = CARTESIAN_POINT ( 'NONE',  ( -3.481411583659053566, 7.283673624236017830, 0.000000000000000000 ) ) ;
#185222 = CARTESIAN_POINT ( 'NONE',  ( -1.360316468750066843, -0.09895833299191045263, -0.7853790794159082322 ) ) ;
#185223 = CARTESIAN_POINT ( 'NONE',  ( 3.940491328593588971, 7.322805182156911563, -0.8893161052136487887 ) ) ;
#185224 = CARTESIAN_POINT ( 'NONE',  ( 0.4675213905811578807, 1.889292113317426969, 1.069767032291484288 ) ) ;
#185225 = CARTESIAN_POINT ( 'NONE',  ( 0.8488426437929346147, -1.825078332268307513, -0.8578388575243289793 ) ) ;
#185226 =( BOUNDED_CURVE ( )  B_SPLINE_CURVE ( 2, ( #118405, #183336, #101013, #99963, #19759, #184392, #36012 ),
 .UNSPECIFIED., .F., .T. ) 
 B_SPLINE_CURVE_WITH_KNOTS ( ( 3, 2, 2, 3 ),
 ( 0.3214285714285716744, 0.3273809523809525501, 0.3333333333333334259, 0.3392857142857143571 ),
 .UNSPECIFIED. ) 
 CURVE ( )  GEOMETRIC_REPRESENTATION_ITEM ( )  RATIONAL_B_SPLINE_CURVE ( ( 0.9999999999999950040, 0.8660254037844437036, 1.000000000000000000, 0.8660254037844387076, 1.000000000000000000, 0.8660254037844374864, 1.000000000000001332 ) ) 
 REPRESENTATION_ITEM ( '' )  );
#185227 = CARTESIAN_POINT ( 'NONE',  ( 0.6823417656249917140, 5.592708333674749177, 1.181850606188765695 ) ) ;
#185228 = CARTESIAN_POINT ( 'NONE',  ( 4.406810040222974401, 1.488408744443140863, -1.223127719473691588 ) ) ;
#185229 = CARTESIAN_POINT ( 'NONE',  ( -1.402160292154681736E-14, 11.92187500034140157, 1.575800808251682339 ) ) ;
#185230 = CARTESIAN_POINT ( 'NONE',  ( 0.8091801829576624749, -0.5468400522714472745, -2.152931845550176249 ) ) ;
#185232 = VERTEX_POINT ( 'NONE', #41815 ) ;
#185231 = CARTESIAN_POINT ( 'NONE',  ( 0.1247927721447598948, 7.629137130509083597, -2.455404827119290978 ) ) ;
#185234 = DIRECTION ( 'NONE',  ( -1.084202172485362439E-14, -1.000000000000000000, -3.260636891504970529E-14 ) ) ;
#185233 = CARTESIAN_POINT ( 'NONE',  ( 1.177110729581195114, 2.995878374463980531, -0.7749999999999840350 ) ) ;
#185235 =( NAMED_UNIT ( * ) SI_UNIT ( $, .STERADIAN. ) SOLID_ANGLE_UNIT ( ) );
#185236 = CARTESIAN_POINT ( 'NONE',  ( 8.703444544968814256, 12.24143683818393313, -1.199719254218446718 ) ) ;
#185237 = CARTESIAN_POINT ( 'NONE',  ( 0.000000000000000000, 13.49999999999999822, -1.500000000000000222 ) ) ;
#185238 = CARTESIAN_POINT ( 'NONE',  ( -1.387358672536802340, 7.315968950354509559, 4.254625267136455058 ) ) ;
#185239 = CARTESIAN_POINT ( 'NONE',  ( 4.001278354253400948, -1.735443821832120870, 0.1328310682092836426 ) ) ;
#185241 = ADVANCED_FACE ( 'NONE', ( #45009 ), #177122, .F. ) ;
#185240 = CARTESIAN_POINT ( 'NONE',  ( 2.928120951529111338, 1.047165451586975049, 1.658829547137883775 ) ) ;
#185243 = CARTESIAN_POINT ( 'NONE',  ( -1.364683531250012516, 2.592708333674753174, 0.7879004041258379498 ) ) ;
#185242 = CARTESIAN_POINT ( 'NONE',  ( 5.508690485854129903, 5.321227076451600091, 1.040834085586084257E-14 ) ) ;
#185244 = SURFACE_SIDE_STYLE ('',( #183127 ) ) ;
#185245 = CARTESIAN_POINT ( 'NONE',  ( 10.72111444838738059, -6.105866302527761746, 9.269928574751062911E-15 ) ) ;
#185246 = CARTESIAN_POINT ( 'NONE',  ( 0.3442780524403609155, -0.9739420414685855398, 1.818282578471181132 ) ) ;
#185247 = CARTESIAN_POINT ( 'NONE',  ( -8.179646747746328828, 8.437342715325849341, -0.7998128361456291469 ) ) ;
#185248 = CARTESIAN_POINT ( 'NONE',  ( -3.863710589770277259, 6.491117540498504646, 1.082531754730560403 ) ) ;
#185249 = CARTESIAN_POINT ( 'NONE',  ( 4.997279897388729353, -0.2910847460899004258, 1.995267753224789997 ) ) ;
#185250 = CARTESIAN_POINT ( 'NONE',  ( 1.639924147338491123, -1.639646335682118927, -1.559238602228057990 ) ) ;
#185252 = ORIENTED_EDGE ( 'NONE', *, *, #7040, .F. ) ;
#185251 = CARTESIAN_POINT ( 'NONE',  ( -5.880485940025243607, 7.883652901494672349, 1.599625672291269396 ) ) ;
#185253 = CARTESIAN_POINT ( 'NONE',  ( -1.500000000000001332, 0.1812500006828157706, 0.000000000000000000 ) ) ;
#185254 = CARTESIAN_POINT ( 'NONE',  ( 1.458040028222376439, 0.7530789129696242590, 1.712431740859089668 ) ) ;
#185255 = CARTESIAN_POINT ( 'NONE',  ( 0.08792998612136559977, -0.4660014661636499578, 1.670295066556278352 ) ) ;
#185256 = CARTESIAN_POINT ( 'NONE',  ( 4.212563348414651188, 2.004022095860341413, 0.8874167208733558798 ) ) ;
#185257 = CARTESIAN_POINT ( 'NONE',  ( 5.895647473559280982, 1.742329625737188525, 1.513132890121783536 ) ) ;
#185258 = CARTESIAN_POINT ( 'NONE',  ( 1.709912189389639403, -2.045452440186873666, 0.2511061956092154324 ) ) ;
#185259 = CARTESIAN_POINT ( 'NONE',  ( 3.995986895217980894, -0.6101256969637807170, -1.843678354830182053 ) ) ;
#185260 = CARTESIAN_POINT ( 'NONE',  ( -3.375617059678305054, 5.921675088724528635, 1.082531754730560403 ) ) ;
#185261 = CARTESIAN_POINT ( 'NONE',  ( 5.870339087135666212, -1.187030499695044039, 1.445606174157453738 ) ) ;
#185262 = CARTESIAN_POINT ( 'NONE',  ( 4.344593448898664693E-13, 13.36537488277823371, -1.375075632470054154 ) ) ;
#185263 = CARTESIAN_POINT ( 'NONE',  ( 6.432970213454214381, 1.034009579150240610, 1.730599625746793935 ) ) ;
#185265 = ADVANCED_FACE ( 'NONE', ( #129527 ), #104855, .F. ) ;
#185264 = CARTESIAN_POINT ( 'NONE',  ( 5.424670859243587273, 5.501406555305196733, -0.7216878364870458196 ) ) ;
#185266 = CARTESIAN_POINT ( 'NONE',  ( -3.355169270512988773E-14, 0.9531250003414385441, 1.570758158831740081 ) ) ;
#185267 = CARTESIAN_POINT ( 'NONE',  ( 4.377577386359387646, -0.4445010797573499817, -1.966645064109616481 ) ) ;
#185268 = CARTESIAN_POINT ( 'NONE',  ( -3.240035523541616502, 6.723865844199768738, 0.7216878364870317197 ) ) ;
#185269 = CARTESIAN_POINT ( 'NONE',  ( -5.173318132066234476, 8.193232366456022930, -1.199719254218453823 ) ) ;
#185270 = CARTESIAN_POINT ( 'NONE',  ( 7.235247531187115833, 11.59287255302699648, -0.7998128361456291469 ) ) ;
#185272 = CARTESIAN_POINT ( 'NONE',  ( -6.864213375409984330, -6.776276029125434697, 6.558483974469869082 ) ) ;
#185271 = CARTESIAN_POINT ( 'NONE',  ( 1.875362892791394787, 1.747422460009705913, -0.5287960245906262458 ) ) ;
#185273 = CARTESIAN_POINT ( 'NONE',  ( -6.310394152517827315, 6.326824364217716656, 0.7998128361456281477 ) ) ;
#185274 = CARTESIAN_POINT ( 'NONE',  ( -6.154475385960665790, 6.144919136567696505, 0.000000000000000000 ) ) ;
#185275 = CARTESIAN_POINT ( 'NONE',  ( -10.28135750008142324, 4.005690466847553033, 7.422021812076344816 ) ) ;
#185276 = ORIENTED_EDGE ( 'NONE', *, *, #194138, .T. ) ;
#185277 = CARTESIAN_POINT ( 'NONE',  ( -5.546694241322218666, 8.524874810634301525, 1.082531754730550855 ) ) ;
#185278 = UNCERTAINTY_MEASURE_WITH_UNIT (LENGTH_MEASURE( 1.000000000000000082E-05 ), #107039, 'distance_accuracy_value', 'NONE');
#185279 = CARTESIAN_POINT ( 'NONE',  ( -3.239364772909965661E-16, -5.511313137147274333, -11.00000000000000178 ) ) ;
#185280 = DIRECTION ( 'NONE',  ( 0.000000000000000000, -2.168404344971008079E-15, -1.000000000000000000 ) ) ;
#185281 = CARTESIAN_POINT ( 'NONE',  ( 5.690105174167163327, 1.204846223408085670, 1.620761788888310351 ) ) ;
#185282 = CARTESIAN_POINT ( 'NONE',  ( 0.1356056236470788157, -0.09959319089659908475, 2.118264760961988458 ) ) ;
#185283 = CARTESIAN_POINT ( 'NONE',  ( -5.427006627220116286, 9.553534508390610469, -0.7998128361456362523 ) ) ;
#185284 = CARTESIAN_POINT ( 'NONE',  ( 4.843287188579786573, 6.673587691474970107, -1.599625672291256295 ) ) ;
#185285 = CARTESIAN_POINT ( 'NONE',  ( 4.821196345351608237, -0.1031141679418267343, 2.058443437638860285 ) ) ;
#185286 = CARTESIAN_POINT ( 'NONE',  ( 4.588517629802620235, -0.5350896943857390564, 1.944070981013110933 ) ) ;
#185287 = EDGE_LOOP ( 'NONE', ( #82319, #154170, #195925, #192073 ) ) ;
#185288 = ORIENTED_EDGE ( 'NONE', *, *, #16807, .T. ) ;
#185289 = CARTESIAN_POINT ( 'NONE',  ( 3.590748693434304251, 7.344754702231194976, 0.3435062996885069886 ) ) ;
#185290 = CARTESIAN_POINT ( 'NONE',  ( 2.758194185376297902, 5.305311418659259814, 1.199719254218452047 ) ) ;
#185292 = ORIENTED_EDGE ( 'NONE', *, *, #60516, .F. ) ;
#185291 = CARTESIAN_POINT ( 'NONE',  ( -5.875479466675803231, 7.948088359245467416, -1.599625672291271394 ) ) ;
#185293 = CARTESIAN_POINT ( 'NONE',  ( 4.873468316212648865, 8.167532512703042258, 0.9812947938723035612 ) ) ;
#185294 = CARTESIAN_POINT ( 'NONE',  ( 4.850935385407137979, -0.9528642855485233154, 1.776740034556321568 ) ) ;
#185295 = CARTESIAN_POINT ( 'NONE',  ( 3.609164914601064922, -1.813629950718143702, 0.3161406477080672128 ) ) ;
#185296 = CYLINDRICAL_SURFACE ( 'NONE', #46387, 3.475000000000000089 ) ;
#185297 = CARTESIAN_POINT ( 'NONE',  ( 2.631810907782325071, -2.152760894471450914, 0.8317484501371147365 ) ) ;
#185298 = CARTESIAN_POINT ( 'NONE',  ( 6.047819040147648373, 9.213483425884394507, 1.199719254218452047 ) ) ;
#185299 = CARTESIAN_POINT ( 'NONE',  ( 4.763041337456088264, -1.928505312680216743, -0.9765951867335492809 ) ) ;
#185301 = CARTESIAN_POINT ( 'NONE',  ( 9.257519960032755790, 9.694861462993381807, 0.7998128361456462443 ) ) ;
#185300 = CARTESIAN_POINT ( 'NONE',  ( 3.503138892209650024, -0.1435209762444041581, 2.011451614702438828 ) ) ;
#185302 = CARTESIAN_POINT ( 'NONE',  ( 0.4154419552040686248, -1.039972057064937783, -1.639973222157356636 ) ) ;
#185303 = CARTESIAN_POINT ( 'NONE',  ( -6.098470168048611306, 6.009303372345148553, 1.040834085586084257E-14 ) ) ;
#185304 = CARTESIAN_POINT ( 'NONE',  ( 3.954713598875368774, 1.661701185475419118, 1.588069724787332992 ) ) ;
#185305 = CARTESIAN_POINT ( 'NONE',  ( 2.630984769852976690, 0.3922140236936443869, -0.1649412225328064641 ) ) ;
#185306 = CARTESIAN_POINT ( 'NONE',  ( 1.209255964962522301, 2.820301984786699023, 0.7750000000000117906 ) ) ;
#185307 = CARTESIAN_POINT ( 'NONE',  ( 4.030043484472041193, 1.001115284758803625, -1.580040089582811280 ) ) ;
#185308 = ORIENTED_EDGE ( 'NONE', *, *, #43285, .T. ) ;
#185309 = CARTESIAN_POINT ( 'NONE',  ( 6.403199630258991526, 1.638877779571865423, 1.095505698648422177 ) ) ;
#185310 = VECTOR ( 'NONE', #56401, 1000.000000000000000 ) ;
#185312 = CARTESIAN_POINT ( 'NONE',  ( -7.611976899429754084, 7.845337568948314022, 0.7998128361456341429 ) ) ;
#185311 = CARTESIAN_POINT ( 'NONE',  ( -1.500000000000015099, -1.089583332650509773, -0.8660254037844383745 ) ) ;
#185313 = CARTESIAN_POINT ( 'NONE',  ( 1.225528936851564721, -0.05108506852482053856, 2.206457870188942572 ) ) ;
#185314 = ORIENTED_EDGE ( 'NONE', *, *, #7913, .F. ) ;
#185315 = B_SPLINE_CURVE_WITH_KNOTS ( 'NONE', 3,
 ( #209853, #141726, #127656, #144917, #90814, #189357, #40997, #156878, #107108, #173131 ),
 .UNSPECIFIED., .F., .F.,
 ( 4, 2, 2, 2, 4 ),
 ( 0.000000000000000000, 0.0002216178067634634239, 0.0004432356135269268477, 0.0006648534202903903529, 0.0008864712270538519607 ),
 .UNSPECIFIED. ) ;
#185316 = CARTESIAN_POINT ( 'NONE',  ( 1.252085211431714251, 3.300000000000025135, 0.7750000000000100142 ) ) ;
#185317 = CARTESIAN_POINT ( 'NONE',  ( 4.864678189204997949, 4.569879397027603929, 0.7998128361456341429 ) ) ;
#185318 = CARTESIAN_POINT ( 'NONE',  ( -3.653032323878261600, 6.349289246911547835, -1.199719254218452047 ) ) ;
#185319 = CARTESIAN_POINT ( 'NONE',  ( -7.978162878861394525, -5.230039540835476508, 7.573156686838125928 ) ) ;
#185320 = CARTESIAN_POINT ( 'NONE',  ( 0.4562421353364953802, 0.7503462943320489131, 1.823165437449389081 ) ) ;
#185321 = CARTESIAN_POINT ( 'NONE',  ( 6.639320299308884010, -2.064767919570985821, 1.030881497364994681 ) ) ;
#185322 = CARTESIAN_POINT ( 'NONE',  ( 0.5550359226569913096, 1.633180182981083028, -1.086726831054436682 ) ) ;
#185323 = CARTESIAN_POINT ( 'NONE',  ( 4.399324768961708543, -1.796976987717312291, 1.012281656189101264 ) ) ;
#185324 = CARTESIAN_POINT ( 'NONE',  ( 6.331294547901813452, 6.488857848747989543, 1.040834085586084257E-14 ) ) ;
#185325 = EDGE_CURVE ( 'NONE', #188755, #32206, #127073, .T. ) ;
#185326 = CARTESIAN_POINT ( 'NONE',  ( 6.313256805818848960, 7.394496357324014113, 1.199719254218452047 ) ) ;
#185327 = ORIENTED_EDGE ( 'NONE', *, *, #110606, .T. ) ;
#185328 = CARTESIAN_POINT ( 'NONE',  ( 8.744645890689993095, 9.304434415334227992, -0.7216878364870197293 ) ) ;
#185329 = CARTESIAN_POINT ( 'NONE',  ( 1.364683531249990311, 4.926041667008083991, 0.7879004041258500513 ) ) ;
#185330 = CARTESIAN_POINT ( 'NONE',  ( -10.79402553208788795, 4.457662888968881632, -5.246225075943923066 ) ) ;
#185331 = CARTESIAN_POINT ( 'NONE',  ( 4.161989969270883272, 7.799479364217271282, 0.7216878364870317197 ) ) ;
#185332 = CARTESIAN_POINT ( 'NONE',  ( 6.039545795398320926, 2.008403840061912859, -0.8252953610491889913 ) ) ;
#185334 = CARTESIAN_POINT ( 'NONE',  ( 5.601068772352080671, -0.4412860211496574814, 1.787476196608045464 ) ) ;
#185333 = CARTESIAN_POINT ( 'NONE',  ( 0.3282377607281135035, 0.4888354509981784335, -1.225000000000015410 ) ) ;
#185335 = CARTESIAN_POINT ( 'NONE',  ( -4.207966135563093957, 7.175396087857926375, 1.072179110320391260 ) ) ;
#185336 = CARTESIAN_POINT ( 'NONE',  ( -11.84668730067608422, 12.69999999999999929, -1.400000000000001688 ) ) ;
#185337 = CARTESIAN_POINT ( 'NONE',  ( -11.89829993707161471, 9.770807717488722233, 1.561606677374347552 ) ) ;
#185338 = CARTESIAN_POINT ( 'NONE',  ( -5.084594181526506773, 6.727074486938107611, 1.441884573159227578 ) ) ;
#185339 = CARTESIAN_POINT ( 'NONE',  ( -10.91339599544322780, -6.211932585243250315, -0.000000000000000000 ) ) ;
#185340 = CARTESIAN_POINT ( 'NONE',  ( 5.586791213849657822, 7.504901977030062454, -1.335864709735144817 ) ) ;
#185341 = CARTESIAN_POINT ( 'NONE',  ( -1.364683531250010295, 5.551041667008087543, -0.7879004041258300672 ) ) ;
#185342 = CARTESIAN_POINT ( 'NONE',  ( 1.348149404638066651, 0.9416913409402675184, -1.664245089135652611 ) ) ;
#185343 = CARTESIAN_POINT ( 'NONE',  ( 1.691920373447815207, -1.760920987957525385, -0.1775098275408875104 ) ) ;
#185344 = AXIS2_PLACEMENT_3D ( 'NONE', #58411, #26957, #92001 ) ;
#185345 = CARTESIAN_POINT ( 'NONE',  ( 6.094395157121155648, -1.075028013068216604, 1.701836141867618446 ) ) ;
#185347 = CARTESIAN_POINT ( 'NONE',  ( 4.745656728581866268, 1.894139079640380086, -0.2851870984255585051 ) ) ;
#185346 = CARTESIAN_POINT ( 'NONE',  ( -10.15235809853472126, 10.73883929124566983, -0.7998128361456291469 ) ) ;
#185348 = CARTESIAN_POINT ( 'NONE',  ( -1.713667314260263419, 1.036161614632730377, 1.380621972511379081 ) ) ;
#185349 = CARTESIAN_POINT ( 'NONE',  ( 5.810992205472774508, -1.553620646631387991, 1.210443464816546744 ) ) ;
#185350 = CARTESIAN_POINT ( 'NONE',  ( 0.3520121086563637314, -1.504009422257305495, -1.495223887398588358 ) ) ;
#185351 = DIRECTION ( 'NONE',  ( 0.9055141421511284650, 0.4243160830846573472, 0.000000000000000000 ) ) ;
#185352 = CARTESIAN_POINT ( 'NONE',  ( 4.381629165553334815, 1.221847395770376377, 1.416585496670008659 ) ) ;
#185354 = ORIENTED_EDGE ( 'NONE', *, *, #175553, .T. ) ;
#185353 = CARTESIAN_POINT ( 'NONE',  ( 6.147054438156498435, -1.453121625630097613, 0.9290195162147057983 ) ) ;
#185356 = CARTESIAN_POINT ( 'NONE',  ( 4.216222584169931231, 4.021273891060765493, 1.214306433183764966E-14 ) ) ;
#185355 = CARTESIAN_POINT ( 'NONE',  ( 3.123846942790895476, -2.126788776302591888, 0.5888931905130634359 ) ) ;
#185357 = CARTESIAN_POINT ( 'NONE',  ( 0.6823417656249917140, 3.655208333674754506, 1.181850606188765695 ) ) ;
#185358 = CARTESIAN_POINT ( 'NONE',  ( 0.6782753517312088976, -1.101985112813896883, -1.743456004656674718 ) ) ;
#185359 = CARTESIAN_POINT ( 'NONE',  ( 5.937581207780954884, 9.014596278131406848, -1.199719254218440723 ) ) ;
#185360 = CARTESIAN_POINT ( 'NONE',  ( -7.967387826325084355, 12.44703623068796361, 0.7998128361456481317 ) ) ;
#185361 = CARTESIAN_POINT ( 'NONE',  ( -8.596519480563392435, 15.44749384048859930, -8.311898804283693210 ) ) ;
#185362 = CARTESIAN_POINT ( 'NONE',  ( -3.093231602212184850, 6.760520635889516683, -0.7998128361456282587 ) ) ;
#185363 = AXIS2_PLACEMENT_3D ( 'NONE', #57046, #139376, #175082 ) ;
#185364 = ORIENTED_EDGE ( 'NONE', *, *, #103174, .F. ) ;
#185365 = CARTESIAN_POINT ( 'NONE',  ( 3.701679681979888503, -1.565833156357125278, -1.354537944502069102 ) ) ;
#185366 = CARTESIAN_POINT ( 'NONE',  ( -0.7500000000000215383, 4.941666666666684193, 1.299038105676671107 ) ) ;
#185367 = CARTESIAN_POINT ( 'NONE',  ( 5.066996723205273057, 6.934582148538044777, 1.599625672291267398 ) ) ;
#185368 = CARTESIAN_POINT ( 'NONE',  ( -6.169688749744446810, 7.059909438329341036, 1.079748085779270950 ) ) ;
#185369 = CARTESIAN_POINT ( 'NONE',  ( 0.6627674568651781284, 0.5885975752501994007, 1.931983969097182063 ) ) ;
#185370 = DIRECTION ( 'NONE',  ( 0.000000000000000000, 8.546850786086437571E-32, 1.000000000000000000 ) ) ;
#185371 = EDGE_CURVE ( 'NONE', #150164, #93524, #185660, .T. ) ;
#185372 = VECTOR ( 'NONE', #37425, 1000.000000000000000 ) ;
#185374 = CARTESIAN_POINT ( 'NONE',  ( 7.429504990608736037, 11.61158022244479682, -0.7216878364870267237 ) ) ;
#185373 = CARTESIAN_POINT ( 'NONE',  ( 0.1749903794560566384, 0.2522965209616668814, -1.990827758811020809 ) ) ;
#185375 = CARTESIAN_POINT ( 'NONE',  ( 6.837263156049210089, -1.242709075549037312, 1.588189626643407681 ) ) ;
#185376 = CARTESIAN_POINT ( 'NONE',  ( 5.805858164762184082, -1.070174230454253639, -1.588719782701804695 ) ) ;
#185377 = CARTESIAN_POINT ( 'NONE',  ( 6.539320575229297106, 0.5644099559201658511, 2.255290358406045303 ) ) ;
#185378 = CARTESIAN_POINT ( 'NONE',  ( 3.509492838045696672, -2.158849082856160173, 0.3763758916049686487 ) ) ;
#185379 = EDGE_CURVE ( 'NONE', #90864, #135683, #19960, .T. ) ;
#185380 = CARTESIAN_POINT ( 'NONE',  ( -0.7500000000000215383, 2.722916667349486897, 1.299038105676671107 ) ) ;
#185381 = CARTESIAN_POINT ( 'NONE',  ( 3.972844611716894736, -1.413603510852480927, 1.288168406687495215 ) ) ;
#185382 = CARTESIAN_POINT ( 'NONE',  ( -5.901876940650454095, 5.779944607047298177, -0.7998128361456291469 ) ) ;
#185383 = EDGE_CURVE ( 'NONE', #130448, #53708, #136236, .T. ) ;
#185384 = CARTESIAN_POINT ( 'NONE',  ( 5.002595493318194642, 4.938708951733754127, -0.7216878364870197293 ) ) ;
#185386 = CARTESIAN_POINT ( 'NONE',  ( 0.6324356828835416833, 0.5880426346329314935, 1.928746166857209676 ) ) ;
#185385 = CARTESIAN_POINT ( 'NONE',  ( -4.911752498546917423, 4.707425932596563278, -0.3822207396134598145 ) ) ;
#185387 = CARTESIAN_POINT ( 'NONE',  ( 1.364683531250000303, 11.56770833367472839, -0.7879004041258355073 ) ) ;
#185389 = CARTESIAN_POINT ( 'NONE',  ( -6.303615075710993665, 6.318915441276411471, -0.7998128361456362523 ) ) ;
#185388 = CARTESIAN_POINT ( 'NONE',  ( 5.583573808894983337, -0.9862700065477579825, 1.957137920222583372 ) ) ;
#185391 = EDGE_LOOP ( 'NONE', ( #214031, #119106, #157883, #79013 ) ) ;
#185390 = CARTESIAN_POINT ( 'NONE',  ( 2.959633327367673150, 1.716642837065301519, -0.1670560860976433859 ) ) ;
#185392 = LINE ( 'NONE', #168094, #140241 ) ;
#185393 = CARTESIAN_POINT ( 'NONE',  ( 5.784525094524856748, 9.900363043587685041, 1.040834085586084257E-14 ) ) ;
#185394 = CARTESIAN_POINT ( 'NONE',  ( 4.137209430464448445, 7.978494768850520558, 1.040834085586084257E-14 ) ) ;
#185395 = CARTESIAN_POINT ( 'NONE',  ( -1.734723475976807094E-15, -8.407420853759283830, -10.91970695577494332 ) ) ;
#185396 = CARTESIAN_POINT ( 'NONE',  ( 1.117545225965112188, 0.3861695934333775337, -1.923310697798483293 ) ) ;
#185397 = SPHERICAL_SURFACE ( 'NONE', #126386, 0.5000000000000001110 ) ;
#185398 = CARTESIAN_POINT ( 'NONE',  ( 3.842846474469570062, 6.570739089268092137, -1.199719254218452047 ) ) ;
#185399 = CARTESIAN_POINT ( 'NONE',  ( 0.1751657365761547513, 0.002452341591364578209, -2.044164811867712483 ) ) ;
#185400 = ORIENTED_EDGE ( 'NONE', *, *, #38945, .F. ) ;
#185401 = VERTEX_POINT ( 'NONE', #204024 ) ;
#185402 = CARTESIAN_POINT ( 'NONE',  ( 4.283730857329768327, 1.755957581118623434, -0.4444456398857503099 ) ) ;
#185403 = ORIENTED_EDGE ( 'NONE', *, *, #138676, .T. ) ;
#185404 = CARTESIAN_POINT ( 'NONE',  ( 10.06423010004587759, 10.63602329300870153, 0.000000000000000000 ) ) ;
#185405 = CARTESIAN_POINT ( 'NONE',  ( 4.543917759235442944, 5.330267469643351852, 1.199719254218452935 ) ) ;
#185406 = CARTESIAN_POINT ( 'NONE',  ( 4.740750167454264918, 1.734909645891765662, 0.5210944610908369024 ) ) ;
#185407 = CARTESIAN_POINT ( 'NONE',  ( 6.007671464186812749, 10.02305078494439883, 0.7216878364870317197 ) ) ;
#185408 = DIRECTION ( 'NONE',  ( 5.578564026256490882E-16, 1.000000000000000000, 9.066213480720158442E-32 ) ) ;
#185409 = CARTESIAN_POINT ( 'NONE',  ( 5.512200117181983217, 6.216449928263548586, -0.9568283335872149742 ) ) ;
#185411 = CARTESIAN_POINT ( 'NONE',  ( 1.364683531249997417, 15.23437500034140157, 2.602085213965210642E-15 ) ) ;
#185410 = CARTESIAN_POINT ( 'NONE',  ( 5.125394178454842020, 0.1826033194989445385, -1.852086804783218188 ) ) ;
#185412 = CARTESIAN_POINT ( 'NONE',  ( 2.688967962845473458, 1.619712848077807577, 1.022445119732362961 ) ) ;
#185413 = CARTESIAN_POINT ( 'NONE',  ( -10.91944002402979130, -8.407420853759269619, 0.1105873483556677611 ) ) ;
#185414 = CARTESIAN_POINT ( 'NONE',  ( -10.44369633504468631, 5.112959841837462882, -5.232137017608344820 ) ) ;
#185415 = EDGE_CURVE ( 'NONE', #64278, #100328, #149110, .T. ) ;
#185416 = CARTESIAN_POINT ( 'NONE',  ( -1.201851678989727383E-14, 5.618750000682818602, -1.732050807568863648 ) ) ;
#185417 = CARTESIAN_POINT ( 'NONE',  ( 5.844973620822844218, 6.952128991449046502, 1.082531754730549967 ) ) ;
#185418 = CARTESIAN_POINT ( 'NONE',  ( 5.287316719649520991, 8.151991358691011769, -1.082531754730549078 ) ) ;
#185419 = CARTESIAN_POINT ( 'NONE',  ( -9.490344339885973923, 12.09515436799890331, -1.443375672974059665 ) ) ;
#185420 = CARTESIAN_POINT ( 'NONE',  ( 11.88235317400313917, 12.34335760226970358, -0.9089793033029952563 ) ) ;
#185421 = CARTESIAN_POINT ( 'NONE',  ( -7.110325215724114578, 7.260077271291732082, 0.000000000000000000 ) ) ;
#185422 = CARTESIAN_POINT ( 'NONE',  ( 0.9024203131168639924, 1.581833000263275224, -1.367050110207337799 ) ) ;
#185423 = CARTESIAN_POINT ( 'NONE',  ( 4.505052181490820651, 8.477920988373101707, -0.7998128361456381397 ) ) ;
#185424 = CARTESIAN_POINT ( 'NONE',  ( 0.5690311950540331010, 0.1842100624489529104, -1.816270042949569730 ) ) ;
#185425 = CARTESIAN_POINT ( 'NONE',  ( -4.066556009095094737, 6.831733546331167695, 1.199719254218464037 ) ) ;
#185426 = CARTESIAN_POINT ( 'NONE',  ( 2.590611583786633254, -0.3098195481324728107, -1.798931244660670448 ) ) ;
#185427 = DIRECTION ( 'NONE',  ( 0.000000000000000000, 1.000000000000000000, 0.000000000000000000 ) ) ;
#185428 =( BOUNDED_CURVE ( )  B_SPLINE_CURVE ( 2, ( #188458, #40089, #59521, #106200, #57397, #123561, #42236 ),
 .UNSPECIFIED., .F., .T. ) 
 B_SPLINE_CURVE_WITH_KNOTS ( ( 3, 2, 2, 3 ),
 ( 0.3035714285714285476, 0.3095238095238095899, 0.3154761904761906322, 0.3214285714285716744 ),
 .UNSPECIFIED. ) 
 CURVE ( )  GEOMETRIC_REPRESENTATION_ITEM ( )  RATIONAL_B_SPLINE_CURVE ( ( 1.000000000000000000, 0.8660254037844387076, 1.000000000000000000, 0.8660254037844387076, 1.000000000000000000, 0.8660254037844337116, 1.000000000000005107 ) ) 
 REPRESENTATION_ITEM ( '' )  );
#185429 = CARTESIAN_POINT ( 'NONE',  ( 1.732793293511214472, -1.869146454778564559, -0.6209850235064825474 ) ) ;
#185430 = CARTESIAN_POINT ( 'NONE',  ( 3.772937862106290563, 1.827633595424851043, -0.6570963203050876889 ) ) ;
#185431 = CIRCLE ( 'NONE', #213085, 0.07999999999999977962 ) ;
#185432 = CARTESIAN_POINT ( 'NONE',  ( -5.164730172163054966, 4.990216387137135889, -0.7998128361456362523 ) ) ;
#185434 = CARTESIAN_POINT ( 'NONE',  ( 4.553055379497691568, 0.3652949536288411791, 2.088752307168060707 ) ) ;
#185433 = CARTESIAN_POINT ( 'NONE',  ( 6.535912570239620578, 9.782925877658371405, 1.199719254218452047 ) ) ;
#185435 = SPHERICAL_SURFACE ( 'NONE', #63518, 0.08000000000000000167 ) ;
#185436 = CARTESIAN_POINT ( 'NONE',  ( 7.425061681778431399, 11.81432239538354345, 0.7998128361456462443 ) ) ;
#185437 = CARTESIAN_POINT ( 'NONE',  ( 6.039686174407700392, 6.062845369715991417, 0.4964408002013191989 ) ) ;
#185438 = CARTESIAN_POINT ( 'NONE',  ( -2.926243505372967280E-18, -4.140708350189166609, -0.9999999999999991118 ) ) ;
#185439 = ORIENTED_EDGE ( 'NONE', *, *, #28829, .T. ) ;
#185440 = CARTESIAN_POINT ( 'NONE',  ( 6.688968683495743583, 8.897159112202094988, -1.599625672291283607 ) ) ;
#185441 = DIRECTION ( 'NONE',  ( 1.000000000000000000, -0.000000000000000000, -0.000000000000000000 ) ) ;
#185442 = CARTESIAN_POINT ( 'NONE',  ( 3.510199737632841543, -0.7410081052188906003, -1.668730646197075673 ) ) ;
#185443 = CARTESIAN_POINT ( 'NONE',  ( 10.99956415888072492, -9.918872522958837479, -0.09791994008662846527 ) ) ;
#185444 = CARTESIAN_POINT ( 'NONE',  ( -7.524412065904404479, 11.72230514362308185, 0.000000000000000000 ) ) ;
#185445 = CARTESIAN_POINT ( 'NONE',  ( -5.094039349513959536, 7.939876775568885492, 1.214520887661042936 ) ) ;
#185446 = B_SPLINE_CURVE_WITH_KNOTS ( 'NONE', 3,
 ( #180947, #32569, #164703, #16291, #82376, #35 ),
 .UNSPECIFIED., .F., .F.,
 ( 4, 2, 4 ),
 ( 0.0004065497138311778428, 0.0007003026727366230050, 0.0009940556316420680587 ),
 .UNSPECIFIED. ) ;
#185447 = LINE ( 'NONE', #154036, #139902 ) ;
#185448 = CARTESIAN_POINT ( 'NONE',  ( 4.856247981345184428, 0.7163626499266174674, 1.728251504774950709 ) ) ;
#185449 = CARTESIAN_POINT ( 'NONE',  ( 6.591235234537977661, 10.84152487360300299, 0.7998128361456462443 ) ) ;
#185450 = CARTESIAN_POINT ( 'NONE',  ( 1.787598692544673851, 1.328180555690385845, 1.395690353023341101 ) ) ;
#185451 = CARTESIAN_POINT ( 'NONE',  ( 1.252085211431710698, 2.800000000000024691, 0.7750000000000152323 ) ) ;
#185452 = CARTESIAN_POINT ( 'NONE',  ( 5.054492339796319733, 4.791329239384148231, -0.7998128361456211532 ) ) ;
#185453 = CARTESIAN_POINT ( 'NONE',  ( 0.6823417656249969321, 9.088541667008065872, -1.181850606188757036 ) ) ;
#185454 = CARTESIAN_POINT ( 'NONE',  ( -4.740547266272593596, 8.682388910626682943, -0.7998128361456281477 ) ) ;
#185455 = CARTESIAN_POINT ( 'NONE',  ( 3.985207087413062066, 6.736826471035503694, -1.199719254218452047 ) ) ;
#185456 = CARTESIAN_POINT ( 'NONE',  ( -4.407809337774280856, 7.196175756495025055, 1.082531754730549967 ) ) ;
#185457 = CIRCLE ( 'NONE', #178678, 1.250000000000000000 ) ;
#185458 = CARTESIAN_POINT ( 'NONE',  ( 0.9841680404778062607, -2.117403155482136423, 0.004310642112759220310 ) ) ;
#185459 = CIRCLE ( 'NONE', #99062, 10.97656854249491509 ) ;
#185460 = CARTESIAN_POINT ( 'NONE',  ( -0.3282377607281410370, 0.6138354509981421847, 1.224999999999986766 ) ) ;
#185461 = DIRECTION ( 'NONE',  ( 0.000000000000000000, -1.000000000000000000, 0.000000000000000000 ) ) ;
#185462 = CARTESIAN_POINT ( 'NONE',  ( 6.385608392048681026, -1.951384585020640383, 0.6918703269920488674 ) ) ;
#185464 = CARTESIAN_POINT ( 'NONE',  ( 4.383065840713377348, 7.132475524829186675, -1.069666325224464032 ) ) ;
#185463 = CARTESIAN_POINT ( 'NONE',  ( 0.6437974683802077935, 0.5340323341261629109, 1.762076181610471526 ) ) ;
#185465 = CARTESIAN_POINT ( 'NONE',  ( 6.434253291069976122, -1.843495385113643525, -1.373021106398547131 ) ) ;
#185466 = CARTESIAN_POINT ( 'NONE',  ( 5.178851490740193242, 8.025448591630130579, 1.082531754730558626 ) ) ;
#185467 = CARTESIAN_POINT ( 'NONE',  ( 5.560252395380222090, 5.659585014131299552, 0.7216878364870328300 ) ) ;
#185468 = CARTESIAN_POINT ( 'NONE',  ( 1.219134843238580235, -0.05193690637114551506, 2.291835786607650416 ) ) ;
#185469 = CARTESIAN_POINT ( 'NONE',  ( -1.040834085586084257E-14, -9.911192057434348612, -9.579665964948867796 ) ) ;
#185470 = CARTESIAN_POINT ( 'NONE',  ( -4.911796789900812144, 8.952456364851418158, 0.7998128361456291469 ) ) ;
#185471 = CARTESIAN_POINT ( 'NONE',  ( 6.492136518976993287, -0.5202676277693082385, -1.870896455867506747 ) ) ;
#185472 = ORIENTED_EDGE ( 'NONE', *, *, #10274, .T. ) ;
#185473 = CARTESIAN_POINT ( 'NONE',  ( 8.581948047326003248, 9.114620264742901767, -0.7216878364870197293 ) ) ;
#185474 = CARTESIAN_POINT ( 'NONE',  ( 6.504189997394580480, -0.8109953713257547214, 1.730197269205424160 ) ) ;
#185475 = CARTESIAN_POINT ( 'NONE',  ( 6.333220217719927270, -1.622483202430196725, -1.197309987464048486 ) ) ;
#185476 = CARTESIAN_POINT ( 'NONE',  ( -7.934546212495630968, 10.28005655271014795, -1.599625672291263179 ) ) ;
#185477 = CARTESIAN_POINT ( 'NONE',  ( -1.499999999999960476, 7.000000000000000000, 10.99818166789401985 ) ) ;
#185479 = CARTESIAN_POINT ( 'NONE',  ( 1.639140867700689785, -1.278921918198316465, -1.223650632631252622 ) ) ;
#185478 = CARTESIAN_POINT ( 'NONE',  ( 2.941443032221033427, 0.7519493320215028254, -1.950910760374990671 ) ) ;
#185480 = CARTESIAN_POINT ( 'NONE',  ( -0.1062647551456016304, -6.683951888245086792, -9.488025208486867257 ) ) ;
#185482 = CARTESIAN_POINT ( 'NONE',  ( 4.558679923290005043, -2.046282147472633373, -1.033175111039591698 ) ) ;
#185481 = CARTESIAN_POINT ( 'NONE',  ( 3.250922972226694352, 7.014770244231638863, 0.7998128361456281477 ) ) ;
#185483 = CARTESIAN_POINT ( 'NONE',  ( 3.310250384734690243, 1.573932026098995518, 0.7429073729697617257 ) ) ;
#185484 = CARTESIAN_POINT ( 'NONE',  ( 4.403700966340357681, 4.032072637018845107, -0.7998128361456211532 ) ) ;
#185485 = CARTESIAN_POINT ( 'NONE',  ( 5.224688093219824303, 7.188831756880171397, -1.599625672291283607 ) ) ;
#185486 = CARTESIAN_POINT ( 'NONE',  ( 3.866272716362227690, -0.5049011280162157833, 1.658656615756588959 ) ) ;
#185487 = CARTESIAN_POINT ( 'NONE',  ( 3.719319017856066445, -1.913190415241170728, -1.026542932298198485 ) ) ;
#185488 = CARTESIAN_POINT ( 'NONE',  ( 4.904298879841284098, 6.744767997946721216, 1.599625672291267398 ) ) ;
#185489 = CARTESIAN_POINT ( 'NONE',  ( 4.329314735043091389, -1.561880650076686861, -1.275557594027726394 ) ) ;
#185491 = CIRCLE ( 'NONE', #109515, 0.08000000000000004330 ) ;
#185490 = CARTESIAN_POINT ( 'NONE',  ( 3.468750000000001776, 0.7852924748298147906, -1.895863743164155180 ) ) ;
#185492 = CARTESIAN_POINT ( 'NONE',  ( 1.499999999999989120, 2.306250000682817713, 1.214306433183764966E-14 ) ) ;
#185493 = CARTESIAN_POINT ( 'NONE',  ( 2.397378046164869936, 1.487928659643242169, 1.223526803071661950 ) ) ;
#185494 = CARTESIAN_POINT ( 'NONE',  ( -6.009258394948636914E-15, 8.468750000682796042, -1.732050807568875195 ) ) ;
#185495 = CARTESIAN_POINT ( 'NONE',  ( 4.570683916498400556, 0.8515115505445168820, 2.051917206062872978 ) ) ;
#185496 = ORIENTED_EDGE ( 'NONE', *, *, #79256, .T. ) ;
#185497 = CARTESIAN_POINT ( 'NONE',  ( -15.75000000000000000, 12.29999999999998295, 3.199999999999997957 ) ) ;
#185498 = CARTESIAN_POINT ( 'NONE',  ( 0.7499999999999885647, 1.566666666666688412, -1.299038105676652899 ) ) ;
#185499 = CARTESIAN_POINT ( 'NONE',  ( 7.233438648090761980, 8.397765496649418182, 1.199719254218462483 ) ) ;
#185500 = CARTESIAN_POINT ( 'NONE',  ( 3.511198595814921219, 7.040222761851976152, 0.7216878364870317197 ) ) ;
#185501 = CARTESIAN_POINT ( 'NONE',  ( -3.285556943750000514, -2.238541666188709200, -1.896917185911906722 ) ) ;
#185502 = CARTESIAN_POINT ( 'NONE',  ( 0.3643397115577310941, 0.6907578271265965020, -2.111251545739430302 ) ) ;
#185505 = EDGE_CURVE ( 'NONE', #120494, #189233, #48399, .T. ) ;
#185504 = CARTESIAN_POINT ( 'NONE',  ( 5.635196431686764207, -0.04651148872366302894, -1.961470878453225763 ) ) ;
#185503 = COLOUR_RGB ( '', 0.40784314, 0.44705882, 0.49803922) ;
#185506 = CARTESIAN_POINT ( 'NONE',  ( 7.293923454472077239, 10.49303254931736262, 1.082531754730558626 ) ) ;
#185507 = CARTESIAN_POINT ( 'NONE',  ( 0.2808502495336914206, -2.096634173354972486, -0.5254431554712820640 ) ) ;
#185508 = CARTESIAN_POINT ( 'NONE',  ( 5.578253857379852576, 5.472660686556754861, -0.7998128361456481317 ) ) ;
#185509 = CARTESIAN_POINT ( 'NONE',  ( -5.533136088152923904, 6.588318536667425285, 1.082531754730549078 ) ) ;
#185510 = CARTESIAN_POINT ( 'NONE',  ( 3.156738326643961923, -0.5960753502360670586, -1.974691822637637761 ) ) ;
#185511 = CARTESIAN_POINT ( 'NONE',  ( -5.579343907223557331, 6.467988298970945849, 1.199719254218450271 ) ) ;
#185512 = CARTESIAN_POINT ( 'NONE',  ( 1.499999999999989120, 4.327083334016148086, -0.8660254037844323793 ) ) ;
#185513 = CARTESIAN_POINT ( 'NONE',  ( -1.364683531249997417, 5.071875000341417916, 1.214306433183764966E-14 ) ) ;
#185514 = CARTESIAN_POINT ( 'NONE',  ( 5.202362286721474050, -0.6290170809866748591, -1.761763226176292996 ) ) ;
#185515 = CARTESIAN_POINT ( 'NONE',  ( 5.256420022722958052, 1.669015333217665820, -0.4704954288548191532 ) ) ;
#185516 = CARTESIAN_POINT ( 'NONE',  ( 3.052039328023182119, -1.315916573227500219, 1.139148930295554862 ) ) ;
#185517 = CARTESIAN_POINT ( 'NONE',  ( 0.4688447829373428855, -2.161134926827886549, -0.7649225765839831048 ) ) ;
#185518 = CARTESIAN_POINT ( 'NONE',  ( -1.364683531250010295, 4.592708333674755394, 0.7879004041258379498 ) ) ;
#185519 = CARTESIAN_POINT ( 'NONE',  ( 5.759345132242938092, 2.059656548118168562, -0.3582877099650525476 ) ) ;
#185520 = CARTESIAN_POINT ( 'NONE',  ( 6.439402819763696328, 0.7408549094962694204, -1.795268486070795477 ) ) ;
#185521 = AXIS2_PLACEMENT_3D ( 'NONE', #136455, #74638, #56258 ) ;
#185522 = PLANE ( 'NONE',  #49736 ) ;
#185523 = CARTESIAN_POINT ( 'NONE',  ( 1.336564801266389990, 0.5826540126645517459, -1.930418273149013153 ) ) ;
#185524 = CARTESIAN_POINT ( 'NONE',  ( 0.1467655724766807612, -1.757430454515636509, 1.308964887167404889 ) ) ;
#185525 = CARTESIAN_POINT ( 'NONE',  ( 9.673880494682652653, 13.47554395514287684, -8.174421919205036247 ) ) ;
#185526 = CARTESIAN_POINT ( 'NONE',  ( -8.864333505236459132, 9.236143932397675727, 1.040834085586084257E-14 ) ) ;
#185527 = CARTESIAN_POINT ( 'NONE',  ( 6.817052309572890323, 6.847649204123507083, 0.7998128361456341429 ) ) ;
#185528 = CARTESIAN_POINT ( 'NONE',  ( 2.455864667332839257, -1.573010975769023601, -1.422207447652395373 ) ) ;
#185529 = FACE_OUTER_BOUND ( 'NONE', #113160, .T. ) ;
#185530 = CARTESIAN_POINT ( 'NONE',  ( 4.986841741376339066, -0.2268417095559888130, -1.811474396668552700 ) ) ;
#185531 = ORIENTED_EDGE ( 'NONE', *, *, #182167, .F. ) ;
#185532 = CARTESIAN_POINT ( 'NONE',  ( -7.130662446144611977, 7.283804040115648526, 0.000000000000000000 ) ) ;
#185533 = CARTESIAN_POINT ( 'NONE',  ( 1.734723475976807094E-15, 15.00041888085534758, 12.17999951260719982 ) ) ;
#185534 = CARTESIAN_POINT ( 'NONE',  ( 7.146556367734771875, 8.470642196179646533, 1.082531754730549967 ) ) ;
#185535 = CARTESIAN_POINT ( 'NONE',  ( -1.642778471875000035, -1.305208332855377407, -2.845375778867859751 ) ) ;
#185536 = CARTESIAN_POINT ( 'NONE',  ( -6.184490626128011925, 10.36698949712469364, -0.7998128361456291469 ) ) ;
#185537 = CARTESIAN_POINT ( 'NONE',  ( 2.478776341996299593, -1.389826682745049835, 1.465835156725032506 ) ) ;
#185538 = CARTESIAN_POINT ( 'NONE',  ( 0.3761801408644695477, 1.212865950663596371, 1.721436218156185305 ) ) ;
#185539 = CARTESIAN_POINT ( 'NONE',  ( 9.999301985278609806, 11.62460605670194447, 1.199719254218452047 ) ) ;
#185540 = CARTESIAN_POINT ( 'NONE',  ( 4.065176880270331417, 1.594224420893322725, 0.9597675150698461444 ) ) ;
#185541 = CARTESIAN_POINT ( 'NONE',  ( 9.134442807305049428, 11.67993591332117376, 1.599625672291281386 ) ) ;
#185542 = CARTESIAN_POINT ( 'NONE',  ( -5.000000000000024869, 3.300000000000025135, 0.7750000000000238920 ) ) ;
#185543 = ORIENTED_EDGE ( 'NONE', *, *, #83130, .F. ) ;
#185544 = ORIENTED_EDGE ( 'NONE', *, *, #46958, .T. ) ;
#185545 = CARTESIAN_POINT ( 'NONE',  ( -4.603156847039612920, 5.329103395422994716, 1.199719254218462483 ) ) ;
#185546 = CARTESIAN_POINT ( 'NONE',  ( -8.694856585065634746, 9.038420858865048757, 0.7998128361456462443 ) ) ;
#185547 = CARTESIAN_POINT ( 'NONE',  ( 5.303274670167754223, 1.494737065598227943, 1.048009559513597866 ) ) ;
#185549 = CARTESIAN_POINT ( 'NONE',  ( -4.038790540952651220, 7.763523381248250033, -0.5490930765432913141 ) ) ;
#185548 = CARTESIAN_POINT ( 'NONE',  ( -7.422162748838431412, 7.623887726591770608, -0.7998128361456362523 ) ) ;
#185550 = CARTESIAN_POINT ( 'NONE',  ( -1.364683531250014514, -0.9697916663252473812, 0.7879004041258379498 ) ) ;
#185551 = CARTESIAN_POINT ( 'NONE',  ( 1.545803854144804479, 1.604466568860075437, -0.6577250193331334316 ) ) ;
#185552 = CARTESIAN_POINT ( 'NONE',  ( 0.5502397958263847144, -1.467719461762364341, -0.9348402994967041080 ) ) ;
#185554 = CARTESIAN_POINT ( 'NONE',  ( 8.771762198361678031, 9.336070107617867819, 1.040834085586084257E-14 ) ) ;
#185553 = CARTESIAN_POINT ( 'NONE',  ( 5.092513741553108986, -2.289745732339975692, -0.2867506301261530388 ) ) ;
#185555 = CARTESIAN_POINT ( 'NONE',  ( -10.47476534206535170, 5.237283261923990629, -5.169982392003922733 ) ) ;
#185556 = CARTESIAN_POINT ( 'NONE',  ( 1.739600335799436737, -1.490509515545968666, -1.423327880080206720 ) ) ;
#185557 = CARTESIAN_POINT ( 'NONE',  ( 6.654354466208897811, 6.657835053532175529, 0.7998128361456341429 ) ) ;
#185558 = CARTESIAN_POINT ( 'NONE',  ( 6.485746271079104730, 2.140961846981633609, 0.8364165754714718570 ) ) ;
#185559 = CARTESIAN_POINT ( 'NONE',  ( 8.338567886252109318, 15.10332194136754680, -8.569227703174822963 ) ) ;
#185560 = CARTESIAN_POINT ( 'NONE',  ( -5.413448473606448985, 9.537716662508005427, 0.000000000000000000 ) ) ;
#185561 = CARTESIAN_POINT ( 'NONE',  ( 6.666881909320486521, -1.711340306973156977, -0.7558587634414122292 ) ) ;
#185563 = CARTESIAN_POINT ( 'NONE',  ( -5.144392941742557568, 4.966489618313220333, -0.7998128361456362523 ) ) ;
#185562 = CARTESIAN_POINT ( 'NONE',  ( 3.955252344019274169, -1.661368509396843995, 0.9470704235666274062 ) ) ;
#185564 = CARTESIAN_POINT ( 'NONE',  ( 5.180388087185870738, -1.228261608319089149, 1.833297759731546073 ) ) ;
#185565 = CARTESIAN_POINT ( 'NONE',  ( 0.6124999999999932720, 2.229166667349451014, -1.060881119635948444 ) ) ;
#185566 = CARTESIAN_POINT ( 'NONE',  ( -6.238160075619175515, 10.29195416494877513, 0.000000000000000000 ) ) ;
#185567 = CARTESIAN_POINT ( 'NONE',  ( 3.214691819771663628, 6.764574533126651801, -0.7216878364870338292 ) ) ;
#185568 = CARTESIAN_POINT ( 'NONE',  ( -3.594320120954326292, 6.247105003538398371, 1.082531754730549967 ) ) ;
#185569 = CARTESIAN_POINT ( 'NONE',  ( 6.287751673603878544, 2.029294879081492198, -0.6150919484220889188 ) ) ;
#185570 = ORIENTED_EDGE ( 'NONE', *, *, #99318, .T. ) ;
#185571 = CARTESIAN_POINT ( 'NONE',  ( 4.014917937017292715, 1.634369553669342778, -1.629294119824703069 ) ) ;
#185572 = CARTESIAN_POINT ( 'NONE',  ( 3.842202535371820993, -0.9690557767615382012, 1.705768119890891610 ) ) ;
#185573 = CARTESIAN_POINT ( 'NONE',  ( -4.664887371553763096, 7.600063145858131364, -1.199719254218453823 ) ) ;
#185574 = CARTESIAN_POINT ( 'NONE',  ( 0.8132426064601482318, -1.654215606812576400, -1.054277637385622857 ) ) ;
#185575 = FACE_OUTER_BOUND ( 'NONE', #140945, .T. ) ;
#185576 = CARTESIAN_POINT ( 'NONE',  ( 6.594971851908695726, -6.631671897293982987, 6.818239719371404384 ) ) ;
#185577 = ORIENTED_EDGE ( 'NONE', *, *, #193910, .T. ) ;
#185578 = CARTESIAN_POINT ( 'NONE',  ( 5.805875103277515770, -1.124240986939632592, -1.673857227857282082 ) ) ;
#185579 = CARTESIAN_POINT ( 'NONE',  ( -8.158255747121117452, 10.54105100977322174, 1.599625672291295375 ) ) ;
#185580 = CARTESIAN_POINT ( 'NONE',  ( 10.50000000000000178, 13.39999999999998259, 3.599999999999999201 ) ) ;
#185582 = COLOUR_RGB ( '', 0.08235294, 0.09019608, 0.10196078) ;
#185581 = CARTESIAN_POINT ( 'NONE',  ( 2.659224658930594121, 1.746150167319389990, -1.290005652201154263 ) ) ;
#185583 = DIRECTION ( 'NONE',  ( -0.000000000000000000, 1.000000000000000000, -0.000000000000000000 ) ) ;
#185584 = CARTESIAN_POINT ( 'NONE',  ( 0.4574861729177078229, -1.815669959853306370, 1.095388807130371900 ) ) ;
#185585 = CARTESIAN_POINT ( 'NONE',  ( 0.7499999999999902300, 2.014583334016148530, 1.299038105676669330 ) ) ;
#185586 = CARTESIAN_POINT ( 'NONE',  ( 9.511208455186636712, 11.05516360492796935, 1.199719254218453823 ) ) ;
#185587 = CARTESIAN_POINT ( 'NONE',  ( -4.908660468810629673, 4.653493786480884964, -0.07887673679583749597 ) ) ;
#185588 = CARTESIAN_POINT ( 'NONE',  ( 5.126881573038487794, 7.911131357477594328, 1.221340741751137493 ) ) ;
#185589 = ORIENTED_EDGE ( 'NONE', *, *, #166279, .T. ) ;
#185590 = CARTESIAN_POINT ( 'NONE',  ( 1.598976361298432014, 1.686402000465867301, -1.184152512226148923 ) ) ;
#185592 = CARTESIAN_POINT ( 'NONE',  ( 0.000000000000000000, 0.5000000000000004441, 0.000000000000000000 ) ) ;
#185591 = CARTESIAN_POINT ( 'NONE',  ( -10.15235809853472126, 10.73883929124566983, -0.7998128361456291469 ) ) ;
#185593 = CARTESIAN_POINT ( 'NONE',  ( -1.364683531250012516, 1.530208333674756505, 0.7879004041258379498 ) ) ;
#185594 = CARTESIAN_POINT ( 'NONE',  ( -0.07933194154489606187, -9.609467486116969326, -9.499668754385620417 ) ) ;
#185595 = ORIENTED_EDGE ( 'NONE', *, *, #157678, .F. ) ;
#185596 = CARTESIAN_POINT ( 'NONE',  ( 4.600206319907148789, -0.8982956317880007591, 1.688143452400918454 ) ) ;
#185597 = CARTESIAN_POINT ( 'NONE',  ( 11.89317557362582711, 12.33724156162407937, -1.599935658896034729 ) ) ;
#185598 = CARTESIAN_POINT ( 'NONE',  ( 5.742760583840166966, 8.857581893525663830, 1.199719254218452047 ) ) ;
#185599 = CARTESIAN_POINT ( 'NONE',  ( -3.684065054611367351, 5.321161868511784299, -1.599625672291256295 ) ) ;
#185600 = CARTESIAN_POINT ( 'NONE',  ( 0.4393641590584134171, -1.719983824569010444, 0.5688467837753272693 ) ) ;
#185602 = CARTESIAN_POINT ( 'NONE',  ( 0.4443725376216747236, -1.385435448976629180, 1.323305594895395343 ) ) ;
#185601 = FACE_OUTER_BOUND ( 'NONE', #91306, .T. ) ;
#185603 = CARTESIAN_POINT ( 'NONE',  ( 2.365759603224312446, -0.4558734232973959966, 2.019384234097781228 ) ) ;
#185604 = CARTESIAN_POINT ( 'NONE',  ( -0.6823417656250246877, -0.3864583329919110688, 1.181850606188755259 ) ) ;
#185605 = CARTESIAN_POINT ( 'NONE',  ( 0.2331951027847931901, -1.803461566636242797, 0.7967608462288151561 ) ) ;
#185606 = CARTESIAN_POINT ( 'NONE',  ( 3.035583632137848653, -1.226507576337819483, -1.352503160878690380 ) ) ;
#185608 = CARTESIAN_POINT ( 'NONE',  ( 5.732961426666957294, 7.278201736375829789, 1.206439608388230500 ) ) ;
#185607 = CARTESIAN_POINT ( 'NONE',  ( 6.322910218073367616, 2.057572540570989261, 0.7984293639632376038 ) ) ;
#185609 = CARTESIAN_POINT ( 'NONE',  ( -1.201851678989727383E-14, 1.821875000341421691, 1.575800808251672791 ) ) ;
#185610 = AXIS2_PLACEMENT_3D ( 'NONE', #190579, #157048, #105102 ) ;
#185611 = CARTESIAN_POINT ( 'NONE',  ( 4.264169596968480747, -2.057349986699669397, 0.1488187104187361498 ) ) ;
#185612 = CARTESIAN_POINT ( 'NONE',  ( -6.738566041191992539, 7.820414121934134322, 1.199719254218450271 ) ) ;
#185613 = CARTESIAN_POINT ( 'NONE',  ( 7.751511138711133064, 10.06651563329490529, -1.599625672291262513 ) ) ;
#185614 = CARTESIAN_POINT ( 'NONE',  ( 4.656335691289526402, 7.519809842224722374, -1.199719254218452047 ) ) ;
#185616 = CARTESIAN_POINT ( 'NONE',  ( -0.7499999999999972244, 4.108333333333360038, -1.299038105676652011 ) ) ;
#185615 = CARTESIAN_POINT ( 'NONE',  ( 5.456126526903398499, 2.103703387787753343, -0.1000602029373430374 ) ) ;
#185617 = CIRCLE ( 'NONE', #137247, 0.8300000000000008482 ) ;
#185618 = CARTESIAN_POINT ( 'NONE',  ( 6.232888004217203459, -1.964670499678453197, -0.6532144590316590893 ) ) ;
#185619 = CARTESIAN_POINT ( 'NONE',  ( -0.6823417656250212460, 1.363541667008083547, 1.181850606188755259 ) ) ;
#185620 = CARTESIAN_POINT ( 'NONE',  ( 3.638091081701349871, 0.9754702174074175725, -1.929073278114090684 ) ) ;
#185621 = CARTESIAN_POINT ( 'NONE',  ( 3.879560801468981523, 0.2449043481074340001, -2.004685163654993385 ) ) ;
#185624 = CARTESIAN_POINT ( 'NONE',  ( 5.829642864196168617, 6.863966765392747860, 1.082531754730558626 ) ) ;
#185623 = CARTESIAN_POINT ( 'NONE',  ( -1.642778471874998480, -3.201041666188710000, 2.845375778867863303 ) ) ;
#185622 = CARTESIAN_POINT ( 'NONE',  ( 0.000000000000000000, -3.499999999999999556, 0.000000000000000000 ) ) ;
#185625 = CARTESIAN_POINT ( 'NONE',  ( -5.712781623311813384, 7.758274208654143855, -1.599625672291271394 ) ) ;
#185626 = CARTESIAN_POINT ( 'NONE',  ( 2.747280062631300535, 0.2910806042949847239, -1.995268371848608835 ) ) ;
#185627 = CARTESIAN_POINT ( 'NONE',  ( -8.690940161559884913, 10.09818392903003748, 1.199719254218462483 ) ) ;
#185629 = SURFACE_SIDE_STYLE ('',( #119646 ) ) ;
#185628 = CARTESIAN_POINT ( 'NONE',  ( -3.795392936821753604, 6.515376628678959392, -1.199719254218452047 ) ) ;
#185630 = CARTESIAN_POINT ( 'NONE',  ( 1.499999999999993117, 12.60416666666666785, 0.8660254037844408170 ) ) ;
#185631 = CARTESIAN_POINT ( 'NONE',  ( -11.01445754936173849, 5.351296611813540771, -4.769094010048264387 ) ) ;
#185632 = EDGE_CURVE ( 'NONE', #126635, #88486, #171254, .T. ) ;
#185634 = CARTESIAN_POINT ( 'NONE',  ( 4.868767636308747093, -0.2496254991312534810, -2.000855965115163837 ) ) ;
#185633 = CARTESIAN_POINT ( 'NONE',  ( -6.656690234185426824, 10.70996300661758660, 0.7216878364870458196 ) ) ;
#185635 = CARTESIAN_POINT ( 'NONE',  ( -1.499999999999997780, 5.150000000000022560, 1.214306433183764966E-14 ) ) ;
#185636 = B_SPLINE_CURVE_WITH_KNOTS ( 'NONE', 3,
 ( #175577, #143107, #94339, #107430 ),
 .UNSPECIFIED., .F., .F.,
 ( 4, 4 ),
 ( 2.652056914724157932E-16, 7.241384396125386848E-05 ),
 .UNSPECIFIED. ) ;
#185637 = CARTESIAN_POINT ( 'NONE',  ( 0.1347971297303695026, -1.579520332396977089, 0.6935263066737175075 ) ) ;
#185638 = CARTESIAN_POINT ( 'NONE',  ( 4.766573523656222555, 7.718696989977711809, 1.199719254218452047 ) ) ;
#185640 = CARTESIAN_POINT ( 'NONE',  ( 1.946531837068834925, 3.754233237397152312, 0.4615996190889071760 ) ) ;
#185639 = CARTESIAN_POINT ( 'NONE',  ( 8.758204044748005401, 10.28062147603659504, 1.082531754730549967 ) ) ;
#185641 = CARTESIAN_POINT ( 'NONE',  ( -10.81128737566128528, 6.428770538698215020, 5.224633893128990181 ) ) ;
#185642 = CARTESIAN_POINT ( 'NONE',  ( 5.764887228985436707, -1.690807747980655584, -0.8004016547063924625 ) ) ;
#185643 = CARTESIAN_POINT ( 'NONE',  ( 0.08268127059449237315, -1.313209137626596634, 1.525886470183013044 ) ) ;
#185644 = DIRECTION ( 'NONE',  ( 0.000000000000000000, 1.000000000000000000, 0.000000000000000000 ) ) ;
#185645 = AXIS2_PLACEMENT_3D ( 'NONE', #34359, #18094, #85245 ) ;
#185646 = CARTESIAN_POINT ( 'NONE',  ( 0.7500000000000006661, 12.36458333401613174, 1.299038105676657340 ) ) ;
#185647 = EDGE_LOOP ( 'NONE', ( #144933, #205658, #69011, #68145, #90627, #42391, #137513, #160413, #210279, #14865, #22398, #125204, #202708 ) ) ;
#185648 = CARTESIAN_POINT ( 'NONE',  ( 10.34450801710256584, 11.17094022948226240, 0.7216878364870438212 ) ) ;
#185649 = CARTESIAN_POINT ( 'NONE',  ( 1.142204091441896718, 0.8197918422115093584, 1.842440257734210052 ) ) ;
#185650 = CARTESIAN_POINT ( 'NONE',  ( 3.228249973385329596, 6.780392379009261283, -1.734723475976807094E-15 ) ) ;
#185651 = CARTESIAN_POINT ( 'NONE',  ( 5.606297198005668392, 5.722949621141593113, -0.4987895298722895276 ) ) ;
#185652 = AXIS2_PLACEMENT_3D ( 'NONE', #26786, #162145, #47339 ) ;
#185653 = CARTESIAN_POINT ( 'NONE',  ( 7.985389288324691748, 10.33937347451072775, -1.443375672974058777 ) ) ;
#185654 = CARTESIAN_POINT ( 'NONE',  ( 5.425234023762710578, 9.481190127698507553, -0.7998128361456291469 ) ) ;
#185656 = CARTESIAN_POINT ( 'NONE',  ( 6.239839116978105338, 1.910102730490463641, -0.1462054744419109820 ) ) ;
#185655 = CARTESIAN_POINT ( 'NONE',  ( -5.742041750587549842, 6.657802449562273850, 1.199719254218450271 ) ) ;
#185657 = DIRECTION ( 'NONE',  ( 0.000000000000000000, 0.000000000000000000, 1.000000000000000000 ) ) ;
#185658 = CARTESIAN_POINT ( 'NONE',  ( -2.900957617708239678, -3.232243495192087757, 1.542507481629953103 ) ) ;
#185659 = EDGE_CURVE ( 'NONE', #9995, #128985, #11179, .T. ) ;
#185660 = LINE ( 'NONE', #37290, #32571 ) ;
#185662 = ORIENTED_EDGE ( 'NONE', *, *, #120407, .F. ) ;
#185661 = CARTESIAN_POINT ( 'NONE',  ( 3.334942599281629949, 5.874221551595115720, -1.082531754730543083 ) ) ;
#185663 = CARTESIAN_POINT ( 'NONE',  ( -4.135400547368138113, 4.783387712472935149, 1.199719254218462483 ) ) ;
#185664 =( GEOMETRIC_REPRESENTATION_CONTEXT ( 3 ) GLOBAL_UNCERTAINTY_ASSIGNED_CONTEXT ( ( #159191 ) ) GLOBAL_UNIT_ASSIGNED_CONTEXT ( ( #22164, #88279, #187893 ) ) REPRESENTATION_CONTEXT ( 'NONE', 'WORKASPACE' ) );
#185665 = CARTESIAN_POINT ( 'NONE',  ( 3.749029689823797806, -1.768526636652943296, 1.242828150824742961 ) ) ;
#185666 = CARTESIAN_POINT ( 'NONE',  ( -6.075462232699549325, 9.141770800574526845, 1.082531754730549967 ) ) ;
#185667 = CARTESIAN_POINT ( 'NONE',  ( 4.733205024946604667, 8.536173272497439513, 0.000000000000000000 ) ) ;
#185668 = CARTESIAN_POINT ( 'NONE',  ( 0.9672155168029163974, -1.668165459610539081, 1.309123814877902969 ) ) ;
#185669 = CARTESIAN_POINT ( 'NONE',  ( 5.385714059857480862, 1.227405483141888354, 1.351559456777707835 ) ) ;
#185670 = CARTESIAN_POINT ( 'NONE',  ( 2.635955087654485940, 0.9327151613215716175, -1.736774642614127284 ) ) ;
#185671 = CARTESIAN_POINT ( 'NONE',  ( 4.359561026920276916, -1.481784043772149229, -1.208992945495937610 ) ) ;
#185672 = VERTEX_POINT ( 'NONE', #58881 ) ;
#185673 = CARTESIAN_POINT ( 'NONE',  ( 0.000000000000000000, 14.48154074412737202, 0.000000000000000000 ) ) ;
#185674 = CARTESIAN_POINT ( 'NONE',  ( 5.758249387092365446, -1.969739562807392819, -0.001740234774137705337 ) ) ;
#185675 = CARTESIAN_POINT ( 'NONE',  ( 0.2869206542332564114, 1.438414604794725049, 1.304842588618974952 ) ) ;
#185676 = ORIENTED_EDGE ( 'NONE', *, *, #44682, .T. ) ;
#185677 = CARTESIAN_POINT ( 'NONE',  ( -4.339491684825780737, 7.220434844675483355, -1.199719254218455378 ) ) ;
#185678 = CARTESIAN_POINT ( 'NONE',  ( -2.823841133396259639, 6.516508098929413961, -0.7998128361456481317 ) ) ;
#185680 = CARTESIAN_POINT ( 'NONE',  ( 5.343321937117211817, 9.247976336696488886, 0.000000000000000000 ) ) ;
#185679 = CARTESIAN_POINT ( 'NONE',  ( 8.796542737168120851, 9.157054702984622097, -0.7998128361456211532 ) ) ;
#185682 = ORIENTED_EDGE ( 'NONE', *, *, #33285, .T. ) ;
#185681 = CARTESIAN_POINT ( 'NONE',  ( 4.617770051018644573, -0.5065499601877522240, 1.843912185298258066 ) ) ;
#185683 = CARTESIAN_POINT ( 'NONE',  ( 0.9212656856641410208, 2.039593612490635532, 0.8430313063367624871 ) ) ;
#185684 = CARTESIAN_POINT ( 'NONE',  ( 1.566597853258334894, 8.754643479813763562, 2.463935000416110022 ) ) ;
#185685 = CARTESIAN_POINT ( 'NONE',  ( 6.076820132975093713, -1.421968828841757126, 1.425219213311772926 ) ) ;
#185686 = CARTESIAN_POINT ( 'NONE',  ( -0.02319159430949970999, 4.096340798889516854, -2.366022381217198767 ) ) ;
#185687 = DIRECTION ( 'NONE',  ( 0.000000000000000000, -1.000000000000000000, -0.000000000000000000 ) ) ;
#185688 = CARTESIAN_POINT ( 'NONE',  ( -6.776593369756422902, -7.026643280347922627, -6.796618584848064692 ) ) ;
#185689 = CARTESIAN_POINT ( 'NONE',  ( 2.699741690289765295, -1.532448122638006671, -1.392287113214360605 ) ) ;
#185690 = CARTESIAN_POINT ( 'NONE',  ( -4.388035272317281077, 8.271124917678806199, 0.7998128361456481317 ) ) ;
#185691 = CARTESIAN_POINT ( 'NONE',  ( -4.768476522361002168, 8.183970109320437558, 0.7579922544750415936 ) ) ;
#185693 = CARTESIAN_POINT ( 'NONE',  ( 0.8136072859011161951, -0.3160970183575459447, 2.138355382504661506 ) ) ;
#185692 = CARTESIAN_POINT ( 'NONE',  ( -3.144601563365788444, 5.756120026313656268, -1.199719254218452935 ) ) ;
#185694 = CARTESIAN_POINT ( 'NONE',  ( 5.072158865288245444, 5.090142562357324429, 0.7216878364870338292 ) ) ;
#185695 = CARTESIAN_POINT ( 'NONE',  ( 1.490514837427020067, 7.209629588552884272, 4.246172784737224148 ) ) ;
#185696 = CARTESIAN_POINT ( 'NONE',  ( -1.364683531250014514, 13.40104166700806587, -0.7879004041258335089 ) ) ;
#185698 = CARTESIAN_POINT ( 'NONE',  ( -5.818384198920079520, 6.817144982608731141, 1.199719254218452935 ) ) ;
#185697 = CARTESIAN_POINT ( 'NONE',  ( 0.000000000000000000, 13.49999999999999822, 0.000000000000000000 ) ) ;
#185699 = CARTESIAN_POINT ( 'NONE',  ( 5.414640894582111841, -1.106827951885097638, -1.334981224695269475 ) ) ;
#185700 = CARTESIAN_POINT ( 'NONE',  ( -4.464712657601869417, 4.103252943490596216, 0.7998128361456341429 ) ) ;
#185701 = CARTESIAN_POINT ( 'NONE',  ( 3.309495622959734096, -1.689761761210720525, -1.195817184978978043 ) ) ;
#185702 = CARTESIAN_POINT ( 'NONE',  ( 4.622735098982394319, 0.3634473554468270473, 2.085661844363582595 ) ) ;
#185703 = CARTESIAN_POINT ( 'NONE',  ( 6.588372581236919601, 9.773852880496709972, -1.199719254218440723 ) ) ;
#185704 = CARTESIAN_POINT ( 'NONE',  ( -0.6823417656249969321, 4.467708333674755394, -1.181850606188749264 ) ) ;
#185705 = CARTESIAN_POINT ( 'NONE',  ( 2.500782807205007341, 0.4266943614082556180, 1.922505800989605218 ) ) ;
#185706 = CARTESIAN_POINT ( 'NONE',  ( 1.371198541116287917, -1.641758494746584418, -0.9804709962101465504 ) ) ;
#185707 = CARTESIAN_POINT ( 'NONE',  ( 4.962941676929116142, 0.2283445767556212536, -2.280853557871139525 ) ) ;
#185708 = CARTESIAN_POINT ( 'NONE',  ( 2.947667120405720986, 0.6567698719579934119, -1.703645827024417914 ) ) ;
#185709 = CARTESIAN_POINT ( 'NONE',  ( 5.041653019435334393, 6.975290837464928728, -1.599625672291269396 ) ) ;
#185710 = CARTESIAN_POINT ( 'NONE',  ( 5.300874872818828187, 8.167809204055208383, 1.082531754730558626 ) ) ;
#185711 = CARTESIAN_POINT ( 'NONE',  ( -7.705111371268023923, 7.883718109434487253, 1.040834085586084257E-14 ) ) ;
#185712 = CARTESIAN_POINT ( 'NONE',  ( 4.535406599088565471, -0.09463749723611977749, 2.011077795214308406 ) ) ;
#185713 = CARTESIAN_POINT ( 'NONE',  ( 2.746866186719683967, -0.3305370478365337039, -1.933541032166598672 ) ) ;
#185714 = CARTESIAN_POINT ( 'NONE',  ( -8.016948904382338981, 8.247528564734524892, -0.7998128361456291469 ) ) ;
#185715 = AXIS2_PLACEMENT_3D ( 'NONE', #41114, #29109, #93064 ) ;
#185716 = CARTESIAN_POINT ( 'NONE',  ( -5.545448523189368650, 6.428443684264421698, -1.199719254218446718 ) ) ;
#185717 = CARTESIAN_POINT ( 'NONE',  ( 0.07536363704233400851, 2.864322694550157866, -2.632457840217194089 ) ) ;
#185719 = CARTESIAN_POINT ( 'NONE',  ( 4.363939919551316216, 0.8349522575829392279, 1.560488599360178474 ) ) ;
#185718 = CARTESIAN_POINT ( 'NONE',  ( 6.228480176075449570, 0.2035102421588113053, 2.080708833908810451 ) ) ;
#185720 = FACE_OUTER_BOUND ( 'NONE', #28798, .T. ) ;
#185721 = CARTESIAN_POINT ( 'NONE',  ( 0.6038064816080711550, -2.180521553291506986, 0.2185767975278959385 ) ) ;
#185722 = CARTESIAN_POINT ( 'NONE',  ( 0.1689663589281220069, 0.9994598401263864451, 1.424626921871420926 ) ) ;
#185723 = CARTESIAN_POINT ( 'NONE',  ( 7.426115451983150706, 9.686887332112256388, -1.599625672291262513 ) ) ;
#185724 = DIRECTION ( 'NONE',  ( 0.000000000000000000, 1.000000000000000000, 0.000000000000000000 ) ) ;
#185725 = CARTESIAN_POINT ( 'NONE',  ( 0.3691051123158794467, -0.6094954538576388137, 2.216020297015007134 ) ) ;
#185726 = CARTESIAN_POINT ( 'NONE',  ( 0.3456114054924685486, 0.6817542107791437767, -2.082909237240769151 ) ) ;
#185727 = CARTESIAN_POINT ( 'NONE',  ( 6.819718782980952909, -1.336886906709513712, 1.104006757392479887 ) ) ;
#185728 = CARTESIAN_POINT ( 'NONE',  ( 3.000804911251079510, -0.6410980074830170405, -2.111705341948390657 ) ) ;
#185729 = CARTESIAN_POINT ( 'NONE',  ( 6.549308719555964053, 1.892307808498715049, -1.064380946037797093 ) ) ;
#185730 = FACE_OUTER_BOUND ( 'NONE', #89622, .T. ) ;
#185731 = CARTESIAN_POINT ( 'NONE',  ( 1.235738130824210357, 0.6087300624019938988, -2.027988197625143929 ) ) ;
#185732 = CARTESIAN_POINT ( 'NONE',  ( 3.968750000000002665, 0.7852924748297764879, -1.895863743164168724 ) ) ;
#185733 = CARTESIAN_POINT ( 'NONE',  ( 6.727182134110176293, 6.032839922080010631, 2.883943260000087605 ) ) ;
#185734 = CARTESIAN_POINT ( 'NONE',  ( 5.016589502704805525, 1.328544886203905318, -1.395186341261208884 ) ) ;
#185735 = ORIENTED_EDGE ( 'NONE', *, *, #103939, .T. ) ;
#185737 = CARTESIAN_POINT ( 'NONE',  ( 1.364683531249986537, -1.073958332991911790, 0.7879004041258500513 ) ) ;
#185736 = CARTESIAN_POINT ( 'NONE',  ( 1.453083402393087642, -1.969018001514400540, -1.173635730923931808 ) ) ;
#185738 = CARTESIAN_POINT ( 'NONE',  ( 4.090809663021327758, 5.795697244990093644, 1.599625672291267398 ) ) ;
#185739 = CARTESIAN_POINT ( 'NONE',  ( 5.843727902690005749, 6.776436293681846301, -1.199719254218445830 ) ) ;
#185740 = CARTESIAN_POINT ( 'NONE',  ( 3.299698294838341539, 2.007417196159299255, -0.9513305067451423014 ) ) ;
#185741 = CARTESIAN_POINT ( 'NONE',  ( -6.873620692448438874, 10.96304854125777695, 0.000000000000000000 ) ) ;
#185742 = ADVANCED_FACE ( 'NONE', ( #190992 ), #209370, .T. ) ;
#185743 = CARTESIAN_POINT ( 'NONE',  ( 4.690757960648221037, 7.456006139856155457, 1.082531754730558626 ) ) ;
#185744 = CARTESIAN_POINT ( 'NONE',  ( -8.649738815394339753, 9.193709494155953621, 1.040834085586084257E-14 ) ) ;
#185745 = CARTESIAN_POINT ( 'NONE',  ( 4.733205024946604667, 8.536173272497439513, 0.000000000000000000 ) ) ;
#185746 = AXIS2_PLACEMENT_3D ( 'NONE', #112543, #212086, #177488 ) ;
#185747 = CARTESIAN_POINT ( 'NONE',  ( 2.180314765559120183, 1.560501322096979449, 1.277041908422072991 ) ) ;
#185749 = CARTESIAN_POINT ( 'NONE',  ( 6.478975546884585768, 1.923237475310497047, 0.7459448616168369295 ) ) ;
#185748 = CARTESIAN_POINT ( 'NONE',  ( 6.414979237560321401, 10.63589287712906462, 1.040834085586084257E-14 ) ) ;
#185750 = CARTESIAN_POINT ( 'NONE',  ( -15.75000000000000000, 13.79999999999999893, 0.6999999999999992895 ) ) ;
#185751 = CARTESIAN_POINT ( 'NONE',  ( 5.682275777458841048, 8.683053269460405232, 1.082531754730547524 ) ) ;
#185752 = CARTESIAN_POINT ( 'NONE',  ( 6.321804186586025942, 0.9940233051523542640, -1.428469917405380318 ) ) ;
#185753 = CARTESIAN_POINT ( 'NONE',  ( -3.903950209304078989, 8.999999999999998224, 0.7749999999999996891 ) ) ;
#185754 = CARTESIAN_POINT ( 'NONE',  ( -1.364683531249997417, 2.759375000341422801, 1.214306433183764966E-14 ) ) ;
#185755 = CARTESIAN_POINT ( 'NONE',  ( 2.582953972192280734, 1.619985402465830671, -0.7128798769604760555 ) ) ;
#185756 = CARTESIAN_POINT ( 'NONE',  ( 1.231092510272915552, 2.014232830173094513, 0.09613330637052441840 ) ) ;
#185757 = CARTESIAN_POINT ( 'NONE',  ( 0.4679805871025365382, -1.733519288248483559, -0.6209854868195128219 ) ) ;
#185758 = CARTESIAN_POINT ( 'NONE',  ( 5.724266765471021756, 2.208406811287708660, 0.6146092054917261516 ) ) ;
#185759 = CARTESIAN_POINT ( 'NONE',  ( 2.923586578878138109, 1.022379729796508041, -1.530975008504284141 ) ) ;
#185760 = EDGE_CURVE ( 'NONE', #9480, #212749, #205415, .T. ) ;
#185761 = CARTESIAN_POINT ( 'NONE',  ( 9.271078113646423091, 9.710679308875986848, 1.040834085586084257E-14 ) ) ;
#185762 = CARTESIAN_POINT ( 'NONE',  ( 3.821172736587064023, -0.1348131347885111742, 1.820669774636254346 ) ) ;
#185763 = CARTESIAN_POINT ( 'NONE',  ( 5.309220276109914316, 1.198862193007979471, -1.621181151826488254 ) ) ;
#185764 = CARTESIAN_POINT ( 'NONE',  ( -8.097244055859620815, 10.46987070330147063, -1.599625672291263179 ) ) ;
#185766 = CARTESIAN_POINT ( 'NONE',  ( -6.474900878978163021, 9.711745571186627402, -1.199719254218452047 ) ) ;
#185765 = CARTESIAN_POINT ( 'NONE',  ( 3.081239027650189310, -0.1650901621712965450, -2.256537306257479614 ) ) ;
#185767 = CARTESIAN_POINT ( 'NONE',  ( 6.159223736743516753, -1.804415119744419149, -1.085654967431331164 ) ) ;
#185768 = CARTESIAN_POINT ( 'NONE',  ( -1.387358672527334136, 7.251968950354660493, -4.302625267139479348 ) ) ;
#185769 = CARTESIAN_POINT ( 'NONE',  ( 3.244645865714153032, -2.039272935636734285, -0.3565889006169955522 ) ) ;
#185770 = CARTESIAN_POINT ( 'NONE',  ( 4.729096653068339151, 4.411700938201493116, -0.7998128361456211532 ) ) ;
#185771 = CARTESIAN_POINT ( 'NONE',  ( -4.957638175832625493E-14, 1.734375000341442208, 1.570758158831756068 ) ) ;
#185772 = CARTESIAN_POINT ( 'NONE',  ( 5.690118541956746157, 1.263103799472656164, 1.703077153987264669 ) ) ;
#185773 = APPLICATION_PROTOCOL_DEFINITION ( 'draft international standard', 'automotive_design', 1998, #130779 ) ;
#185775 = CARTESIAN_POINT ( 'NONE',  ( 2.209485269003717445, -0.4220890577730853632, 1.879544223609790565 ) ) ;
#185774 = CARTESIAN_POINT ( 'NONE',  ( -10.31505594189871111, 10.92865344183699428, -0.7998128361456291469 ) ) ;
#185776 = DIRECTION ( 'NONE',  ( 0.000000000000000000, 0.000000000000000000, 1.000000000000000000 ) ) ;
#185777 = CARTESIAN_POINT ( 'NONE',  ( 6.420757345757475143, -1.395243968761919362, 1.390232514205336001 ) ) ;
#185778 = CARTESIAN_POINT ( 'NONE',  ( 5.838973523318124137, 6.009393772954500612, 0.3882124113597507087 ) ) ;
#185779 = CARTESIAN_POINT ( 'NONE',  ( -15.75000000000000000, 10.90000000000000036, -1.400000000000001910 ) ) ;
#185780 = CARTESIAN_POINT ( 'NONE',  ( -2.117044542028253318, 5.621635732341564662, -0.7998128361456281477 ) ) ;
#185781 = CARTESIAN_POINT ( 'NONE',  ( 0.2643399247034176613, 0.6888887472211238094, -2.111998681152967183 ) ) ;
#185782 = CARTESIAN_POINT ( 'NONE',  ( 3.803828919190560764, -0.6134138247068477989, 2.014629399117270125 ) ) ;
#185783 = CARTESIAN_POINT ( 'NONE',  ( -5.167592825464113915, 6.057888380243431570, 1.199719254218452935 ) ) ;
#185784 = CARTESIAN_POINT ( 'NONE',  ( 6.100279051144945619, 9.204410428722734849, -1.199719254218440723 ) ) ;
#185785 = CARTESIAN_POINT ( 'NONE',  ( 0.5021285002191768765, 1.855665429770089636, 0.1426183976328247727 ) ) ;
#185786 = CARTESIAN_POINT ( 'NONE',  ( 7.610204295972345712, 7.772993188256215547, 0.7998128361456341429 ) ) ;
#185787 = CARTESIAN_POINT ( 'NONE',  ( 3.798255590122797898, 7.583048621785260401, -0.7998128361456221525 ) ) ;
#185788 = CARTESIAN_POINT ( 'NONE',  ( -7.431277594066152403, 8.802816960232885179, -1.082531754730549967 ) ) ;
#185790 = CARTESIAN_POINT ( 'NONE',  ( -8.351459436338048548, 8.845716885256940998, -0.7216878364870278340 ) ) ;
#185789 = AXIS2_PLACEMENT_3D ( 'NONE', #133128, #161334, #47601 ) ;
#185791 = CARTESIAN_POINT ( 'NONE',  ( 1.125412309253082332, 1.872817075645373697, 0.9946839901537674056 ) ) ;
#185792 = CARTESIAN_POINT ( 'NONE',  ( -6.454563648557663846, 9.688018802362710957, -1.199719254218452047 ) ) ;
#185794 = CARTESIAN_POINT ( 'NONE',  ( 4.351973852746993110, -0.7528527933186466292, 1.811862133468461922 ) ) ;
#185793 = CARTESIAN_POINT ( 'NONE',  ( 0.6124999999999707345, 0.4166666666666901664, -1.060881119635969094 ) ) ;
#185795 = CARTESIAN_POINT ( 'NONE',  ( 1.622176833581047806, -1.201014165160016356, -1.797165035535647659 ) ) ;
#185796 = CARTESIAN_POINT ( 'NONE',  ( 2.138008341990283778, 0.4048980806483238326, 1.796005048712509655 ) ) ;
#185798 = CARTESIAN_POINT ( 'NONE',  ( -5.357982633755392854, 6.353232995037386033, -1.097174801447881487 ) ) ;
#185797 = CARTESIAN_POINT ( 'NONE',  ( -1.020505294851981049E-14, -5.907420853759271395, -10.91970695577494332 ) ) ;
#185799 = ADVANCED_FACE ( 'NONE', ( #40512 ), #107700, .T. ) ;
#185800 = CARTESIAN_POINT ( 'NONE',  ( 4.031004160980892870, -1.202209430963938619, -1.258585379614601596 ) ) ;
#185801 = FACE_OUTER_BOUND ( 'NONE', #137019, .T. ) ;
#185802 = CARTESIAN_POINT ( 'NONE',  ( 4.853455804012212660, 7.645820290447483458, 1.082531754730558626 ) ) ;
#185803 = CARTESIAN_POINT ( 'NONE',  ( -10.28823555840286552, 6.680969737303435352, 5.325637450257892702 ) ) ;
#185804 = CARTESIAN_POINT ( 'NONE',  ( 0.5499753625364013354, 0.6768306982547143136, -2.053065283773393368 ) ) ;
#185805 = CARTESIAN_POINT ( 'NONE',  ( 3.620470095612156047, 0.4925664443866035191, -1.954873191151075940 ) ) ;
#185806 = LINE ( 'NONE', #37439, #186291 ) ;
#185807 = DIRECTION ( 'NONE',  ( -1.000000000000000000, 7.771561172376097755E-16, 4.440892098500627148E-16 ) ) ;
#185808 = CARTESIAN_POINT ( 'NONE',  ( 3.344560887785383851, 0.4775036937760200884, 1.912655531573831835 ) ) ;
#185809 = ADVANCED_FACE ( 'NONE', ( #140158 ), #29025, .F. ) ;
#185810 = CARTESIAN_POINT ( 'NONE',  ( 6.609000000000018638, 2.976782768882420438, 2.353557172130323227 ) ) ;
#185811 = CARTESIAN_POINT ( 'NONE',  ( 2.612754452619329371, -0.1881026344860724786, 1.932912858947251511 ) ) ;
#185814 = ORIENTED_EDGE ( 'NONE', *, *, #103222, .T. ) ;
#185813 = CARTESIAN_POINT ( 'NONE',  ( -4.828112100242294424, 5.765790550771681566, -1.082531754730549967 ) ) ;
#185812 = CARTESIAN_POINT ( 'NONE',  ( 6.469012471580376733, -1.473683540339595810, 1.218514635347216046 ) ) ;
#185816 = ADVANCED_FACE ( 'NONE', ( #28516 ), #160650, .F. ) ;
#185815 = CARTESIAN_POINT ( 'NONE',  ( -3.485854892044994102, 7.080931450778859215, -0.7216878364870458196 ) ) ;
#185817 = CARTESIAN_POINT ( 'NONE',  ( 6.086684617892325733, 6.065829907154645539, -0.7998128361456481317 ) ) ;
#185818 = CARTESIAN_POINT ( 'NONE',  ( -4.685224601974262271, 7.623789914682047808, -1.199719254218453823 ) ) ;
#185819 = CARTESIAN_POINT ( 'NONE',  ( -6.794571259104023930, 7.956029886156682274, 1.199719254218452047 ) ) ;
#185820 = CARTESIAN_POINT ( 'NONE',  ( -8.473482818416664841, 11.86918514058604757, -1.082531754730543083 ) ) ;
#185821 = CARTESIAN_POINT ( 'NONE',  ( 0.5170026063063514199, 1.520138765826519300, -1.599913083071627273 ) ) ;
#185822 = CARTESIAN_POINT ( 'NONE',  ( -9.771731810572180876, 4.446950909175569677, 6.897090129977483386 ) ) ;
#185823 = CARTESIAN_POINT ( 'NONE',  ( 4.680490258543752446, 1.210089798712219222, -1.543956201849092658 ) ) ;
#185824 = CARTESIAN_POINT ( 'NONE',  ( 8.457588896826466751, 8.761608555919362828, 1.040834085586084257E-14 ) ) ;
#185825 = CARTESIAN_POINT ( 'NONE',  ( 1.881482635453747720, -0.5404922439061732309, -1.942541187959702764 ) ) ;
#185826 = ORIENTED_EDGE ( 'NONE', *, *, #97562, .F. ) ;
#185827 = CARTESIAN_POINT ( 'NONE',  ( 2.202504513770195516, 1.378945901905674232, -1.606877091071600816 ) ) ;
#185828 = CARTESIAN_POINT ( 'NONE',  ( -1.499999999999997780, 2.181250000682817713, 1.214306433183764966E-14 ) ) ;
#185830 = CARTESIAN_POINT ( 'NONE',  ( -5.473741331615264549, 7.409117525016355010, -1.599625672291256295 ) ) ;
#185829 = CARTESIAN_POINT ( 'NONE',  ( -2.137381772448751605, 5.645362501165475777, -0.7998128361456281477 ) ) ;
#185831 = CARTESIAN_POINT ( 'NONE',  ( 3.450948914068392881, 0.4461466885457600062, -1.786139022923169506 ) ) ;
#185832 = ORIENTED_EDGE ( 'NONE', *, *, #56390, .T. ) ;
#185833 = CARTESIAN_POINT ( 'NONE',  ( -8.779068160048691283, 10.20099992726700933, -1.199719254218446718 ) ) ;
#185834 = SURFACE_STYLE_USAGE ( .BOTH. , #119856 ) ;
#185835 = CARTESIAN_POINT ( 'NONE',  ( 4.324552338190708056, -0.9094542848507057853, -1.915842285305848769 ) ) ;
#185836 = DIRECTION ( 'NONE',  ( -1.000000000000000000, 0.000000000000000000, 0.000000000000000000 ) ) ;
#185837 = CARTESIAN_POINT ( 'NONE',  ( 7.474622759835693131, 7.614814729430110951, -0.7998128361456281477 ) ) ;
#185838 = CARTESIAN_POINT ( 'NONE',  ( 5.360643824631334375, -1.495535663558609674, 1.418079957933044755 ) ) ;
#185840 = CARTESIAN_POINT ( 'NONE',  ( 2.753256032281672372, 1.832158412346639453, -0.1828795585285883096 ) ) ;
#185839 = CARTESIAN_POINT ( 'NONE',  ( -5.852315862593199469, 9.979452273000736895, 0.7998128361456481317 ) ) ;
#185841 = CARTESIAN_POINT ( 'NONE',  ( 9.433775957010412938, 9.900493459467314850, 0.000000000000000000 ) ) ;
#185842 = DIRECTION ( 'NONE',  ( 0.000000000000000000, 1.000000000000000000, 0.000000000000000000 ) ) ;
#185843 =( BOUNDED_SURFACE ( )  B_SPLINE_SURFACE ( 1, 2, ( 
 ( #176652, #146307, #30411, #113856, #97549, #81278, #63958, #65006, #192878, #27187, #145257, #130114, #179851, #129055, #211262, #93293, #95430, #45600, #28265, #110651, #212321, #77001, #163606, #44533, #15188, #31474, #94357, #196104, #127998, #62886, #195029, #47740, #143127, #209122, #160399, #147355, #46663, #193952, #112784, #144200, #60760, #96495, #111717, #177725, #162545, #14115, #69253, #119159, #66052, #183029, #164660, #152665, #84463, #117034, #34645, #101784, #165724, #17312, #132196, #83390, #98598, #181954, #33582, #198203, #100715, #115964, #99655, #149474, #70318, #1057, #4249, #67122, #136435, #151615, #202450, #20514, #133255, #114903, #199261, #180900, #32523, #86599, #150554, #16242, #118103, #168911, #82328, #167851, #49838, #19450, #135370, #2115, #166792, #18386, #148420, #35707, #50906, #184088, #68189, #3182, #185144, #134322, #200328, #51978, #85526, #201388, #53026, #36769, #102855, #111133, #172123, #6390, #120240, #173203, #25848, #141792, #9605, #75682, #187290, #56235, #155872, #24783, #38917, #122395, #54105, #186218, #107177, #22638, #41070, #88747, #23717, #37849, #103927, #153738, #205664, #188353, #89824, #73540, #105001, #169972, #171040, #87666, #39992, #190478, #21560, #123465, #5305, #158017, #71387, #137499, #91956, #57302, #189428, #203516, #139642, #90886, #55170, #121315, #154804, #106101, #7461, #72463, #138563, #174273, #204584, #156945, #8536, #74617, #140723, #206736, #58367, #124521, #108252, #42137, #47465, #44259, #30127, #191542, #178516, #125582, #176387, #77803, #61557, #179582, #144980, #113580, #13854, #161198, #76731, #159063, #97278, #60484, #210984, #112505, #27992, #26913, #146036, #96216, #129844, #43207, #193682, #162267, #110382, #126642, #10659, #79930, #175330, #109322, #59424, #31204, #128774, #127723, #81006, #94089, #192607, #160128, #11727, #143923, #93022, #209919, #142849, #12785, #163332, #45326, #207796, #212050, #14912, #208853, #111445, #177450, #63690, #29064, #95147, #78859, #62612, #194751, #46388, #195826, #115692, #147094, #778, #134062, #183833, #168652, #181685, #82061, #201129, #116762, #200071, #32259, #118903, #52767, #33314, #149203, #85267, #68996, #184887, #35442, #36511, #164393, #213117, #50635, #101521, #151354, #100450, #182759, #64748, #66845, #17044, #148153, #214154, #167591, #48522, #135113, #15975, #102596, #2923, #65780, #117841, #99396, #198989, #132989, #19190, #20256, #130890, #131930, #196884, #34377, #165449, #166523, #197940, #114642, #18114, #180635, #98327, #49568, #83123, #84201, #150290, #1857, #67916, #51720, #124272, #55980, #88491, #6131, #73274, #137246, #203267, #103672, #54913, #70060, #153483, #5054, #169720, #72200, #87417, #71129, #121064, #41889, #187031, #190230, #38664, #108000, #123213, #174027, #206483, #104743, #86340, #170790, #152412, #3991, #58113, #122133, #136172, #89567, #140471, #202191, #139377, #21310, #205409, #40814, #188098, #138308, #154551, #53847, #7201, #22381, #155616, #37590, #189176, #90634, #204323, #39729, #105834, #171860, #23455, #57049, #106922, #172946, #24525, #156694, #8284, #119980, #74369, #185958, #113339, #195588, #47222, #158818, #27746, #127476, #210754, #10414, #93842, #25598, #91711, #128540, #157760, #26669, #62376, #94903, #194506, #9359, #92774, #46154, #160954, #178281, #162028, #145805, #112267, #63449, #42958, #75432, #143680, #29890, #95975, #193447, #209672, #141544, #159880, #110134, #76486, #175083, #13619, #207550, #79692, #109067, #211812, #129602, #142596, #59170, #60238, #77557, #11485, #125329, #191292, #208606, #126397, #192357, #61315, #44014, #45091, #176146, #111200, #177204, #28818, #12544, #78618, #144743, #133808, #183578, #130656, #33079, #14675, #2671, #148958, #181448, #99154, #166268, #15740, #81825, #196647, #147907, #163095, #32018, #98103, #48287, #165207, #180397, #164154, #213923, #134866, #65546, #68744, #131691, #200873, #1604, #52518, #85017, #197697, #179345, #49339, #30967, #97042, #151106, #530, #80772, #182502, #18931, #146859, #17860, #114399, #83943, #199821, #66597, #16797, #82881, #212881, #100202, #115458 ),
 ( #132743, #198745, #150034, #50393, #67664, #116513, #34133, #64512, #51463, #117587, #35185, #101261, #167345, #138052, #103407, #73021, #118650, #20001, #87150, #185700, #69806, #184636, #56789, #153221, #36253, #186777, #105566, #155355, #140207, #4791, #53586, #172686, #88225, #171599, #3731, #90369, #24264, #70869, #120801, #23191, #136984, #89306, #203011, #154294, #74112, #102333, #135912, #55717, #38404, #22114, #204065, #169468, #168405, #21053, #152162, #104486, #40555, #86086, #187842, #201930, #8021, #119721, #37332, #156437, #121871, #39468, #54651, #6940, #139119, #170529, #206227, #5869, #71941, #205146, #122957, #188917, #106659, #58923, #25348, #107747, #143418, #209413, #192103, #93586, #41633, #112018, #109882, #178019, #108813, #94651, #173772, #28563, #189981, #26414, #142348, #126142, #29637, #61059, #95722, #78369, #11225, #141291, #9104, #161774, #125082, #127218, #176947, #92526, #91448, #210496, #160695, #194254, #157509, #43769, #12288, #174836, #191039, #75180, #144489, #207300, #42705, #124014, #13367, #193186, #175894, #145558, #158565, #10165, #76239, #208357, #59988, #27486, #159630, #77306, #44835, #79441, #110941, #57854, #62132, #128292, #45899, #129355, #48040, #17608, #164954, #80508, #162841, #103966, #64265, #282, #116265, #31774, #30708, #149781, #33881, #133560, #46964, #197446, #166023, #114155, #130409, #14419, #99958, #179086, #113081, #63190, #120279, #132499, #65296, #87701, #180148, #196397, #97845, #163909, #15485, #195333, #81572, #146605, #16546, #186253, #49087, #211556, #83693, #170008, #96792, #212624, #147656, #1356, #213672, #131443, #115206, #181197, #32825, #98901, #67418, #82627, #148713, #66354, #198498, #202491, #21596, #50143, #182256, #54143, #37888, #188392, #203555, #73580, #7496, #171078, #88786, #40028, #105041, #106140, #22674, #72502, #139682, #153774, #55208, #122434, #6428, #138601, #56275, #38958, #71426, #154843, #121354, #204624, #205704, #137538, #172163, #5344, #187329, #23756, #89861, #155911, #129447, #97942, #147747, #96883, #47059, #143515, #211649, #13459, #144583, #78464, #180241, #44929, #65386, #12385, #197535, #81661, #210597, #114244, #178116, #195429, #63286, #163998, #98992, #32915, #128383, #15573, #113176, #29731, #179180, #194351, #213765, #30803, #131533, #49180, #209511, #112113, #79535, #162932, #115298, #80606, #181288, #165047, #14513, #62226, #94746, #16639, #45993, #146701, #48131, #95813, #177044, #61152, #31865, #127314, #193284, #212716, #111037, #161871, #145653, #160793, #28660, #64356, #130502, #196489, #202850, #3576, #150947, #170370, #51302, #149878, #133655, #117427, #199656, #66443, #35026, #33973, #36095, #54498, #68584, #82723, #103250, #38247, #132584, #369, #183425, #37175, #148800, #198587, #101099, #83784, #85932, #69651, #100048, #152004, #166112, #185546, #86991, #1444, #167185, #67509, #84858, #18773, #17697, #135759, #2511, #201781, #200716, #134709, #50233, #53422, #120642, #116354, #104322, #182343, #52367, #118496, #184477, #119558, #102179, #168246, #19845, #169311, #20895, #153064, #4640, #70711, #136823, #186621, #158403, #142179, #124916, #108648, #41472, #23035, #7862, #190879, #26248, #189823, #140042, #21956, #90214, #106499, #89150, #171445, #58763, #137898, #10003, #105408, #76079, #174676, #155204, #207139, #56634, #73949, #156278, #42544, #191938, #125980, #6785, #92367, #206066, #122799, #208195, #71783, #75018, #72862, #141128, #59828, #43602, #25187, #138968, #91291, #157349, #39313, #8938, #187684, #109720, #88065, #204990, #188757, #40398, #24111, #172527, #57701, #154137, #123857, #5706, #107582, #173615, #203917, #55565, #121719, #48922, #131293, #197282, #94492, #177861, #63027, #146444, #160530, #29473, #175726, #27321, #64102, #93423, #176781, #212456, #30546, #113991, #97683, #81411, #130243, #47877, #195171, #28397, #161614, #196235, #179986, #129194, #79280, #159461, #95563, #45737, #12135, #110780, #31608, #77140, #163742, #44668, #15321, #147492, #78207, #213514, #210331, #13205, #145398, #65136, #11061, #143261, #144332, #209251, #211397, #61970, #46805, #128125 ) ),
 .UNSPECIFIED., .F., .F., .T. ) 
 B_SPLINE_SURFACE_WITH_KNOTS ( ( 2, 2 ),
 ( 3, 2, 2, 2, 2, 2, 2, 2, 2, 2, 2, 2, 2, 2, 2, 2, 2, 2, 2, 2, 2, 2, 2, 2, 2, 2, 2, 2, 2, 2, 2, 2, 2, 2, 2, 2, 2, 2, 2, 2, 2, 2, 2, 2, 2, 2, 2, 2, 2, 2, 2, 2, 2, 2, 2, 2, 2, 2, 2, 2, 2, 2, 2, 2, 2, 2, 2, 2, 2, 2, 2, 2, 2, 2, 2, 2, 2, 2, 2, 2, 2, 2, 2, 2, 2, 2, 2, 2, 2, 2, 2, 2, 2, 2, 2, 2, 2, 2, 2, 2, 2, 2, 2, 2, 2, 2, 2, 2, 2, 2, 2, 2, 2, 2, 2, 2, 2, 2, 2, 2, 2, 2, 2, 2, 2, 2, 2, 2, 2, 2, 2, 2, 2, 2, 2, 2, 2, 2, 2, 2, 2, 2, 2, 2, 2, 2, 2, 2, 2, 2, 2, 2, 2, 2, 2, 2, 2, 2, 2, 2, 2, 2, 2, 2, 2, 2, 2, 2, 2, 2, 2, 2, 2, 2, 2, 2, 2, 2, 2, 2, 2, 2, 2, 2, 2, 2, 2, 2, 2, 2, 2, 2, 2, 2, 2, 2, 2, 2, 2, 2, 2, 2, 2, 2, 2, 2, 2, 2, 2, 2, 2, 2, 2, 2, 2, 2, 2, 2, 2, 2, 2, 2, 2, 2, 2, 2, 2, 2, 2, 2, 2, 2, 2, 2, 2, 2, 2, 2, 2, 2, 3 ),
 ( 0.000000000000000000, 1.000000000000000000 ),
 ( 0.000000000000000000, 0.004166666666666666609, 0.008333333333333333218, 0.01250000000000000069, 0.01666666666666666644, 0.02083333333333333218, 0.02500000000000000139, 0.02916666666666666713, 0.03333333333333333287, 0.03749999999999999861, 0.04166666666666666435, 0.04583333333333333010, 0.05000000000000000278, 0.05416666666666666852, 0.05833333333333333426, 0.06250000000000000000, 0.06666666666666666574, 0.07083333333333333148, 0.07499999999999999722, 0.07916666666666666297, 0.08333333333333332871, 0.08749999999999999445, 0.09166666666666666019, 0.09583333333333333981, 0.1000000000000000056, 0.1041666666666666713, 0.1083333333333333370, 0.1125000000000000028, 0.1166666666666666685, 0.1208333333333333343, 0.1250000000000000000, 0.1291666666666666796, 0.1333333333333333315, 0.1375000000000000111, 0.1416666666666666630, 0.1458333333333333426, 0.1499999999999999944, 0.1541666666666666741, 0.1583333333333333259, 0.1625000000000000056, 0.1666666666666666574, 0.1708333333333333370, 0.1749999999999999889, 0.1791666666666666685, 0.1833333333333333204, 0.1875000000000000000, 0.1916666666666666796, 0.1958333333333333315, 0.2000000000000000111, 0.2041666666666666630, 0.2083333333333333426, 0.2124999999999999944, 0.2166666666666666741, 0.2208333333333333259, 0.2250000000000000056, 0.2291666666666666574, 0.2333333333333333370, 0.2374999999999999889, 0.2416666666666666685, 0.2458333333333333204, 0.2500000000000000000, 0.2541666666666666519, 0.2583333333333333592, 0.2625000000000000111, 0.2666666666666666630, 0.2708333333333333148, 0.2750000000000000222, 0.2791666666666666741, 0.2833333333333333259, 0.2874999999999999778, 0.2916666666666666852, 0.2958333333333333370, 0.2999999999999999889, 0.3041666666666666408, 0.3083333333333333481, 0.3125000000000000000, 0.3166666666666666519, 0.3208333333333333592, 0.3250000000000000111, 0.3291666666666666630, 0.3333333333333333148, 0.3375000000000000222, 0.3416666666666666741, 0.3458333333333333259, 0.3499999999999999778, 0.3541666666666666852, 0.3583333333333333370, 0.3624999999999999889, 0.3666666666666666408, 0.3708333333333333481, 0.3750000000000000000, 0.3791666666666666519, 0.3833333333333333592, 0.3875000000000000111, 0.3916666666666666630, 0.3958333333333333148, 0.4000000000000000222, 0.4041666666666666741, 0.4083333333333333259, 0.4124999999999999778, 0.4166666666666666852, 0.4208333333333333370, 0.4249999999999999889, 0.4291666666666666408, 0.4333333333333333481, 0.4375000000000000000, 0.4416666666666666519, 0.4458333333333333592, 0.4500000000000000111, 0.4541666666666666630, 0.4583333333333333148, 0.4625000000000000222, 0.4666666666666666741, 0.4708333333333333259, 0.4749999999999999778, 0.4791666666666666852, 0.4833333333333333370, 0.4874999999999999889, 0.4916666666666666408, 0.4958333333333333481, 0.5000000000000000000, 0.5041666666666666519, 0.5083333333333333037, 0.5124999999999999556, 0.5166666666666667185, 0.5208333333333333703, 0.5250000000000000222, 0.5291666666666666741, 0.5333333333333333259, 0.5374999999999999778, 0.5416666666666666297, 0.5458333333333332815, 0.5500000000000000444, 0.5541666666666666963, 0.5583333333333333481, 0.5625000000000000000, 0.5666666666666666519, 0.5708333333333333037, 0.5749999999999999556, 0.5791666666666667185, 0.5833333333333333703, 0.5875000000000000222, 0.5916666666666666741, 0.5958333333333333259, 0.5999999999999999778, 0.6041666666666666297, 0.6083333333333332815, 0.6125000000000000444, 0.6166666666666666963, 0.6208333333333333481, 0.6250000000000000000, 0.6291666666666666519, 0.6333333333333333037, 0.6374999999999999556, 0.6416666666666667185, 0.6458333333333333703, 0.6500000000000000222, 0.6541666666666666741, 0.6583333333333333259, 0.6624999999999999778, 0.6666666666666666297, 0.6708333333333332815, 0.6750000000000000444, 0.6791666666666666963, 0.6833333333333333481, 0.6875000000000000000, 0.6916666666666666519, 0.6958333333333333037, 0.6999999999999999556, 0.7041666666666667185, 0.7083333333333333703, 0.7125000000000000222, 0.7166666666666666741, 0.7208333333333333259, 0.7249999999999999778, 0.7291666666666666297, 0.7333333333333332815, 0.7375000000000000444, 0.7416666666666666963, 0.7458333333333333481, 0.7500000000000000000, 0.7541666666666666519, 0.7583333333333333037, 0.7624999999999999556, 0.7666666666666667185, 0.7708333333333333703, 0.7750000000000000222, 0.7791666666666666741, 0.7833333333333333259, 0.7874999999999999778, 0.7916666666666666297, 0.7958333333333332815, 0.8000000000000000444, 0.8041666666666666963, 0.8083333333333333481, 0.8125000000000000000, 0.8166666666666666519, 0.8208333333333333037, 0.8249999999999999556, 0.8291666666666667185, 0.8333333333333333703, 0.8375000000000000222, 0.8416666666666666741, 0.8458333333333333259, 0.8499999999999999778, 0.8541666666666666297, 0.8583333333333332815, 0.8625000000000000444, 0.8666666666666666963, 0.8708333333333333481, 0.8750000000000000000, 0.8791666666666666519, 0.8833333333333333037, 0.8874999999999999556, 0.8916666666666667185, 0.8958333333333333703, 0.9000000000000000222, 0.9041666666666666741, 0.9083333333333333259, 0.9124999999999999778, 0.9166666666666666297, 0.9208333333333332815, 0.9250000000000000444, 0.9291666666666666963, 0.9333333333333333481, 0.9375000000000000000, 0.9416666666666666519, 0.9458333333333333037, 0.9499999999999999556, 0.9541666666666667185, 0.9583333333333333703, 0.9625000000000000222, 0.9666666666666666741, 0.9708333333333333259, 0.9749999999999999778, 0.9791666666666666297, 0.9833333333333332815, 0.9875000000000000444, 0.9916666666666666963, 0.9958333333333333481, 1.000000000000000000 ),
 .UNSPECIFIED. ) 
 GEOMETRIC_REPRESENTATION_ITEM ( )  RATIONAL_B_SPLINE_SURFACE ( (
 ( 1.000000000000000000, 0.8660254037844387076, 1.000000000000000000, 0.8660254037844387076, 1.000000000000000000, 0.8660254037844387076, 1.000000000000000000, 0.8660254037844387076, 1.000000000000000000, 0.8660254037844387076, 1.000000000000000000, 0.8660254037844387076, 1.000000000000000000, 0.8660254037844387076, 1.000000000000000000, 0.8660254037844387076, 1.000000000000000000, 0.8660254037844387076, 1.000000000000000000, 0.8660254037844387076, 1.000000000000000000, 0.8660254037844387076, 1.000000000000000000, 0.8660254037844387076, 1.000000000000000000, 0.8660254037844387076, 1.000000000000000000, 0.8660254037844387076, 1.000000000000000000, 0.8660254037844387076, 1.000000000000000000, 0.8660254037844387076, 1.000000000000000000, 0.8660254037844387076, 1.000000000000000000, 0.8660254037844387076, 1.000000000000000000, 0.8660254037844387076, 1.000000000000000000, 0.8660254037844387076, 1.000000000000000000, 0.8660254037844387076, 1.000000000000000000, 0.8660254037844387076, 1.000000000000000000, 0.8660254037844387076, 1.000000000000000000, 0.8660254037844387076, 1.000000000000000000, 0.8660254037844387076, 1.000000000000000000, 0.8660254037844387076, 1.000000000000000000, 0.8660254037844387076, 1.000000000000000000, 0.8660254037844387076, 1.000000000000000000, 0.8660254037844387076, 1.000000000000000000, 0.8660254037844387076, 1.000000000000000000, 0.8660254037844387076, 1.000000000000000000, 0.8660254037844387076, 1.000000000000000000, 0.8660254037844387076, 1.000000000000000000, 0.8660254037844387076, 1.000000000000000000, 0.8660254037844387076, 1.000000000000000000, 0.8660254037844387076, 1.000000000000000000, 0.8660254037844387076, 1.000000000000000000, 0.8660254037844387076, 1.000000000000000000, 0.8660254037844387076, 1.000000000000000000, 0.8660254037844387076, 1.000000000000000000, 0.8660254037844387076, 1.000000000000000000, 0.8660254037844387076, 1.000000000000000000, 0.8660254037844387076, 1.000000000000000000, 0.8660254037844387076, 1.000000000000000000, 0.8660254037844387076, 1.000000000000000000, 0.8660254037844387076, 1.000000000000000000, 0.8660254037844387076, 1.000000000000000000, 0.8660254037844387076, 1.000000000000000000, 0.8660254037844387076, 1.000000000000000000, 0.8660254037844387076, 1.000000000000000000, 0.8660254037844387076, 1.000000000000000000, 0.8660254037844387076, 1.000000000000000000, 0.8660254037844387076, 1.000000000000000000, 0.8660254037844387076, 1.000000000000000000, 0.8660254037844387076, 1.000000000000000000, 0.8660254037844387076, 1.000000000000000000, 0.8660254037844387076, 1.000000000000000000, 0.8660254037844387076, 1.000000000000000000, 0.8660254037844387076, 1.000000000000000000, 0.8660254037844387076, 1.000000000000000000, 0.8660254037844387076, 1.000000000000000000, 0.8660254037844387076, 1.000000000000000000, 0.8660254037844387076, 1.000000000000000000, 0.8660254037844387076, 1.000000000000000000, 0.8660254037844387076, 1.000000000000000000, 0.8660254037844387076, 1.000000000000000000, 0.8660254037844387076, 1.000000000000000000, 0.8660254037844387076, 1.000000000000000000, 0.8660254037844387076, 1.000000000000000000, 0.8660254037844387076, 1.000000000000000000, 0.8660254037844387076, 1.000000000000000000, 0.8660254037844387076, 1.000000000000000000, 0.8660254037844387076, 1.000000000000000000, 0.8660254037844387076, 1.000000000000000000, 0.8660254037844387076, 1.000000000000000000, 0.8660254037844387076, 1.000000000000000000, 0.8660254037844387076, 1.000000000000000000, 0.8660254037844387076, 1.000000000000000000, 0.8660254037844387076, 1.000000000000000000, 0.8660254037844387076, 1.000000000000000000, 0.8660254037844387076, 1.000000000000000000, 0.8660254037844387076, 1.000000000000000000, 0.8660254037844387076, 1.000000000000000000, 0.8660254037844387076, 1.000000000000000000, 0.8660254037844387076, 1.000000000000000000, 0.8660254037844387076, 1.000000000000000000, 0.8660254037844387076, 1.000000000000000000, 0.8660254037844387076, 1.000000000000000000, 0.8660254037844387076, 1.000000000000000000, 0.8660254037844387076, 1.000000000000000000, 0.8660254037844387076, 1.000000000000000000, 0.8660254037844387076, 1.000000000000000000, 0.8660254037844387076, 1.000000000000000000, 0.8660254037844387076, 1.000000000000000000, 0.8660254037844387076, 1.000000000000000000, 0.8660254037844387076, 1.000000000000000000, 0.8660254037844387076, 1.000000000000000000, 0.8660254037844387076, 1.000000000000000000, 0.8660254037844387076, 1.000000000000000000, 0.8660254037844387076, 1.000000000000000000, 0.8660254037844387076, 1.000000000000000000, 0.8660254037844387076, 1.000000000000000000, 0.8660254037844387076, 1.000000000000000000, 0.8660254037844387076, 1.000000000000000000, 0.8660254037844387076, 1.000000000000000000, 0.8660254037844387076, 1.000000000000000000, 0.8660254037844387076, 1.000000000000000000, 0.8660254037844387076, 1.000000000000000000, 0.8660254037844387076, 1.000000000000000000, 0.8660254037844387076, 1.000000000000000000, 0.8660254037844387076, 1.000000000000000000, 0.8660254037844387076, 1.000000000000000000, 0.8660254037844387076, 1.000000000000000000, 0.8660254037844387076, 1.000000000000000000, 0.8660254037844387076, 1.000000000000000000, 0.8660254037844387076, 1.000000000000000000, 0.8660254037844387076, 1.000000000000000000, 0.8660254037844387076, 1.000000000000000000, 0.8660254037844387076, 1.000000000000000000, 0.8660254037844387076, 1.000000000000000000, 0.8660254037844387076, 1.000000000000000000, 0.8660254037844387076, 1.000000000000000000, 0.8660254037844387076, 1.000000000000000000, 0.8660254037844387076, 1.000000000000000000, 0.8660254037844387076, 1.000000000000000000, 0.8660254037844387076, 1.000000000000000000, 0.8660254037844387076, 1.000000000000000000, 0.8660254037844387076, 1.000000000000000000, 0.8660254037844387076, 1.000000000000000000, 0.8660254037844387076, 1.000000000000000000, 0.8660254037844387076, 1.000000000000000000, 0.8660254037844387076, 1.000000000000000000, 0.8660254037844387076, 1.000000000000000000, 0.8660254037844387076, 1.000000000000000000, 0.8660254037844387076, 1.000000000000000000, 0.8660254037844387076, 1.000000000000000000, 0.8660254037844387076, 1.000000000000000000, 0.8660254037844387076, 1.000000000000000000, 0.8660254037844387076, 1.000000000000000000, 0.8660254037844387076, 1.000000000000000000, 0.8660254037844387076, 1.000000000000000000, 0.8660254037844387076, 1.000000000000000000, 0.8660254037844387076, 1.000000000000000000, 0.8660254037844387076, 1.000000000000000000, 0.8660254037844387076, 1.000000000000000000, 0.8660254037844387076, 1.000000000000000000, 0.8660254037844387076, 1.000000000000000000, 0.8660254037844387076, 1.000000000000000000, 0.8660254037844387076, 1.000000000000000000, 0.8660254037844387076, 1.000000000000000000, 0.8660254037844387076, 1.000000000000000000, 0.8660254037844387076, 1.000000000000000000, 0.8660254037844387076, 1.000000000000000000, 0.8660254037844387076, 1.000000000000000000, 0.8660254037844387076, 1.000000000000000000, 0.8660254037844387076, 1.000000000000000000, 0.8660254037844387076, 1.000000000000000000, 0.8660254037844387076, 1.000000000000000000, 0.8660254037844387076, 1.000000000000000000, 0.8660254037844387076, 1.000000000000000000, 0.8660254037844387076, 1.000000000000000000, 0.8660254037844387076, 1.000000000000000000, 0.8660254037844387076, 1.000000000000000000, 0.8660254037844387076, 1.000000000000000000, 0.8660254037844387076, 1.000000000000000000, 0.8660254037844387076, 1.000000000000000000, 0.8660254037844387076, 1.000000000000000000, 0.8660254037844387076, 1.000000000000000000, 0.8660254037844387076, 1.000000000000000000, 0.8660254037844387076, 1.000000000000000000, 0.8660254037844387076, 1.000000000000000000, 0.8660254037844387076, 1.000000000000000000, 0.8660254037844387076, 1.000000000000000000, 0.8660254037844387076, 1.000000000000000000, 0.8660254037844387076, 1.000000000000000000, 0.8660254037844387076, 1.000000000000000000, 0.8660254037844387076, 1.000000000000000000, 0.8660254037844387076, 1.000000000000000000, 0.8660254037844387076, 1.000000000000000000, 0.8660254037844387076, 1.000000000000000000, 0.8660254037844387076, 1.000000000000000000, 0.8660254037844387076, 1.000000000000000000, 0.8660254037844387076, 1.000000000000000000, 0.8660254037844387076, 1.000000000000000000, 0.8660254037844387076, 1.000000000000000000, 0.8660254037844387076, 1.000000000000000000, 0.8660254037844387076, 1.000000000000000000, 0.8660254037844387076, 1.000000000000000000, 0.8660254037844387076, 1.000000000000000000, 0.8660254037844387076, 1.000000000000000000, 0.8660254037844387076, 1.000000000000000000, 0.8660254037844387076, 1.000000000000000000, 0.8660254037844387076, 1.000000000000000000, 0.8660254037844387076, 1.000000000000000000, 0.8660254037844387076, 1.000000000000000000, 0.8660254037844387076, 1.000000000000000000, 0.8660254037844387076, 1.000000000000000000, 0.8660254037844387076, 1.000000000000000000, 0.8660254037844387076, 1.000000000000000000, 0.8660254037844387076, 1.000000000000000000, 0.8660254037844387076, 1.000000000000000000, 0.8660254037844387076, 1.000000000000000000, 0.8660254037844387076, 1.000000000000000000, 0.8660254037844387076, 1.000000000000000000, 0.8660254037844387076, 1.000000000000000000, 0.8660254037844387076, 1.000000000000000000, 0.8660254037844387076, 1.000000000000000000, 0.8660254037844387076, 1.000000000000000000, 0.8660254037844387076, 1.000000000000000000, 0.8660254037844387076, 1.000000000000000000, 0.8660254037844387076, 1.000000000000000000, 0.8660254037844387076, 1.000000000000000000, 0.8660254037844387076, 1.000000000000000000, 0.8660254037844387076, 1.000000000000000000, 0.8660254037844387076, 1.000000000000000000, 0.8660254037844387076, 1.000000000000000000, 0.8660254037844387076, 1.000000000000000000, 0.8660254037844387076, 1.000000000000000000, 0.8660254037844387076, 1.000000000000000000, 0.8660254037844387076, 1.000000000000000000, 0.8660254037844387076, 1.000000000000000000, 0.8660254037844387076, 1.000000000000000000, 0.8660254037844387076, 1.000000000000000000, 0.8660254037844387076, 1.000000000000000000, 0.8660254037844387076, 1.000000000000000000, 0.8660254037844387076, 1.000000000000000000, 0.8660254037844387076, 1.000000000000000000, 0.8660254037844387076, 1.000000000000000000, 0.8660254037844387076, 1.000000000000000000, 0.8660254037844387076, 1.000000000000000000, 0.8660254037844387076, 1.000000000000000000, 0.8660254037844387076, 1.000000000000000000, 0.8660254037844387076, 1.000000000000000000, 0.8660254037844387076, 1.000000000000000000, 0.8660254037844387076, 1.000000000000000000, 0.8660254037844387076, 1.000000000000000000, 0.8660254037844387076, 1.000000000000000000, 0.8660254037844387076, 1.000000000000000000, 0.8660254037844387076, 1.000000000000000000, 0.8660254037844387076, 1.000000000000000000),
 ( 1.000000000000000000, 0.8660254037844387076, 1.000000000000000000, 0.8660254037844387076, 1.000000000000000000, 0.8660254037844387076, 1.000000000000000000, 0.8660254037844387076, 1.000000000000000000, 0.8660254037844387076, 1.000000000000000000, 0.8660254037844387076, 1.000000000000000000, 0.8660254037844387076, 1.000000000000000000, 0.8660254037844387076, 1.000000000000000000, 0.8660254037844387076, 1.000000000000000000, 0.8660254037844387076, 1.000000000000000000, 0.8660254037844387076, 1.000000000000000000, 0.8660254037844387076, 1.000000000000000000, 0.8660254037844387076, 1.000000000000000000, 0.8660254037844387076, 1.000000000000000000, 0.8660254037844387076, 1.000000000000000000, 0.8660254037844387076, 1.000000000000000000, 0.8660254037844387076, 1.000000000000000000, 0.8660254037844387076, 1.000000000000000000, 0.8660254037844387076, 1.000000000000000000, 0.8660254037844387076, 1.000000000000000000, 0.8660254037844387076, 1.000000000000000000, 0.8660254037844387076, 1.000000000000000000, 0.8660254037844387076, 1.000000000000000000, 0.8660254037844387076, 1.000000000000000000, 0.8660254037844387076, 1.000000000000000000, 0.8660254037844387076, 1.000000000000000000, 0.8660254037844387076, 1.000000000000000000, 0.8660254037844387076, 1.000000000000000000, 0.8660254037844387076, 1.000000000000000000, 0.8660254037844387076, 1.000000000000000000, 0.8660254037844387076, 1.000000000000000000, 0.8660254037844387076, 1.000000000000000000, 0.8660254037844387076, 1.000000000000000000, 0.8660254037844387076, 1.000000000000000000, 0.8660254037844387076, 1.000000000000000000, 0.8660254037844387076, 1.000000000000000000, 0.8660254037844387076, 1.000000000000000000, 0.8660254037844387076, 1.000000000000000000, 0.8660254037844387076, 1.000000000000000000, 0.8660254037844387076, 1.000000000000000000, 0.8660254037844387076, 1.000000000000000000, 0.8660254037844387076, 1.000000000000000000, 0.8660254037844387076, 1.000000000000000000, 0.8660254037844387076, 1.000000000000000000, 0.8660254037844387076, 1.000000000000000000, 0.8660254037844387076, 1.000000000000000000, 0.8660254037844387076, 1.000000000000000000, 0.8660254037844387076, 1.000000000000000000, 0.8660254037844387076, 1.000000000000000000, 0.8660254037844387076, 1.000000000000000000, 0.8660254037844387076, 1.000000000000000000, 0.8660254037844387076, 1.000000000000000000, 0.8660254037844387076, 1.000000000000000000, 0.8660254037844387076, 1.000000000000000000, 0.8660254037844387076, 1.000000000000000000, 0.8660254037844387076, 1.000000000000000000, 0.8660254037844387076, 1.000000000000000000, 0.8660254037844387076, 1.000000000000000000, 0.8660254037844387076, 1.000000000000000000, 0.8660254037844387076, 1.000000000000000000, 0.8660254037844387076, 1.000000000000000000, 0.8660254037844387076, 1.000000000000000000, 0.8660254037844387076, 1.000000000000000000, 0.8660254037844387076, 1.000000000000000000, 0.8660254037844387076, 1.000000000000000000, 0.8660254037844387076, 1.000000000000000000, 0.8660254037844387076, 1.000000000000000000, 0.8660254037844387076, 1.000000000000000000, 0.8660254037844387076, 1.000000000000000000, 0.8660254037844387076, 1.000000000000000000, 0.8660254037844387076, 1.000000000000000000, 0.8660254037844387076, 1.000000000000000000, 0.8660254037844387076, 1.000000000000000000, 0.8660254037844387076, 1.000000000000000000, 0.8660254037844387076, 1.000000000000000000, 0.8660254037844387076, 1.000000000000000000, 0.8660254037844387076, 1.000000000000000000, 0.8660254037844387076, 1.000000000000000000, 0.8660254037844387076, 1.000000000000000000, 0.8660254037844387076, 1.000000000000000000, 0.8660254037844387076, 1.000000000000000000, 0.8660254037844387076, 1.000000000000000000, 0.8660254037844387076, 1.000000000000000000, 0.8660254037844387076, 1.000000000000000000, 0.8660254037844387076, 1.000000000000000000, 0.8660254037844387076, 1.000000000000000000, 0.8660254037844387076, 1.000000000000000000, 0.8660254037844387076, 1.000000000000000000, 0.8660254037844387076, 1.000000000000000000, 0.8660254037844387076, 1.000000000000000000, 0.8660254037844387076, 1.000000000000000000, 0.8660254037844387076, 1.000000000000000000, 0.8660254037844387076, 1.000000000000000000, 0.8660254037844387076, 1.000000000000000000, 0.8660254037844387076, 1.000000000000000000, 0.8660254037844387076, 1.000000000000000000, 0.8660254037844387076, 1.000000000000000000, 0.8660254037844387076, 1.000000000000000000, 0.8660254037844387076, 1.000000000000000000, 0.8660254037844387076, 1.000000000000000000, 0.8660254037844387076, 1.000000000000000000, 0.8660254037844387076, 1.000000000000000000, 0.8660254037844387076, 1.000000000000000000, 0.8660254037844387076, 1.000000000000000000, 0.8660254037844387076, 1.000000000000000000, 0.8660254037844387076, 1.000000000000000000, 0.8660254037844387076, 1.000000000000000000, 0.8660254037844387076, 1.000000000000000000, 0.8660254037844387076, 1.000000000000000000, 0.8660254037844387076, 1.000000000000000000, 0.8660254037844387076, 1.000000000000000000, 0.8660254037844387076, 1.000000000000000000, 0.8660254037844387076, 1.000000000000000000, 0.8660254037844387076, 1.000000000000000000, 0.8660254037844387076, 1.000000000000000000, 0.8660254037844387076, 1.000000000000000000, 0.8660254037844387076, 1.000000000000000000, 0.8660254037844387076, 1.000000000000000000, 0.8660254037844387076, 1.000000000000000000, 0.8660254037844387076, 1.000000000000000000, 0.8660254037844387076, 1.000000000000000000, 0.8660254037844387076, 1.000000000000000000, 0.8660254037844387076, 1.000000000000000000, 0.8660254037844387076, 1.000000000000000000, 0.8660254037844387076, 1.000000000000000000, 0.8660254037844387076, 1.000000000000000000, 0.8660254037844387076, 1.000000000000000000, 0.8660254037844387076, 1.000000000000000000, 0.8660254037844387076, 1.000000000000000000, 0.8660254037844387076, 1.000000000000000000, 0.8660254037844387076, 1.000000000000000000, 0.8660254037844387076, 1.000000000000000000, 0.8660254037844387076, 1.000000000000000000, 0.8660254037844387076, 1.000000000000000000, 0.8660254037844387076, 1.000000000000000000, 0.8660254037844387076, 1.000000000000000000, 0.8660254037844387076, 1.000000000000000000, 0.8660254037844387076, 1.000000000000000000, 0.8660254037844387076, 1.000000000000000000, 0.8660254037844387076, 1.000000000000000000, 0.8660254037844387076, 1.000000000000000000, 0.8660254037844387076, 1.000000000000000000, 0.8660254037844387076, 1.000000000000000000, 0.8660254037844387076, 1.000000000000000000, 0.8660254037844387076, 1.000000000000000000, 0.8660254037844387076, 1.000000000000000000, 0.8660254037844387076, 1.000000000000000000, 0.8660254037844387076, 1.000000000000000000, 0.8660254037844387076, 1.000000000000000000, 0.8660254037844387076, 1.000000000000000000, 0.8660254037844387076, 1.000000000000000000, 0.8660254037844387076, 1.000000000000000000, 0.8660254037844387076, 1.000000000000000000, 0.8660254037844387076, 1.000000000000000000, 0.8660254037844387076, 1.000000000000000000, 0.8660254037844387076, 1.000000000000000000, 0.8660254037844387076, 1.000000000000000000, 0.8660254037844387076, 1.000000000000000000, 0.8660254037844387076, 1.000000000000000000, 0.8660254037844387076, 1.000000000000000000, 0.8660254037844387076, 1.000000000000000000, 0.8660254037844387076, 1.000000000000000000, 0.8660254037844387076, 1.000000000000000000, 0.8660254037844387076, 1.000000000000000000, 0.8660254037844387076, 1.000000000000000000, 0.8660254037844387076, 1.000000000000000000, 0.8660254037844387076, 1.000000000000000000, 0.8660254037844387076, 1.000000000000000000, 0.8660254037844387076, 1.000000000000000000, 0.8660254037844387076, 1.000000000000000000, 0.8660254037844387076, 1.000000000000000000, 0.8660254037844387076, 1.000000000000000000, 0.8660254037844387076, 1.000000000000000000, 0.8660254037844387076, 1.000000000000000000, 0.8660254037844387076, 1.000000000000000000, 0.8660254037844387076, 1.000000000000000000, 0.8660254037844387076, 1.000000000000000000, 0.8660254037844387076, 1.000000000000000000, 0.8660254037844387076, 1.000000000000000000, 0.8660254037844387076, 1.000000000000000000, 0.8660254037844387076, 1.000000000000000000, 0.8660254037844387076, 1.000000000000000000, 0.8660254037844387076, 1.000000000000000000, 0.8660254037844387076, 1.000000000000000000, 0.8660254037844387076, 1.000000000000000000, 0.8660254037844387076, 1.000000000000000000, 0.8660254037844387076, 1.000000000000000000, 0.8660254037844387076, 1.000000000000000000, 0.8660254037844387076, 1.000000000000000000, 0.8660254037844387076, 1.000000000000000000, 0.8660254037844387076, 1.000000000000000000, 0.8660254037844387076, 1.000000000000000000, 0.8660254037844387076, 1.000000000000000000, 0.8660254037844387076, 1.000000000000000000, 0.8660254037844387076, 1.000000000000000000, 0.8660254037844387076, 1.000000000000000000, 0.8660254037844387076, 1.000000000000000000, 0.8660254037844387076, 1.000000000000000000, 0.8660254037844387076, 1.000000000000000000, 0.8660254037844387076, 1.000000000000000000, 0.8660254037844387076, 1.000000000000000000, 0.8660254037844387076, 1.000000000000000000, 0.8660254037844387076, 1.000000000000000000, 0.8660254037844387076, 1.000000000000000000, 0.8660254037844387076, 1.000000000000000000, 0.8660254037844387076, 1.000000000000000000, 0.8660254037844387076, 1.000000000000000000, 0.8660254037844387076, 1.000000000000000000, 0.8660254037844387076, 1.000000000000000000, 0.8660254037844387076, 1.000000000000000000, 0.8660254037844387076, 1.000000000000000000, 0.8660254037844387076, 1.000000000000000000, 0.8660254037844387076, 1.000000000000000000, 0.8660254037844387076, 1.000000000000000000, 0.8660254037844387076, 1.000000000000000000, 0.8660254037844387076, 1.000000000000000000, 0.8660254037844387076, 1.000000000000000000, 0.8660254037844387076, 1.000000000000000000, 0.8660254037844387076, 1.000000000000000000, 0.8660254037844387076, 1.000000000000000000, 0.8660254037844387076, 1.000000000000000000, 0.8660254037844387076, 1.000000000000000000, 0.8660254037844387076, 1.000000000000000000, 0.8660254037844387076, 1.000000000000000000, 0.8660254037844387076, 1.000000000000000000, 0.8660254037844387076, 1.000000000000000000, 0.8660254037844387076, 1.000000000000000000, 0.8660254037844387076, 1.000000000000000000, 0.8660254037844387076, 1.000000000000000000, 0.8660254037844387076, 1.000000000000000000, 0.8660254037844387076, 1.000000000000000000, 0.8660254037844387076, 1.000000000000000000, 0.8660254037844387076, 1.000000000000000000, 0.8660254037844387076, 1.000000000000000000, 0.8660254037844387076, 1.000000000000000000, 0.8660254037844387076, 1.000000000000000000, 0.8660254037844387076, 1.000000000000000000, 0.8660254037844387076, 1.000000000000000000, 0.8660254037844387076, 1.000000000000000000, 0.8660254037844387076, 1.000000000000000000) ) ) 
 REPRESENTATION_ITEM ( '' )  SURFACE ( )  );
#185844 = CARTESIAN_POINT ( 'NONE',  ( 0.000000000000000000, -1.500000000000001332, 0.000000000000000000 ) ) ;
#185845 = CARTESIAN_POINT ( 'NONE',  ( 10.18461545817735470, 3.956598013261175772, -5.433575010662928584 ) ) ;
#185846 = B_SPLINE_CURVE_WITH_KNOTS ( 'NONE', 3,
 ( #188030, #190168, #124204, #58040 ),
 .UNSPECIFIED., .F., .F.,
 ( 4, 4 ),
 ( 0.000000000000000000, 9.170750102251527260E-05 ),
 .UNSPECIFIED. ) ;
#185847 = CARTESIAN_POINT ( 'NONE',  ( 1.911028901235469313, 1.633884665098099598, -1.483674895440662667 ) ) ;
#185848 = CARTESIAN_POINT ( 'NONE',  ( 4.200629628819559258, -0.7044727654359562719, -2.150022973637927048 ) ) ;
#185849 = CARTESIAN_POINT ( 'NONE',  ( -6.222829318992474157, 10.20379193889247382, 0.000000000000000000 ) ) ;
#185850 = CARTESIAN_POINT ( 'NONE',  ( 3.199259029290311140, 1.635763741490828593, -0.7788767334107206119 ) ) ;
#185851 = CARTESIAN_POINT ( 'NONE',  ( 4.346842662630929333, -1.713972709756344859, -0.8558225519783541069 ) ) ;
#185852 = CARTESIAN_POINT ( 'NONE',  ( 1.364683531249990311, 4.696875000341417916, 1.214306433183764966E-14 ) ) ;
#185853 = CARTESIAN_POINT ( 'NONE',  ( 4.241065053910620719, -1.715758787085974957, 0.9708604712577516560 ) ) ;
#185854 = CARTESIAN_POINT ( 'NONE',  ( 0.5164664324388609229, 1.330803901959699997, -1.393038531337851493 ) ) ;
#185855 = CARTESIAN_POINT ( 'NONE',  ( 4.996879044411707937, 1.554903924810165705, -1.039696167511289238 ) ) ;
#185856 = CARTESIAN_POINT ( 'NONE',  ( 3.668876216774307863, -1.550535085938867352, 1.709345553852769095 ) ) ;
#185857 = CARTESIAN_POINT ( 'NONE',  ( 5.389040371011321717, 0.1367655989435011543, 1.856064314752596145 ) ) ;
#185858 = CARTESIAN_POINT ( 'NONE',  ( -1.201851678989727383E-14, 5.446875000341422357, -1.575800808251660134 ) ) ;
#185859 = CARTESIAN_POINT ( 'NONE',  ( 6.902720183911293717, 15.44694763437295570, -9.761920501353824164 ) ) ;
#185861 = CARTESIAN_POINT ( 'NONE',  ( 1.647240615436126543, -1.778467030350115774, 1.127781350514756475 ) ) ;
#185860 = CARTESIAN_POINT ( 'NONE',  ( -3.104453987404957260, 6.565687385373657925, -0.7216878364870257245 ) ) ;
#185862 = CARTESIAN_POINT ( 'NONE',  ( 2.345197385039651472, 5.679888015947478941, -0.7216878364870267237 ) ) ;
#185864 = DIRECTION ( 'NONE',  ( 0.7592566023653010143, -0.6507913734559633845, -5.900213523162838665E-32 ) ) ;
#185863 = CARTESIAN_POINT ( 'NONE',  ( -1.201851678989727383E-14, 5.009375000341421469, -1.575800808251660134 ) ) ;
#185865 = CARTESIAN_POINT ( 'NONE',  ( 2.795306286867365486, -0.1602278063087131110, -2.114629986603839829 ) ) ;
#185866 = CARTESIAN_POINT ( 'NONE',  ( 0.000000000000000000, 0.000000000000000000, 0.000000000000000000 ) ) ;
#185867 = CARTESIAN_POINT ( 'NONE',  ( 1.054951293920348698, 0.3981946776167448188, 1.979963216457211850 ) ) ;
#185868 = CARTESIAN_POINT ( 'NONE',  ( 1.364683531249988757, 1.384375000341421469, 0.000000000000000000 ) ) ;
#185869 = CARTESIAN_POINT ( 'NONE',  ( -2.792616454734997866, 6.201876930592042925, 0.7216878364870317197 ) ) ;
#185870 = CARTESIAN_POINT ( 'NONE',  ( 6.010342169559767633, 5.906487374108181143, -0.7998128361456281477 ) ) ;
#185871 = CARTESIAN_POINT ( 'NONE',  ( 1.739762150092131643, -1.564342989677082629, -1.491970722459233345 ) ) ;
#185872 = CARTESIAN_POINT ( 'NONE',  ( 6.610000000000006537, 7.629137130509094256, 2.600000000000001421 ) ) ;
#185875 = CARTESIAN_POINT ( 'NONE',  ( -3.912682303000325046, 8.998411203033816363, -0.7749999999999979128 ) ) ;
#185874 = DIRECTION ( 'NONE',  ( 1.039099362110107450E-15, 1.000000000000000000, -4.583713267641621330E-32 ) ) ;
#185873 = CARTESIAN_POINT ( 'NONE',  ( 4.278479993564246797, 7.149254538203735798, 1.199719254218452047 ) ) ;
#185876 = FACE_BOUND ( 'NONE', #147958, .T. ) ;
#185877 = CARTESIAN_POINT ( 'NONE',  ( 5.665250009225348826, 1.861346387706263261, -0.7762253298396750711 ) ) ;
#185878 = CARTESIAN_POINT ( 'NONE',  ( -8.432808358020034589, 10.86136238915529084, 1.443375672974064550 ) ) ;
#185879 = AXIS2_PLACEMENT_3D ( 'NONE', #175424, #27009, #93116 ) ;
#185880 = CARTESIAN_POINT ( 'NONE',  ( 0.01162390915069450026, -2.148011843722149372, 0.4338911918742721641 ) ) ;
#185881 = CARTESIAN_POINT ( 'NONE',  ( 4.355419904288084787, 3.138961374172543284, 0.7750000000000117906 ) ) ;
#185883 = CARTESIAN_POINT ( 'NONE',  ( -1.364683531250014514, 11.83854166700806587, -0.7879004041258335089 ) ) ;
#185882 = CARTESIAN_POINT ( 'NONE',  ( 0.9544393508495727652, 2.259765469927646375, -0.1136819296270324686 ) ) ;
#185884 = CARTESIAN_POINT ( 'NONE',  ( -9.332089804907933939, 9.781859615347734405, 1.040834085586084257E-14 ) ) ;
#185885 = EDGE_CURVE ( 'NONE', #89432, #40908, #74022, .T. ) ;
#185886 = CARTESIAN_POINT ( 'NONE',  ( -4.351804119862249465, 7.060559992272473551, 1.082531754730560403 ) ) ;
#185887 = CARTESIAN_POINT ( 'NONE',  ( 1.364683531249988535, 1.676041667008085101, 0.7879004041258500513 ) ) ;
#185888 = CARTESIAN_POINT ( 'NONE',  ( 5.717785742877098620, 7.006476535625818514, 2.500000000000000444 ) ) ;
#185889 = CARTESIAN_POINT ( 'NONE',  ( 1.500000000000001332, 10.12500000000000178, 0.000000000000000000 ) ) ;
#185890 = CARTESIAN_POINT ( 'NONE',  ( 4.195721234439112379, -0.6572638427989171417, 1.594953032058670894 ) ) ;
#185891 = CARTESIAN_POINT ( 'NONE',  ( 6.229045230835819069, 6.231917288922055320, -0.7998128361456481317 ) ) ;
#185892 = CARTESIAN_POINT ( 'NONE',  ( 1.844620604044054035, -1.498293487275937697, 0.9415191625909284934 ) ) ;
#185893 = CARTESIAN_POINT ( 'NONE',  ( 4.981566806912656631, 2.060606067865732527, -0.7902562557115796471 ) ) ;
#185894 = ORIENTED_EDGE ( 'NONE', *, *, #72042, .F. ) ;
#185895 = CARTESIAN_POINT ( 'NONE',  ( 3.849871613625083899, -1.395920841890609498, -1.459997210279185831 ) ) ;
#185896 = CARTESIAN_POINT ( 'NONE',  ( -5.427006627220116286, 9.553534508390610469, -0.7998128361456362523 ) ) ;
#185898 = CARTESIAN_POINT ( 'NONE',  ( 3.585564690064909854, -0.5826378547920657569, 1.930424337232887977 ) ) ;
#185897 = CARTESIAN_POINT ( 'NONE',  ( 4.863993733624056404, 0.6645719631460760279, -2.013739200842738608 ) ) ;
#185900 = ORIENTED_EDGE ( 'NONE', *, *, #44124, .T. ) ;
#185899 = CARTESIAN_POINT ( 'NONE',  ( 4.183730900115702589, 1.755568954123175596, -0.4464138967742969366 ) ) ;
#185901 = ORIENTED_EDGE ( 'NONE', *, *, #152381, .T. ) ;
#185902 = CARTESIAN_POINT ( 'NONE',  ( 1.182252951876180180, -1.824241171369020531, -0.4133900166373091767 ) ) ;
#185903 = CARTESIAN_POINT ( 'NONE',  ( -11.97929049433705373, 11.37999999999999901, -0.7046979865771834106 ) ) ;
#185904 = CARTESIAN_POINT ( 'NONE',  ( 6.533875575962896143, -1.755123972569608615, 0.4478894030855648523 ) ) ;
#185905 = LINE ( 'NONE', #119930, #74357 ) ;
#185906 = CIRCLE ( 'NONE', #92573, 5.799999999999999822 ) ;
#185907 = CARTESIAN_POINT ( 'NONE',  ( -10.40894566972866286, 4.029202461753065734, -7.241727701387177696 ) ) ;
#185908 = CARTESIAN_POINT ( 'NONE',  ( 4.489158259456265121, 7.291082831790689056, -1.082531754730548412 ) ) ;
#185909 = CARTESIAN_POINT ( 'NONE',  ( -1.201851678989727383E-14, 3.384375000341421469, 1.575800808251672791 ) ) ;
#185910 = CARTESIAN_POINT ( 'NONE',  ( 0.1231139863388103495, 1.664874722635242277, 0.9407772870168448209 ) ) ;
#185911 = EDGE_LOOP ( 'NONE', ( #76204, #178113, #123076, #85615 ) ) ;
#185912 = CARTESIAN_POINT ( 'NONE',  ( 6.563555762791525972, 6.830105609444471426, -0.7216878364870458196 ) ) ;
#185913 = CARTESIAN_POINT ( 'NONE',  ( 2.014041202081144011, 1.956828179156915315, -0.1411808619533050091 ) ) ;
#185914 = CARTESIAN_POINT ( 'NONE',  ( -3.689227196694346400, 6.357829925235092716, -1.082531754730546636 ) ) ;
#185915 = CARTESIAN_POINT ( 'NONE',  ( -6.608673532018475960, 6.674816973635147477, -0.7998128361456362523 ) ) ;
#185916 = CARTESIAN_POINT ( 'NONE',  ( 3.726904977748810577, 1.497142547446396410, -1.502090761940577002 ) ) ;
#185917 = CARTESIAN_POINT ( 'NONE',  ( 10.42352117080803708, 11.05519620889787724, -0.7998128361456281477 ) ) ;
#185918 = CARTESIAN_POINT ( 'NONE',  ( 5.044191579798307679, 1.965876612296811654, 0.1480472272742116568 ) ) ;
#185919 = CARTESIAN_POINT ( 'NONE',  ( -1.364683531250012516, 1.280208333674755172, 0.7879004041258379498 ) ) ;
#185920 = CARTESIAN_POINT ( 'NONE',  ( 0.8264323289940983530, -0.9090603351678091526, -1.796376205119714298 ) ) ;
#185921 = ORIENTED_EDGE ( 'NONE', *, *, #85262, .F. ) ;
#185922 = CARTESIAN_POINT ( 'NONE',  ( 1.388444276177196235, -0.7657061372807508759, -1.974083799386998406 ) ) ;
#185923 = CARTESIAN_POINT ( 'NONE',  ( 11.69944783379995812, 7.009427230352428317, -2.678979863565422725 ) ) ;
#185924 = CARTESIAN_POINT ( 'NONE',  ( 2.277862540309500083, -2.008769142935047380, 0.5008063122204224893 ) ) ;
#185925 = CARTESIAN_POINT ( 'NONE',  ( 3.230585741806197841, 6.991043475407723307, 0.7998128361456271485 ) ) ;
#185926 = CARTESIAN_POINT ( 'NONE',  ( 4.688087255275310561, 8.691461907788344377, -0.7998128361456381397 ) ) ;
#185927 = VERTEX_POINT ( 'NONE', #196355 ) ;
#185929 = CARTESIAN_POINT ( 'NONE',  ( 4.320244504248938355, 8.192035688265757898, 1.040834085586084257E-14 ) ) ;
#185928 = CARTESIAN_POINT ( 'NONE',  ( 5.173812367756161379, -1.161941297927127525, 1.737786252440294055 ) ) ;
#185932 = ORIENTED_EDGE ( 'NONE', *, *, #19034, .T. ) ;
#185931 = CARTESIAN_POINT ( 'NONE',  ( 1.752323211514599688, 1.791785093909546323, 0.2653131528348381396 ) ) ;
#185930 = CARTESIAN_POINT ( 'NONE',  ( 3.328933297416610593, 0.04358344136132231289, 1.825221112333124340 ) ) ;
#185933 = CARTESIAN_POINT ( 'NONE',  ( 6.305322857734435793, 1.832379230283949667, 1.229636283518860118 ) ) ;
#185934 = DIRECTION ( 'NONE',  ( -1.000000000000000000, -3.451266460341927087E-31, 0.000000000000000000 ) ) ;
#185935 = CARTESIAN_POINT ( 'NONE',  ( 10.75721414819643584, 8.375941707272300363, -4.789107451334092325 ) ) ;
#185936 = CARTESIAN_POINT ( 'NONE',  ( 5.596761079150560647, -0.5311557606857522096, -2.141783596114990917 ) ) ;
#185937 = CARTESIAN_POINT ( 'NONE',  ( 7.796102023057898123, 9.054206100777749455, -1.199719254218441611 ) ) ;
#185938 = CARTESIAN_POINT ( 'NONE',  ( -0.6823417656250003738, 9.463541667008065872, 1.181850606188754593 ) ) ;
#185939 = VERTEX_POINT ( 'NONE', #66313 ) ;
#185940 = CARTESIAN_POINT ( 'NONE',  ( 3.984940423737866055, -1.785409543757199291, -0.6854135386504257577 ) ) ;
#185941 = B_SPLINE_CURVE_WITH_KNOTS ( 'NONE', 3,
 ( #57185, #187172, #108135, #91845, #25734, #173083, #158953, #9496, #39875, #92907, #122277, #24664, #75568, #207690, #59309, #38800 ),
 .UNSPECIFIED., .F., .F.,
 ( 4, 3, 3, 3, 3, 4 ),
 ( 5.421010862428817358E-20, 2.208392919728564190E-05, 5.593630375490294554E-05, 8.978950068604114713E-05, 0.0001236430975991122182, 0.0001574962648025070408 ),
 .UNSPECIFIED. ) ;
#185943 = CARTESIAN_POINT ( 'NONE',  ( -3.972702704004144714, 4.593573561881607148, 1.199719254218462483 ) ) ;
#185942 = CIRCLE ( 'NONE', #165236, 11.09999999999999964 ) ;
#185944 = CARTESIAN_POINT ( 'NONE',  ( 8.796542737168120851, 9.157054702984622097, -0.7998128361456211532 ) ) ;
#185945 = CARTESIAN_POINT ( 'NONE',  ( 6.268043187460373922, -2.055199631210804068, 0.2494731385529954104 ) ) ;
#185946 = CARTESIAN_POINT ( 'NONE',  ( -9.340724465469280702, 15.44694763438213947, 7.462818192253868332 ) ) ;
#185947 = CARTESIAN_POINT ( 'NONE',  ( 6.075747529084263299, -1.173811750163206158, 1.850510016281024850 ) ) ;
#185948 = CARTESIAN_POINT ( 'NONE',  ( 5.862225131719664972, 7.287605523280396902, -1.268052015211480033 ) ) ;
#185949 = CARTESIAN_POINT ( 'NONE',  ( -3.101822900477640754, 15.47022932557438324, -11.60075578494621595 ) ) ;
#185950 = ORIENTED_EDGE ( 'NONE', *, *, #169514, .T. ) ;
#185951 = ORIENTED_EDGE ( 'NONE', *, *, #91258, .F. ) ;
#185952 = CIRCLE ( 'NONE', #26868, 0.08000000000000012657 ) ;
#185953 = CARTESIAN_POINT ( 'NONE',  ( 5.606900530694575835, 7.430539361494464146, 1.295638170384592947 ) ) ;
#185954 = EDGE_CURVE ( 'NONE', #103946, #57811, #84514, .T. ) ;
#185955 = CARTESIAN_POINT ( 'NONE',  ( 3.444469828353762697, 0.4513171681363346011, 1.815172769691273613 ) ) ;
#185956 = CARTESIAN_POINT ( 'NONE',  ( -0.02319159430949970652, 2.891346550825596218, -2.299931007135449512 ) ) ;
#185957 = CARTESIAN_POINT ( 'NONE',  ( 10.59765138761703085, 9.799999999999982947, 3.303242380465396533 ) ) ;
#185958 = CARTESIAN_POINT ( 'NONE',  ( -9.002250809794013264, 9.604973487622245898, -0.7216878364870267237 ) ) ;
#185959 = CARTESIAN_POINT ( 'NONE',  ( 5.083381250481017410, 4.895309311841474553, 0.7998128361456352531 ) ) ;
#185960 = CARTESIAN_POINT ( 'NONE',  ( 6.543811353064236336, 1.423268159695538326, 1.503672778047180358 ) ) ;
#185961 = CARTESIAN_POINT ( 'NONE',  ( 0.7027501817156033281, 1.864177386631181044, 0.7691025790682111118 ) ) ;
#185962 = CARTESIAN_POINT ( 'NONE',  ( -9.378489572351046633, 11.96465713920816043, -1.599625672291263179 ) ) ;
#185963 = CARTESIAN_POINT ( 'NONE',  ( 7.178115983792402233, 7.339166500704784823, 0.7998128361456281477 ) ) ;
#185964 = CARTESIAN_POINT ( 'NONE',  ( -9.336326716892640931, 8.920000000000001705, -2.500000000000000444 ) ) ;
#185965 = CARTESIAN_POINT ( 'NONE',  ( 1.078377591563362436, -2.138745004354754897, -0.4770250503970187572 ) ) ;
#185966 = CARTESIAN_POINT ( 'NONE',  ( 5.988856447087388624, -0.2726756491404982441, -1.805090154579996442 ) ) ;
#185967 = CARTESIAN_POINT ( 'NONE',  ( -2.839543107058306592, 5.400218493954923815, -1.199719254218446718 ) ) ;
#185968 = CARTESIAN_POINT ( 'NONE',  ( 3.445180431648313224, 7.033477913649446300, 0.7216878364870257245 ) ) ;
#185969 = CARTESIAN_POINT ( 'NONE',  ( 10.08456733046637765, 10.65975006183261087, 0.000000000000000000 ) ) ;
#185970 = CARTESIAN_POINT ( 'NONE',  ( 3.083589872104280705, 5.684939719841914929, 1.199719254218450271 ) ) ;
#185971 = CARTESIAN_POINT ( 'NONE',  ( 3.984117037569365305, 5.741498858621315371, 1.599625672291261402 ) ) ;
#185972 = VERTEX_POINT ( 'NONE', #197403 ) ;
#185974 = CARTESIAN_POINT ( 'NONE',  ( 1.190090860395363492, 1.200783890555771283, 1.615600688039710020 ) ) ;
#185973 = CARTESIAN_POINT ( 'NONE',  ( 4.212339636135824961, 1.685202893791247769, 0.7422218904534692019 ) ) ;
#185975 = CARTESIAN_POINT ( 'NONE',  ( 2.056460162951703197, 1.999754300726686029, -1.132793482217157033 ) ) ;
#185977 = CARTESIAN_POINT ( 'NONE',  ( 6.139501739389007007, 1.813922436357641388, -0.7475906808915923074 ) ) ;
#185976 = CARTESIAN_POINT ( 'NONE',  ( 3.795919822146273326, 5.451659097302528068, -1.443375672974051449 ) ) ;
#185978 = CARTESIAN_POINT ( 'NONE',  ( 1.642778471875001811, -3.492708332855375630, 2.845375778867859751 ) ) ;
#185979 = CARTESIAN_POINT ( 'NONE',  ( -5.576481253922474401, 5.400316305864651056, -0.7998128361456221525 ) ) ;
#185980 = CARTESIAN_POINT ( 'NONE',  ( 4.201352949932454450, 1.705870964349815333, -0.8646410313453978258 ) ) ;
#185981 = CARTESIAN_POINT ( 'NONE',  ( -8.136864746495904299, 12.64475930422059768, -0.7998128361456281477 ) ) ;
#185982 = CARTESIAN_POINT ( 'NONE',  ( 6.453003701063230402, 6.772902045581084884, 0.3391303328579304277 ) ) ;
#185983 = CARTESIAN_POINT ( 'NONE',  ( -5.171509248969888617, 4.998125310078441075, 0.7998128361456281477 ) ) ;
#185985 = CARTESIAN_POINT ( 'NONE',  ( 2.588565208901713266, -0.3177388942022137397, -1.843305967786903032 ) ) ;
#185984 = CARTESIAN_POINT ( 'NONE',  ( 3.175413592762990067, 1.328342846777453845, 1.614508523670985740 ) ) ;
#185986 = CARTESIAN_POINT ( 'NONE',  ( 9.259855728453651125, 9.905512559391842942, 1.040834085586084257E-14 ) ) ;
#185987 = CARTESIAN_POINT ( 'NONE',  ( -1.364683531249997417, 5.571875000341417916, 1.214306433183764966E-14 ) ) ;
#185988 = CARTESIAN_POINT ( 'NONE',  ( 2.999246388560794951, -1.738348057599903074, 0.08809733484680536131 ) ) ;
#185989 = CARTESIAN_POINT ( 'NONE',  ( 4.822949958159288286, 6.649860922651058992, -1.599625672291256295 ) ) ;
#185991 = DIRECTION ( 'NONE',  ( 0.000000000000000000, 0.000000000000000000, -1.000000000000000000 ) ) ;
#185990 = LINE ( 'NONE', #201163, #134465 ) ;
#185992 = CARTESIAN_POINT ( 'NONE',  ( 4.266008093515370803, 0.8158808812368329999, 1.519711535667643609 ) ) ;
#185993 = CARTESIAN_POINT ( 'NONE',  ( 4.089532599075940134, -0.8378280566024614018, 2.025282237563410526 ) ) ;
#185994 = CARTESIAN_POINT ( 'NONE',  ( 6.533804136697315634, -1.437950210024591780, -1.674183229976949905 ) ) ;
#185995 = CARTESIAN_POINT ( 'NONE',  ( -10.44369633504468631, 5.112959841837462882, -5.232137017608346596 ) ) ;
#185996 = CARTESIAN_POINT ( 'NONE',  ( 3.854478708947015164, -2.168323188329326801, -0.1120144502513506779 ) ) ;
#185997 = CARTESIAN_POINT ( 'NONE',  ( 1.717148762710469789, -0.2249250470785572054, 1.811706739299999924 ) ) ;
#185998 = CARTESIAN_POINT ( 'NONE',  ( -15.75000000000000000, 10.89999999999998259, 1.399999999999998579 ) ) ;
#185999 = CARTESIAN_POINT ( 'NONE',  ( 4.469977352714805008, -0.9950975051371075963, 1.868896417504315677 ) ) ;
#186000 = EDGE_CURVE ( 'NONE', #178739, #175679, #193400, .T. ) ;
#186001 = ORIENTED_EDGE ( 'NONE', *, *, #65459, .T. ) ;
#186003 = CARTESIAN_POINT ( 'NONE',  ( -1.364683531250000748, 2.321875000341422357, 1.214306433183764966E-14 ) ) ;
#186002 = CARTESIAN_POINT ( 'NONE',  ( 4.511445251964079084, -2.248337965441957742, 0.4463705457610280258 ) ) ;
#186004 = CARTESIAN_POINT ( 'NONE',  ( 6.620655732516647518, 7.053381450551401421, 2.424417106520880161 ) ) ;
#186005 = CARTESIAN_POINT ( 'NONE',  ( 3.891353782322113375, 4.498666486585943147, -1.199719254218446718 ) ) ;
#186006 = CARTESIAN_POINT ( 'NONE',  ( 0.7332529803791461021, 1.960763319057107879, 0.8078710241638600298 ) ) ;
#186007 = CARTESIAN_POINT ( 'NONE',  ( -4.772106882330234612, 6.590544000850479200, -1.443375672974053447 ) ) ;
#186008 = FACE_OUTER_BOUND ( 'NONE', #95555, .T. ) ;
#186009 = CARTESIAN_POINT ( 'NONE',  ( -4.975479186090865369, 6.827811688571220117, 1.443375672974064550 ) ) ;
#186011 = CARTESIAN_POINT ( 'NONE',  ( -1.500000000000008216, 10.78125000068279249, 3.469446951953614189E-15 ) ) ;
#186010 = CARTESIAN_POINT ( 'NONE',  ( -5.983791420057156252, 7.107340751733106643, 1.079986564815892613 ) ) ;
#186012 = EDGE_LOOP ( 'NONE', ( #101300, #119926, #144871, #96233 ) ) ;
#186013 = CARTESIAN_POINT ( 'NONE',  ( 5.643203987388664800, 0.8197706014990979728, 1.842448445624145226 ) ) ;
#186015 = CARTESIAN_POINT ( 'NONE',  ( 4.944214452789121417, -0.9770834884576683477, 1.816490783314741231 ) ) ;
#186014 = CARTESIAN_POINT ( 'NONE',  ( 5.392392409933256303, 7.314210449720692786, 1.599625672291267398 ) ) ;
#186017 = CARTESIAN_POINT ( 'NONE',  ( -0.2409995289980003397, 0.7158067089181943121, -2.082568332340509087 ) ) ;
#186016 = CARTESIAN_POINT ( 'NONE',  ( 6.313256805818848960, 7.394496357324014113, 1.199719254218452047 ) ) ;
#186018 = CARTESIAN_POINT ( 'NONE',  ( 7.862802741282558294, 8.137967717776607657, 0.000000000000000000 ) ) ;
#186019 = CARTESIAN_POINT ( 'NONE',  ( -3.285556943750000514, -1.888541666188711110, -1.896917185911906500 ) ) ;
#186020 = SURFACE_SIDE_STYLE ('',( #157826 ) ) ;
#186021 = CARTESIAN_POINT ( 'NONE',  ( 0.1993191639408486426, -0.5556045495253292277, 2.015383906575985318 ) ) ;
#186022 = CARTESIAN_POINT ( 'NONE',  ( 4.834611377684539413, 0.6298767044488963185, -1.915599524792414465 ) ) ;
#186023 = CARTESIAN_POINT ( 'NONE',  ( 3.808014051635350672, 1.299385917162833692, -1.304790556973287163 ) ) ;
#186024 = EDGE_CURVE ( 'NONE', #41882, #85209, #209123, .T. ) ;
#186025 = CARTESIAN_POINT ( 'NONE',  ( 4.496500501226593727, 8.397667684739696270, 0.7998128361456462443 ) ) ;
#186026 = FILL_AREA_STYLE_COLOUR ( '', #68982 ) ;
#186027 = CARTESIAN_POINT ( 'NONE',  ( 0.2347969022384633897, -1.580228140511737100, 0.6916409326972148275 ) ) ;
#186028 = CARTESIAN_POINT ( 'NONE',  ( -2.819205876637805641, 5.376491725131008259, -1.199719254218446718 ) ) ;
#186029 =( BOUNDED_CURVE ( )  B_SPLINE_CURVE ( 2, ( #133589, #82654, #31798, #15509, #99982 ),
 .UNSPECIFIED., .F., .T. ) 
 B_SPLINE_CURVE_WITH_KNOTS ( ( 3, 2, 3 ),
 ( 0.01067668659529985575, 0.01250000000000000069, 0.01407841936770214651 ),
 .UNSPECIFIED. ) 
 CURVE ( )  GEOMETRIC_REPRESENTATION_ITEM ( )  RATIONAL_B_SPLINE_CURVE ( ( 0.9340561916853913349, 0.9413733574794107550, 1.000000000000000000, 0.9492476566127880933, 0.9369473844697258080 ) ) 
 REPRESENTATION_ITEM ( '' )  );
#186030 = CARTESIAN_POINT ( 'NONE',  ( 0.6515572338587878320, 1.139979866233470807, 1.996073129511093169 ) ) ;
#186031 = CARTESIAN_POINT ( 'NONE',  ( -6.250472511100020334, 7.250971670160158311, 1.199719254218450271 ) ) ;
#186032 = CARTESIAN_POINT ( 'NONE',  ( 6.332949636392265269, 0.2142684956521986317, 2.252356394309730003 ) ) ;
#186033 = CARTESIAN_POINT ( 'NONE',  ( 3.440152538952054861, 0.9466726917620759130, -1.881381795136138679 ) ) ;
#186034 = CARTESIAN_POINT ( 'NONE',  ( -5.255720823952942489, 6.160704378480398979, -1.199719254218453823 ) ) ;
#186035 = CARTESIAN_POINT ( 'NONE',  ( 7.100719765255169236, 9.307259030929609267, -1.599625672291262513 ) ) ;
#186036 = CARTESIAN_POINT ( 'NONE',  ( 6.251718229232841928, 8.387033582228703210, -1.443375672974078761 ) ) ;
#186037 = SURFACE_STYLE_USAGE ( .BOTH. , #201212 ) ;
#186038 = CARTESIAN_POINT ( 'NONE',  ( -5.716734326456539783, 9.821273814174633188, -0.7998128361456231517 ) ) ;
#186039 = B_SPLINE_CURVE_WITH_KNOTS ( 'NONE', 3,
 ( #109451, #124649, #92085, #127861, #192736, #110512, #160258, #77937, #42264, #30265, #29198, #59549, #210053, #58493 ),
 .UNSPECIFIED., .F., .F.,
 ( 4, 2, 2, 2, 2, 2, 4 ),
 ( 0.001478211208292421830, 0.001788443044005901591, 0.002098674879719381568, 0.002408906715432861112, 0.002719138551146341089, 0.003339602222573304080, 0.003960065894000266637 ),
 .UNSPECIFIED. ) ;
#186040 = CARTESIAN_POINT ( 'NONE',  ( 5.897433631820129918, 8.863794422890064695, -1.082531754730537976 ) ) ;
#186041 = CARTESIAN_POINT ( 'NONE',  ( 4.133273095458231516, 7.653358944556723387, 0.7702195724684970379 ) ) ;
#186042 = CARTESIAN_POINT ( 'NONE',  ( -5.447678794592645701, 5.250046769979851646, 0.000000000000000000 ) ) ;
#186044 = CARTESIAN_POINT ( 'NONE',  ( 3.551236150222897958, 0.3290391446359001715, 2.196816492004387111 ) ) ;
#186043 = CARTESIAN_POINT ( 'NONE',  ( 2.461320219219771843, -1.760565900816572826, 1.181798851529712646 ) ) ;
#186045 = CARTESIAN_POINT ( 'NONE',  ( 1.869323357045350686, 2.096458975851514861, -0.6381942758529115522 ) ) ;
#186046 = CARTESIAN_POINT ( 'NONE',  ( -5.768104287610143821, 8.816873204598778102, -1.199719254218440723 ) ) ;
#186047 = CARTESIAN_POINT ( 'NONE',  ( -3.688700311369816909, 6.461178242310183784, -1.199719254218450271 ) ) ;
#186048 = CARTESIAN_POINT ( 'NONE',  ( 5.793401095800717826, -1.774274828963496198, 0.8374297333502839225 ) ) ;
#186049 = CARTESIAN_POINT ( 'NONE',  ( -1.364683531250014514, 1.738541667008085545, -0.7879004041258289570 ) ) ;
#186050 = CARTESIAN_POINT ( 'NONE',  ( -3.472296738875691346, 6.104744391113324120, 1.082531754730549967 ) ) ;
#186051 = CARTESIAN_POINT ( 'NONE',  ( -4.284013352238250860, 7.941839977679187257, -0.7216878364870267237 ) ) ;
#186053 = CARTESIAN_POINT ( 'NONE',  ( 4.816704082729271086, -0.7169179515637627009, -1.995842421597990413 ) ) ;
#186052 = AXIS2_PLACEMENT_3D ( 'NONE', #156175, #26148, #77027 ) ;
#186054 = CARTESIAN_POINT ( 'NONE',  ( -4.930325137224961907, 5.781076077297750970, -1.199719254218453823 ) ) ;
#186055 = ORIENTED_EDGE ( 'NONE', *, *, #112616, .F. ) ;
#186057 = CARTESIAN_POINT ( 'NONE',  ( -1.500000000000022204, 7.240846818246208905, 4.154462424328226433 ) ) ;
#186056 = CARTESIAN_POINT ( 'NONE',  ( -4.800995793014949165, 8.615262501910491366, 0.7216878364870267237 ) ) ;
#186058 = CARTESIAN_POINT ( 'NONE',  ( 5.686755365928134687, 8.721966129303114101, 1.199719254218462483 ) ) ;
#186059 = CARTESIAN_POINT ( 'NONE',  ( 5.618664544990171095, -0.03892770779775727580, 1.841008343696965310 ) ) ;
#186060 = DIRECTION ( 'NONE',  ( 0.000000000000000000, 0.000000000000000000, 1.000000000000000000 ) ) ;
#186061 = CARTESIAN_POINT ( 'NONE',  ( 0.6823417656249882723, 2.738541667008084879, -1.181850606188749264 ) ) ;
#186062 = CARTESIAN_POINT ( 'NONE',  ( 0.9600616587607477825, -1.572830678042375974, -0.7454570610717390355 ) ) ;
#186063 = CARTESIAN_POINT ( 'NONE',  ( 11.35569630219391968, 12.48731560708632138, 3.554478010595061743 ) ) ;
#186064 = CARTESIAN_POINT ( 'NONE',  ( 0.000000000000000000, 4.999999999999997335, 0.000000000000000000 ) ) ;
#186065 = CARTESIAN_POINT ( 'NONE',  ( 9.452230854652610148, 11.00900109668812377, -7.398976902094164032 ) ) ;
#186066 = CARTESIAN_POINT ( 'NONE',  ( 4.909125497034264818, 1.879091090907711425, 1.068517025386829467 ) ) ;
#186067 = CARTESIAN_POINT ( 'NONE',  ( -4.517891501851816649, 6.293959390292322986, -1.599625672291256295 ) ) ;
#186068 = CARTESIAN_POINT ( 'NONE',  ( -6.846504384776755714, 9.971043634672792422, -1.082531754730537088 ) ) ;
#186070 = AXIS2_PLACEMENT_3D ( 'NONE', #104469, #39454, #154282 ) ;
#186069 = CIRCLE ( 'NONE', #172338, 0.07999999999999946043 ) ;
#186071 = CARTESIAN_POINT ( 'NONE',  ( 5.049776242366147194, 0.6816224847111511664, -2.051488706027407183 ) ) ;
#186072 = CARTESIAN_POINT ( 'NONE',  ( 5.307875201598577064, -1.962095876955988638, 0.1906144227653387424 ) ) ;
#186073 = CARTESIAN_POINT ( 'NONE',  ( 4.094866968876837987, 0.9280426781237434142, -1.464329598137555477 ) ) ;
#186074 = ADVANCED_FACE ( 'NONE', ( #128246 ), #64223, .F. ) ;
#186075 = CARTESIAN_POINT ( 'NONE',  ( 0.7147126110796617748, 2.027027023440019171, 0.8336157706642086662 ) ) ;
#186076 = CARTESIAN_POINT ( 'NONE',  ( 1.817812757297363691, -0.2812075768990837665, 2.290339019377229945 ) ) ;
#186077 = CARTESIAN_POINT ( 'NONE',  ( 3.655589845848466801, 0.5043569952981543647, -1.997962123967106374 ) ) ;
#186078 = CARTESIAN_POINT ( 'NONE',  ( 6.216353431943378638, 1.813724785205795609, 0.6947406154040984827 ) ) ;
#186080 = ORIENTED_EDGE ( 'NONE', *, *, #100779, .T. ) ;
#186079 = CARTESIAN_POINT ( 'NONE',  ( -6.982085920913410071, 11.08959130780024260, 0.7216878364870458196 ) ) ;
#186082 = ADVANCED_FACE ( 'NONE', ( #179046 ), #47996, .F. ) ;
#186081 = CARTESIAN_POINT ( 'NONE',  ( -4.132202957115018727, 8.042930226601317401, 0.000000000000000000 ) ) ;
#186083 = DIRECTION ( 'NONE',  ( 0.000000000000000000, 0.000000000000000000, 1.000000000000000000 ) ) ;
#186084 = CARTESIAN_POINT ( 'NONE',  ( -2.844178363816758814, 6.540234867753325076, -0.7998128361456481317 ) ) ;
#186085 = CARTESIAN_POINT ( 'NONE',  ( -6.304178240230145391, 9.338329799368375816, 1.082531754730548412 ) ) ;
#186086 = CARTESIAN_POINT ( 'NONE',  ( 3.610573252990852744, -0.8922430012947217826, -2.018528625508857921 ) ) ;
#186087 = CARTESIAN_POINT ( 'NONE',  ( -3.285556943750000514, -2.676041666188707424, -1.896917185911906500 ) ) ;
#186088 = ORIENTED_EDGE ( 'NONE', *, *, #130618, .F. ) ;
#186089 = CARTESIAN_POINT ( 'NONE',  ( 0.7954780101973528694, -1.310620071111982421, -1.321417528198569613 ) ) ;
#186090 = CARTESIAN_POINT ( 'NONE',  ( -0.1288028175206544224, 1.298820314038674928, -2.522219681210400744 ) ) ;
#186091 = CARTESIAN_POINT ( 'NONE',  ( -1.001543065824772872E-14, 5.243750000682815937, 1.732050807568877637 ) ) ;
#186092 = CARTESIAN_POINT ( 'NONE',  ( -9.498564853506350047, -8.073984524010683117, 0.1796516426514711273 ) ) ;
#186094 = CARTESIAN_POINT ( 'NONE',  ( 6.825078400183568483, -0.002763825414428457399, 2.044262525762724270 ) ) ;
#186093 = CARTESIAN_POINT ( 'NONE',  ( -5.978723031652583231, 7.198045494411626777, -1.221819409761595088 ) ) ;
#186095 = CARTESIAN_POINT ( 'NONE',  ( 0.000000000000000000, 1.000000000000000888, 0.000000000000000000 ) ) ;
#186096 = EDGE_LOOP ( 'NONE', ( #192929, #79567, #176380, #10906 ) ) ;
#186097 = CARTESIAN_POINT ( 'NONE',  ( 2.799741500914772807, -0.6479443615096942555, 1.956441213939211554 ) ) ;
#186098 = CARTESIAN_POINT ( 'NONE',  ( 1.360316468749963592, 0.03645833367470611985, -0.7853790794159122290 ) ) ;
#186099 = CARTESIAN_POINT ( 'NONE',  ( -6.715366157470410435, 6.729015360003925750, -0.7998128361456291469 ) ) ;
#186100 = FACE_OUTER_BOUND ( 'NONE', #69040, .T. ) ;
#186101 = SURFACE_STYLE_FILL_AREA ( #37731 ) ;
#186102 = CARTESIAN_POINT ( 'NONE',  ( 3.388648328411762556, 6.040841252200647382, 1.199719254218462483 ) ) ;
#186103 = CARTESIAN_POINT ( 'NONE',  ( 1.481398948507294477, 1.904550386266171902, -0.7878645111692607061 ) ) ;
#186105 = CARTESIAN_POINT ( 'NONE',  ( 0.6823417656249969321, 13.52604166700806232, -1.181850606188757036 ) ) ;
#186104 = CARTESIAN_POINT ( 'NONE',  ( 4.856179778084614540, 5.010200168423447842, 0.6077543439236311462 ) ) ;
#186106 = CARTESIAN_POINT ( 'NONE',  ( 5.957918438201454059, 9.038323046955323292, -1.199719254218440723 ) ) ;
#186107 = CARTESIAN_POINT ( 'NONE',  ( 1.420000000000001039, 7.176846818246214177, -4.202462424328213153 ) ) ;
#186108 = CARTESIAN_POINT ( 'NONE',  ( 5.813141826352885566, 1.944573597739504889, 1.043518232037063287 ) ) ;
#186109 = CARTESIAN_POINT ( 'NONE',  ( 0.3687372981288695728, -1.412185959430117821, 1.636573055046482983 ) ) ;
#186110 = CARTESIAN_POINT ( 'NONE',  ( -3.931501358282937009, 7.530575984731317618, 0.7216878364870317197 ) ) ;
#186111 = CARTESIAN_POINT ( 'NONE',  ( 0.3390778084843976137, -1.706115258973059490, -1.074657883261991076 ) ) ;
#186112 = CIRCLE ( 'NONE', #23449, 12.00000000000000178 ) ;
#186113 = CARTESIAN_POINT ( 'NONE',  ( 1.599382804601066743, 1.132622197759477478, -1.999898178936350357 ) ) ;
#186114 = CARTESIAN_POINT ( 'NONE',  ( -4.255895783434943347, 3.981256129034934421, -0.3686001492455212025 ) ) ;
#186115 = DIRECTION ( 'NONE',  ( 0.000000000000000000, 0.000000000000000000, 1.000000000000000000 ) ) ;
#186116 = FILL_AREA_STYLE_COLOUR ( '', #30112 ) ;
#186117 = CARTESIAN_POINT ( 'NONE',  ( 2.324885834233282544, -0.002380789299309681549, 1.870836310375329381 ) ) ;
#186118 = CARTESIAN_POINT ( 'NONE',  ( 3.503138892209650024, -0.1435209762444041581, 2.011451614702438828 ) ) ;
#186120 = DIRECTION ( 'NONE',  ( 1.000000000000000000, -0.000000000000000000, -0.000000000000000000 ) ) ;
#186119 = CARTESIAN_POINT ( 'NONE',  ( -1.402160292154681736E-14, 1.196875000341419026, -1.575800808251659024 ) ) ;
#186122 = CARTESIAN_POINT ( 'NONE',  ( 4.565121803138184831, -1.881030885445551304, -0.9473677958443439406 ) ) ;
#186121 = CARTESIAN_POINT ( 'NONE',  ( -6.418895661066105873, 9.576129806964074120, -1.199719254218440723 ) ) ;
#186123 = CARTESIAN_POINT ( 'NONE',  ( 6.283314124929436417, 9.417951348137970413, -1.199719254218440723 ) ) ;
#186125 = CARTESIAN_POINT ( 'NONE',  ( -7.725448601688521322, 7.907444878258402809, 1.040834085586084257E-14 ) ) ;
#186124 = CARTESIAN_POINT ( 'NONE',  ( 3.736153849017632922, 6.516540702899320081, -1.199719254218453823 ) ) ;
#186126 = CARTESIAN_POINT ( 'NONE',  ( 1.286956418854607431, 3.652345658002486672, 0.4592741676706121323 ) ) ;
#186127 = CARTESIAN_POINT ( 'NONE',  ( 4.060810560252373413, 0.5428485958907465214, 1.945370397410832730 ) ) ;
#186128 = CARTESIAN_POINT ( 'NONE',  ( 1.499999999999985123, -0.4229166659838508036, -0.8660254037844323793 ) ) ;
#186129 = CARTESIAN_POINT ( 'NONE',  ( 1.024372331059967056, 1.013329571420513053, 1.796381585629814426 ) ) ;
#186130 = CARTESIAN_POINT ( 'NONE',  ( 7.239690840017413365, 10.42976116578691403, -1.082531754730537976 ) ) ;
#186131 = CARTESIAN_POINT ( 'NONE',  ( 5.817692603468245238, -2.110333850551704415, 0.4673072906974176655 ) ) ;
#186132 = CARTESIAN_POINT ( 'NONE',  ( 5.417364897112183719, 8.477953592343014932, 1.199719254218451159 ) ) ;
#186133 = CARTESIAN_POINT ( 'NONE',  ( 0.6823417656249864960, -0.7614583329919113464, -1.181850606188749264 ) ) ;
#186134 = CARTESIAN_POINT ( 'NONE',  ( 6.204791576909545192, 7.267953590263130259, -1.199719254218452047 ) ) ;
#186135 = CARTESIAN_POINT ( 'NONE',  ( 6.100805936025112786, 10.06143132543056673, 1.040834085586084257E-14 ) ) ;
#186137 = CARTESIAN_POINT ( 'NONE',  ( -3.591468823281545930, 3.560404793497018439, -2.500000000000000444 ) ) ;
#186136 = CARTESIAN_POINT ( 'NONE',  ( 2.699877945841188343, -1.607453219145397849, -1.459642119406568739 ) ) ;
#186139 = CARTESIAN_POINT ( 'NONE',  ( 1.962219809069129184, -1.683971100191889336, -0.7449956418128443891 ) ) ;
#186138 = CARTESIAN_POINT ( 'NONE',  ( -6.399085315970155285, 6.567947078161039620, -0.7216878364870278340 ) ) ;
#186140 = CARTESIAN_POINT ( 'NONE',  ( -1.201851678989727383E-14, 3.321875000341421025, 1.575800808251672791 ) ) ;
#186141 = CARTESIAN_POINT ( 'NONE',  ( 3.650093349144762023, 0.7902683543556283663, 2.044282924279612779 ) ) ;
#186142 = CARTESIAN_POINT ( 'NONE',  ( 6.883263157960421097, 0.5621630953002605402, 2.205140871664055702 ) ) ;
#186143 = CARTESIAN_POINT ( 'NONE',  ( 4.715850076732730045, -2.219782111298532978, 0.4368881197941154038 ) ) ;
#186144 = CARTESIAN_POINT ( 'NONE',  ( -6.826694039680798021, 7.923230120171105284, -1.199719254218446718 ) ) ;
#186146 = AXIS2_PLACEMENT_3D ( 'NONE', #185866, #37501, #52682 ) ;
#186145 = CARTESIAN_POINT ( 'NONE',  ( -11.84100621633422179, 9.989584257766621178, 1.444132586618105174 ) ) ;
#186147 = CARTESIAN_POINT ( 'NONE',  ( 6.373787108001086388, 6.824503602047865769, -0.5760177672454840359 ) ) ;
#186148 = CARTESIAN_POINT ( 'NONE',  ( -0.7500000000000006661, 13.20833333333333570, -1.299038105676657340 ) ) ;
#186149 = CARTESIAN_POINT ( 'NONE',  ( -5.438229012412890917, 8.398332043573416783, -1.082531754730549967 ) ) ;
#186151 = VECTOR ( 'NONE', #2645, 1000.000000000000000 ) ;
#186150 = CARTESIAN_POINT ( 'NONE',  ( 6.102578539926878598, 7.252668063737060855, -1.082531754730548412 ) ) ;
#186152 = CARTESIAN_POINT ( 'NONE',  ( 4.885902211565920972, -0.8344178305333300738, 1.560695085661115922 ) ) ;
#186153 = CARTESIAN_POINT ( 'NONE',  ( 7.248805684800777804, 11.60869039890961218, 1.040834085586084257E-14 ) ) ;
#186154 = CARTESIAN_POINT ( 'NONE',  ( 1.465998146299499094, 2.074868464730471374, -0.3595401751291906756 ) ) ;
#186156 = CARTESIAN_POINT ( 'NONE',  ( 1.499999999999987121, 2.545833333333351156, -0.8660254037844262731 ) ) ;
#186155 = CARTESIAN_POINT ( 'NONE',  ( 0.6823417656249934904, 12.44270833367473017, 1.181850606188764807 ) ) ;
#186157 = CARTESIAN_POINT ( 'NONE',  ( 2.031642458604762780, 1.885605923395494044, -0.5689241207685117319 ) ) ;
#186158 =( GEOMETRIC_REPRESENTATION_CONTEXT ( 3 ) GLOBAL_UNCERTAINTY_ASSIGNED_CONTEXT ( ( #110212 ) ) GLOBAL_UNIT_ASSIGNED_CONTEXT ( ( #176099, #46106, #112224 ) ) REPRESENTATION_CONTEXT ( 'NONE', 'WORKASPACE' ) );
#186159 = DIRECTION ( 'NONE',  ( 0.000000000000000000, 0.000000000000000000, -1.000000000000000000 ) ) ;
#186160 = CARTESIAN_POINT ( 'NONE',  ( 1.004302930252164871E-16, 3.599999999999999201, 1.500000000000000222 ) ) ;
#186162 = EDGE_LOOP ( 'NONE', ( #37463, #15866, #194203, #51050, #188044, #114006, #139081, #47960, #192414, #63408 ) ) ;
#186161 = CARTESIAN_POINT ( 'NONE',  ( 6.240474538790502734, 1.035194401182498281, -1.486496517754380742 ) ) ;
#186163 = CARTESIAN_POINT ( 'NONE',  ( 6.155038550924150087, 7.243595066575396757, 1.082531754730558626 ) ) ;
#186164 = CARTESIAN_POINT ( 'NONE',  ( 0.6823417656249864960, -0.5114583329919111243, -1.181850606188749264 ) ) ;
#186165 = CARTESIAN_POINT ( 'NONE',  ( 5.330866702616011921, 0.1386157390740362649, 1.865562100978317206 ) ) ;
#186166 = CARTESIAN_POINT ( 'NONE',  ( 5.541872263726007830, 1.386227983376321582, 1.537841262885197846 ) ) ;
#186167 = CYLINDRICAL_SURFACE ( 'NONE', #208211, 0.2500000000000578981 ) ;
#186168 = CARTESIAN_POINT ( 'NONE',  ( -4.787437638956935082, 6.678706226906775179, -1.443375672974066548 ) ) ;
#186169 = CARTESIAN_POINT ( 'NONE',  ( 2.373851744317274193, 1.000000000000000888, -11.76285798163019969 ) ) ;
#186170 = CARTESIAN_POINT ( 'NONE',  ( -1.402160292154681736E-14, -0.1624999999999815481, -1.732050807568870754 ) ) ;
#186171 = CARTESIAN_POINT ( 'NONE',  ( 7.721532178182734185, 8.967207948423393304, 1.199719254218462483 ) ) ;
#186172 = CARTESIAN_POINT ( 'NONE',  ( -8.853638004923878313, 10.28799807962136548, 1.199719254218462483 ) ) ;
#186173 = CARTESIAN_POINT ( 'NONE',  ( 6.530187263637528439, 7.647581891445782709, -1.199719254218452047 ) ) ;
#186174 = CARTESIAN_POINT ( 'NONE',  ( -1.402160292154681736E-14, -0.5531249996585814177, -1.575800808251665908 ) ) ;
#186175 = CARTESIAN_POINT ( 'NONE',  ( -1.402160292154681736E-14, 1.587500000000018785, -1.732050807568863648 ) ) ;
#186177 = CARTESIAN_POINT ( 'NONE',  ( 5.229694566569264680, 7.124396299129368337, 1.599625672291267398 ) ) ;
#186176 = CARTESIAN_POINT ( 'NONE',  ( 5.230891786122516152, -1.846674803186045821, -0.6626716404555529349 ) ) ;
#186178 = CARTESIAN_POINT ( 'NONE',  ( 3.022814370378481552, 2.006652721595225675, -0.1948103792988181704 ) ) ;
#186179 = CARTESIAN_POINT ( 'NONE',  ( 2.782342135839787289, -0.5608490805640730104, -1.831745072482870107 ) ) ;
#186180 = DIRECTION ( 'NONE',  ( 0.000000000000000000, -1.000000000000000000, 0.000000000000000000 ) ) ;
#186181 = CARTESIAN_POINT ( 'NONE',  ( 0.06437606466144081552, -1.426665095847098330, 1.663708609037084951 ) ) ;
#186182 = CYLINDRICAL_SURFACE ( 'NONE', #87470, 1.500000000000000222 ) ;
#186183 = CARTESIAN_POINT ( 'NONE',  ( 2.389737607000471442, -0.8038258883538218491, 1.689183408448757362 ) ) ;
#186184 = CARTESIAN_POINT ( 'NONE',  ( 0.6823417656249899377, 5.426041667008087543, -1.181850606188754593 ) ) ;
#186185 = CARTESIAN_POINT ( 'NONE',  ( 4.447525235540350508, -1.838889683631849348, 0.8198632543043646859 ) ) ;
#186186 = CARTESIAN_POINT ( 'NONE',  ( -9.332089804907933939, 9.781859615347734405, 1.040834085586084257E-14 ) ) ;
#186188 = CARTESIAN_POINT ( 'NONE',  ( 4.148151592129151410, 0.9998098737230370903, 1.866312969332243998 ) ) ;
#186187 = CARTESIAN_POINT ( 'NONE',  ( -6.073689629242176480, 6.188318776978391611, -0.7216878364870278340 ) ) ;
#186189 = CARTESIAN_POINT ( 'NONE',  ( 0.1747926744264668986, 7.629137130509083597, -2.455305974604498953 ) ) ;
#186190 = CARTESIAN_POINT ( 'NONE',  ( 6.268043187460373922, -2.055199631210803624, 0.2494731385529954104 ) ) ;
#186192 = CARTESIAN_POINT ( 'NONE',  ( 6.620655732516651071, -0.002413161512292844035, 2.173887093218453082 ) ) ;
#186191 = CARTESIAN_POINT ( 'NONE',  ( 1.734041596967655252, 2.068474147835582144, 0.3034153833333247396 ) ) ;
#186194 = ORIENTED_EDGE ( 'NONE', *, *, #91960, .F. ) ;
#186193 = CARTESIAN_POINT ( 'NONE',  ( 0.1293586867831516274, -1.054425554818343880, -1.365251215659948558 ) ) ;
#186195 = CARTESIAN_POINT ( 'NONE',  ( 7.426115451983150706, 9.686887332112256388, -1.599625672291262513 ) ) ;
#186196 = CARTESIAN_POINT ( 'NONE',  ( 7.905503641038563956, -6.808400134080580202, -7.455003611050280199 ) ) ;
#186197 = CARTESIAN_POINT ( 'NONE',  ( 2.920214025141053327, 6.445393704534057910, 0.4458799699700779495 ) ) ;
#186198 = CARTESIAN_POINT ( 'NONE',  ( -9.645001968711920171, 4.042125922905831281, 6.587946042608958663 ) ) ;
#186199 = CARTESIAN_POINT ( 'NONE',  ( 5.775410249297131315, 9.681803024247919609, 1.040834085586084257E-14 ) ) ;
#186200 = CARTESIAN_POINT ( 'NONE',  ( -1.907713928855389263, 3.283019769909803820, 0.4154771360143557635 ) ) ;
#186202 = CARTESIAN_POINT ( 'NONE',  ( 0.3459856143687444208, 0.9327069207067508749, -1.552719410179828952 ) ) ;
#186201 = CARTESIAN_POINT ( 'NONE',  ( 7.178115983792402233, 7.339166500704784823, 0.7998128361456281477 ) ) ;
#186203 = CARTESIAN_POINT ( 'NONE',  ( -7.857113714319432063, 9.125386407249497012, 1.199719254218462483 ) ) ;
#186204 = AXIS2_PLACEMENT_3D ( 'NONE', #83158, #168688, #182794 ) ;
#186205 = CARTESIAN_POINT ( 'NONE',  ( 5.412729640353754590, 7.337937218544611895, 1.599625672291267398 ) ) ;
#186206 = CARTESIAN_POINT ( 'NONE',  ( 2.345197385039651472, 5.679888015947478941, -0.7216878364870267237 ) ) ;
#186207 = CARTESIAN_POINT ( 'NONE',  ( 4.586165880992507660, 5.350526861157986147, -7.499999999999997335 ) ) ;
#186208 = CARTESIAN_POINT ( 'NONE',  ( 2.835626683552519012, 6.459981564119914310, 0.000000000000000000 ) ) ;
#186209 = ORIENTED_EDGE ( 'NONE', *, *, #195119, .T. ) ;
#186210 = EDGE_CURVE ( 'NONE', #195242, #171893, #1056, .T. ) ;
#186211 = EDGE_CURVE ( 'NONE', #55695, #152681, #178232, .T. ) ;
#186212 = CARTESIAN_POINT ( 'NONE',  ( 5.941029844038744123, -1.730876725876070221, -1.034150010194856417 ) ) ;
#186213 = CARTESIAN_POINT ( 'NONE',  ( -0.05774110376318035420, -1.308430771297011130, -1.669371405835825550 ) ) ;
#186214 = CARTESIAN_POINT ( 'NONE',  ( -3.007132747898833447, 6.372410370188839934, -0.7689175719093130912 ) ) ;
#186215 = CIRCLE ( 'NONE', #16752, 0.08000000000000020983 ) ;
#186216 = CARTESIAN_POINT ( 'NONE',  ( 0.000000000000000000, -3.600000000000005862, 0.000000000000000000 ) ) ;
#186217 = CARTESIAN_POINT ( 'NONE',  ( -1.543281805264341777, 8.695372333414642441, -2.508924166024196989 ) ) ;
#186218 = CARTESIAN_POINT ( 'NONE',  ( -5.748293942514189681, 5.808690475795744490, -0.7216878364870207285 ) ) ;
#186219 = CARTESIAN_POINT ( 'NONE',  ( 2.171277156482887882, 5.684907115872006145, -0.7998128361456291469 ) ) ;
#186220 = CARTESIAN_POINT ( 'NONE',  ( 3.221498965751792731, 0.2935017643310656177, -1.947342446911073610 ) ) ;
#186221 = CARTESIAN_POINT ( 'NONE',  ( 5.044546077387519922, -1.458546410489666600, 1.392558106302365095 ) ) ;
#186222 = CARTESIAN_POINT ( 'NONE',  ( -6.693975156845199059, 8.832723654451292816, 1.599625672291283607 ) ) ;
#186223 = CARTESIAN_POINT ( 'NONE',  ( -10.95855051086948606, -7.723431457505092190, 0.6286713519884027379 ) ) ;
#186224 = CARTESIAN_POINT ( 'NONE',  ( 4.593798273609356997, -2.190911875110569174, -0.05534364095756416635 ) ) ;
#186225 = DIRECTION ( 'NONE',  ( 0.000000000000000000, -1.000000000000000000, 0.000000000000000000 ) ) ;
#186226 = CARTESIAN_POINT ( 'NONE',  ( 3.030207491816420795, 1.071487476811390449, -1.600714694641630853 ) ) ;
#186227 = CARTESIAN_POINT ( 'NONE',  ( -8.128276786592724790, 9.441743324901704426, -1.199719254218446718 ) ) ;
#186228 = CARTESIAN_POINT ( 'NONE',  ( 0.000000000000000000, 15.50000000000019362, 0.000000000000000000 ) ) ;
#186229 = CARTESIAN_POINT ( 'NONE',  ( 0.1331565106231571705, 6.948071080078889850, -2.540993614958915181 ) ) ;
#186230 = FILL_AREA_STYLE ('',( #167866 ) ) ;
#186231 = VERTEX_POINT ( 'NONE', #169176 ) ;
#186232 = CARTESIAN_POINT ( 'NONE',  ( 5.126391479742934187, 6.113783160189109722, -1.082531754730548412 ) ) ;
#186233 = CARTESIAN_POINT ( 'NONE',  ( 4.592606226310515183, 1.930599660924517957, 0.3882996684868595394 ) ) ;
#186234 = ORIENTED_EDGE ( 'NONE', *, *, #180308, .T. ) ;
#186236 = CARTESIAN_POINT ( 'NONE',  ( 3.651042523073198431, 0.2976914719170896118, 1.990856138409332843 ) ) ;
#186235 = CARTESIAN_POINT ( 'NONE',  ( 0.8549040543346017040, 0.3774493213832031402, -1.904865965088814228 ) ) ;
#186237 = CARTESIAN_POINT ( 'NONE',  ( 5.448667688119189556, 1.537605954158068666, 1.708491323253034100 ) ) ;
#186238 = CARTESIAN_POINT ( 'NONE',  ( 3.783913598179854176, -1.105313619694109795, -1.496993097346049462 ) ) ;
#186239 = CARTESIAN_POINT ( 'NONE',  ( 6.282224075085741433, 8.422623735723785643, 1.599625672291268286 ) ) ;
#186240 = CARTESIAN_POINT ( 'NONE',  ( -1.115562610750309283E-14, 11.56249999999999822, 1.500000000000001554 ) ) ;
#186241 = DIRECTION ( 'NONE',  ( -0.2460297208025352678, 6.661338147750954034E-16, 0.9692622846690294169 ) ) ;
#186242 = CARTESIAN_POINT ( 'NONE',  ( -5.520141099058386125, 9.591915048876776595, 0.000000000000000000 ) ) ;
#186243 = CARTESIAN_POINT ( 'NONE',  ( -3.662110889467009578, 7.286563447771212232, 0.7216878364870338292 ) ) ;
#186244 = CARTESIAN_POINT ( 'NONE',  ( 0.08191350661116909848, -1.027414926483052326, 1.935800647029708443 ) ) ;
#186245 = CARTESIAN_POINT ( 'NONE',  ( 6.805829924380118356, 7.042482454639357847, 0.7216878364870317197 ) ) ;
#186246 = ORIENTED_EDGE ( 'NONE', *, *, #65502, .F. ) ;
#186247 = CARTESIAN_POINT ( 'NONE',  ( -0.4359508081057549833, -6.362962251423736504, -9.827407719474871683 ) ) ;
#186248 = CARTESIAN_POINT ( 'NONE',  ( 0.08226035653636187828, -1.769965142718381124, -0.4472663993063328847 ) ) ;
#186249 = CARTESIAN_POINT ( 'NONE',  ( -3.273404022695637572, 5.906389562198459231, 1.199719254218462483 ) ) ;
#186250 = CARTESIAN_POINT ( 'NONE',  ( 2.426026400502009128, -1.286032909179233297, -1.163566193670103832 ) ) ;
#186251 = CARTESIAN_POINT ( 'NONE',  ( -4.462041952228919861, 8.219816354326827224, -0.7216878364870170648 ) ) ;
#186252 = CARTESIAN_POINT ( 'NONE',  ( 6.509000000000047415, 2.458121647476101401, 2.283885694139938138 ) ) ;
#186253 = CARTESIAN_POINT ( 'NONE',  ( -4.530395885260773525, 8.437212299446219532, 0.7998128361456481317 ) ) ;
#186254 = DIRECTION ( 'NONE',  ( 0.000000000000000000, 0.000000000000000000, 1.000000000000000000 ) ) ;
#186255 = CARTESIAN_POINT ( 'NONE',  ( 0.4091448426733998445, -1.664836780672280803, 1.230395522420650201 ) ) ;
#186256 = CARTESIAN_POINT ( 'NONE',  ( 5.566980414702134894, -1.652319403193935887, -0.7768266693391965294 ) ) ;
#186257 = CARTESIAN_POINT ( 'NONE',  ( 3.379693149055284174, -1.891888713350448947, 0.5187481205842572329 ) ) ;
#186258 = AXIS2_PLACEMENT_3D ( 'NONE', #164863, #14328, #146518 ) ;
#186259 = CARTESIAN_POINT ( 'NONE',  ( -0.6125000000000331291, -0.6458333326505374394, 1.060881119635882497 ) ) ;
#186260 = CARTESIAN_POINT ( 'NONE',  ( -9.504429378379839477, 11.04725468198666150, 1.199719254218462483 ) ) ;
#186261 = CARTESIAN_POINT ( 'NONE',  ( 6.479907352327590964, 9.647310113435821677, 1.199719254218462483 ) ) ;
#186262 = CARTESIAN_POINT ( 'NONE',  ( 3.967525559752110631, -1.763746451813380967, -1.176840329774282212 ) ) ;
#186263 = CARTESIAN_POINT ( 'NONE',  ( 7.991605200612358573, 8.288237253661408843, 0.7998128361456281477 ) ) ;
#186264 = CARTESIAN_POINT ( 'NONE',  ( -9.429859533504656000, 10.96025652963230534, -1.199719254218441611 ) ) ;
#186265 = CARTESIAN_POINT ( 'NONE',  ( 1.375928118113247667, -2.020660359122231409, 0.4497719141252010111 ) ) ;
#186267 = CARTESIAN_POINT ( 'NONE',  ( -0.6823417656250003738, -0.7197916663252492686, -1.181850606188749264 ) ) ;
#186266 = FACE_OUTER_BOUND ( 'NONE', #47447, .T. ) ;
#186269 = ORIENTED_EDGE ( 'NONE', *, *, #137160, .T. ) ;
#186268 = CARTESIAN_POINT ( 'NONE',  ( 4.389451384964074165, 0.0001031656717501855256, -2.221473415372441806 ) ) ;
#186270 = CARTESIAN_POINT ( 'NONE',  ( 1.635759689059889554, 0.7259864748365916221, 2.181091778573934103 ) ) ;
#186271 = CARTESIAN_POINT ( 'NONE',  ( 8.378575743565351175, 11.75846021992619406, -1.082531754730543083 ) ) ;
#186273 = CARTESIAN_POINT ( 'NONE',  ( -1.737499999999997824, -0.6416666666666653862, 3.009438278150925683 ) ) ;
#186272 = CARTESIAN_POINT ( 'NONE',  ( 5.885648082108177803, 9.880690172519326353, 0.7216878364870317197 ) ) ;
#186274 = CARTESIAN_POINT ( 'NONE',  ( 0.000000000000000000, 0.000000000000000000, 0.000000000000000000 ) ) ;
#186275 = LINE ( 'NONE', #98655, #124015 ) ;
#186276 = CARTESIAN_POINT ( 'NONE',  ( -5.465417954149238255, 6.280545163089921168, -1.016043258478748434 ) ) ;
#186277 = EDGE_CURVE ( 'NONE', #167113, #81793, #39523, .T. ) ;
#186278 = CARTESIAN_POINT ( 'NONE',  ( 2.777492966359981441, 0.2764497561681695803, -1.892163382976944419 ) ) ;
#186279 = CARTESIAN_POINT ( 'NONE',  ( -0.3695500129099597020, 6.511094381872901238, -3.314792509164075529 ) ) ;
#186280 = CARTESIAN_POINT ( 'NONE',  ( 3.944159270863063060, 1.716513557549454339, 0.1685945156147239388 ) ) ;
#186281 = CARTESIAN_POINT ( 'NONE',  ( 2.729704159269104924, 0.7212915320151757070, -1.883313052590728454 ) ) ;
#186282 = CARTESIAN_POINT ( 'NONE',  ( 3.621995078338976715, 0.3387333280310041994, 2.273515639168000035 ) ) ;
#186283 = DIRECTION ( 'NONE',  ( 0.000000000000000000, 0.000000000000000000, -1.000000000000000000 ) ) ;
#186284 = CARTESIAN_POINT ( 'NONE',  ( 6.094376849853386346, -2.095768364502542003, -0.2079484218287275255 ) ) ;
#186285 = CARTESIAN_POINT ( 'NONE',  ( -6.292392690518223475, 6.513748691792265788, -0.7216878364870338292 ) ) ;
#186286 = CARTESIAN_POINT ( 'NONE',  ( 5.219873587733063758, -0.9469346145933134062, -1.494860035008038324 ) ) ;
#186288 = CARTESIAN_POINT ( 'NONE',  ( 1.342159615362942704, 2.289816521768207380, 0.1084569774388414870 ) ) ;
#186287 = CARTESIAN_POINT ( 'NONE',  ( 7.361151057576892143, 7.552707420120024828, 0.7998128361456291469 ) ) ;
#186289 = CARTESIAN_POINT ( 'NONE',  ( 6.439398882927052981, 0.6998097629446423662, -1.703160347957879850 ) ) ;
#186290 = CARTESIAN_POINT ( 'NONE',  ( -4.192495815123836955, 5.914331089109674089, -1.599625672291256295 ) ) ;
#186291 = VECTOR ( 'NONE', #4901, 1000.000000000000000 ) ;
#186292 = CARTESIAN_POINT ( 'NONE',  ( 5.173855182012670362, -1.219361875273092366, 1.820681821249593657 ) ) ;
#186293 = CARTESIAN_POINT ( 'NONE',  ( -5.815521545619021460, 5.749472989502435460, -0.7998128361456362523 ) ) ;
#186294 = CARTESIAN_POINT ( 'NONE',  ( 0.000000000000000000, 4.000000000000002665, 0.000000000000000000 ) ) ;
#186295 = CARTESIAN_POINT ( 'NONE',  ( 9.500102690074733403, -7.891095720666440272, -0.004933703209193082348 ) ) ;
#186296 = EDGE_CURVE ( 'NONE', #147150, #201525, #188261, .T. ) ;
#186297 = CARTESIAN_POINT ( 'NONE',  ( 0.7136160920222310855, -1.834322530278935215, -1.161324927271490060 ) ) ;
#186298 = CARTESIAN_POINT ( 'NONE',  ( 1.657435761918718331, 1.928256795251210631, -0.5899901959932273288 ) ) ;
#186299 = CARTESIAN_POINT ( 'NONE',  ( -1.500000000000015099, -0.5479166659838513587, 0.8660254037844403729 ) ) ;
#186300 = CARTESIAN_POINT ( 'NONE',  ( 4.143132006054106142, -1.675477906314150056, 0.9507637539484592448 ) ) ;
#186301 = CARTESIAN_POINT ( 'NONE',  ( 1.364683531249996529, 11.96354166700806765, 0.7879004041258405033 ) ) ;
#186302 = CARTESIAN_POINT ( 'NONE',  ( 1.705654399339423311, 1.929789488239462836, -1.100201954495036549 ) ) ;
#186304 = ORIENTED_EDGE ( 'NONE', *, *, #116619, .T. ) ;
#186303 = CARTESIAN_POINT ( 'NONE',  ( 9.134442807305049428, 11.67993591332117376, 1.599625672291281386 ) ) ;
#186306 = DIRECTION ( 'NONE',  ( -5.551115123125782702E-17, 0.000000000000000000, 1.000000000000000000 ) ) ;
#186305 = CARTESIAN_POINT ( 'NONE',  ( 1.150222622689962781, 2.983395032273045366, -0.7749999999993620881 ) ) ;
#186307 = CARTESIAN_POINT ( 'NONE',  ( 1.499999999999959588, 7.378742179571330162, -10.87908636427991382 ) ) ;
#186308 = CARTESIAN_POINT ( 'NONE',  ( 9.999301985278609806, 11.62460605670194447, 1.199719254218452047 ) ) ;
#186309 = DIRECTION ( 'NONE',  ( -1.000000000000000000, 0.000000000000000000, 0.000000000000000000 ) ) ;
#186310 = CARTESIAN_POINT ( 'NONE',  ( 6.882015208740342338, 14.48195938056239385, 9.732639244658489730 ) ) ;
#186311 = AXIS2_PLACEMENT_3D ( 'NONE', #58553, #9793, #73734 ) ;
#186312 = CARTESIAN_POINT ( 'NONE',  ( 4.106796630993492236, -0.2923914088966376723, 1.715523938624329281 ) ) ;
#186313 = CARTESIAN_POINT ( 'NONE',  ( 2.664445928352857429, -0.7481792696971514278, -1.813797970468238985 ) ) ;
#186315 = CARTESIAN_POINT ( 'NONE',  ( -1.201851678989727383E-14, 2.884375000341418804, 1.575800808251672791 ) ) ;
#186314 = CARTESIAN_POINT ( 'NONE',  ( 4.985647801523278133, 6.839675073242382553, -1.599625672291256295 ) ) ;
#186316 = CARTESIAN_POINT ( 'NONE',  ( -4.653572958549120564, 6.905085616583060748, 1.214936962016188726 ) ) ;
#186317 = CARTESIAN_POINT ( 'NONE',  ( -11.38999389752409819, 1.405705671057795092, 3.777644806142836487 ) ) ;
#186318 = CARTESIAN_POINT ( 'NONE',  ( 6.725062055625550705, -1.793239977796506457, -0.7961783947641184467 ) ) ;
#186319 = CARTESIAN_POINT ( 'NONE',  ( -6.157374318900681764, 10.33535380535947290, 0.7998128361456481317 ) ) ;
#186320 = CARTESIAN_POINT ( 'NONE',  ( -4.731432421044877934, 6.543090462684225450, -1.443375672974051449 ) ) ;
#186321 = CARTESIAN_POINT ( 'NONE',  ( 5.102750050473856547, 1.865045247124358818, 0.7672954931761333253 ) ) ;
#186322 = CARTESIAN_POINT ( 'NONE',  ( 1.376233744030544104, 1.349093794351564624, 1.816168808025316661 ) ) ;
#186324 = ORIENTED_EDGE ( 'NONE', *, *, #211148, .F. ) ;
#186323 = CARTESIAN_POINT ( 'NONE',  ( -7.067878151425722955, 7.140279352951794500, 0.7998128361456341429 ) ) ;
#186325 = CARTESIAN_POINT ( 'NONE',  ( 0.7499999999999885647, 0.2645833340161538039, 1.299038105676657340 ) ) ;
#186326 = CARTESIAN_POINT ( 'NONE',  ( 1.651402116136031051, 0.5479989942898423338, -1.788454331708405620 ) ) ;
#186327 = CARTESIAN_POINT ( 'NONE',  ( 0.7032560681843272876, 1.601581415593232860, 0.6654971025301190668 ) ) ;
#186328 = EDGE_CURVE ( 'NONE', #21185, #6643, #146616, .T. ) ;
#186330 = CARTESIAN_POINT ( 'NONE',  ( 4.599289333468261631, -0.5842463895667610041, 2.112197083089427885 ) ) ;
#186329 = CARTESIAN_POINT ( 'NONE',  ( 0.6801582343749865700, 1.307291667008089853, -1.178068619123883165 ) ) ;
#186331 = CARTESIAN_POINT ( 'NONE',  ( 5.526528793889518454, 1.380124021263717804, -1.849252619965065847 ) ) ;
#186332 = CARTESIAN_POINT ( 'NONE',  ( 6.626252497008212394, 1.190392663088507552, -1.681986249806742384 ) ) ;
#186333 = CARTESIAN_POINT ( 'NONE',  ( 3.257691520677992614, 0.8739490649069777684, 1.734254922796226506 ) ) ;
#186334 = CARTESIAN_POINT ( 'NONE',  ( -4.948362878863562742, 5.835806782504650236, 1.082531754730558626 ) ) ;
#186335 = EDGE_CURVE ( 'NONE', #135649, #55386, #126197, .T. ) ;
#186336 = DIRECTION ( 'NONE',  ( 1.000000000000000000, 0.000000000000000000, -0.000000000000000000 ) ) ;
#186337 = CARTESIAN_POINT ( 'NONE',  ( 4.904922738988922504, -1.081064280317966420, -1.701948707654332704 ) ) ;
#186338 = CARTESIAN_POINT ( 'NONE',  ( -3.077337680177623103, 6.534051693608437184, 0.7216878364870317197 ) ) ;
#186339 = CARTESIAN_POINT ( 'NONE',  ( -6.981522756394290319, 7.109807735406931783, 0.7998128361456341429 ) ) ;
#186340 = CARTESIAN_POINT ( 'NONE',  ( 7.425061681778431399, 11.81432239538354345, 0.7998128361456462443 ) ) ;
#186342 = CARTESIAN_POINT ( 'NONE',  ( 7.847520364415523808, -5.402328468025352493, -7.653681110113485175 ) ) ;
#186341 = CARTESIAN_POINT ( 'NONE',  ( 0.9260630535584664091, 1.089557764695957554, -1.464779044915397455 ) ) ;
#186343 = CARTESIAN_POINT ( 'NONE',  ( -6.473091995881817162, 6.516638514809040217, 0.7998128361456281477 ) ) ;
#186344 = CARTESIAN_POINT ( 'NONE',  ( -3.820365424000704557, 7.679119771301276209, -0.7998128361456481317 ) ) ;
#186345 = CARTESIAN_POINT ( 'NONE',  ( -10.21581353488473987, 4.000000000000001776, 7.512123095767014647 ) ) ;
#186346 = ORIENTED_EDGE ( 'NONE', *, *, #98433, .F. ) ;
#186347 = CARTESIAN_POINT ( 'NONE',  ( 6.403207051292992169, 1.711950105385249055, 1.147064539034772679 ) ) ;
#186348 = CARTESIAN_POINT ( 'NONE',  ( -6.089020385868862739, 8.197219431637373432, -1.443375672974066548 ) ) ;
#186349 = CARTESIAN_POINT ( 'NONE',  ( -3.789667630219657912, 4.380032642466370696, 1.199719254218462483 ) ) ;
#186350 = CARTESIAN_POINT ( 'NONE',  ( -10.48453286206953727, 11.12637651536962125, 0.7998128361456462443 ) ) ;
#186351 = CARTESIAN_POINT ( 'NONE',  ( 5.479167871109219767, -1.826835719847461847, -0.8615247647300682265 ) ) ;
#186353 = ORIENTED_EDGE ( 'NONE', *, *, #187477, .T. ) ;
#186352 = CARTESIAN_POINT ( 'NONE',  ( 5.936230101866142306, -1.231883464771424075, -1.848230934346828391 ) ) ;
#186354 = CARTESIAN_POINT ( 'NONE',  ( -6.994027139803241866, 9.253060644560830994, -1.599625672291271394 ) ) ;
#186355 = CARTESIAN_POINT ( 'NONE',  ( 6.006425746053997372, 6.966250444273174303, -1.199719254218445830 ) ) ;
#186356 = CARTESIAN_POINT ( 'NONE',  ( 5.787979943833009067, -0.9286772032993969583, 1.839872548930401974 ) ) ;
#186357 = CARTESIAN_POINT ( 'NONE',  ( 4.395157833011634096, -0.8647231026696032830, -1.821742675176166060 ) ) ;
#186358 = ORIENTED_EDGE ( 'NONE', *, *, #192214, .T. ) ;
#186359 = EDGE_LOOP ( 'NONE', ( #150610, #45712, #25543, #193926, #51010, #128051 ) ) ;
#186360 = CARTESIAN_POINT ( 'NONE',  ( 1.907713928855353069, 3.283019769909847785, -0.4154771360144025039 ) ) ;
#186361 = CARTESIAN_POINT ( 'NONE',  ( 4.054051625686104998, 4.688480637177271149, -1.199719254218446718 ) ) ;
#186363 = ORIENTED_EDGE ( 'NONE', *, *, #26050, .T. ) ;
#186362 = CARTESIAN_POINT ( 'NONE',  ( -5.447343857640614573, 9.577261277214532242, -0.7998128361456362523 ) ) ;
#186364 = CARTESIAN_POINT ( 'NONE',  ( 4.725438941449205288, 8.332574750205820280, 0.7120043264817934592 ) ) ;
#186365 = CARTESIAN_POINT ( 'NONE',  ( 3.831407535526813124, -1.356092489331266027, 1.492026659919619247 ) ) ;
#186366 = CARTESIAN_POINT ( 'NONE',  ( 3.591602706507342369, -1.839109287420921834, -0.08896477992388628075 ) ) ;
#186367 = CARTESIAN_POINT ( 'NONE',  ( -0.006200074199070590604, 15.44435154591194070, 11.95073779513205992 ) ) ;
#186368 = CARTESIAN_POINT ( 'NONE',  ( 2.702171824926146826, -0.7227257407616082263, 2.191671519121952461 ) ) ;
#186369 = CARTESIAN_POINT ( 'NONE',  ( 2.925527285498711549, 6.635141943048991742, 0.7998128361456281477 ) ) ;
#186370 = CARTESIAN_POINT ( 'NONE',  ( 5.009125465012424172, 1.878017946038791575, 1.070212309444783294 ) ) ;
#186371 = CARTESIAN_POINT ( 'NONE',  ( 9.108380270282433244, 9.520865158284665952, 1.040834085586084257E-14 ) ) ;
#186372 = CARTESIAN_POINT ( 'NONE',  ( 0.1341856092403709844, 0.3330598185416616119, 1.913145364980510799 ) ) ;
#186373 = CARTESIAN_POINT ( 'NONE',  ( -4.412288926243578935, 7.235088616337731260, 1.199719254218464037 ) ) ;
#186374 = CARTESIAN_POINT ( 'NONE',  ( -3.165656458280237118, 15.51990984979156352, 11.58349828325590991 ) ) ;
#186375 = CARTESIAN_POINT ( 'NONE',  ( -0.4019237886466837106, 12.72991455036743069, -1.500000000000000666 ) ) ;
#186376 = CARTESIAN_POINT ( 'NONE',  ( 2.817106861211693847, -0.1851908181382568019, 1.861470920997858380 ) ) ;
#186377 = AXIS2_PLACEMENT_3D ( 'NONE', #201962, #5900, #120832 ) ;
#186378 = CARTESIAN_POINT ( 'NONE',  ( 6.649300054797159909, -1.583302550941813491, -1.174460211130315512 ) ) ;
#186380 = CARTESIAN_POINT ( 'NONE',  ( -6.050681693448748177, 10.28115541899069463, 0.7998128361456291469 ) ) ;
#186379 = CARTESIAN_POINT ( 'NONE',  ( -1.402160292154681736E-14, -1.006249999317181620, 1.732050807568877637 ) ) ;
#186381 = CARTESIAN_POINT ( 'NONE',  ( 1.928631425534212074, 1.268998755960360603, -1.805353087401928569 ) ) ;
#186382 = ORIENTED_EDGE ( 'NONE', *, *, #180626, .F. ) ;
#186383 = CARTESIAN_POINT ( 'NONE',  ( 3.914023514147235261, 8.998170835453741745, -0.7749999999999996891 ) ) ;
#186384 = CARTESIAN_POINT ( 'NONE',  ( 4.650610384687404952, 5.384465856012134566, 1.199719254218462483 ) ) ;
#186385 = CARTESIAN_POINT ( 'NONE',  ( -3.574546055497324737, 7.322054164722185732, 0.7998128361456341429 ) ) ;
#186386 = CARTESIAN_POINT ( 'NONE',  ( -7.761717428875326341, -5.600320323339592399, 7.717216217110903109 ) ) ;
#186387 = CARTESIAN_POINT ( 'NONE',  ( 6.614144449397460157, -0.9292204182751627739, -1.738729380627493049 ) ) ;
#186388 = CARTESIAN_POINT ( 'NONE',  ( 0.2711454947614586608, -1.503558885491006247, 1.750568091222578282 ) ) ;
#186389 = CARTESIAN_POINT ( 'NONE',  ( 0.3616705494772323726, -0.5269360983083425376, 1.889693748445469224 ) ) ;
#186390 = CARTESIAN_POINT ( 'NONE',  ( 4.205966187000295342, 0.6995128471476423915, -1.940432845919232374 ) ) ;
#186391 = CARTESIAN_POINT ( 'NONE',  ( 6.344852701515477200, 6.504675694630598137, -0.7216878364870257245 ) ) ;
#186392 = CARTESIAN_POINT ( 'NONE',  ( 7.343676480457483002, 8.596652644402405841, -1.199719254218452047 ) ) ;
#186393 = VERTEX_POINT ( 'NONE', #134585 ) ;
#186394 = CARTESIAN_POINT ( 'NONE',  ( 6.765155463094740362, 10.83650577367847667, 0.7216878364870438212 ) ) ;
#186395 = CARTESIAN_POINT ( 'NONE',  ( -1.201851678989727383E-14, 3.884375000341423689, 1.575800808251672791 ) ) ;
#186396 = CARTESIAN_POINT ( 'NONE',  ( -10.84194285507322952, 4.687756354094246625, -5.144713108483911057 ) ) ;
#186397 = CARTESIAN_POINT ( 'NONE',  ( 5.802526556524483681, 5.871961858807763335, 1.040834085586084257E-14 ) ) ;
#186398 = CARTESIAN_POINT ( 'NONE',  ( 0.2393977111345606534, -0.1477851991248577135, -2.137246755706405210 ) ) ;
#186400 = CARTESIAN_POINT ( 'NONE',  ( 5.302248432823610358, 1.390444127666954355, -1.207098008268410183 ) ) ;
#186399 = CARTESIAN_POINT ( 'NONE',  ( 0.6124999999999862776, 0.3958333340161462877, 1.060881119635934455 ) ) ;
#186401 = ADVANCED_FACE ( 'NONE', ( #100967 ), #167056, .F. ) ;
#186402 = CARTESIAN_POINT ( 'NONE',  ( -2.391594655221676469, 3.742896273583256050, 11.51132696612781814 ) ) ;
#186403 = CARTESIAN_POINT ( 'NONE',  ( 0.000000000000000000, 6.999999999999999112, 0.000000000000000000 ) ) ;
#186404 = CARTESIAN_POINT ( 'NONE',  ( 0.4736314445139556684, 1.071599637473351629, 1.532994764490814177 ) ) ;
#186405 = CARTESIAN_POINT ( 'NONE',  ( -4.974982779204009553, 6.815313220028144769, 1.450550931683711298 ) ) ;
#186406 = CARTESIAN_POINT ( 'NONE',  ( 4.989037339704528229, 4.922891105851139315, 1.040834085586084257E-14 ) ) ;
#186407 = CARTESIAN_POINT ( 'NONE',  ( 6.184762415132515123, 7.051423785172313607, -1.050594063207562545 ) ) ;
#186408 = AXIS2_PLACEMENT_3D ( 'NONE', #74465, #171967, #73378 ) ;
#186409 = CARTESIAN_POINT ( 'NONE',  ( -1.264911064067347324, 3.734364735516694012, 0.5000000000000092149 ) ) ;
#186410 = CARTESIAN_POINT ( 'NONE',  ( 2.184116879877880724, -1.735013770989551896, -0.3484325113714877298 ) ) ;
#186411 = CARTESIAN_POINT ( 'NONE',  ( 0.06490398442321809735, -1.535895564731554863, 1.139000086266952483 ) ) ;
#186413 = CARTESIAN_POINT ( 'NONE',  ( 4.200734335399162411, 1.752999579934441998, 0.7727710859696481638 ) ) ;
#186412 = CARTESIAN_POINT ( 'NONE',  ( -8.306341666666730461, 12.84248237775322643, 1.040834085586084257E-14 ) ) ;
#186414 = CARTESIAN_POINT ( 'NONE',  ( -1.420000000000021911, 6.200000000000045475, 2.873333333333347728 ) ) ;
#186415 = CARTESIAN_POINT ( 'NONE',  ( 5.723099352235532677, -1.779878778038428200, -0.8436364978330126441 ) ) ;
#186416 = CARTESIAN_POINT ( 'NONE',  ( 0.03560581989598374242, -0.09759080014098624190, 2.118463022953632091 ) ) ;
#186417 = CARTESIAN_POINT ( 'NONE',  ( -4.634189577772691138, 4.300976017023221409, 1.214306433183764966E-14 ) ) ;
#186418 = CARTESIAN_POINT ( 'NONE',  ( 2.799504582125960095, -0.5885537693137884441, 1.775713401224961574 ) ) ;
#186420 = ORIENTED_EDGE ( 'NONE', *, *, #57578, .F. ) ;
#186419 = CARTESIAN_POINT ( 'NONE',  ( 6.305283062370508063, 1.438394668203015092, 0.9516435707833100777 ) ) ;
#186422 = CARTESIAN_POINT ( 'NONE',  ( 1.499999999999961364, 7.000000000000000000, -10.64483442802188939 ) ) ;
#186421 = CARTESIAN_POINT ( 'NONE',  ( 3.405080638938757343, 1.739790774466195789, -1.357627211771177178 ) ) ;
#186423 = CARTESIAN_POINT ( 'NONE',  ( 0.6823417656249882723, 2.988541667008084879, -1.181850606188754593 ) ) ;
#186424 = CARTESIAN_POINT ( 'NONE',  ( 1.029816311724339961, 1.988459969548944439, -0.5481627708354539497 ) ) ;
#186426 = AXIS2_PLACEMENT_3D ( 'NONE', #88388, #104645, #122038 ) ;
#186425 = CARTESIAN_POINT ( 'NONE',  ( 7.637320603199683866, 7.804628880021436288, -0.7998128361456281477 ) ) ;
#186427 = CARTESIAN_POINT ( 'NONE',  ( -8.422639742587602285, 10.84949900448412841, -1.599625672291263179 ) ) ;
#186428 = DIRECTION ( 'NONE',  ( -5.578564026256490882E-16, -1.000000000000000000, -9.066213480720158442E-32 ) ) ;
#186429 = CARTESIAN_POINT ( 'NONE',  ( -5.440899717785814715, 5.242137847038546461, 0.7998128361456341429 ) ) ;
#186430 = CARTESIAN_POINT ( 'NONE',  ( -7.439168848974001769, -6.893137084989842123, -8.103009739377998955 ) ) ;
#186431 = EDGE_LOOP ( 'NONE', ( #100812, #148553, #66790, #54830 ) ) ;
#186432 = CARTESIAN_POINT ( 'NONE',  ( 3.121598655985452275, 0.3063859900464052100, -2.047459029603612368 ) ) ;
#186433 = CARTESIAN_POINT ( 'NONE',  ( -1.499999999999997780, 3.900000000000021672, 1.214306433183764966E-14 ) ) ;
#186434 = CARTESIAN_POINT ( 'NONE',  ( 4.690231075323689325, 7.559354456931247412, 1.199719254218462483 ) ) ;
#186435 = CARTESIAN_POINT ( 'NONE',  ( -6.081163491871431681, 7.123212080692602477, 1.153528356629534013 ) ) ;
#186436 = CARTESIAN_POINT ( 'NONE',  ( 0.8912779446055114629, -0.05177971647825175411, -2.019189627193836323 ) ) ;
#186437 = FILL_AREA_STYLE ('',( #20725 ) ) ;
#186438 = CARTESIAN_POINT ( 'NONE',  ( 0.6823417656249899377, 3.426041667008085323, -1.181850606188754593 ) ) ;
#186439 = ORIENTED_EDGE ( 'NONE', *, *, #44801, .T. ) ;
#186441 = CARTESIAN_POINT ( 'NONE',  ( 9.897088948295946764, 10.64895131587453569, 0.7216878364870438212 ) ) ;
#186440 = CARTESIAN_POINT ( 'NONE',  ( 0.1745949693968797123, 1.415412180343596837, -2.016327490378281073 ) ) ;
#186442 = CARTESIAN_POINT ( 'NONE',  ( 6.884150277402729223, -0.1485532345978715640, 1.983297619905934006 ) ) ;
#186443 = CARTESIAN_POINT ( 'NONE',  ( 5.841025094292755071, -1.646784362596087625, -0.9785371348113005574 ) ) ;
#186444 = FILL_AREA_STYLE_COLOUR ( '', #162317 ) ;
#186445 = CARTESIAN_POINT ( 'NONE',  ( 3.368858348882136422, 0.05182064297618373117, -2.191103300807801801 ) ) ;
#186446 =( BOUNDED_CURVE ( )  B_SPLINE_CURVE ( 2, ( #1677, #3799, #120871, #20068, #84014, #86157, #165275 ),
 .UNSPECIFIED., .F., .T. ) 
 B_SPLINE_CURVE_WITH_KNOTS ( ( 3, 2, 2, 3 ),
 ( 0.1964285714285713413, 0.2023809523809523836, 0.2083333333333334536, 0.2142857142857144681 ),
 .UNSPECIFIED. ) 
 CURVE ( )  GEOMETRIC_REPRESENTATION_ITEM ( )  RATIONAL_B_SPLINE_CURVE ( ( 1.000000000000001776, 0.8660254037844368202, 1.000000000000000000, 0.8660254037844387076, 1.000000000000000000, 0.8660254037844343777, 1.000000000000004441 ) ) 
 REPRESENTATION_ITEM ( '' )  );
#186447 = CARTESIAN_POINT ( 'NONE',  ( -1.500000000000013101, 2.660416667349483788, -0.8660254037844313801 ) ) ;
#186448 = CARTESIAN_POINT ( 'NONE',  ( 2.496234081663367022, -0.9796988711565941532, 1.642222327643327873 ) ) ;
#186449 = CARTESIAN_POINT ( 'NONE',  ( -5.687809136132860210, 6.594531066031826150, -1.199719254218446718 ) ) ;
#186450 = CARTESIAN_POINT ( 'NONE',  ( 5.802526556524483681, 5.871961858807763335, 1.040834085586084257E-14 ) ) ;
#186452 = CARTESIAN_POINT ( 'NONE',  ( 1.476185646619165626, -2.006963189339417308, -0.1948195631672477446 ) ) ;
#186451 = LINE ( 'NONE', #57537, #180621 ) ;
#186453 = CARTESIAN_POINT ( 'NONE',  ( -8.012344526598182026E-15, 10.60937500034139624, -1.575800808251669460 ) ) ;
#186455 = CARTESIAN_POINT ( 'NONE',  ( -3.630551273409382329, 7.457669928944732796, 0.7998128361456352531 ) ) ;
#186454 = CARTESIAN_POINT ( 'NONE',  ( 6.614806895146394972, -0.1608752592793839531, 2.155998228907447523 ) ) ;
#186457 = VERTEX_POINT ( 'NONE', #38119 ) ;
#186456 = CARTESIAN_POINT ( 'NONE',  ( 2.748708976905740897, -1.435238111852419562, 0.9561691852014215787 ) ) ;
#186458 = CARTESIAN_POINT ( 'NONE',  ( -0.1405533004718312329, 0.7798934913714054007, -1.807795836271476331 ) ) ;
#186459 = CARTESIAN_POINT ( 'NONE',  ( 7.741869408603235136, 8.990934717247309749, 1.199719254218462483 ) ) ;
#186460 = CARTESIAN_POINT ( 'NONE',  ( 3.825371897350130723, 7.614684313550482031, 0.7998128361456321445 ) ) ;
#186461 = EDGE_CURVE ( 'NONE', #82463, #207870, #79451, .T. ) ;
#186462 = CARTESIAN_POINT ( 'NONE',  ( -0.8537267228922215123, 13.37576698399828423, -1.079790317083570761 ) ) ;
#186463 = CARTESIAN_POINT ( 'NONE',  ( 1.416376618315864144, 0.7919773292732554815, 1.795081228748253377 ) ) ;
#186464 =( BOUNDED_CURVE ( )  B_SPLINE_CURVE ( 2, ( #152644, #21541, #140704 ),
 .UNSPECIFIED., .F., .T. ) 
 B_SPLINE_CURVE_WITH_KNOTS ( ( 3, 3 ),
 ( 0.2461080272610979280, 0.2500000000000002776 ),
 .UNSPECIFIED. ) 
 CURVE ( )  GEOMETRIC_REPRESENTATION_ITEM ( )  RATIONAL_B_SPLINE_CURVE ( ( 0.9333038493907171995, 0.9374289428588350459, 1.000000000000004441 ) ) 
 REPRESENTATION_ITEM ( '' )  );
#186465 = CARTESIAN_POINT ( 'NONE',  ( 4.222474775652216294, 7.013638773981186958, 1.199719254218462483 ) ) ;
#186466 = CARTESIAN_POINT ( 'NONE',  ( 3.189213936345663747, 2.817530495244580102, -2.450448857954562243 ) ) ;
#186467 = ORIENTED_EDGE ( 'NONE', *, *, #178523, .T. ) ;
#186468 = CARTESIAN_POINT ( 'NONE',  ( 0.4373349612950711007, -5.212340523078045962, 10.97895254167818280 ) ) ;
#186469 = ORIENTED_EDGE ( 'NONE', *, *, #84254, .F. ) ;
#186470 = CARTESIAN_POINT ( 'NONE',  ( 3.809066866439265286, 1.528366121442883196, -0.9720638507800370975 ) ) ;
#186471 = ORIENTED_EDGE ( 'NONE', *, *, #70737, .F. ) ;
#186472 = CARTESIAN_POINT ( 'NONE',  ( 10.37606763316019531, 10.99983374830873650, 0.7998128361456462443 ) ) ;
#186473 = CARTESIAN_POINT ( 'NONE',  ( 4.435452530326143616, 5.203724702582467998, -1.199719254218452047 ) ) ;
#186474 = CARTESIAN_POINT ( 'NONE',  ( 4.512255818007496977, -1.811207030272870000, -0.03965706671436861758 ) ) ;
#186475 = CARTESIAN_POINT ( 'NONE',  ( 0.04765083308771843329, -6.900199406649612399, 9.605391220871890567 ) ) ;
#186476 = AXIS2_PLACEMENT_3D ( 'NONE', #210169, #178772, #79115 ) ;
#186477 = CARTESIAN_POINT ( 'NONE',  ( 10.98535488200954902, 13.75822556747230330, -1.593017372382192098 ) ) ;
#186478 = CARTESIAN_POINT ( 'NONE',  ( 5.886971415934090679, 5.980320297827544707, -0.1280069804882408846 ) ) ;
#186479 = EDGE_CURVE ( 'NONE', #115124, #110438, #115814, .T. ) ;
#186480 = STYLED_ITEM ( 'NONE', ( #101563 ), #158480 ) ;
#186482 = CARTESIAN_POINT ( 'NONE',  ( -8.012344526598182026E-15, 15.04687500034140157, -1.575800808251669460 ) ) ;
#186481 = CARTESIAN_POINT ( 'NONE',  ( 5.687920738472253213, -1.181023890769626217, -1.438316992653262627 ) ) ;
#186483 = EDGE_CURVE ( 'NONE', #100589, #58795, #107450, .T. ) ;
#186484 = CARTESIAN_POINT ( 'NONE',  ( 2.372541684819210683, -0.3298082299327957378, -1.886833909188085912 ) ) ;
#186485 = CARTESIAN_POINT ( 'NONE',  ( -2.788906526875773208E-15, 10.68750000000000000, -1.499999999999998446 ) ) ;
#186486 = CARTESIAN_POINT ( 'NONE',  ( -10.47476534206535170, 5.237283261923990629, -5.169982392003922733 ) ) ;
#186487 = CARTESIAN_POINT ( 'NONE',  ( 9.499750697158754420, -9.920000000031521381, -0.06885943948997400033 ) ) ;
#186488 = CARTESIAN_POINT ( 'NONE',  ( 11.41157692552970637, 13.75910337086997792, 3.404533818002357215 ) ) ;
#186489 = CARTESIAN_POINT ( 'NONE',  ( 7.782016984564065432, 8.181367358187307204, 0.7216878364870458196 ) ) ;
#186490 = CARTESIAN_POINT ( 'NONE',  ( 2.553923023464285347, 1.082840749376843270, 1.700961377887353798 ) ) ;
#186491 = CARTESIAN_POINT ( 'NONE',  ( -4.952806187693842510, 4.672695395264567786, 0.7998128361456341429 ) ) ;
#186492 = CARTESIAN_POINT ( 'NONE',  ( 0.000000000000000000, 8.500000000000000000, 0.000000000000000000 ) ) ;
#186493 = CARTESIAN_POINT ( 'NONE',  ( 1.341864181646670540, 2.088322648670298598, 0.1009416716012418447 ) ) ;
#186494 = CARTESIAN_POINT ( 'NONE',  ( 4.694866332082116678, 8.699370830729650450, 0.7998128361456341429 ) ) ;
#186495 = CARTESIAN_POINT ( 'NONE',  ( 6.774445256934315651, -1.184694399318196201, 1.519801669933226407 ) ) ;
#186496 = CARTESIAN_POINT ( 'NONE',  ( -4.446184310277715213, 7.274633231044262516, -1.199719254218452047 ) ) ;
#186497 = CARTESIAN_POINT ( 'NONE',  ( 2.502731746374619259, 1.467688513602287470, -1.085450786651315225 ) ) ;
#186498 = EDGE_CURVE ( 'NONE', #58494, #169262, #124786, .T. ) ;
#186499 = CARTESIAN_POINT ( 'NONE',  ( 10.91804383151479740, -8.407420853759283830, -0.1905751639681655396 ) ) ;
#186500 = CARTESIAN_POINT ( 'NONE',  ( 2.074333847954575205, 0.8209984392052707136, 1.727357542596375861 ) ) ;
#186501 = CARTESIAN_POINT ( 'NONE',  ( 1.433975083751269697, 1.170624227716898780, 1.583764482814524088 ) ) ;
#186502 = CARTESIAN_POINT ( 'NONE',  ( 3.579573000355208645, -0.9547435552521261748, 1.691086383587044883 ) ) ;
#186503 = ORIENTED_EDGE ( 'NONE', *, *, #54197, .F. ) ;
#186504 = CARTESIAN_POINT ( 'NONE',  ( -4.911285141672522059, 4.693790260148114513, 0.3511878651327460243 ) ) ;
#186505 = CARTESIAN_POINT ( 'NONE',  ( -5.113360211009450040, 5.994616996712990975, -1.199719254218453823 ) ) ;
#186507 = CARTESIAN_POINT ( 'NONE',  ( 4.623349522974431025, 1.846400237221163865, 1.042759738753673338 ) ) ;
#186506 = CARTESIAN_POINT ( 'NONE',  ( 2.925527285498711549, 6.635141943048991742, 0.7998128361456281477 ) ) ;
#186508 = CARTESIAN_POINT ( 'NONE',  ( 6.684387857553273804, -6.724344753046613832, 6.908358566921364741 ) ) ;
#186509 = CARTESIAN_POINT ( 'NONE',  ( 9.420217803396747414, 9.884675613584706255, 0.7998128361456462443 ) ) ;
#186510 = CARTESIAN_POINT ( 'NONE',  ( 5.593492625449885125, 6.357122791843209164, 1.180528715873955692 ) ) ;
#186511 = CARTESIAN_POINT ( 'NONE',  ( 1.499999999999993117, 11.63541666734946567, 0.8660254037844408170 ) ) ;
#186512 = CARTESIAN_POINT ( 'NONE',  ( 6.875920180786008196, 8.050936961452347163, -1.199719254218452047 ) ) ;
#186513 = LINE ( 'NONE', #86891, #13045 ) ;
#186515 = CARTESIAN_POINT ( 'NONE',  ( 6.139861302770143858, 2.010801613648224961, -0.1531635369260639090 ) ) ;
#186514 = CARTESIAN_POINT ( 'NONE',  ( 3.809063337113669068, 1.566667275063510445, 0.9371452329686791316 ) ) ;
#186516 = CARTESIAN_POINT ( 'NONE',  ( 10.99944088594791580, -9.904389777384739801, -0.1109062511178756510 ) ) ;
#186517 = CARTESIAN_POINT ( 'NONE',  ( -9.571693261567968847, 12.19006144329456731, 1.443375672974076540 ) ) ;
#186518 =( BOUNDED_CURVE ( )  B_SPLINE_CURVE ( 3, ( #17740, #197582, #181336, #133698 ),
 .UNSPECIFIED., .F., .T. ) 
 B_SPLINE_CURVE_WITH_KNOTS ( ( 4, 4 ),
 ( 0.000000000000000000, 0.4999999999999988898 ),
 .UNSPECIFIED. ) 
 CURVE ( )  GEOMETRIC_REPRESENTATION_ITEM ( )  RATIONAL_B_SPLINE_CURVE ( ( 1.000000000000000000, 0.3333333333333348691, 0.3333333333333333703, 0.9999999999999985567 ) ) 
 REPRESENTATION_ITEM ( '' )  );
#186519 = MECHANICAL_DESIGN_GEOMETRIC_PRESENTATION_REPRESENTATION (  '', ( #27424 ), #100098 ) ;
#186520 = CARTESIAN_POINT ( 'NONE',  ( -4.592595068035599581, 8.488991103336598343, 0.1827531742817755656 ) ) ;
#186521 = DIRECTION ( 'NONE',  ( 0.7347175152297782397, 3.929830605827906454E-15, -0.6783731810844091381 ) ) ;
#186522 = CARTESIAN_POINT ( 'NONE',  ( 4.346470048663173102, 0.4987854378066917116, 1.802870001028591407 ) ) ;
#186523 = CARTESIAN_POINT ( 'NONE',  ( 6.740374924288304648, 11.01552117831172062, 1.040834085586084257E-14 ) ) ;
#186524 = CARTESIAN_POINT ( 'NONE',  ( 2.068856375562718508, -1.761265384887151342, -0.7809992120406393790 ) ) ;
#186525 = CARTESIAN_POINT ( 'NONE',  ( 6.737165023268617325, -0.09304339776683605290, -1.959646862056351857 ) ) ;
#186526 = CARTESIAN_POINT ( 'NONE',  ( -1.364683531250010295, 8.692708333674730170, 0.7879004041258445001 ) ) ;
#186527 = CARTESIAN_POINT ( 'NONE',  ( -4.713430959045263435, 8.650753218861462202, 0.7998128361456481317 ) ) ;
#186528 = CARTESIAN_POINT ( 'NONE',  ( 3.011882680530176604, 6.665613560593854459, 0.7998128361456341429 ) ) ;
#186529 = CARTESIAN_POINT ( 'NONE',  ( -5.112833325684920993, 6.097965313788082931, -1.082531754730549967 ) ) ;
#186531 = CARTESIAN_POINT ( 'NONE',  ( 0.9665973488726641305, -2.066607521123296376, -0.4595904307344770290 ) ) ;
#186530 = B_SPLINE_CURVE_WITH_KNOTS ( 'NONE', 3,
 ( #38815, #186114, #21460, #182921, #85424, #67010 ),
 .UNSPECIFIED., .F., .F.,
 ( 4, 2, 4 ),
 ( 1.734723475976807865E-18, 0.0004981609494469188592, 0.0009963218988938357668 ),
 .UNSPECIFIED. ) ;
#186532 = CARTESIAN_POINT ( 'NONE',  ( 8.516493047678546091, 13.08765898893368629, -0.7998128361456352531 ) ) ;
#186533 = CARTESIAN_POINT ( 'NONE',  ( 0.4609910511476702499, 6.639638261665985475, 3.327981402927758570 ) ) ;
#186534 = CARTESIAN_POINT ( 'NONE',  ( 4.821179601816666604, -1.846891146645711412, -0.9356023351853595127 ) ) ;
#186536 = CARTESIAN_POINT ( 'NONE',  ( 4.019508774049570299, 7.801013956325979493, 0.3192432753683968061 ) ) ;
#186535 = CARTESIAN_POINT ( 'NONE',  ( 0.3097736896383457839, 1.270387085892955792, -1.333027339516623888 ) ) ;
#186537 = CARTESIAN_POINT ( 'NONE',  ( 5.116020035227313301, 0.1674390183682184785, 2.292669612833755810 ) ) ;
#186538 = CARTESIAN_POINT ( 'NONE',  ( 5.165293337126522388, 8.969999960048859577, 1.040834085586084257E-14 ) ) ;
#186540 = CARTESIAN_POINT ( 'NONE',  ( -6.773376349083141790, -7.246166700180801001, -6.661184041420938229 ) ) ;
#186539 = CARTESIAN_POINT ( 'NONE',  ( 4.936577329151614180, 4.931964103531220722, -0.7216878364870458196 ) ) ;
#186541 = CARTESIAN_POINT ( 'NONE',  ( 0.9730957290566042417, -0.06121152481648738097, -2.291606990885884265 ) ) ;
#186542 = CARTESIAN_POINT ( 'NONE',  ( -1.040834085586084257E-14, -9.900000000000005684, -9.579665964948867796 ) ) ;
#186543 = CARTESIAN_POINT ( 'NONE',  ( -6.473091995881817162, 6.516638514809040217, 0.7998128361456281477 ) ) ;
#186544 = CARTESIAN_POINT ( 'NONE',  ( 5.718683143142158087, -0.04558518807709806275, 1.941574535162658544 ) ) ;
#186545 = ORIENTED_EDGE ( 'NONE', *, *, #1351, .T. ) ;
#186546 = CARTESIAN_POINT ( 'NONE',  ( 7.822691444960700125, 10.14955932391940330, -1.443375672974058777 ) ) ;
#186547 = EDGE_CURVE ( 'NONE', #49868, #75305, #190746, .T. ) ;
#186548 = VERTEX_POINT ( 'NONE', #23981 ) ;
#186549 = CARTESIAN_POINT ( 'NONE',  ( -0.08764186210430401081, -2.012836238882615980, -0.04531326932211143105 ) ) ;
#186550 = CARTESIAN_POINT ( 'NONE',  ( 5.190638768449240104, 1.523797776992100061, -1.320824044268428032 ) ) ;
#186552 = CARTESIAN_POINT ( 'NONE',  ( 3.449547071718269020, 5.499999999999998224, -2.024999999999999023 ) ) ;
#186551 = CARTESIAN_POINT ( 'NONE',  ( -7.503547950159405566, 10.84155747757291266, 1.199719254218453823 ) ) ;
#186553 = CARTESIAN_POINT ( 'NONE',  ( 1.642778471875001811, -2.180208332855374742, 2.845375778867859751 ) ) ;
#186555 = CARTESIAN_POINT ( 'NONE',  ( 1.410649291501327118, 1.558696297929580199, 0.8383436984091273692 ) ) ;
#186554 = CARTESIAN_POINT ( 'NONE',  ( 2.308638494240814687, 1.867967618895223447, 0.9389952993345984655 ) ) ;
#186556 = CARTESIAN_POINT ( 'NONE',  ( 6.469375277500488686, -1.978045142091336306, -0.3906011616893814709 ) ) ;
#186558 = CARTESIAN_POINT ( 'NONE',  ( 3.961076342171603315, 0.2821129637899103537, -2.274769079453589526 ) ) ;
#186557 = CARTESIAN_POINT ( 'NONE',  ( 4.923546060418115822, 5.773167154356443120, -1.199719254218452047 ) ) ;
#186559 = CARTESIAN_POINT ( 'NONE',  ( 2.941039689149751890, 0.6260299441606477222, -1.624016774299047228 ) ) ;
#186560 = CARTESIAN_POINT ( 'NONE',  ( 10.05353459973327368, 11.68787744023238417, -1.199719254218440723 ) ) ;
#186561 = TOROIDAL_SURFACE ( 'NONE', #93216, 3.399419719642636561, 0.1000000000000000056 ) ;
#186562 = CARTESIAN_POINT ( 'NONE',  ( -2.680610894905847363, -0.4704162359921021386, -0.1034257855107231783 ) ) ;
#186563 = CARTESIAN_POINT ( 'NONE',  ( 3.145509197426650694, -0.1243275703598344523, -1.729419848027229367 ) ) ;
#186564 = CARTESIAN_POINT ( 'NONE',  ( 3.789651875377809898, -2.007375656734013969, 0.8277776116962390907 ) ) ;
#186565 = CARTESIAN_POINT ( 'NONE',  ( 4.741601036477289810, 6.554953847355395880, 1.599625672291267398 ) ) ;
#186566 = CARTESIAN_POINT ( 'NONE',  ( 4.135954056172497673, 2.015980767636461835, -0.05432360925018697717 ) ) ;
#186567 = CARTESIAN_POINT ( 'NONE',  ( 2.500000000000002220, -1.483785425626877107E-13, -2.052068128417949389 ) ) ;
#186568 = CARTESIAN_POINT ( 'NONE',  ( -1.500000000000013101, 2.202083334016153859, 0.8660254037844403729 ) ) ;
#186569 = CARTESIAN_POINT ( 'NONE',  ( 1.360239512323542010, 0.7782574302275366840, 1.762357998526616232 ) ) ;
#186570 = CARTESIAN_POINT ( 'NONE',  ( -1.500000000000008216, 8.531250000682797818, 3.469446951953614189E-15 ) ) ;
#186571 = CARTESIAN_POINT ( 'NONE',  ( 4.394933515450586192, -2.155188642370196916, -0.5379869938199193236 ) ) ;
#186572 = ORIENTED_EDGE ( 'NONE', *, *, #141701, .F. ) ;
#186573 = CARTESIAN_POINT ( 'NONE',  ( -0.2106854629475037044, 2.877407191259284680, -2.485613835449883346 ) ) ;
#186574 = CARTESIAN_POINT ( 'NONE',  ( -0.7500000000000006661, 1.358333333333357151, -1.299038105676652011 ) ) ;
#186575 = CARTESIAN_POINT ( 'NONE',  ( 5.913327553854682783, 10.05063257947248800, -0.7998128361456291469 ) ) ;
#186576 = CARTESIAN_POINT ( 'NONE',  ( 3.809477975315569864, 7.388215371269402532, -0.7216878364870197293 ) ) ;
#186577 = CARTESIAN_POINT ( 'NONE',  ( -1.642778471874998480, -1.451041666188708446, 2.845375778867863303 ) ) ;
#186578 = CARTESIAN_POINT ( 'NONE',  ( 1.172868535947855673, 0.9048325283492463234, 2.028842389263245227 ) ) ;
#186579 = CARTESIAN_POINT ( 'NONE',  ( 5.371523934717264304, -0.2895824386080196322, 1.940264742196501802 ) ) ;
#186580 = CARTESIAN_POINT ( 'NONE',  ( 10.05978679165993839, 10.83876546646586014, 0.7216878364870438212 ) ) ;
#186581 = AXIS2_PLACEMENT_3D ( 'NONE', #74851, #206963, #108479 ) ;
#186582 = CARTESIAN_POINT ( 'NONE',  ( 0.4138360523464839069, 3.000267424193761467, 2.020124146241416785 ) ) ;
#186583 = CARTESIAN_POINT ( 'NONE',  ( 0.5796411875719498230, 2.017120475678677582, -0.7774783797904263327 ) ) ;
#186584 = CARTESIAN_POINT ( 'NONE',  ( -4.909461021924285795, 6.821066840368686712, 1.443375672974058777 ) ) ;
#186585 = CARTESIAN_POINT ( 'NONE',  ( 3.824720269693319796, -1.387356309220557193, 1.526538889744559313 ) ) ;
#186586 = CARTESIAN_POINT ( 'NONE',  ( -6.417086777969760902, 6.381022750586497594, 0.7998128361456341429 ) ) ;
#186587 = CARTESIAN_POINT ( 'NONE',  ( 0.7499999999999920064, 4.014583334016149863, 1.299038105676669330 ) ) ;
#186588 = CARTESIAN_POINT ( 'NONE',  ( -0.6823417656250212460, 4.863541667008086655, 1.181850606188767472 ) ) ;
#186589 = CARTESIAN_POINT ( 'NONE',  ( 5.149604166610965095, 0.5880212298954893280, -1.775756280894603689 ) ) ;
#186590 = CARTESIAN_POINT ( 'NONE',  ( 4.148821288392518625, 0.8220224570679548481, 1.526945684688446381 ) ) ;
#186591 = CARTESIAN_POINT ( 'NONE',  ( 3.561793593276740388, -1.166016580864630781, 1.292293876973077182 ) ) ;
#186592 = EDGE_CURVE ( 'NONE', #116549, #56116, #38019, .T. ) ;
#186593 = CARTESIAN_POINT ( 'NONE',  ( 1.031297522511119613, -2.069548003639944511, 0.9861895074133855132 ) ) ;
#186594 = CARTESIAN_POINT ( 'NONE',  ( 1.364683531249988535, 4.467708333674754506, -0.7879004041258300672 ) ) ;
#186595 = CARTESIAN_POINT ( 'NONE',  ( 4.036730150552261698, -1.818196258471163729, 1.032062162679239892 ) ) ;
#186596 = CARTESIAN_POINT ( 'NONE',  ( 0.1636598862229492191, -1.205073137261414962, 1.392071761982638378 ) ) ;
#186597 = DIRECTION ( 'NONE',  ( -0.000000000000000000, -1.000000000000000000, -0.000000000000000000 ) ) ;
#186598 = CARTESIAN_POINT ( 'NONE',  ( 1.969375177810539945, -1.978050944945686673, -0.3905967402937361443 ) ) ;
#186599 = CARTESIAN_POINT ( 'NONE',  ( 0.2698121887318750689, 1.265274936352598134, 1.789097752032620114 ) ) ;
#186600 = CARTESIAN_POINT ( 'NONE',  ( 8.063487870853403905, 13.54606852283923857, -8.646108417490655285 ) ) ;
#186601 = CARTESIAN_POINT ( 'NONE',  ( -7.069687034522070590, 10.33538640932937724, -1.199719254218440723 ) ) ;
#186602 = CARTESIAN_POINT ( 'NONE',  ( 7.332262146892202459, 7.448727347662698506, -0.7998128361456281477 ) ) ;
#186603 = CARTESIAN_POINT ( 'NONE',  ( 2.121885542695590487, -0.4617877489709980576, 2.069441001874790409 ) ) ;
#186604 = CARTESIAN_POINT ( 'NONE',  ( -3.090895833791289071, 6.549869539491048442, 1.040834085586084257E-14 ) ) ;
#186606 = EDGE_CURVE ( 'NONE', #29173, #139878, #109591, .T. ) ;
#186605 = CARTESIAN_POINT ( 'NONE',  ( 5.953692858212231265, 0.5253669772854427933, -1.748464709795935157 ) ) ;
#186607 = ORIENTED_EDGE ( 'NONE', *, *, #101175, .T. ) ;
#186608 = CARTESIAN_POINT ( 'NONE',  ( -5.986807348886189040, 9.142303119412650503, -1.199719254218452047 ) ) ;
#186609 = CARTESIAN_POINT ( 'NONE',  ( -0.005641171162459664157, 8.210923785194999880, -2.038653139403752590 ) ) ;
#186610 = CARTESIAN_POINT ( 'NONE',  ( 6.333067150914805765, 9.442309871825708356, 1.082531754730549967 ) ) ;
#186611 = CARTESIAN_POINT ( 'NONE',  ( -3.475000000000000533, -3.835416665710750905, -2.006292185433948827 ) ) ;
#186612 = CARTESIAN_POINT ( 'NONE',  ( -5.533699252672048985, 9.607732894759390518, -0.7998128361456231517 ) ) ;
#186613 = CARTESIAN_POINT ( 'NONE',  ( 1.969016121511291795, -1.558499072447929956, 1.284715733913702085 ) ) ;
#186614 = CARTESIAN_POINT ( 'NONE',  ( 6.106501571484221458, -0.7887142981495840477, -2.061199855587454444 ) ) ;
#186615 = CARTESIAN_POINT ( 'NONE',  ( 10.55232363013785246, 11.20546574478267132, 0.000000000000000000 ) ) ;
#186616 = CARTESIAN_POINT ( 'NONE',  ( 4.030005733973434978, 1.030655172484344684, 1.549249419044882226 ) ) ;
#186617 = CARTESIAN_POINT ( 'NONE',  ( 8.191097360950562845, 12.70803068775103739, -0.7998128361456352531 ) ) ;
#186618 = CARTESIAN_POINT ( 'NONE',  ( -4.906445432736048495, 4.819153361833998339, 0.2530815521472702390 ) ) ;
#186619 = ORIENTED_EDGE ( 'NONE', *, *, #184050, .F. ) ;
#186620 = CARTESIAN_POINT ( 'NONE',  ( -3.958090780185743451, 6.705190779270287393, -1.199719254218452047 ) ) ;
#186621 = CARTESIAN_POINT ( 'NONE',  ( -8.076906825439122528, 10.44614393447756129, -1.599625672291263179 ) ) ;
#186622 = CARTESIAN_POINT ( 'NONE',  ( 5.637271085457097541, -1.648663388651723460, 0.7845467231081537651 ) ) ;
#186624 = CARTESIAN_POINT ( 'NONE',  ( -4.338732707277040745, 7.407397761066524922, -1.160996969951762159 ) ) ;
#186623 = CARTESIAN_POINT ( 'NONE',  ( -4.842197138736131556, 5.678260079060780008, 1.199719254218452935 ) ) ;
#186625 = CARTESIAN_POINT ( 'NONE',  ( -1.402160292154681736E-14, -0.5531249996585814177, -1.575800808251665908 ) ) ;
#186626 = CARTESIAN_POINT ( 'NONE',  ( 0.6140417155099803237, 0.5521904297083098934, -1.643632271941943612 ) ) ;
#186627 = CARTESIAN_POINT ( 'NONE',  ( 0.3216633777232960067, 1.663872621647478622, 0.5102041932069888430 ) ) ;
#186628 = CARTESIAN_POINT ( 'NONE',  ( 5.584705890799654071, -2.250326009109602232, -0.5107660753775817852 ) ) ;
#186629 = CARTESIAN_POINT ( 'NONE',  ( 3.718679271898170491, 7.560485927181699317, 0.7998128361456271485 ) ) ;
#186630 = CARTESIAN_POINT ( 'NONE',  ( 1.229839986812499175, -1.305282058118014010, -1.594721697489847045 ) ) ;
#186631 = CARTESIAN_POINT ( 'NONE',  ( 5.738125327081736060, 7.717565519727259904, 1.599625672291267398 ) ) ;
#186632 = CARTESIAN_POINT ( 'NONE',  ( 6.696599425470320277, -1.493074370650529392, -1.747488531831635550 ) ) ;
#186633 = CARTESIAN_POINT ( 'NONE',  ( -2.760655612144408799, -3.232243495192088201, 1.806370170574614464 ) ) ;
#186634 = CARTESIAN_POINT ( 'NONE',  ( -4.776215253764153346, 8.794277906025310898, -0.7998128361456362523 ) ) ;
#186635 = EDGE_CURVE ( 'NONE', #18108, #184431, #160605, .T. ) ;
#186636 = CARTESIAN_POINT ( 'NONE',  ( 6.209813078548920728, -1.856259414618817383, 0.2309603555875269776 ) ) ;
#186638 = CARTESIAN_POINT ( 'NONE',  ( -4.496464221587651799, 5.274905009054215554, 1.199719254218452935 ) ) ;
#186637 = CARTESIAN_POINT ( 'NONE',  ( 3.673993457511487204, 1.897360377298975553, -0.2389773157873422427 ) ) ;
#186639 = CARTESIAN_POINT ( 'NONE',  ( 4.512475528931441104, -0.9420208833846724916, -1.995868093903986118 ) ) ;
#186640 = CARTESIAN_POINT ( 'NONE',  ( -4.356712336337761644E-14, 2.250000000682782719, -1.414508159514601626 ) ) ;
#186641 = CARTESIAN_POINT ( 'NONE',  ( -7.580882385731773532, -6.105993949506148155, -7.580882385731739781 ) ) ;
#186642 = CARTESIAN_POINT ( 'NONE',  ( 3.838366886000300404, 6.531826229425389485, -1.082531754730548412 ) ) ;
#186643 = CARTESIAN_POINT ( 'NONE',  ( -5.600926855776901192, 5.707038551260711579, -0.7216878364870338292 ) ) ;
#186644 = CARTESIAN_POINT ( 'NONE',  ( 6.111998723603361938, -0.7147493727725148238, 1.996541221815250733 ) ) ;
#186645 = VERTEX_POINT ( 'NONE', #174543 ) ;
#186646 = CARTESIAN_POINT ( 'NONE',  ( 3.311855287401725523, -0.4521268412439309325, 2.262704599374213643 ) ) ;
#186647 = CARTESIAN_POINT ( 'NONE',  ( 3.525789274851616639, 1.914599547803575330, -0.4273510147508317591 ) ) ;
#186648 = CARTESIAN_POINT ( 'NONE',  ( -5.181866634007240791, 6.340624232048664766, 1.284222742053082733 ) ) ;
#186649 = CARTESIAN_POINT ( 'NONE',  ( 0.3210474040165818277, -1.749687966165301312, -0.8873976775175674847 ) ) ;
#186650 = DIRECTION ( 'NONE',  ( 0.000000000000000000, 0.000000000000000000, 1.000000000000000000 ) ) ;
#186651 = CARTESIAN_POINT ( 'NONE',  ( 4.415115299905642665, 5.179997933758551554, -1.199719254218450271 ) ) ;
#186652 = ORIENTED_EDGE ( 'NONE', *, *, #195653, .T. ) ;
#186653 = CARTESIAN_POINT ( 'NONE',  ( 5.858611323429600226, -1.916351766245901977, -0.6279953093112633500 ) ) ;
#186654 = CARTESIAN_POINT ( 'NONE',  ( -9.820183334999905256, 10.35130206712171130, 1.040834085586084257E-14 ) ) ;
#186655 = CARTESIAN_POINT ( 'NONE',  ( 0.2164228883963260908, -0.09351453081237262599, 1.838880455306932227 ) ) ;
#186656 = CARTESIAN_POINT ( 'NONE',  ( 2.641674518982541020, 1.986514366401496590, -0.8763142005700165216 ) ) ;
#186657 = CARTESIAN_POINT ( 'NONE',  ( 0.000000000000000000, -6.893137084989842123, 0.000000000000000000 ) ) ;
#186658 = CARTESIAN_POINT ( 'NONE',  ( 0.9848172835694012361, -1.340914915981223476, 1.642866500755429948 ) ) ;
#186659 = CARTESIAN_POINT ( 'NONE',  ( 1.499999999999989120, 1.306250000682816825, 0.000000000000000000 ) ) ;
#186660 = CARTESIAN_POINT ( 'NONE',  ( 9.541187415715040032, 12.15447128979948310, -1.599625672291262513 ) ) ;
#186661 = CARTESIAN_POINT ( 'NONE',  ( 5.720439131930858956, 7.397432110343761025, 1.315134405782365956 ) ) ;
#186662 = CARTESIAN_POINT ( 'NONE',  ( 0.4739915956469250014, 1.184468288027096694, 1.686179815164081219 ) ) ;
#186664 = CARTESIAN_POINT ( 'NONE',  ( 0.7500000000000006661, 8.447916667349467446, -1.299038105676657340 ) ) ;
#186663 = CARTESIAN_POINT ( 'NONE',  ( -4.296393142825893463, -2.000000000000001776, 4.470011852588161361 ) ) ;
#186665 = CARTESIAN_POINT ( 'NONE',  ( 1.364683531249986537, 1.405208333674755838, -0.7879004041258239610 ) ) ;
#186666 = CARTESIAN_POINT ( 'NONE',  ( -0.05436647835300534304, -9.474608021433725824, -9.500000000000147438 ) ) ;
#186667 = ORIENTED_EDGE ( 'NONE', *, *, #202198, .T. ) ;
#186668 = CARTESIAN_POINT ( 'NONE',  ( 3.949791169003769475, -1.320912084567291034, -1.382976300589415342 ) ) ;
#186669 = CARTESIAN_POINT ( 'NONE',  ( 5.489024251479373895, 1.559478583775832261, -0.8368352093669585434 ) ) ;
#186670 = CARTESIAN_POINT ( 'NONE',  ( 6.333594036239346359, 7.418223126147930557, 1.199719254218453823 ) ) ;
#186671 = CARTESIAN_POINT ( 'NONE',  ( -3.602716132929368875, 5.226254793216122074, 1.599625672291267398 ) ) ;
#186672 = CARTESIAN_POINT ( 'NONE',  ( 0.5096461351858303512, -0.6515609501748579335, 1.690550641884549954 ) ) ;
#186674 = CARTESIAN_POINT ( 'NONE',  ( 1.094790513324794601, 1.691201413147478183, 0.8998118624304138891 ) ) ;
#186673 = CARTESIAN_POINT ( 'NONE',  ( -6.722000117219788073, -7.189371949512781690, 6.713552092916484249 ) ) ;
#186675 = CARTESIAN_POINT ( 'NONE',  ( 2.436061438456170958, 1.271862942251865691, 1.633573898902056731 ) ) ;
#186676 = CARTESIAN_POINT ( 'NONE',  ( -1.402160292154681736E-14, 0.009375000341421267647, -1.575800808251665908 ) ) ;
#186677 = CARTESIAN_POINT ( 'NONE',  ( 0.4441303031895106890, 1.966005183986684335, 0.1476035654904006011 ) ) ;
#186678 = CARTESIAN_POINT ( 'NONE',  ( 2.701551412915685457, -0.5726843992823158480, 1.733614832724015731 ) ) ;
#186680 = CARTESIAN_POINT ( 'NONE',  ( 5.542547785767838242, 7.428594929708664196, 1.247761615041423244 ) ) ;
#186679 = CARTESIAN_POINT ( 'NONE',  ( 0.3116875490984937214, 2.011018277352360606, 1.131832386414432179 ) ) ;
#186681 = CARTESIAN_POINT ( 'NONE',  ( -1.364683531250000748, 0.7593750003414210248, 0.000000000000000000 ) ) ;
#186682 = CARTESIAN_POINT ( 'NONE',  ( 4.686014676054621297, -1.266354490919174403, -1.628128356427221313 ) ) ;
#186683 = CARTESIAN_POINT ( 'NONE',  ( -5.201524489137236529, 9.220195670635433771, 0.7998128361456481317 ) ) ;
#186684 = CARTESIAN_POINT ( 'NONE',  ( 6.916630921265960019, 11.22115317478565188, 0.7998128361456462443 ) ) ;
#186685 = CARTESIAN_POINT ( 'NONE',  ( 3.344057444064992168, 7.053150784717805877, 1.040834085586084257E-14 ) ) ;
#186686 = CARTESIAN_POINT ( 'NONE',  ( 5.952193131599331721, 6.902979060742733708, 1.199719254218462483 ) ) ;
#186688 = CARTESIAN_POINT ( 'NONE',  ( -1.500000000000013101, 3.629166666666692187, -0.8660254037844313801 ) ) ;
#186687 = CARTESIAN_POINT ( 'NONE',  ( 4.805753954608172229, -0.5644290981201576241, 2.028831172856554677 ) ) ;
#186689 = CARTESIAN_POINT ( 'NONE',  ( 6.865700769154306826, -0.4580177224273937475, 2.026514595051785772 ) ) ;
#186690 = CARTESIAN_POINT ( 'NONE',  ( 0.6823417656249899377, 1.405208333674752508, 1.181850606188755259 ) ) ;
#186691 = CARTESIAN_POINT ( 'NONE',  ( 3.515052679271633895, 1.952536648612019921, 0.9277410485990513767 ) ) ;
#186692 = CARTESIAN_POINT ( 'NONE',  ( 4.002606914492294443, -1.998013091498285654, -0.2940530905436929410 ) ) ;
#186693 = CARTESIAN_POINT ( 'NONE',  ( 6.620655732516659064, 2.000981103421325180, 2.575746817850287140 ) ) ;
#186696 = CARTESIAN_POINT ( 'NONE',  ( 5.504247177468175600, 8.405076892812779477, 1.082531754730558626 ) ) ;
#186695 = CARTESIAN_POINT ( 'NONE',  ( 0.000000000000000000, -3.346874999522042149, -3.793834371823813001 ) ) ;
#186694 = DIRECTION ( 'NONE',  ( 0.000000000000000000, -1.000000000000000000, 0.000000000000000000 ) ) ;
#186697 = CARTESIAN_POINT ( 'NONE',  ( -4.606738333593328072, 8.596554832492683929, 0.7998128361456281477 ) ) ;
#186698 = CARTESIAN_POINT ( 'NONE',  ( 2.764861550476094276, -0.1531697945360478985, -2.010801143277194392 ) ) ;
#186699 = CARTESIAN_POINT ( 'NONE',  ( -5.689618019229208734, 9.789638122409414223, 0.7998128361456481317 ) ) ;
#186701 = CARTESIAN_POINT ( 'NONE',  ( 1.945152801660263719, 0.4725272983826271367, 0.7134944055886273118 ) ) ;
#186700 = CARTESIAN_POINT ( 'NONE',  ( -3.469997250093771246, 6.135748327496311383, -1.199719254218452935 ) ) ;
#186702 = LINE ( 'NONE', #4723, #32348 ) ;
#186703 = CARTESIAN_POINT ( 'NONE',  ( 5.748291730981217817, 0.9368611416523885405, -1.667099895225135686 ) ) ;
#186704 = CARTESIAN_POINT ( 'NONE',  ( 6.992767129439140028, -7.336076765398686028, 7.649321060469624456 ) ) ;
#186706 = CARTESIAN_POINT ( 'NONE',  ( 4.077750037130567939, -0.7691059624741981571, 1.864175985064358665 ) ) ;
#186705 = CARTESIAN_POINT ( 'NONE',  ( -8.961576348508655698, 9.557519949455999253, -0.7216878364870267237 ) ) ;
#186707 = CARTESIAN_POINT ( 'NONE',  ( -1.499999999999997780, 5.400000000000022560, 1.214306433183764966E-14 ) ) ;
#186708 = CARTESIAN_POINT ( 'NONE',  ( -1.364683531250010295, 8.380208333674730170, 0.7879004041258445001 ) ) ;
#186709 = CARTESIAN_POINT ( 'NONE',  ( 6.598688221398479214, -0.4661808427693337475, -1.660524940999157373 ) ) ;
#186710 = CARTESIAN_POINT ( 'NONE',  ( 5.387385936583818591, 7.378645907471495846, -1.599625672291283607 ) ) ;
#186712 = CARTESIAN_POINT ( 'NONE',  ( -6.082945924897037671, 5.998665437213099416, -0.3423739784766628991 ) ) ;
#186711 = CARTESIAN_POINT ( 'NONE',  ( 9.408995418203971894, 11.03987807840189816, 1.082531754730549967 ) ) ;
#186713 =( GEOMETRIC_REPRESENTATION_CONTEXT ( 3 ) GLOBAL_UNCERTAINTY_ASSIGNED_CONTEXT ( ( #118722 ) ) GLOBAL_UNIT_ASSIGNED_CONTEXT ( ( #2030, #166705, #68099 ) ) REPRESENTATION_CONTEXT ( 'NONE', 'WORKASPACE' ) );
#186714 = CARTESIAN_POINT ( 'NONE',  ( -3.863710589770277259, 6.491117540498504646, 1.082531754730560403 ) ) ;
#186715 = CARTESIAN_POINT ( 'NONE',  ( 5.483624757375023862, 1.255567903217995829, 1.386730702750748945 ) ) ;
#186716 = CARTESIAN_POINT ( 'NONE',  ( 6.486586620031766337, -1.235515937849906321, 1.590312944162165287 ) ) ;
#186717 = DIRECTION ( 'NONE',  ( -5.551115123125765446E-17, 0.000000000000000000, 1.000000000000000000 ) ) ;
#186718 = CARTESIAN_POINT ( 'NONE',  ( 1.868117093089691538, -2.055091939184821026, 0.2493290443424806546 ) ) ;
#186719 = CARTESIAN_POINT ( 'NONE',  ( -5.926322542504860458, 9.928143709648733051, -0.7216878364870338292 ) ) ;
#186720 = EDGE_LOOP ( 'NONE', ( #107717, #106341, #165427, #60477, #122689, #176237 ) ) ;
#186721 = CARTESIAN_POINT ( 'NONE',  ( 9.205623113554612047, 12.72334881824701469, 1.082531754730546636 ) ) ;
#186722 = CARTESIAN_POINT ( 'NONE',  ( 0.6148615108944045504, 0.1511614643284354409, 2.010825953887733775 ) ) ;
#186723 = CARTESIAN_POINT ( 'NONE',  ( 1.195247182365884564, 1.673216051897677747, -0.6948750315247439469 ) ) ;
#186724 = CARTESIAN_POINT ( 'NONE',  ( 3.377389663135653031, 6.954388683717978026, -0.7216878364870338292 ) ) ;
#186725 = DIRECTION ( 'NONE',  ( 0.000000000000000000, 0.000000000000000000, 1.000000000000000000 ) ) ;
#186726 = EDGE_CURVE ( 'NONE', #60692, #166808, #93292, .T. ) ;
#186727 = PRODUCT_RELATED_PRODUCT_CATEGORY ( 'part', '', ( #67584 ) ) ;
#186728 = CARTESIAN_POINT ( 'NONE',  ( 7.361714222096048310, 10.57212177821199184, -1.082531754730537976 ) ) ;
#186729 = CIRCLE ( 'NONE', #58724, 0.05000000000000007910 ) ;
#186730 = CARTESIAN_POINT ( 'NONE',  ( 8.274553823041976841, 8.548067636504127265, 1.040834085586084257E-14 ) ) ;
#186732 = CARTESIAN_POINT ( 'NONE',  ( 6.433208386744649232, -1.541796563146474286, -1.136648034191472645 ) ) ;
#186731 = CARTESIAN_POINT ( 'NONE',  ( -6.043183783389232566, 8.073467052085995022, 1.599625672291269396 ) ) ;
#186733 = CARTESIAN_POINT ( 'NONE',  ( -1.201851678989727383E-14, 5.087500000000019007, -1.732050807568863648 ) ) ;
#186734 = CARTESIAN_POINT ( 'NONE',  ( -11.48243876534946040, 13.88000000000000078, -3.200000000000001510 ) ) ;
#186735 = CARTESIAN_POINT ( 'NONE',  ( 7.104109303436412226, 7.390475063538369582, 1.040834085586084257E-14 ) ) ;
#186736 = CARTESIAN_POINT ( 'NONE',  ( -1.364683531250014514, -0.6989583329919100141, -0.7879004041258359514 ) ) ;
#186738 = EDGE_LOOP ( 'NONE', ( #144682, #88619, #210304, #53972 ) ) ;
#186737 = CARTESIAN_POINT ( 'NONE',  ( 2.711267533052988732, 6.106969855296372707, -0.7216878364870267237 ) ) ;
#186739 = CARTESIAN_POINT ( 'NONE',  ( -2.449219305563052895, 6.009172956465517856, 1.040834085586084257E-14 ) ) ;
#186740 = CARTESIAN_POINT ( 'NONE',  ( 2.483474991488154870, 1.976725341044349271, -0.8753317036461552014 ) ) ;
#186741 = CARTESIAN_POINT ( 'NONE',  ( -4.981695098378565945, 4.776675467721892332, -0.7998128361456362523 ) ) ;
#186742 = CARTESIAN_POINT ( 'NONE',  ( 6.536439455564168277, 6.798469917679251573, 0.7216878364870328300 ) ) ;
#186743 = CARTESIAN_POINT ( 'NONE',  ( 0.7562902151678205787, 0.8540304730459827853, -1.941197329821432227 ) ) ;
#186744 = CARTESIAN_POINT ( 'NONE',  ( 5.262654937129007671, -1.321179299781930938, 1.260103332352560779 ) ) ;
#186745 = EDGE_CURVE ( 'NONE', #129277, #92086, #195293, .T. ) ;
#186746 = CARTESIAN_POINT ( 'NONE',  ( 1.792193567899300177, -1.961476155570774926, -0.1973719964898524026 ) ) ;
#186747 = CARTESIAN_POINT ( 'NONE',  ( 4.588094604188536429, 1.105678411722615051, 1.560157546714964871 ) ) ;
#186748 = ORIENTED_EDGE ( 'NONE', *, *, #155670, .F. ) ;
#186749 = CARTESIAN_POINT ( 'NONE',  ( 6.875078400183573635, 7.629137130509068498, 2.744348168701661095 ) ) ;
#186750 = CARTESIAN_POINT ( 'NONE',  ( 4.598083368088573764, 0.8440023354334601491, -1.779705283501178181 ) ) ;
#186751 = CARTESIAN_POINT ( 'NONE',  ( 0.4275465750286939204, 0.9991681100989335818, -1.665045846455282863 ) ) ;
#186752 = ORIENTED_EDGE ( 'NONE', *, *, #31970, .T. ) ;
#186753 = CARTESIAN_POINT ( 'NONE',  ( -6.473091995881817162, 6.516638514809040217, 0.7998128361456281477 ) ) ;
#186754 = CARTESIAN_POINT ( 'NONE',  ( -7.919371124158132602, 8.411890197705517380, -0.7216878364870338292 ) ) ;
#186756 = CARTESIAN_POINT ( 'NONE',  ( 4.543390873910894356, 8.314723429622471684, 0.7216878364870317197 ) ) ;
#186755 = CARTESIAN_POINT ( 'NONE',  ( 7.796102023057898123, 9.054206100777749455, -1.199719254218441611 ) ) ;
#186757 = CARTESIAN_POINT ( 'NONE',  ( 5.004515039866801906, -1.898294113557968510, -0.2302225566794338651 ) ) ;
#186758 = CARTESIAN_POINT ( 'NONE',  ( 0.8685540286928780107, 1.089157903960279672, 1.919174906450902274 ) ) ;
#186759 = CARTESIAN_POINT ( 'NONE',  ( 1.458525620005609147, 8.740196138359117128, 2.548959422810368913 ) ) ;
#186760 = CARTESIAN_POINT ( 'NONE',  ( 6.059245300855401695, -1.699386736952392285, 1.078915776541150340 ) ) ;
#186761 = CYLINDRICAL_SURFACE ( 'NONE', #210658, 1.250000000000000000 ) ;
#186762 = CARTESIAN_POINT ( 'NONE',  ( -5.337312369484060071, 7.713579007861619985, 1.331290254527866201 ) ) ;
#186763 = DIRECTION ( 'NONE',  ( -0.9999980456341538426, 0.000000000000000000, -0.001977050295949311660 ) ) ;
#186764 = CARTESIAN_POINT ( 'NONE',  ( 2.717306809760032138, -1.800131872397674471, -1.022606600864908621 ) ) ;
#186765 = CARTESIAN_POINT ( 'NONE',  ( -5.215082642750900277, 9.236013516518044142, 0.000000000000000000 ) ) ;
#186766 = CARTESIAN_POINT ( 'NONE',  ( -4.764376198328064582, 8.188698463893414825, 0.7498042881181687935 ) ) ;
#186768 = CARTESIAN_POINT ( 'NONE',  ( 0.5675189469334164238, 0.2105291993744831114, -2.151437729447757796 ) ) ;
#186767 = CARTESIAN_POINT ( 'NONE',  ( -4.090809663021341969, 5.795697244990093644, 1.599625672291267398 ) ) ;
#186769 = CARTESIAN_POINT ( 'NONE',  ( -11.81451294207098179, 8.720850203416988577, 2.122579420461416344 ) ) ;
#186770 = CARTESIAN_POINT ( 'NONE',  ( 3.431622278034673901, 7.017660067766835930, -1.734723475976807094E-15 ) ) ;
#186771 = CARTESIAN_POINT ( 'NONE',  ( 0.1062647697984270417, -6.683951901172196841, 9.488025208946959665 ) ) ;
#186772 = VECTOR ( 'NONE', #179084, 1000.000000000000000 ) ;
#186773 = CARTESIAN_POINT ( 'NONE',  ( 0.6823417656249934904, 13.00520833367473017, 1.181850606188764807 ) ) ;
#186775 = CARTESIAN_POINT ( 'NONE',  ( -5.173318132066234476, 8.193232366456022930, -1.199719254218453823 ) ) ;
#186774 = CARTESIAN_POINT ( 'NONE',  ( 6.925078400183550364, 4.698656493127392864, 2.418320467900983761 ) ) ;
#186776 = CARTESIAN_POINT ( 'NONE',  ( 4.342224273253515676, 0.3742292800460333413, -1.693095411864028677 ) ) ;
#186777 = CARTESIAN_POINT ( 'NONE',  ( -2.442440228756222353, 6.001264033524212671, -0.7998128361456281477 ) ) ;
#186778 = CARTESIAN_POINT ( 'NONE',  ( 3.608316154870555792, 2.070434559819031684, 0.004826415812286819970 ) ) ;
#186779 = CARTESIAN_POINT ( 'NONE',  ( 5.009417666957850734, -2.010078760914670859, 0.6651486602928055047 ) ) ;
#186781 = CARTESIAN_POINT ( 'NONE',  ( 6.317209508963599340, 9.457495962844502557, 1.199719254218462483 ) ) ;
#186780 = B_SPLINE_CURVE_WITH_KNOTS ( 'NONE', 3,
 ( #119329, #136597, #120408, #38020, #186383, #149637, #204750 ),
 .UNSPECIFIED., .F., .F.,
 ( 4, 3, 4 ),
 ( 0.000000000000000000, 2.757963454290271384E-05, 5.739065715766676189E-05 ),
 .UNSPECIFIED. ) ;
#186782 = CARTESIAN_POINT ( 'NONE',  ( -0.6823417656249969321, 4.717708333674755394, -1.181850606188749264 ) ) ;
#186783 = CARTESIAN_POINT ( 'NONE',  ( 2.307411487444132270, -1.578694758215667404, -1.177220170345204098 ) ) ;
#186784 = CARTESIAN_POINT ( 'NONE',  ( 0.8614045922798494459, -1.509235727096858826, -1.174430983434850972 ) ) ;
#186785 = CARTESIAN_POINT ( 'NONE',  ( 4.347812307665041232, 2.291787294364412642, -0.05403505903618135986 ) ) ;
#186786 = CARTESIAN_POINT ( 'NONE',  ( 2.314841291766779108, 1.630546960418734148, 0.8213866120303781049 ) ) ;
#186787 = CARTESIAN_POINT ( 'NONE',  ( 4.583538449871731757, 7.505156070562471804, 1.199719254218451159 ) ) ;
#186788 = CARTESIAN_POINT ( 'NONE',  ( 6.277061933002785032, 7.385955679000473673, 1.082531754730558626 ) ) ;
#186789 = CARTESIAN_POINT ( 'NONE',  ( -8.453672473320708036, 9.821371626084353323, -1.199719254218446718 ) ) ;
#186790 = CARTESIAN_POINT ( 'NONE',  ( 2.918229521859570408, -2.010703624536396728, 0.1031290223681199103 ) ) ;
#186791 = CARTESIAN_POINT ( 'NONE',  ( 3.450005804356533812, -0.7992637590314204399, 1.791754569076028147 ) ) ;
#186792 = CARTESIAN_POINT ( 'NONE',  ( -6.008234629150358330, 10.16135750065076060, 0.000000000000000000 ) ) ;
#186793 = CARTESIAN_POINT ( 'NONE',  ( -5.168682875307782254, 7.053215992657626110, -1.599625672291256295 ) ) ;
#186794 = CARTESIAN_POINT ( 'NONE',  ( 0.07556134207191073093, 7.629137130509040077, -2.844199257382596269 ) ) ;
#186796 = CARTESIAN_POINT ( 'NONE',  ( 4.821055670345097077, -0.08498437303107277130, 1.767940285534306488 ) ) ;
#186795 = CARTESIAN_POINT ( 'NONE',  ( 6.035123006257053113, -1.513425687198214353, -1.442577094899047063 ) ) ;
#186797 = CARTESIAN_POINT ( 'NONE',  ( 4.905139262582266291, 4.827437033166341429, 0.6004564335717228474 ) ) ;
#186798 = CARTESIAN_POINT ( 'NONE',  ( 0.6565081633774123571, -1.584678946828571133, 1.513927167823600595 ) ) ;
#186799 = CARTESIAN_POINT ( 'NONE',  ( 6.404260164931634414, 1.284261220195097808, -1.174706115135275342 ) ) ;
#186800 = CARTESIAN_POINT ( 'NONE',  ( 6.775324078527185989, 8.927630729746953264, -1.599625672291262513 ) ) ;
#186801 = CARTESIAN_POINT ( 'NONE',  ( -5.777182852754558340, 5.912670547734647286, 0.000000000000000000 ) ) ;
#186802 = CARTESIAN_POINT ( 'NONE',  ( 0.2811772945982879968, -2.253408246774822210, 0.4517706223704387458 ) ) ;
#186803 = CARTESIAN_POINT ( 'NONE',  ( 2.972313222866368676, 6.545497292499366182, 0.5012468031770876964 ) ) ;
#186804 = CARTESIAN_POINT ( 'NONE',  ( 6.292339289836506033, -1.631180892843343999, 0.5882027141154468897 ) ) ;
#186805 = CARTESIAN_POINT ( 'NONE',  ( 1.735297346119796691, 0.2185962045802778420, 2.196029071591873993 ) ) ;
#186806 = AXIS2_PLACEMENT_3D ( 'NONE', #172751, #90434, #206292 ) ;
#186807 = CARTESIAN_POINT ( 'NONE',  ( 0.6554289830566867314, 1.805916262795668192, -1.204791683884984810 ) ) ;
#186808 = DIRECTION ( 'NONE',  ( -1.000000000000000000, -0.000000000000000000, -0.000000000000000000 ) ) ;
#186809 = CARTESIAN_POINT ( 'NONE',  ( 1.077539098219507663, 1.607448503539260054, 1.378281722515703800 ) ) ;
#186810 = CARTESIAN_POINT ( 'NONE',  ( 4.000000000000002665, -2.278188019141646974E-13, -2.052068128417946280 ) ) ;
#186811 = CARTESIAN_POINT ( 'NONE',  ( 6.727182134110219813, 2.036943547479725058, 2.394510323907019345 ) ) ;
#186812 = CARTESIAN_POINT ( 'NONE',  ( 4.735331810261827812, -1.761409202268785057, 0.7803939243795944281 ) ) ;
#186813 = ORIENTED_EDGE ( 'NONE', *, *, #48845, .F. ) ;
#186815 = CARTESIAN_POINT ( 'NONE',  ( -0.7499999999999972244, 5.108333333333353821, -1.299038105676652011 ) ) ;
#186814 = CARTESIAN_POINT ( 'NONE',  ( 1.734309787148346382, 2.268178062924830041, 0.3313793973579847729 ) ) ;
#186816 = CARTESIAN_POINT ( 'NONE',  ( 3.960953433486789521, 7.772862772376584850, -0.7998128361456221525 ) ) ;
#186817 = CARTESIAN_POINT ( 'NONE',  ( 5.035963992472171746, 7.962709526937818083, 1.199719254218462483 ) ) ;
#186818 = CARTESIAN_POINT ( 'NONE',  ( 4.283969606688295961, 2.154612580813870082, -0.5396949931109666920 ) ) ;
#186819 = CARTESIAN_POINT ( 'NONE',  ( -7.537970219518066450, 11.73812298950569044, -0.7216878364870267237 ) ) ;
#186820 = DIRECTION ( 'NONE',  ( 0.000000000000000000, 0.000000000000000000, 1.000000000000000000 ) ) ;
#186821 = CARTESIAN_POINT ( 'NONE',  ( 6.643132081016117851, 8.773406732650713025, 1.443375672974076540 ) ) ;
#186822 = CARTESIAN_POINT ( 'NONE',  ( -8.663296969008007054, 9.209527340038563992, 0.7216878364870438212 ) ) ;
#186823 = CARTESIAN_POINT ( 'NONE',  ( 4.746763178560241769, 8.551991118380046331, 0.7216878364870328300 ) ) ;
#186824 = VERTEX_POINT ( 'NONE', #175597 ) ;
#186825 = CARTESIAN_POINT ( 'NONE',  ( 1.512342498431101134, -1.897697209584522815, 0.6819976561535444626 ) ) ;
#186827 = CARTESIAN_POINT ( 'NONE',  ( 0.2685208109398624088, -0.8776176662104094861, -1.864379643416124166 ) ) ;
#186826 = CARTESIAN_POINT ( 'NONE',  ( 8.911787042884274257, 9.291506392986812912, 0.7998128361456462443 ) ) ;
#186828 = CARTESIAN_POINT ( 'NONE',  ( -10.99968117833243220, -6.698521824825906634, 0.09510031644099410653 ) ) ;
#186829 = CARTESIAN_POINT ( 'NONE',  ( 6.821160681006793070, 7.130644680695653825, 0.7216878364870328300 ) ) ;
#186830 = CARTESIAN_POINT ( 'NONE',  ( 0.1164230846485321547, -0.09151219166612066525, 1.839079034809627755 ) ) ;
#186831 = CARTESIAN_POINT ( 'NONE',  ( -0.6823417656250212460, 2.051041667008083991, 1.181850606188767472 ) ) ;
#186832 = CARTESIAN_POINT ( 'NONE',  ( 1.475481261428980506, 1.048764899322068622, 1.425360520505250417 ) ) ;
#186833 = CARTESIAN_POINT ( 'NONE',  ( 0.08851783505585240908, -0.5350849913869708541, 1.944072358963434555 ) ) ;
#186834 = CARTESIAN_POINT ( 'NONE',  ( 0.04610459085982108324, -1.479553692838073475, 1.095721268101347734 ) ) ;
#186835 = CARTESIAN_POINT ( 'NONE',  ( 4.036908492867667064, -1.994400080153370558, 1.130107982421886481 ) ) ;
#186836 = CARTESIAN_POINT ( 'NONE',  ( 3.802549092506895878, 1.579937072410386278, 0.9450539169142122553 ) ) ;
#186837 = CARTESIAN_POINT ( 'NONE',  ( 9.097684769969825780, 10.57271930550834860, -1.199719254218446718 ) ) ;
#186838 = CARTESIAN_POINT ( 'NONE',  ( 0.000000000000000000, 15.00000000000000000, -12.00000000000000178 ) ) ;
#186839 = CARTESIAN_POINT ( 'NONE',  ( 4.102439050647597618, -0.5725816820084869141, -1.733541218493547476 ) ) ;
#186840 = CARTESIAN_POINT ( 'NONE',  ( 4.570935502227962743, -0.9480417383296577682, 1.779625852769652905 ) ) ;
#186841 = CARTESIAN_POINT ( 'NONE',  ( -10.50487009249003378, 11.15010328419353947, 0.7998128361456462443 ) ) ;
#186843 = CARTESIAN_POINT ( 'NONE',  ( -5.935437387732586778, 10.14670372898850381, -0.7998128361456362523 ) ) ;
#186842 = CARTESIAN_POINT ( 'NONE',  ( 3.555803421180541157, 0.5519491744547943002, -2.194038648399123215 ) ) ;
#186844 = CARTESIAN_POINT ( 'NONE',  ( 0.1707221987203759173, -1.373943582462642921, 1.596272430080846405 ) ) ;
#186845 = CARTESIAN_POINT ( 'NONE',  ( 11.78331023100045627, 9.719999999999982876, 1.799999999999999600 ) ) ;
#186846 = CARTESIAN_POINT ( 'NONE',  ( 4.053231837324381637, 1.750648263899981849, -1.104974720517466480 ) ) ;
#186847 = CARTESIAN_POINT ( 'NONE',  ( 9.622536337397022521, 12.24937836509514710, 1.599625672291281386 ) ) ;
#186848 = CARTESIAN_POINT ( 'NONE',  ( 0.6801582343749900117, 1.338541667008072533, -1.178068619123872729 ) ) ;
#186849 = CARTESIAN_POINT ( 'NONE',  ( 5.742871283745087041, 2.043606947765171267, 0.5656136300068030920 ) ) ;
#186850 = CONTEXT_DEPENDENT_SHAPE_REPRESENTATION ( #184765, #28111 ) ;
#186853 = EDGE_CURVE ( 'NONE', #170487, #98224, #207002, .T. ) ;
#186852 = CARTESIAN_POINT ( 'NONE',  ( 2.314956460678399885, 1.720770591318865339, 0.8663633404912238767 ) ) ;
#186851 = CARTESIAN_POINT ( 'NONE',  ( -8.479735010343349089, 11.98044238112085758, 1.199719254218453823 ) ) ;
#186854 = FACE_OUTER_BOUND ( 'NONE', #13225, .T. ) ;
#186855 = CARTESIAN_POINT ( 'NONE',  ( 6.561384255921438147, 1.635440365473137536, 1.096959908523033711 ) ) ;
#186856 = CARTESIAN_POINT ( 'NONE',  ( 4.787437638956922648, 6.678706226906775179, -1.443375672974068769 ) ) ;
#186857 = CARTESIAN_POINT ( 'NONE',  ( 5.407503677813131127, 6.286683671216334091, 1.048937882774292785 ) ) ;
#186858 = FACE_OUTER_BOUND ( 'NONE', #70444, .T. ) ;
#186859 = CARTESIAN_POINT ( 'NONE',  ( -3.242371291962510504, 6.934516940598226320, 1.040834085586084257E-14 ) ) ;
#186860 = CARTESIAN_POINT ( 'NONE',  ( 0.2467152807458715680, 1.134915856054707906, -1.909484979926486137 ) ) ;
#186861 = CARTESIAN_POINT ( 'NONE',  ( 3.592891271941214271, -0.4089703316215765883, -2.065685861495478726 ) ) ;
#186862 = CARTESIAN_POINT ( 'NONE',  ( -4.462568837553487100, 5.235360394347691404, -1.199719254218453823 ) ) ;
#186863 = CARTESIAN_POINT ( 'NONE',  ( 7.233438648090761980, 8.397765496649418182, 1.199719254218462483 ) ) ;
#186864 = CARTESIAN_POINT ( 'NONE',  ( 0.6778921365368529850, -0.9907528278601520633, -1.575212976145045518 ) ) ;
#186865 = CARTESIAN_POINT ( 'NONE',  ( 7.461064606222022277, 7.598996883547496139, 1.040834085586084257E-14 ) ) ;
#186866 = CARTESIAN_POINT ( 'NONE',  ( 4.660252114795294887, 6.460046772059735432, -1.599625672291256295 ) ) ;
#186867 = CARTESIAN_POINT ( 'NONE',  ( -5.966997003790221576, 9.015228033513643879, -1.082531754730549967 ) ) ;
#186868 = CARTESIAN_POINT ( 'NONE',  ( 1.389100911873580646, -2.015333191458138273, -0.6601287711371638389 ) ) ;
#186869 = CARTESIAN_POINT ( 'NONE',  ( -5.725286006720766707, 9.901527117808042178, 0.7998128361456291469 ) ) ;
#186871 = CARTESIAN_POINT ( 'NONE',  ( 3.121486724888074882, 0.2905151309811822569, -1.940125473959073421 ) ) ;
#186870 = CARTESIAN_POINT ( 'NONE',  ( 0.6124999999999776179, 0.6666666666666626329, -1.060881119635955327 ) ) ;
#186872 = CARTESIAN_POINT ( 'NONE',  ( 2.290102563249151402, -0.9248296759884739870, 1.954025333243500917 ) ) ;
#186873 = CARTESIAN_POINT ( 'NONE',  ( 2.190726087351921425, 1.424366561657765207, 1.166803476217087576 ) ) ;
#186875 = CARTESIAN_POINT ( 'NONE',  ( -4.932901803036217281, 6.667582871412107259, -1.248097486420626900 ) ) ;
#186874 = DIRECTION ( 'NONE',  ( -0.000000000000000000, -1.000000000000000000, -0.000000000000000000 ) ) ;
#186876 = CARTESIAN_POINT ( 'NONE',  ( 4.048569170814999119, -1.448435850583905671, -0.9644227198624519826 ) ) ;
#186877 = CARTESIAN_POINT ( 'NONE',  ( 6.344852701515477200, 6.504675694630598137, -0.7216878364870257245 ) ) ;
#186878 = CARTESIAN_POINT ( 'NONE',  ( -10.05278092738192619, 5.876216011288541985, -5.831672646394378212 ) ) ;
#186879 = CARTESIAN_POINT ( 'NONE',  ( 0.8839147992780393981, 1.452536163361785260, 1.601146772000871188 ) ) ;
#186880 = CARTESIAN_POINT ( 'NONE',  ( 3.181017370561005198, -0.9912469002804729090, -1.755500664876320727 ) ) ;
#186881 = CARTESIAN_POINT ( 'NONE',  ( -10.45297324601190425, 11.29748299654313470, 0.7216878364870438212 ) ) ;
#186882 = CARTESIAN_POINT ( 'NONE',  ( -4.604929450496978660, 5.401447776115099408, -1.199719254218453823 ) ) ;
#186883 = EDGE_CURVE ( 'NONE', #115502, #16328, #132941, .T. ) ;
#186884 = CARTESIAN_POINT ( 'NONE',  ( 3.537922462266992252, 0.8877721971902104992, -1.760348037230663021 ) ) ;
#186885 = CARTESIAN_POINT ( 'NONE',  ( 6.609000000000036401, 1.265604115953523845, 2.115306440354140172 ) ) ;
#186886 = CARTESIAN_POINT ( 'NONE',  ( 2.735803960117746403, 1.927664933923057600, 0.2353960755621438972 ) ) ;
#186889 = ORIENTED_EDGE ( 'NONE', *, *, #133466, .T. ) ;
#186888 = CARTESIAN_POINT ( 'NONE',  ( -4.746763178560296836, 6.631252689777363152, 1.443375672974058777 ) ) ;
#186887 = CARTESIAN_POINT ( 'NONE',  ( -11.04536101718726293, 10.19999999999999929, 1.099999999999996758 ) ) ;
#186890 = CARTESIAN_POINT ( 'NONE',  ( -5.004368096775595021, 5.971422546727199077, 1.082531754730549078 ) ) ;
#186891 = CARTESIAN_POINT ( 'NONE',  ( -0.2108831679770924727, 4.091978752061476321, -2.452067053820900622 ) ) ;
#186892 = CARTESIAN_POINT ( 'NONE',  ( 4.199993725183334803, 8.122019456014369254, -0.7998128361456362523 ) ) ;
#186893 = CARTESIAN_POINT ( 'NONE',  ( -6.466312919074983512, 6.508729591867735031, -0.7998128361456362523 ) ) ;
#186894 = CARTESIAN_POINT ( 'NONE',  ( -5.433785704026946384, 9.561443431331920095, 0.000000000000000000 ) ) ;
#186895 = DIRECTION ( 'NONE',  ( 0.000000000000000000, 0.000000000000000000, 1.000000000000000000 ) ) ;
#186896 = CARTESIAN_POINT ( 'NONE',  ( 6.458097596740710600, 2.302054065074070177, -0.1608065221961554325 ) ) ;
#186897 = DIRECTION ( 'NONE',  ( 0.000000000000000000, -1.000000000000000000, 0.000000000000000000 ) ) ;
#186898 = CARTESIAN_POINT ( 'NONE',  ( 4.434394140398959294, -1.132915509570767476, 1.601352629973289199 ) ) ;
#186899 = CARTESIAN_POINT ( 'NONE',  ( 7.151035956204054855, 10.43029348462504124, 1.199719254218460707 ) ) ;
#186900 = CARTESIAN_POINT ( 'NONE',  ( 2.268204128460939550, 1.842446992372799963, -0.8197738674571022344 ) ) ;
#186901 = ORIENTED_EDGE ( 'NONE', *, *, #149694, .T. ) ;
#186902 = CARTESIAN_POINT ( 'NONE',  ( 2.026704517097451586, 0.4691240347775883501, 2.064561701657470660 ) ) ;
#186903 = CARTESIAN_POINT ( 'NONE',  ( -1.500000000000001332, 1.431250000682816825, 0.000000000000000000 ) ) ;
#186905 = CARTESIAN_POINT ( 'NONE',  ( -6.552668314106420588, 6.539201209412602189, -0.7998128361456291469 ) ) ;
#186904 = CARTESIAN_POINT ( 'NONE',  ( -3.216308754939891212, 4.775446185561722956, -1.599625672291262513 ) ) ;
#186906 = CARTESIAN_POINT ( 'NONE',  ( 3.327899939431624876, 1.796474422365784029, 0.4023406486387756664 ) ) ;
#186907 = ORIENTED_EDGE ( 'NONE', *, *, #84677, .T. ) ;
#186908 = CARTESIAN_POINT ( 'NONE',  ( -8.676328237741483207, 12.20980114641871062, -1.199719254218446718 ) ) ;
#186909 = DIRECTION ( 'NONE',  ( 1.000000000000000000, -0.000000000000000000, -0.000000000000000000 ) ) ;
#186910 = CARTESIAN_POINT ( 'NONE',  ( 4.183913158364858553, 2.056144659531285779, -0.5182805708664262045 ) ) ;
#186911 = CARTESIAN_POINT ( 'NONE',  ( 0.7086343398283838635, -0.2726298849291541870, 1.820711063333625646 ) ) ;
#186912 = LINE ( 'NONE', #102473, #211997 ) ;
#186913 = CARTESIAN_POINT ( 'NONE',  ( 7.284808609244363353, 7.393364887073558656, 0.7998128361456341429 ) ) ;
#186914 = B_SPLINE_CURVE_WITH_KNOTS ( 'NONE', 3,
 ( #198437, #37013, #184324, #2356, #83633, #16485, #68432, #66290, #148652, #50083 ),
 .UNSPECIFIED., .F., .F.,
 ( 4, 3, 3, 4 ),
 ( 0.000000000000000000, 8.893179197954873439E-05, 0.0001334007970840211997, 0.0001778705873659022839 ),
 .UNSPECIFIED. ) ;
#186915 = CARTESIAN_POINT ( 'NONE',  ( 4.481748981177747559, 1.343215529357727478, 1.562995469165892493 ) ) ;
#186916 = PRESENTATION_LAYER_ASSIGNMENT (  '', '', ( #52108 ) ) ;
#186918 = CARTESIAN_POINT ( 'NONE',  ( 1.100829259350871281, -0.4471758257712907247, 1.786007343351428966 ) ) ;
#186917 = CARTESIAN_POINT ( 'NONE',  ( -5.879432169820529630, 10.01108796476595764, -0.7998128361456221525 ) ) ;
#186919 = CARTESIAN_POINT ( 'NONE',  ( -0.6823417656250212460, 5.551041667008087543, 1.181850606188767472 ) ) ;
#186920 = FILL_AREA_STYLE_COLOUR ( '', #84143 ) ;
#186921 = DIRECTION ( 'NONE',  ( 1.000000000000000000, -0.000000000000000000, -0.000000000000000000 ) ) ;
#186922 = CARTESIAN_POINT ( 'NONE',  ( 10.99873804690151147, -8.265528217051443249, -0.1803058380980962216 ) ) ;
#186923 = CARTESIAN_POINT ( 'NONE',  ( 1.735297346119796691, 0.2185962045802778420, 2.196029071591873993 ) ) ;
#186924 = CARTESIAN_POINT ( 'NONE',  ( 3.884249253383244227, -1.119368145229171052, 1.966044450452981929 ) ) ;
#186925 = CARTESIAN_POINT ( 'NONE',  ( -8.378575743565381373, 8.877352577022161739, 0.7216878364870438212 ) ) ;
#186926 = CARTESIAN_POINT ( 'NONE',  ( 4.130988372668517705, 1.658889437441883441, 0.7283703743019008803 ) ) ;
#186927 = CARTESIAN_POINT ( 'NONE',  ( 4.118306542938309889, 1.879866726353071060, 0.3679503660072875881 ) ) ;
#186928 = CARTESIAN_POINT ( 'NONE',  ( 5.336411075974297979, -1.153114810915600641, 1.719314882265559286 ) ) ;
#186929 = CARTESIAN_POINT ( 'NONE',  ( -0.6823417656249969321, 4.030208333674754506, -1.181850606188749264 ) ) ;
#186930 = CIRCLE ( 'NONE', #200672, 0.04999999999999929501 ) ;
#186931 = CARTESIAN_POINT ( 'NONE',  ( 3.344560887785383851, 0.4775036937760200884, 1.912655531573831835 ) ) ;
#186932 = CARTESIAN_POINT ( 'NONE',  ( 1.588762598846172436, -0.2802010128373257913, -1.905785462699102206 ) ) ;
#186933 = CARTESIAN_POINT ( 'NONE',  ( 4.399188623838041323, 1.502396186649012311, 1.114296746780506497 ) ) ;
#186934 = CARTESIAN_POINT ( 'NONE',  ( 3.036059619770274498, -1.550059391276232601, -1.709768245815939780 ) ) ;
#186935 = CARTESIAN_POINT ( 'NONE',  ( 4.000341067899515046, 1.851953036565538335, 0.1839423254178795542 ) ) ;
#186936 = CARTESIAN_POINT ( 'NONE',  ( 1.364683531249988535, 3.905208333674751842, -0.7879004041258239610 ) ) ;
#186937 = CARTESIAN_POINT ( 'NONE',  ( 0.4019237886466847653, 8.854914550367425363, 1.499999999999997113 ) ) ;
#186938 = CARTESIAN_POINT ( 'NONE',  ( 1.963634227113943087, 0.3588053174017143965, -2.075111507017588064 ) ) ;
#186939 = CARTESIAN_POINT ( 'NONE',  ( 4.500943809612556024, 4.353448654077163305, 1.214306433183764966E-14 ) ) ;
#186941 = CARTESIAN_POINT ( 'NONE',  ( 0.7500000000000006661, 8.916666666666669627, -1.299038105676657340 ) ) ;
#186940 = CARTESIAN_POINT ( 'NONE',  ( 1.364683531249990311, 5.426041667008086655, 0.7879004041258500513 ) ) ;
#186942 = CARTESIAN_POINT ( 'NONE',  ( 2.724977724663907530, 1.532976055022855499, -1.465462182430438798 ) ) ;
#186943 = CARTESIAN_POINT ( 'NONE',  ( 2.979851157752180235, 6.482852879502049248, -0.5607284034093787950 ) ) ;
#186944 = CARTESIAN_POINT ( 'NONE',  ( 0.2463608477257169804, 1.034524919618844407, -1.734561685378380957 ) ) ;
#186945 = CARTESIAN_POINT ( 'NONE',  ( 1.364683531249986537, 1.113541667008082658, 0.7879004041258500513 ) ) ;
#186946 = CARTESIAN_POINT ( 'NONE',  ( -2.806174608348664723, 6.217694776474651519, 1.040834085586084257E-14 ) ) ;
#186947 = CARTESIAN_POINT ( 'NONE',  ( 4.147904930777053245, 6.926640621626830807, -1.199719254218452047 ) ) ;
#186948 = ORIENTED_EDGE ( 'NONE', *, *, #16428, .F. ) ;
#186949 = CARTESIAN_POINT ( 'NONE',  ( 1.687033600898584895, -0.3153356727807927196, -2.138329785107299319 ) ) ;
#186950 = CARTESIAN_POINT ( 'NONE',  ( 6.889999999999967706, 0.005249217920031550542, 1.719840535937327664 ) ) ;
#186953 = CARTESIAN_POINT ( 'NONE',  ( 3.894033820048787398, 8.999999999999998224, 0.7749999999999996891 ) ) ;
#186952 = CARTESIAN_POINT ( 'NONE',  ( 5.747733515963313167, 7.238988828695343436, -1.232940794674276974 ) ) ;
#186951 = CARTESIAN_POINT ( 'NONE',  ( 6.059568310664962709, 6.034194215389424798, 0.7998128361456352531 ) ) ;
#186954 = CARTESIAN_POINT ( 'NONE',  ( -0.4294425147611594107, -9.006862915010128035, 9.490288674561789151 ) ) ;
#186955 = CARTESIAN_POINT ( 'NONE',  ( 5.384000029850495750, -2.016708404008683786, 0.004832792792668073358 ) ) ;
#186956 = CARTESIAN_POINT ( 'NONE',  ( -8.242994207428740339, 9.679543332497402730, 1.082531754730558626 ) ) ;
#186957 = CARTESIAN_POINT ( 'NONE',  ( 6.356985058417449430, 0.3567463788109735967, -2.059909276252298582 ) ) ;
#186958 = PLANE ( 'NONE',  #84367 ) ;
#186960 = CARTESIAN_POINT ( 'NONE',  ( -1.364683531250010740, 11.88020833367473017, 0.7879004041258445001 ) ) ;
#186959 = CARTESIAN_POINT ( 'NONE',  ( 6.649309733611729278, -1.732918351142084035, -1.292073167451508686 ) ) ;
#186961 = CARTESIAN_POINT ( 'NONE',  ( -9.429859533504656000, 10.96025652963230534, -1.199719254218441611 ) ) ;
#186962 = CARTESIAN_POINT ( 'NONE',  ( -5.327991180046197428, 8.199444895820425572, 1.082531754730548412 ) ) ;
#186963 = CARTESIAN_POINT ( 'NONE',  ( -0.6823417656250003738, 1.530208333674752730, -1.181850606188749264 ) ) ;
#186964 = CARTESIAN_POINT ( 'NONE',  ( -3.511198596259319960, 6.271927390929313617, 2.420000000000010587 ) ) ;
#186965 = CARTESIAN_POINT ( 'NONE',  ( -0.7500000000000179856, 10.29166666666667140, 1.299038105676658228 ) ) ;
#186966 = CARTESIAN_POINT ( 'NONE',  ( 2.877275982374318364, 1.637783285604855088, -0.5413683153251740432 ) ) ;
#186967 = CARTESIAN_POINT ( 'NONE',  ( 3.932747076415766596, 6.745899468197171345, 1.199719254218451159 ) ) ;
#186968 = CARTESIAN_POINT ( 'NONE',  ( 2.477515592860125349, 1.084993897938502760, 1.398054747847920609 ) ) ;
#186970 = CARTESIAN_POINT ( 'NONE',  ( 2.701816853162309684, 1.425160482578791354, 1.422027561765064174 ) ) ;
#186969 = AXIS2_PLACEMENT_3D ( 'NONE', #110210, #15811, #127551 ) ;
#186971 = CARTESIAN_POINT ( 'NONE',  ( 5.754950181447250124, -1.742976869204535983, 1.353379275444612562 ) ) ;
#186972 = VERTEX_POINT ( 'NONE', #159328 ) ;
#186973 = CARTESIAN_POINT ( 'NONE',  ( -7.611976899429754084, 7.845337568948314022, 0.7998128361456341429 ) ) ;
#186975 = CARTESIAN_POINT ( 'NONE',  ( 3.743767684670766371, 2.000855813463810584, -0.2496267151909299931 ) ) ;
#186974 = CARTESIAN_POINT ( 'NONE',  ( 4.811248821985151913, 1.762591750878339081, -1.178568461981117643 ) ) ;
#186977 = VERTEX_POINT ( 'NONE', #208064 ) ;
#186976 = CARTESIAN_POINT ( 'NONE',  ( 4.658376882426285448, 1.807244876408566681, 0.1260263862136162261 ) ) ;
#186978 = CARTESIAN_POINT ( 'NONE',  ( 6.059568310664962709, 6.034194215389424798, 0.7998128361456352531 ) ) ;
#186979 = EDGE_LOOP ( 'NONE', ( #46934, #52752, #148568, #95849, #125028 ) ) ;
#186980 = EDGE_CURVE ( 'NONE', #129569, #193266, #138521, .T. ) ;
#186981 = CARTESIAN_POINT ( 'NONE',  ( 1.973319494866377699, 1.790917844098998124, -0.5403536831049270406 ) ) ;
#186982 = CARTESIAN_POINT ( 'NONE',  ( 6.727182134110220701, 0.005875948494733078051, 1.810970247402940103 ) ) ;
#186983 = CARTESIAN_POINT ( 'NONE',  ( 6.516260798181108704, -1.810903427820510503, 0.05229752674829404868 ) ) ;
#186984 = FACE_OUTER_BOUND ( 'NONE', #19538, .T. ) ;
#186985 = CARTESIAN_POINT ( 'NONE',  ( -10.41986968326957808, 5.020773655391575829, -5.279272669861445166 ) ) ;
#186986 = CARTESIAN_POINT ( 'NONE',  ( -7.721398836998370818, -5.907420853759296264, 7.721398836998400128 ) ) ;
#186987 = EDGE_CURVE ( 'NONE', #142253, #24930, #16853, .T. ) ;
#186988 = CARTESIAN_POINT ( 'NONE',  ( 0.6823417656249917140, 3.655208333674754506, 1.181850606188765695 ) ) ;
#186989 = CARTESIAN_POINT ( 'NONE',  ( 0.4043728756845180183, -1.898191424145349471, -0.2318213773434482650 ) ) ;
#186990 = EDGE_LOOP ( 'NONE', ( #139891, #2559, #173525, #194225, #124473 ) ) ;
#186991 = CARTESIAN_POINT ( 'NONE',  ( 6.861835142292135536, 9.098836647464588978, 1.443375672974065660 ) ) ;
#186992 = CARTESIAN_POINT ( 'NONE',  ( 2.101936620064443151, 0.7537240185569763495, -1.811501260397870405 ) ) ;
#186993 = CARTESIAN_POINT ( 'NONE',  ( -5.167065940583949413, 5.200867483535597913, 0.000000000000000000 ) ) ;
#186994 = CARTESIAN_POINT ( 'NONE',  ( -4.599959256786493533, 8.588645909551377855, 0.000000000000000000 ) ) ;
#186995 = CARTESIAN_POINT ( 'NONE',  ( 4.447591161967184625, -1.937652164471121763, 0.8620916771790233524 ) ) ;
#186997 = SURFACE_SIDE_STYLE ('',( #134025 ) ) ;
#186996 = CARTESIAN_POINT ( 'NONE',  ( -0.1296875068448159751, 0.001480089298542403009, -1.826395826379861864 ) ) ;
#186998 = CARTESIAN_POINT ( 'NONE',  ( 5.852796007109359877, -1.555770171409420977, 1.210649060634989560 ) ) ;
#186999 = CARTESIAN_POINT ( 'NONE',  ( -1.201851678989727383E-14, 1.321875000341419248, 1.575800808251672791 ) ) ;
#187000 = CARTESIAN_POINT ( 'NONE',  ( 0.6682274066662279299, 2.010706302723582972, -0.1030755154480169355 ) ) ;
#187001 = ORIENTED_EDGE ( 'NONE', *, *, #171547, .T. ) ;
#187002 = CARTESIAN_POINT ( 'NONE',  ( -0.1349523647116790404, -0.1509472049114955194, -2.083628827036696052 ) ) ;
#187003 = CARTESIAN_POINT ( 'NONE',  ( 11.52860214534722694, 7.264370032338475447, 3.363647956867556132 ) ) ;
#187004 = CARTESIAN_POINT ( 'NONE',  ( 1.873570696236816158, -0.2555354716398828274, 2.054483085851127377 ) ) ;
#187005 = CARTESIAN_POINT ( 'NONE',  ( 3.878514461961128479, 6.682628084666728085, -1.199719254218448494 ) ) ;
#187006 = CARTESIAN_POINT ( 'NONE',  ( 4.766573523656222555, 7.718696989977711809, 1.199719254218452047 ) ) ;
#187007 = VERTEX_POINT ( 'NONE', #181677 ) ;
#187009 = CARTESIAN_POINT ( 'NONE',  ( 5.518332215962025167, 6.396807992499198292, -1.199719254218445830 ) ) ;
#187008 = CARTESIAN_POINT ( 'NONE',  ( 5.279275078172800839, 1.403616728028998395, 1.549557787628618399 ) ) ;
#187012 = ORIENTED_EDGE ( 'NONE', *, *, #12707, .T. ) ;
#187011 = CARTESIAN_POINT ( 'NONE',  ( 2.015983567491559381, -1.811083833189537806, 0.04518873659950343319 ) ) ;
#187010 = CARTESIAN_POINT ( 'NONE',  ( 3.592628304870106870, -0.3553021837224104584, -1.790491875447843384 ) ) ;
#187013 = CARTESIAN_POINT ( 'NONE',  ( 6.111994396789379280, -2.190734547077430872, 0.2660306753756238041 ) ) ;
#187014 = DIRECTION ( 'NONE',  ( -0.2079116908177593703, 0.000000000000000000, 0.9781476007338056888 ) ) ;
#187015 = CARTESIAN_POINT ( 'NONE',  ( 3.926972183325681875, 2.094573593246536802, 0.6948772193901550098 ) ) ;
#187016 = CARTESIAN_POINT ( 'NONE',  ( -1.402160292154681736E-14, 9.734375000341399797, 1.575800808251682339 ) ) ;
#187017 = CARTESIAN_POINT ( 'NONE',  ( 2.490748672031910083, -1.830495558572857728, -0.5533032672612181457 ) ) ;
#187018 = CARTESIAN_POINT ( 'NONE',  ( 8.259941899223605333, 10.65968485389279508, -1.599625672291268286 ) ) ;
#187019 = CARTESIAN_POINT ( 'NONE',  ( 6.391088794356012848, 0.1989163192229244648, 2.060770550043041993 ) ) ;
#187020 = CARTESIAN_POINT ( 'NONE',  ( -0.7500000000000179856, 10.32291666734946922, 1.299038105676658228 ) ) ;
#187021 = ADVANCED_FACE ( 'NONE', ( #99389 ), #200327, .T. ) ;
#187022 = CARTESIAN_POINT ( 'NONE',  ( 5.987848539424092564, -2.180829346447300310, -0.2163489798085171945 ) ) ;
#187023 = CARTESIAN_POINT ( 'NONE',  ( 5.269423316188119877, 7.778230059001682406, -1.291559732514224068 ) ) ;
#187024 = FACE_OUTER_BOUND ( 'NONE', #41314, .T. ) ;
#187025 = VERTEX_POINT ( 'NONE', #196876 ) ;
#187026 = CARTESIAN_POINT ( 'NONE',  ( 9.498884310698274547, -9.900000000000076739, -0.1658036423890195676 ) ) ;
#187027 = CARTESIAN_POINT ( 'NONE',  ( 3.936663633328242096, 0.2718032920513112627, 1.850550731861917653 ) ) ;
#187028 = CARTESIAN_POINT ( 'NONE',  ( -1.642778471874998480, -1.188541666188709600, 2.845375778867863303 ) ) ;
#187029 = CARTESIAN_POINT ( 'NONE',  ( 5.722950238744209273, 6.809768379023969587, 1.082531754730549967 ) ) ;
#187030 = AXIS2_PLACEMENT_3D ( 'NONE', #47815, #161551, #159400 ) ;
#187031 = CARTESIAN_POINT ( 'NONE',  ( -7.917598520700757980, 9.299915031314755609, 1.082531754730558626 ) ) ;
#187032 = CARTESIAN_POINT ( 'NONE',  ( 3.464990776744291345, 6.200183785247111778, 1.199719254218452047 ) ) ;
#187033 = CARTESIAN_POINT ( 'NONE',  ( 6.719590346122157776, 0.3599300073104904074, -2.038585587018165945 ) ) ;
#187034 = EDGE_CURVE ( 'NONE', #35153, #33663, #56843, .T. ) ;
#187035 = CARTESIAN_POINT ( 'NONE',  ( 1.423454079394898875, -1.462460055423294047, -1.388472309132340321 ) ) ;
#187036 = CARTESIAN_POINT ( 'NONE',  ( -7.797910906154257304, 12.24931315715533486, 0.000000000000000000 ) ) ;
#187037 = CARTESIAN_POINT ( 'NONE',  ( 5.508355548902068577, 9.648441583686274470, 0.7998128361456331437 ) ) ;
#187038 = CARTESIAN_POINT ( 'NONE',  ( 2.240623464304030588, 5.557885108422582654, 0.2071306710573883048 ) ) ;
#187039 = CARTESIAN_POINT ( 'NONE',  ( 1.359612608069911133, 2.158557413232742750, -0.3773744582575569995 ) ) ;
#187040 = CARTESIAN_POINT ( 'NONE',  ( 4.758326833623739205, 0.7015320795021735556, 1.685726030614169924 ) ) ;
#187041 = CARTESIAN_POINT ( 'NONE',  ( -2.449219305563052895, 6.009172956465517856, 1.040834085586084257E-14 ) ) ;
#187042 = CARTESIAN_POINT ( 'NONE',  ( 7.038091139269835317, 7.383730215335837954, 0.000000000000000000 ) ) ;
#187043 = CARTESIAN_POINT ( 'NONE',  ( 8.387690588348714726, 12.93738945304888333, 1.040834085586084257E-14 ) ) ;
#187044 = CARTESIAN_POINT ( 'NONE',  ( -4.471156797456668386, 8.438376373666578445, -0.7998128361456362523 ) ) ;
#187045 = CARTESIAN_POINT ( 'NONE',  ( 4.701980345841006326, 4.380065246436280368, 0.7998128361456341429 ) ) ;
#187046 = CARTESIAN_POINT ( 'NONE',  ( 7.187230829020129441, 8.518095734345896730, 1.082531754730549967 ) ) ;
#187047 = ORIENTED_EDGE ( 'NONE', *, *, #4172, .F. ) ;
#187049 = CARTESIAN_POINT ( 'NONE',  ( 5.730732165690560542, 1.348809278943388534, -1.494750323444839601 ) ) ;
#187048 = CARTESIAN_POINT ( 'NONE',  ( 3.438839575862782549, -1.396446551253815782, -1.200180114512699792 ) ) ;
#187050 = CARTESIAN_POINT ( 'NONE',  ( 2.302535375473542700, -2.053259096611260937, 1.032894330136547856 ) ) ;
#187052 = CARTESIAN_POINT ( 'NONE',  ( 6.684431423333510480, 1.132142624513672091, -1.601896353945003071 ) ) ;
#187051 = CARTESIAN_POINT ( 'NONE',  ( 3.226477370372293763, 6.708047998835573900, 0.7216878364870317197 ) ) ;
#187053 = CARTESIAN_POINT ( 'NONE',  ( -4.904298879841297421, 6.744767997946721216, 1.599625672291267398 ) ) ;
#187054 = DIRECTION ( 'NONE',  ( -0.6507913734559640506, -0.7592566023653004592, 0.000000000000000000 ) ) ;
#187055 = CARTESIAN_POINT ( 'NONE',  ( 3.427896188528327226, -1.883279545317056547, 0.3315703044584616399 ) ) ;
#187056 = CARTESIAN_POINT ( 'NONE',  ( -9.297140650669053485, 11.86975006391249643, 1.599625672291281386 ) ) ;
#187057 = CARTESIAN_POINT ( 'NONE',  ( 6.476386945563378461, 6.757828299745357370, 0.2189195654383000456 ) ) ;
#187058 = CARTESIAN_POINT ( 'NONE',  ( -6.116136693540540570, 10.14959355252370266, 0.000000000000000000 ) ) ;
#187060 = CARTESIAN_POINT ( 'NONE',  ( 1.463515404423965105, 1.843522461416190250, -0.3164952454337774390 ) ) ;
#187059 = CARTESIAN_POINT ( 'NONE',  ( 3.122686798916929352, 0.05371976762510695391, 2.090236283336026180 ) ) ;
#187061 = CARTESIAN_POINT ( 'NONE',  ( 2.161482305958133399, -0.5350050527693461788, -1.943774068525660148 ) ) ;
#187062 = CARTESIAN_POINT ( 'NONE',  ( 7.402388683381404988, 10.61957531637824204, -1.082531754730537976 ) ) ;
#187063 = CARTESIAN_POINT ( 'NONE',  ( 1.364683531249988535, 3.967708333674752286, -0.7879004041258239610 ) ) ;
#187064 = CARTESIAN_POINT ( 'NONE',  ( 3.104748464929545371, -0.3365338927540823533, 1.707397895346264738 ) ) ;
#187065 = AXIS2_PLACEMENT_3D ( 'NONE', #94046, #59385, #9567 ) ;
#187066 = CARTESIAN_POINT ( 'NONE',  ( 5.118366684358879759, 5.930181538962194132, 1.199719254218462483 ) ) ;
#187067 = DIRECTION ( 'NONE',  ( 0.000000000000000000, 1.000000000000000000, 0.000000000000000000 ) ) ;
#187068 = CARTESIAN_POINT ( 'NONE',  ( 3.404663882806455266, 1.358838683821527393, -1.062305643495575103 ) ) ;
#187069 = CARTESIAN_POINT ( 'NONE',  ( 4.423480980095358284, -1.348712413769267426, -1.727291790683552541 ) ) ;
#187070 = CARTESIAN_POINT ( 'NONE',  ( 5.795608111622330583, 1.668732747960173235, 1.444295198399044855 ) ) ;
#187071 = CARTESIAN_POINT ( 'NONE',  ( -10.47097306639366820, 4.046871294038967726, -7.151610515452683003 ) ) ;
#187072 = CARTESIAN_POINT ( 'NONE',  ( 3.573241956510754491, 1.960547127731948613, 0.9329660139856699175 ) ) ;
#187073 = CARTESIAN_POINT ( 'NONE',  ( 2.754317325142870754, 0.6151756178996542479, 1.719052816137212503 ) ) ;
#187074 = CARTESIAN_POINT ( 'NONE',  ( -0.4019237886467001974, 9.332585450998170273, 1.500000000000001998 ) ) ;
#187075 = CARTESIAN_POINT ( 'NONE',  ( 4.505136581001433882, -0.1005046246093168893, 2.115047560132724325 ) ) ;
#187076 = CARTESIAN_POINT ( 'NONE',  ( 6.539320575229215393, 2.445213257098968640, 2.379920919941742152 ) ) ;
#187077 = ORIENTED_EDGE ( 'NONE', *, *, #180630, .F. ) ;
#187079 = CARTESIAN_POINT ( 'NONE',  ( -0.6823417656250003738, 3.030208333674754062, -1.181850606188749264 ) ) ;
#187078 = CARTESIAN_POINT ( 'NONE',  ( 4.616876278103482001, -0.1136277499396514262, 2.289655339347085317 ) ) ;
#187080 = CARTESIAN_POINT ( 'NONE',  ( 6.720655732516649827, 7.053635520514346169, 2.324416633011537225 ) ) ;
#187081 = CARTESIAN_POINT ( 'NONE',  ( 2.354312230267378236, 5.898448035287240820, -0.7998128361456281477 ) ) ;
#187082 = CARTESIAN_POINT ( 'NONE',  ( 0.2938078718510480081, 1.976988316466289142, -0.7672523047414223640 ) ) ;
#187083 = CARTESIAN_POINT ( 'NONE',  ( -5.910991785878175975, 6.958873840688411860, -1.082531754730544860 ) ) ;
#187084 = CARTESIAN_POINT ( 'NONE',  ( 4.067082894419602468, 3.847277586352047862, -0.7216878364870188411 ) ) ;
#187085 = CARTESIAN_POINT ( 'NONE',  ( -4.568734577680880093, 7.313645526394248364, -1.082531754730548412 ) ) ;
#187086 = LINE ( 'NONE', #85325, #196599 ) ;
#187087 = ORIENTED_EDGE ( 'NONE', *, *, #71800, .T. ) ;
#187088 = CARTESIAN_POINT ( 'NONE',  ( 5.590470263882489910, -0.4872053753022275169, 1.956560708789633285 ) ) ;
#187090 = CARTESIAN_POINT ( 'NONE',  ( 3.186439481354142789, 1.149679979862153756, -1.712247615763124120 ) ) ;
#187089 = CARTESIAN_POINT ( 'NONE',  ( 4.985647801523278133, 6.839675073242382553, -1.599625672291256295 ) ) ;
#187092 = CARTESIAN_POINT ( 'NONE',  ( -0.1408020194050328411, 7.629137130509059617, -2.700278568655100742 ) ) ;
#187091 = CARTESIAN_POINT ( 'NONE',  ( 5.936491157937257235, 8.019268665717216749, 1.599625672291268286 ) ) ;
#187093 = CARTESIAN_POINT ( 'NONE',  ( 6.176621499477501054, 9.363752961769195693, -1.199719254218452047 ) ) ;
#187094 = CARTESIAN_POINT ( 'NONE',  ( -3.285556943750000514, -0.4885416661887091450, -1.896917185911906500 ) ) ;
#187095 = DIRECTION ( 'NONE',  ( 1.276756478318932585E-15, -1.000000000000000000, 1.665334536937738262E-16 ) ) ;
#187096 = CARTESIAN_POINT ( 'NONE',  ( 5.806613533822880591, 1.931179984464112653, 1.035834350304319695 ) ) ;
#187097 = CARTESIAN_POINT ( 'NONE',  ( 4.096327398540238640, -0.3419367296172080017, 1.987046374476949095 ) ) ;
#187098 = CARTESIAN_POINT ( 'NONE',  ( 3.702549152423353807, 1.581054339307564449, 0.9433870219286569769 ) ) ;
#187099 = CARTESIAN_POINT ( 'NONE',  ( 5.198661835836162481, 8.152523677529138979, 1.199719254218462483 ) ) ;
#187100 = CARTESIAN_POINT ( 'NONE',  ( 0.5336903687956630060, 0.8928529924820073349, -1.475541649381803433 ) ) ;
#187101 = CARTESIAN_POINT ( 'NONE',  ( -3.195971524519394702, 4.751719416737803847, -1.599625672291262513 ) ) ;
#187102 = CARTESIAN_POINT ( 'NONE',  ( 1.020660257703887908, -2.075033540828072454, 0.9893533861183384515 ) ) ;
#187103 = CARTESIAN_POINT ( 'NONE',  ( -5.280010757518168063, 8.247430752824802980, -1.199719254218446718 ) ) ;
#187104 = CARTESIAN_POINT ( 'NONE',  ( 0.6501784551898766029, 0.7083214130543177278, -2.148700229429708841 ) ) ;
#187105 = CARTESIAN_POINT ( 'NONE',  ( 3.510471945985794928, -0.8535800194418289299, -1.925527614133336840 ) ) ;
#187106 = CARTESIAN_POINT ( 'NONE',  ( -5.822300622425855110, 5.757381912443740646, 0.7998128361456281477 ) ) ;
#187107 = CARTESIAN_POINT ( 'NONE',  ( 8.260995669428309540, 8.532249790621511565, 0.7998128361456481317 ) ) ;
#187108 = CARTESIAN_POINT ( 'NONE',  ( 6.495764994278809823, 6.751016379513001375, 0.7216878364870328300 ) ) ;
#187109 = FILL_AREA_STYLE_COLOUR ( '', #93615 ) ;
#187111 = EDGE_CURVE ( 'NONE', #195163, #108282, #108865, .T. ) ;
#187110 = CARTESIAN_POINT ( 'NONE',  ( -7.223796917982883592, 7.322184580601816428, -0.7998128361456291469 ) ) ;
#187112 = CARTESIAN_POINT ( 'NONE',  ( 5.788968402910795064, 9.697620870130524651, 0.7216878364870438212 ) ) ;
#187113 = CARTESIAN_POINT ( 'NONE',  ( 5.132834705836428313, 6.694876404991986441, 1.408819685294822932 ) ) ;
#187114 = CARTESIAN_POINT ( 'NONE',  ( -4.141125853970233806, 6.918731698685530063, -1.199719254218452047 ) ) ;
#187116 = CARTESIAN_POINT ( 'NONE',  ( 4.254274768897357006, 0.9481281144863746846, -2.009013624686401212 ) ) ;
#187115 = CARTESIAN_POINT ( 'NONE',  ( 2.215225606797793567, 1.700350911433265555, -1.266953333846132512 ) ) ;
#187117 = CARTESIAN_POINT ( 'NONE',  ( 2.308753661914957345, 1.958203289975643191, 0.9839491227633669901 ) ) ;
#187118 = CARTESIAN_POINT ( 'NONE',  ( -7.413611068574208041, 7.543634422958360730, 0.7998128361456341429 ) ) ;
#187119 = CARTESIAN_POINT ( 'NONE',  ( -5.957882158562513908, 5.915560371269843465, -0.7998128361456362523 ) ) ;
#187120 = CARTESIAN_POINT ( 'NONE',  ( 5.512146440779991607, 1.959692598237902761, -0.09458084330612320789 ) ) ;
#187121 =( BOUNDED_SURFACE ( )  B_SPLINE_SURFACE ( 1, 2, ( 
 ( #199212, #214372, #130066, #30360, #162498, #196059, #83340, #114854, #64961, #81228, #211215, #37535, #47691, #198158, #80157, #115917, #17265, #146263, #113803, #212275, #15142, #97500, #31424, #164612, #66002, #147310, #79091, #112737, #16197, #163557, #213336, #103613, #13014, #145209, #131113, #67072, #181904, #197100, #33538, #48741, #133208, #49791, #62841, #129002, #180854, #32476, #98549, #194979, #82278, #132152, #99610, #165676, #149425, #1008, #46615, #124221, #173975, #123165, #73221, #169668, #23401, #39673, #170737, #104688, #206432, #71074, #91657, #125279, #22323, #137192, #9307, #7150, #121011, #21254, #189126, #190183, #191241, #59122, #154500, #207500, #25549, #141494, #90582, #186978, #40761, #6078, #88436, #42904, #156642, #87360, #204271, #41838, #55925, #8234, #72149, #157710, #140414, #153429, #155568, #74317, #138258, #122082, #38610, #188043, #4998, #105784, #171809, #107949, #203215, #89514, #139328, #205358, #54860, #56992, #106867, #172894, #24469, #58056, #75380, #14622, #159825, #212826, #209618, #211759, #143623, #80717, #26619, #110080, #195533, #146808, #92720, #177148, #196595, #163042, #64462, #158766, #10361, #144689, #160900, #96991, #46100, #95924, #47172, #45034, #145759, #30916, #76438, #94849, #63397, #11428, #176092, #60186, #61260, #142546, #109013, #27690, #130607, #29840, #28765, #175032, #77504, #93789, #127418, #193390, #111148, #208552, #12496, #126345, #129551, #192305, #178225, #210700, #78569, #43964, #62330, #112216, #128489, #194455, #161978, #13568, #79640, #113286, #179292, #48236, #152108, #3678, #2620, #184584, #35134, #84964, #69757, #82830, #197645, #102277, #17807, #101207, #167293, #16745, #114350, #33024, #51412, #83890, #18880, #199767, #148906, #149981, #135861, #180347, #480, #81774, #31968, #168354, #68691, #117532, #134813, #98051, #198696, #200818, #66546, #49290, #132689, #166215, #50340, #164104, #15687, #213873, #116460, #151053, #147854, #133758, #183526, #65495, #131642, #115407, #182453, #1552, #181400, #99101, #19947, #165154, #67613 ),
 ( #34081, #100150, #52469, #86033, #118595, #36202, #122906, #153167, #155307, #57804, #172635, #75125, #187789, #188864, #38350, #104428, #4742, #170475, #185650, #54601, #120749, #7966, #201883, #55663, #121820, #22061, #157456, #88171, #25294, #186724, #9050, #24210, #91395, #107690, #154243, #53532, #5815, #90312, #71890, #173718, #119664, #202960, #74057, #37282, #137999, #70818, #136933, #204017, #123962, #89256, #39418, #105512, #103353, #169417, #171544, #156384, #23139, #140149, #206173, #6889, #72967, #139072, #205097, #56738, #40502, #106607, #189931, #41576, #21001, #87098, #78313, #27431, #192048, #14367, #96741, #162789, #59932, #195281, #95670, #143362, #29582, #11169, #46913, #111965, #125026, #141234, #43711, #93529, #44781, #108757, #159571, #61004, #28506, #13315, #76183, #77245, #144437, #161723, #145507, #94596, #110887, #207243, #209359, #127161, #142291, #208302, #177968, #42647, #63142, #58869, #126087, #174781, #113031, #193132, #92472, #190983, #160639, #79388, #26356, #30655, #109829, #179037, #211505, #158510, #62080, #10110, #12239, #175839, #176893, #210439, #128237, #194200, #45846, #129304, #181151, #1307, #65247, #118352, #213620, #102041, #117282, #184340, #200577, #131397, #35963, #32773, #183280, #115156, #52224, #212576, #81524, #167047, #168110, #197394, #31720, #163855, #49036, #150806, #182205, #132452, #148665, #64215, #80458, #98852, #51160, #97795, #34884, #84718, #147602, #164903, #16496, #82577, #231, #15435, #17556, #67367, #66303, #146556, #180096, #83642, #198450, #50096, #130355, #196347, #47989, #116217, #134576, #100957, #33831, #18639, #99910, #114105, #2370, #165971, #149729, #133511, #199515, #68447, #201639, #38111, #153995, #121574, #106358, #169167, #120504, #171300, #188615, #23970, #187545, #137757, #19709, #87921, #104183, #20762, #86856, #56494, #135619, #156135, #189678, #152921, #53287, #73801, #71644, #185407, #85788, #39176, #40247, #41328, #123717, #4500, #57559, #90072, #205926, #155060, #37025, #105259, #70568, #136687, #107438, #6647, #151868 ) ),
 .UNSPECIFIED., .F., .F., .T. ) 
 B_SPLINE_SURFACE_WITH_KNOTS ( ( 2, 2 ),
 ( 3, 2, 2, 2, 2, 2, 2, 2, 2, 2, 2, 2, 2, 2, 2, 2, 2, 2, 2, 2, 2, 2, 2, 2, 2, 2, 2, 2, 2, 2, 2, 2, 2, 2, 2, 2, 2, 2, 2, 2, 2, 2, 2, 2, 2, 2, 2, 2, 2, 2, 2, 2, 2, 2, 2, 2, 2, 2, 2, 2, 2, 2, 2, 2, 2, 2, 2, 2, 2, 2, 2, 2, 2, 2, 2, 2, 2, 2, 2, 2, 2, 2, 2, 2, 2, 2, 2, 2, 2, 2, 2, 2, 2, 2, 2, 2, 2, 2, 2, 2, 2, 2, 2, 2, 2, 2, 2, 2, 2, 2, 2, 2, 2, 2, 2, 2, 2, 2, 2, 2, 3 ),
 ( 0.000000000000000000, 1.000000000000000000 ),
 ( 0.000000000000000000, 0.008333333333333333218, 0.01666666666666666644, 0.02500000000000000139, 0.03333333333333333287, 0.04166666666666666435, 0.05000000000000000278, 0.05833333333333333426, 0.06666666666666666574, 0.07499999999999999722, 0.08333333333333332871, 0.09166666666666666019, 0.1000000000000000056, 0.1083333333333333370, 0.1166666666666666685, 0.1250000000000000000, 0.1333333333333333315, 0.1416666666666666630, 0.1499999999999999944, 0.1583333333333333259, 0.1666666666666666574, 0.1749999999999999889, 0.1833333333333333204, 0.1916666666666666796, 0.2000000000000000111, 0.2083333333333333426, 0.2166666666666666741, 0.2250000000000000056, 0.2333333333333333370, 0.2416666666666666685, 0.2500000000000000000, 0.2583333333333333592, 0.2666666666666666630, 0.2750000000000000222, 0.2833333333333333259, 0.2916666666666666852, 0.2999999999999999889, 0.3083333333333333481, 0.3166666666666666519, 0.3250000000000000111, 0.3333333333333333148, 0.3416666666666666741, 0.3499999999999999778, 0.3583333333333333370, 0.3666666666666666408, 0.3750000000000000000, 0.3833333333333333592, 0.3916666666666666630, 0.4000000000000000222, 0.4083333333333333259, 0.4166666666666666852, 0.4249999999999999889, 0.4333333333333333481, 0.4416666666666666519, 0.4500000000000000111, 0.4583333333333333148, 0.4666666666666666741, 0.4749999999999999778, 0.4833333333333333370, 0.4916666666666666408, 0.5000000000000000000, 0.5083333333333333037, 0.5166666666666667185, 0.5250000000000000222, 0.5333333333333333259, 0.5416666666666666297, 0.5500000000000000444, 0.5583333333333333481, 0.5666666666666666519, 0.5749999999999999556, 0.5833333333333333703, 0.5916666666666666741, 0.5999999999999999778, 0.6083333333333332815, 0.6166666666666666963, 0.6250000000000000000, 0.6333333333333333037, 0.6416666666666667185, 0.6500000000000000222, 0.6583333333333333259, 0.6666666666666666297, 0.6750000000000000444, 0.6833333333333333481, 0.6916666666666666519, 0.6999999999999999556, 0.7083333333333333703, 0.7166666666666666741, 0.7249999999999999778, 0.7333333333333332815, 0.7416666666666666963, 0.7500000000000000000, 0.7583333333333333037, 0.7666666666666667185, 0.7750000000000000222, 0.7833333333333333259, 0.7916666666666666297, 0.8000000000000000444, 0.8083333333333333481, 0.8166666666666666519, 0.8249999999999999556, 0.8333333333333333703, 0.8416666666666666741, 0.8499999999999999778, 0.8583333333333332815, 0.8666666666666666963, 0.8750000000000000000, 0.8833333333333333037, 0.8916666666666667185, 0.9000000000000000222, 0.9083333333333333259, 0.9166666666666666297, 0.9250000000000000444, 0.9333333333333333481, 0.9416666666666666519, 0.9499999999999999556, 0.9583333333333333703, 0.9666666666666666741, 0.9749999999999999778, 0.9833333333333332815, 0.9916666666666666963, 1.000000000000000000 ),
 .UNSPECIFIED. ) 
 GEOMETRIC_REPRESENTATION_ITEM ( )  RATIONAL_B_SPLINE_SURFACE ( (
 ( 1.000000000000000000, 0.8660254037844387076, 1.000000000000000000, 0.8660254037844387076, 1.000000000000000000, 0.8660254037844387076, 1.000000000000000000, 0.8660254037844387076, 1.000000000000000000, 0.8660254037844387076, 1.000000000000000000, 0.8660254037844387076, 1.000000000000000000, 0.8660254037844387076, 1.000000000000000000, 0.8660254037844387076, 1.000000000000000000, 0.8660254037844387076, 1.000000000000000000, 0.8660254037844387076, 1.000000000000000000, 0.8660254037844387076, 1.000000000000000000, 0.8660254037844387076, 1.000000000000000000, 0.8660254037844387076, 1.000000000000000000, 0.8660254037844387076, 1.000000000000000000, 0.8660254037844387076, 1.000000000000000000, 0.8660254037844387076, 1.000000000000000000, 0.8660254037844387076, 1.000000000000000000, 0.8660254037844387076, 1.000000000000000000, 0.8660254037844387076, 1.000000000000000000, 0.8660254037844387076, 1.000000000000000000, 0.8660254037844387076, 1.000000000000000000, 0.8660254037844387076, 1.000000000000000000, 0.8660254037844387076, 1.000000000000000000, 0.8660254037844387076, 1.000000000000000000, 0.8660254037844387076, 1.000000000000000000, 0.8660254037844387076, 1.000000000000000000, 0.8660254037844387076, 1.000000000000000000, 0.8660254037844387076, 1.000000000000000000, 0.8660254037844387076, 1.000000000000000000, 0.8660254037844387076, 1.000000000000000000, 0.8660254037844387076, 1.000000000000000000, 0.8660254037844387076, 1.000000000000000000, 0.8660254037844387076, 1.000000000000000000, 0.8660254037844387076, 1.000000000000000000, 0.8660254037844387076, 1.000000000000000000, 0.8660254037844387076, 1.000000000000000000, 0.8660254037844387076, 1.000000000000000000, 0.8660254037844387076, 1.000000000000000000, 0.8660254037844387076, 1.000000000000000000, 0.8660254037844387076, 1.000000000000000000, 0.8660254037844387076, 1.000000000000000000, 0.8660254037844387076, 1.000000000000000000, 0.8660254037844387076, 1.000000000000000000, 0.8660254037844387076, 1.000000000000000000, 0.8660254037844387076, 1.000000000000000000, 0.8660254037844387076, 1.000000000000000000, 0.8660254037844387076, 1.000000000000000000, 0.8660254037844387076, 1.000000000000000000, 0.8660254037844387076, 1.000000000000000000, 0.8660254037844387076, 1.000000000000000000, 0.8660254037844387076, 1.000000000000000000, 0.8660254037844387076, 1.000000000000000000, 0.8660254037844387076, 1.000000000000000000, 0.8660254037844387076, 1.000000000000000000, 0.8660254037844387076, 1.000000000000000000, 0.8660254037844387076, 1.000000000000000000, 0.8660254037844387076, 1.000000000000000000, 0.8660254037844387076, 1.000000000000000000, 0.8660254037844387076, 1.000000000000000000, 0.8660254037844387076, 1.000000000000000000, 0.8660254037844387076, 1.000000000000000000, 0.8660254037844387076, 1.000000000000000000, 0.8660254037844387076, 1.000000000000000000, 0.8660254037844387076, 1.000000000000000000, 0.8660254037844387076, 1.000000000000000000, 0.8660254037844387076, 1.000000000000000000, 0.8660254037844387076, 1.000000000000000000, 0.8660254037844387076, 1.000000000000000000, 0.8660254037844387076, 1.000000000000000000, 0.8660254037844387076, 1.000000000000000000, 0.8660254037844387076, 1.000000000000000000, 0.8660254037844387076, 1.000000000000000000, 0.8660254037844387076, 1.000000000000000000, 0.8660254037844387076, 1.000000000000000000, 0.8660254037844387076, 1.000000000000000000, 0.8660254037844387076, 1.000000000000000000, 0.8660254037844387076, 1.000000000000000000, 0.8660254037844387076, 1.000000000000000000, 0.8660254037844387076, 1.000000000000000000, 0.8660254037844387076, 1.000000000000000000, 0.8660254037844387076, 1.000000000000000000, 0.8660254037844387076, 1.000000000000000000, 0.8660254037844387076, 1.000000000000000000, 0.8660254037844387076, 1.000000000000000000, 0.8660254037844387076, 1.000000000000000000, 0.8660254037844387076, 1.000000000000000000, 0.8660254037844387076, 1.000000000000000000, 0.8660254037844387076, 1.000000000000000000, 0.8660254037844387076, 1.000000000000000000, 0.8660254037844387076, 1.000000000000000000, 0.8660254037844387076, 1.000000000000000000, 0.8660254037844387076, 1.000000000000000000, 0.8660254037844387076, 1.000000000000000000, 0.8660254037844387076, 1.000000000000000000, 0.8660254037844387076, 1.000000000000000000, 0.8660254037844387076, 1.000000000000000000, 0.8660254037844387076, 1.000000000000000000, 0.8660254037844387076, 1.000000000000000000, 0.8660254037844387076, 1.000000000000000000, 0.8660254037844387076, 1.000000000000000000, 0.8660254037844387076, 1.000000000000000000, 0.8660254037844387076, 1.000000000000000000, 0.8660254037844387076, 1.000000000000000000, 0.8660254037844387076, 1.000000000000000000, 0.8660254037844387076, 1.000000000000000000, 0.8660254037844387076, 1.000000000000000000, 0.8660254037844387076, 1.000000000000000000, 0.8660254037844387076, 1.000000000000000000, 0.8660254037844387076, 1.000000000000000000, 0.8660254037844387076, 1.000000000000000000, 0.8660254037844387076, 1.000000000000000000, 0.8660254037844387076, 1.000000000000000000, 0.8660254037844387076, 1.000000000000000000, 0.8660254037844387076, 1.000000000000000000, 0.8660254037844387076, 1.000000000000000000, 0.8660254037844387076, 1.000000000000000000, 0.8660254037844387076, 1.000000000000000000, 0.8660254037844387076, 1.000000000000000000, 0.8660254037844387076, 1.000000000000000000, 0.8660254037844387076, 1.000000000000000000),
 ( 1.000000000000000000, 0.8660254037844387076, 1.000000000000000000, 0.8660254037844387076, 1.000000000000000000, 0.8660254037844387076, 1.000000000000000000, 0.8660254037844387076, 1.000000000000000000, 0.8660254037844387076, 1.000000000000000000, 0.8660254037844387076, 1.000000000000000000, 0.8660254037844387076, 1.000000000000000000, 0.8660254037844387076, 1.000000000000000000, 0.8660254037844387076, 1.000000000000000000, 0.8660254037844387076, 1.000000000000000000, 0.8660254037844387076, 1.000000000000000000, 0.8660254037844387076, 1.000000000000000000, 0.8660254037844387076, 1.000000000000000000, 0.8660254037844387076, 1.000000000000000000, 0.8660254037844387076, 1.000000000000000000, 0.8660254037844387076, 1.000000000000000000, 0.8660254037844387076, 1.000000000000000000, 0.8660254037844387076, 1.000000000000000000, 0.8660254037844387076, 1.000000000000000000, 0.8660254037844387076, 1.000000000000000000, 0.8660254037844387076, 1.000000000000000000, 0.8660254037844387076, 1.000000000000000000, 0.8660254037844387076, 1.000000000000000000, 0.8660254037844387076, 1.000000000000000000, 0.8660254037844387076, 1.000000000000000000, 0.8660254037844387076, 1.000000000000000000, 0.8660254037844387076, 1.000000000000000000, 0.8660254037844387076, 1.000000000000000000, 0.8660254037844387076, 1.000000000000000000, 0.8660254037844387076, 1.000000000000000000, 0.8660254037844387076, 1.000000000000000000, 0.8660254037844387076, 1.000000000000000000, 0.8660254037844387076, 1.000000000000000000, 0.8660254037844387076, 1.000000000000000000, 0.8660254037844387076, 1.000000000000000000, 0.8660254037844387076, 1.000000000000000000, 0.8660254037844387076, 1.000000000000000000, 0.8660254037844387076, 1.000000000000000000, 0.8660254037844387076, 1.000000000000000000, 0.8660254037844387076, 1.000000000000000000, 0.8660254037844387076, 1.000000000000000000, 0.8660254037844387076, 1.000000000000000000, 0.8660254037844387076, 1.000000000000000000, 0.8660254037844387076, 1.000000000000000000, 0.8660254037844387076, 1.000000000000000000, 0.8660254037844387076, 1.000000000000000000, 0.8660254037844387076, 1.000000000000000000, 0.8660254037844387076, 1.000000000000000000, 0.8660254037844387076, 1.000000000000000000, 0.8660254037844387076, 1.000000000000000000, 0.8660254037844387076, 1.000000000000000000, 0.8660254037844387076, 1.000000000000000000, 0.8660254037844387076, 1.000000000000000000, 0.8660254037844387076, 1.000000000000000000, 0.8660254037844387076, 1.000000000000000000, 0.8660254037844387076, 1.000000000000000000, 0.8660254037844387076, 1.000000000000000000, 0.8660254037844387076, 1.000000000000000000, 0.8660254037844387076, 1.000000000000000000, 0.8660254037844387076, 1.000000000000000000, 0.8660254037844387076, 1.000000000000000000, 0.8660254037844387076, 1.000000000000000000, 0.8660254037844387076, 1.000000000000000000, 0.8660254037844387076, 1.000000000000000000, 0.8660254037844387076, 1.000000000000000000, 0.8660254037844387076, 1.000000000000000000, 0.8660254037844387076, 1.000000000000000000, 0.8660254037844387076, 1.000000000000000000, 0.8660254037844387076, 1.000000000000000000, 0.8660254037844387076, 1.000000000000000000, 0.8660254037844387076, 1.000000000000000000, 0.8660254037844387076, 1.000000000000000000, 0.8660254037844387076, 1.000000000000000000, 0.8660254037844387076, 1.000000000000000000, 0.8660254037844387076, 1.000000000000000000, 0.8660254037844387076, 1.000000000000000000, 0.8660254037844387076, 1.000000000000000000, 0.8660254037844387076, 1.000000000000000000, 0.8660254037844387076, 1.000000000000000000, 0.8660254037844387076, 1.000000000000000000, 0.8660254037844387076, 1.000000000000000000, 0.8660254037844387076, 1.000000000000000000, 0.8660254037844387076, 1.000000000000000000, 0.8660254037844387076, 1.000000000000000000, 0.8660254037844387076, 1.000000000000000000, 0.8660254037844387076, 1.000000000000000000, 0.8660254037844387076, 1.000000000000000000, 0.8660254037844387076, 1.000000000000000000, 0.8660254037844387076, 1.000000000000000000, 0.8660254037844387076, 1.000000000000000000, 0.8660254037844387076, 1.000000000000000000, 0.8660254037844387076, 1.000000000000000000, 0.8660254037844387076, 1.000000000000000000, 0.8660254037844387076, 1.000000000000000000, 0.8660254037844387076, 1.000000000000000000, 0.8660254037844387076, 1.000000000000000000, 0.8660254037844387076, 1.000000000000000000, 0.8660254037844387076, 1.000000000000000000, 0.8660254037844387076, 1.000000000000000000, 0.8660254037844387076, 1.000000000000000000, 0.8660254037844387076, 1.000000000000000000, 0.8660254037844387076, 1.000000000000000000, 0.8660254037844387076, 1.000000000000000000, 0.8660254037844387076, 1.000000000000000000, 0.8660254037844387076, 1.000000000000000000, 0.8660254037844387076, 1.000000000000000000, 0.8660254037844387076, 1.000000000000000000, 0.8660254037844387076, 1.000000000000000000, 0.8660254037844387076, 1.000000000000000000, 0.8660254037844387076, 1.000000000000000000, 0.8660254037844387076, 1.000000000000000000, 0.8660254037844387076, 1.000000000000000000, 0.8660254037844387076, 1.000000000000000000, 0.8660254037844387076, 1.000000000000000000, 0.8660254037844387076, 1.000000000000000000, 0.8660254037844387076, 1.000000000000000000, 0.8660254037844387076, 1.000000000000000000, 0.8660254037844387076, 1.000000000000000000, 0.8660254037844387076, 1.000000000000000000, 0.8660254037844387076, 1.000000000000000000) ) ) 
 REPRESENTATION_ITEM ( '' )  SURFACE ( )  );
#187122 = AXIS2_PLACEMENT_3D ( 'NONE', #98175, #146934, #195664 ) ;
#187123 = CARTESIAN_POINT ( 'NONE',  ( -0.6823417656250003738, 1.967708333674753174, -1.181850606188749264 ) ) ;
#187124 = CARTESIAN_POINT ( 'NONE',  ( -3.689227196694346400, 6.357829925235092716, -1.082531754730546636 ) ) ;
#187126 = ORIENTED_EDGE ( 'NONE', *, *, #79219, .F. ) ;
#187125 = CARTESIAN_POINT ( 'NONE',  ( -5.477130870240893401, 6.452702772444876445, 1.082531754730548412 ) ) ;
#187127 = AXIS2_PLACEMENT_3D ( 'NONE', #29213, #12934, #79014 ) ;
#187128 = CARTESIAN_POINT ( 'NONE',  ( 4.763993809689464065, 0.6627061821620899851, -2.014485251161435286 ) ) ;
#187129 = CARTESIAN_POINT ( 'NONE',  ( -5.144392941742557568, 4.966489618313220333, -0.7998128361456362523 ) ) ;
#187130 = VERTEX_POINT ( 'NONE', #163323 ) ;
#187131 = CARTESIAN_POINT ( 'NONE',  ( 5.471600609837615536, 2.084441204114939161, -0.5725544205837928002 ) ) ;
#187132 = CARTESIAN_POINT ( 'NONE',  ( 4.632082037363250748, 8.555846143565791095, -0.7998128361456231517 ) ) ;
#187133 = CARTESIAN_POINT ( 'NONE',  ( 5.249485218566786848, 1.838879873951340782, -0.09611505855997713732 ) ) ;
#187134 = CARTESIAN_POINT ( 'NONE',  ( -5.733986265252455361, 6.108121862465037744, 0.6873297539724126937 ) ) ;
#187135 = CARTESIAN_POINT ( 'NONE',  ( 1.364683531249988535, 1.676041667008085101, 0.7879004041258500513 ) ) ;
#187136 = CARTESIAN_POINT ( 'NONE',  ( 0.2568327444973814155, 1.721937519821172602, -0.2522849218079876721 ) ) ;
#187137 = CARTESIAN_POINT ( 'NONE',  ( 6.827182134110161726, 7.629137130509051623, 2.510944104600740356 ) ) ;
#187138 = CARTESIAN_POINT ( 'NONE',  ( 1.364683531249986537, -1.073958332991911790, 0.7879004041258500513 ) ) ;
#187139 = CARTESIAN_POINT ( 'NONE',  ( 1.499999999999989120, 6.200000000000045475, -2.579999999999995630 ) ) ;
#187140 = CARTESIAN_POINT ( 'NONE',  ( 3.907220446582274853, 1.852832235905249370, 1.113321777468062823 ) ) ;
#187141 = EDGE_CURVE ( 'NONE', #123984, #201902, #212539, .T. ) ;
#187142 = CARTESIAN_POINT ( 'NONE',  ( -4.786191920824102830, 5.542644314838231168, 1.199719254218462483 ) ) ;
#187143 = CARTESIAN_POINT ( 'NONE',  ( -6.521108698048767138, 10.55178454779148289, -0.7216878364870267237 ) ) ;
#187144 = CARTESIAN_POINT ( 'NONE',  ( 3.344745324850742385, 0.5235245934552492653, 2.097234944377385002 ) ) ;
#187145 = CARTESIAN_POINT ( 'NONE',  ( 4.446526809179438544, 0.5226573815438217974, 1.900768696068744434 ) ) ;
#187146 = CARTESIAN_POINT ( 'NONE',  ( 3.620171223323872756, 0.4232754169638303643, -1.681204106648684693 ) ) ;
#187147 = CARTESIAN_POINT ( 'NONE',  ( 0.9783777488623355278, -2.139296967303818686, -0.4750931833387496694 ) ) ;
#187148 = CARTESIAN_POINT ( 'NONE',  ( 1.237850453945861906, -2.084960033126967982, 0.9891342380793988198 ) ) ;
#187149 = CARTESIAN_POINT ( 'NONE',  ( 3.602854949731192136, 1.626725521824391230, -1.265059968925500211 ) ) ;
#187150 = CARTESIAN_POINT ( 'NONE',  ( 5.741732329385339284, 1.940029712683045915, 0.09120231522616148445 ) ) ;
#187152 = ORIENTED_EDGE ( 'NONE', *, *, #84784, .T. ) ;
#187151 = CARTESIAN_POINT ( 'NONE',  ( -8.663296969008007054, 9.209527340038563992, 0.7216878364870438212 ) ) ;
#187153 = CARTESIAN_POINT ( 'NONE',  ( -6.791708605802965870, 6.888357893050385705, -0.7998128361456362523 ) ) ;
#187154 = FACE_OUTER_BOUND ( 'NONE', #102128, .T. ) ;
#187155 = CARTESIAN_POINT ( 'NONE',  ( -3.142457743317409680, 6.888227477170756785, 0.7998128361456352531 ) ) ;
#187156 = CARTESIAN_POINT ( 'NONE',  ( -8.487040972030346353, 9.003895343564625620, 1.040834085586084257E-14 ) ) ;
#187157 = CARTESIAN_POINT ( 'NONE',  ( 3.962124768131184638, 2.190450126196175074, -0.2673064950309556043 ) ) ;
#187158 = CARTESIAN_POINT ( 'NONE',  ( 0.000000000000000000, -3.434374999522041616, -3.793834371823813001 ) ) ;
#187159 = ORIENTED_EDGE ( 'NONE', *, *, #135726, .T. ) ;
#187160 = CARTESIAN_POINT ( 'NONE',  ( 0.7427237327431088776, -0.2200284318808701234, -1.847805914472876232 ) ) ;
#187161 = CARTESIAN_POINT ( 'NONE',  ( 6.539320575229276677, 6.035451701470580410, 2.698157228745074576 ) ) ;
#187162 = CARTESIAN_POINT ( 'NONE',  ( -1.201851678989727383E-14, 5.618750000682818602, -1.732050807568863648 ) ) ;
#187163 = CARTESIAN_POINT ( 'NONE',  ( 4.203240766677102336, 7.568734712931471265, -0.9219714408205395006 ) ) ;
#187165 = CARTESIAN_POINT ( 'NONE',  ( 6.825078400183550720, 4.691998341648846882, 2.606919129228836507 ) ) ;
#187164 = CARTESIAN_POINT ( 'NONE',  ( 1.499999999999990896, 5.556250000682820378, 1.214306433183764966E-14 ) ) ;
#187166 = CARTESIAN_POINT ( 'NONE',  ( 6.615202361034350886, -1.784545987531281019, 0.4526050685512914007 ) ) ;
#187167 = ORIENTED_EDGE ( 'NONE', *, *, #137354, .F. ) ;
#187168 = CARTESIAN_POINT ( 'NONE',  ( 2.096624111547572777, -0.5486670241920866831, -1.986447216630163659 ) ) ;
#187169 = CARTESIAN_POINT ( 'NONE',  ( -0.6801582343750299797, 0.9322916670080338974, 1.178068619123803451 ) ) ;
#187170 = B_SPLINE_CURVE_WITH_KNOTS ( 'NONE', 3,
 ( #100748, #136470, #5342, #55207, #119197, #121353 ),
 .UNSPECIFIED., .F., .F.,
 ( 4, 2, 4 ),
 ( 0.9260018899588919883, 0.9630662328098654745, 1.000130575660838961 ),
 .UNSPECIFIED. ) ;
#187171 = CARTESIAN_POINT ( 'NONE',  ( -5.371001409308059138, 9.417918744168066070, -0.7998128361456231517 ) ) ;
#187172 = CARTESIAN_POINT ( 'NONE',  ( 10.91804383151480806, -9.907361309732431565, -0.1905751639681794174 ) ) ;
#187173 = FACE_OUTER_BOUND ( 'NONE', #38234, .T. ) ;
#187174 = CARTESIAN_POINT ( 'NONE',  ( 3.822509244049070887, 6.547012320444182798, -1.199719254218452047 ) ) ;
#187175 = CARTESIAN_POINT ( 'NONE',  ( 1.340775744366573541, 0.4011420747369342510, 2.021288966927562214 ) ) ;
#187177 = CARTESIAN_POINT ( 'NONE',  ( 1.364683531249997417, 13.48437500034139980, 2.602085213965210642E-15 ) ) ;
#187176 = CARTESIAN_POINT ( 'NONE',  ( -8.002408263930261612, -6.836568542494980250, 7.346809171966449448 ) ) ;
#187178 = CARTESIAN_POINT ( 'NONE',  ( 5.144429221381498607, 8.089252293998699272, -1.199719254218452047 ) ) ;
#187179 = CARTESIAN_POINT ( 'NONE',  ( 1.802380875475168898, 2.439898602870735456, 2.460315029152825961 ) ) ;
#187180 = CARTESIAN_POINT ( 'NONE',  ( 5.567066847960510323, -1.993696164035433371, -0.9465883713010987410 ) ) ;
#187181 = CARTESIAN_POINT ( 'NONE',  ( 6.608658273995139609, 1.683185115790312603, -1.511970481837302760 ) ) ;
#187182 = CARTESIAN_POINT ( 'NONE',  ( -4.772106882330241717, 5.630174786549132726, -1.082531754730544860 ) ) ;
#187183 = CARTESIAN_POINT ( 'NONE',  ( 0.2637284958507991606, 0.5978344860198721022, -1.816641584731902626 ) ) ;
#187184 = CARTESIAN_POINT ( 'NONE',  ( 0.9367328597341374463, -1.586666764284098807, 1.244388658875786424 ) ) ;
#187185 = CARTESIAN_POINT ( 'NONE',  ( 5.817857313595521163, 9.801600942587855414, -0.7216878364870458196 ) ) ;
#187186 = CARTESIAN_POINT ( 'NONE',  ( 1.441203352352852463, 1.369654091668540241, 1.845602877388529572 ) ) ;
#187187 = CARTESIAN_POINT ( 'NONE',  ( 4.579720705251352442, 8.490788101113528441, 0.3661988261168963588 ) ) ;
#187188 = CARTESIAN_POINT ( 'NONE',  ( 0.4019237886466847653, 12.10491455036742536, 1.499999999999997113 ) ) ;
#187189 = CARTESIAN_POINT ( 'NONE',  ( 1.865214468731738018, 8.973543201141316317, -0.7749999999999996891 ) ) ;
#187190 = AXIS2_PLACEMENT_3D ( 'NONE', #10041, #11098, #93461 ) ;
#187191 = CARTESIAN_POINT ( 'NONE',  ( 1.674454752297813265, -1.775319108138155633, -0.5897529795871117031 ) ) ;
#187192 = CARTESIAN_POINT ( 'NONE',  ( 2.044158018538293042, 0.8666093899718421145, 1.820985203412978093 ) ) ;
#187194 = CARTESIAN_POINT ( 'NONE',  ( -5.586581854188635177, 5.810800913040471194, -0.4357733342581562863 ) ) ;
#187193 = CARTESIAN_POINT ( 'NONE',  ( -1.201851678989727383E-14, 0.8218750003414171390, 1.575800808251672791 ) ) ;
#187196 = CARTESIAN_POINT ( 'NONE',  ( 5.338542076627605937, 2.074711179890481816, 0.3611063368853023592 ) ) ;
#187195 = CARTESIAN_POINT ( 'NONE',  ( -8.528242318195895066, 9.908369778438709474, 1.199719254218462483 ) ) ;
#187197 = CARTESIAN_POINT ( 'NONE',  ( 6.771407655021410399, 9.987393799911945536, -1.199719254218441611 ) ) ;
#187199 = CARTESIAN_POINT ( 'NONE',  ( -8.525379664894808585, 8.840697785332414682, -0.7998128361456291469 ) ) ;
#187198 = CARTESIAN_POINT ( 'NONE',  ( 5.734172623936983904, 5.654565914206774124, 0.7998128361456352531 ) ) ;
#187200 = CARTESIAN_POINT ( 'NONE',  ( 0.01979922387977678389, -6.863887327018420415, -9.496663239506007770 ) ) ;
#187201 = CARTESIAN_POINT ( 'NONE',  ( 4.324476463189423470, -0.8673186339709404447, -1.824254535609586725 ) ) ;
#187202 = CARTESIAN_POINT ( 'NONE',  ( -1.001543065824772872E-14, 5.321875000341422357, 1.575800808251672791 ) ) ;
#187203 = CARTESIAN_POINT ( 'NONE',  ( 6.795384964414455276, -1.844194740592384196, 0.9240657454356243639 ) ) ;
#187204 = CARTESIAN_POINT ( 'NONE',  ( 9.625925876022625616, 11.29296361252366765, -1.082531754730537088 ) ) ;
#187205 = CARTESIAN_POINT ( 'NONE',  ( 5.044278900083454253, 2.155409826167026477, 0.1645634770654491874 ) ) ;
#187206 = CARTESIAN_POINT ( 'NONE',  ( 5.851225812749518695, 8.984124660586543243, -1.199719254218452047 ) ) ;
#187207 = CARTESIAN_POINT ( 'NONE',  ( -1.364683531250014514, -1.157291666325248158, 0.7879004041258379498 ) ) ;
#187209 = FACE_OUTER_BOUND ( 'NONE', #71265, .T. ) ;
#187208 = CARTESIAN_POINT ( 'NONE',  ( 5.773793314573267388, 7.829454515125894964, 1.599625672291268286 ) ) ;
#187210 = CARTESIAN_POINT ( 'NONE',  ( 8.093854517234030155, 8.545177812968924869, -0.7216878364870267237 ) ) ;
#187212 = CARTESIAN_POINT ( 'NONE',  ( 0.01154776750823807881, -8.267087321559200674, 11.00021059652653754 ) ) ;
#187211 = CARTESIAN_POINT ( 'NONE',  ( 2.453800908837290518, 1.677244079947149302, 1.378686777781912065 ) ) ;
#187214 = CARTESIAN_POINT ( 'NONE',  ( 1.593040506729075823, -0.6195558395927207584, 1.734028948791266345 ) ) ;
#187213 = CARTESIAN_POINT ( 'NONE',  ( -6.751597309925468693, 6.979211071108916364, 0.7216878364870317197 ) ) ;
#187215 = CARTESIAN_POINT ( 'NONE',  ( 0.6823417656249899377, 2.842708333674753618, 1.181850606188765695 ) ) ;
#187216 = CARTESIAN_POINT ( 'NONE',  ( 3.579775959861815515, -1.078688530630707243, 1.907616655872627964 ) ) ;
#187217 = CARTESIAN_POINT ( 'NONE',  ( 6.883263157960366030, 0.5727201817382967519, 2.105997115537924902 ) ) ;
#187218 = CARTESIAN_POINT ( 'NONE',  ( 3.907294183660753539, 1.938944517003845736, 1.165763813888931688 ) ) ;
#187219 = CARTESIAN_POINT ( 'NONE',  ( -4.869349725602420520, 8.832658446511480577, 1.040834085586084257E-14 ) ) ;
#187220 = CARTESIAN_POINT ( 'NONE',  ( -0.6823417656249969321, 5.530208333674756283, -1.181850606188749264 ) ) ;
#187221 = CARTESIAN_POINT ( 'NONE',  ( 6.176125489850557315, 6.957122458884915872, -0.8945188991977878201 ) ) ;
#187222 = AXIS2_PLACEMENT_3D ( 'NONE', #184590, #36208, #86041 ) ;
#187223 = CARTESIAN_POINT ( 'NONE',  ( 1.499999999999997113, 13.39583333333333570, -0.8660254037844378194 ) ) ;
#187224 = CARTESIAN_POINT ( 'NONE',  ( 5.478903473698239601, 7.485416367438324059, -1.443375672974078761 ) ) ;
#187225 = CARTESIAN_POINT ( 'NONE',  ( 5.676936032674533728, -0.04454931526533602304, -1.769330457910125443 ) ) ;
#187226 = CARTESIAN_POINT ( 'NONE',  ( 8.392660782059197189, 9.750191319612612872, 1.199719254218462483 ) ) ;
#187227 = CARTESIAN_POINT ( 'NONE',  ( 2.151528103076968179, -1.690815887601760270, -1.255243123012689921 ) ) ;
#187229 = CARTESIAN_POINT ( 'NONE',  ( 1.499999999999987121, 3.045833333333353377, -0.8660254037844262731 ) ) ;
#187228 = CARTESIAN_POINT ( 'NONE',  ( -1.402160292154681736E-14, 11.67187500034140157, 1.575800808251682339 ) ) ;
#187231 = EDGE_CURVE ( 'NONE', #43527, #13744, #18789, .T. ) ;
#187230 = CARTESIAN_POINT ( 'NONE',  ( 0.5902130973520075541, 1.015489506344388282, -1.687439782384107634 ) ) ;
#187232 = CARTESIAN_POINT ( 'NONE',  ( -5.157951095356222204, 4.982307464195829816, 0.000000000000000000 ) ) ;
#187233 = CARTESIAN_POINT ( 'NONE',  ( -0.2863318758520757568, 8.150007921796362353, -2.019927845748578310 ) ) ;
#187235 = ORIENTED_EDGE ( 'NONE', *, *, #66529, .F. ) ;
#187234 = CARTESIAN_POINT ( 'NONE',  ( 6.398695480837623961, -1.778505541023298386, -0.3437013697835926140 ) ) ;
#187236 = CARTESIAN_POINT ( 'NONE',  ( 6.643132081016125845, 6.852668304048034287, 0.7216878364870317197 ) ) ;
#187237 = CARTESIAN_POINT ( 'NONE',  ( -1.402160292154681736E-14, -0.4906249996585810846, -1.575800808251665908 ) ) ;
#187238 = EDGE_CURVE ( 'NONE', #203495, #181928, #167545, .T. ) ;
#187239 = CARTESIAN_POINT ( 'NONE',  ( 4.346470048663173102, 0.4987854378066917116, 1.802870001028591629 ) ) ;
#187240 = CARTESIAN_POINT ( 'NONE',  ( 3.541704441667858472, 5.155074486744371853, -1.599625672291262513 ) ) ;
#187241 = ORIENTED_EDGE ( 'NONE', *, *, #165357, .T. ) ;
#187242 = CARTESIAN_POINT ( 'NONE',  ( 5.928598010555854891, -1.317819122799672504, 1.596621505246295314 ) ) ;
#187243 = CARTESIAN_POINT ( 'NONE',  ( -0.6125000000000089262, 1.791666666666677621, 1.060881119635936232 ) ) ;
#187244 = CARTESIAN_POINT ( 'NONE',  ( -3.784134271545645412, 7.428924060196286483, 0.7216878364870338292 ) ) ;
#187245 = CARTESIAN_POINT ( 'NONE',  ( 1.499999999999985123, -0.2041666666666457353, -0.8660254037844323793 ) ) ;
#187246 = CARTESIAN_POINT ( 'NONE',  ( 6.238723240582662477, 10.43026088065513513, -0.7998128361456291469 ) ) ;
#187247 = CARTESIAN_POINT ( 'NONE',  ( -9.840520565420403543, 10.37502883594562597, 1.040834085586084257E-14 ) ) ;
#187248 = CARTESIAN_POINT ( 'NONE',  ( 6.852720297064418986, 6.959538199522133262, 0.7998128361456331437 ) ) ;
#187249 = CARTESIAN_POINT ( 'NONE',  ( -0.6823417656250246877, 0.05104166700808931978, 1.181850606188755259 ) ) ;
#187251 = EDGE_CURVE ( 'NONE', #55298, #23033, #195244, .T. ) ;
#187250 = CARTESIAN_POINT ( 'NONE',  ( -1.402160292154681736E-14, 0.8375000000000232259, -1.732050807568863648 ) ) ;
#187253 = CARTESIAN_POINT ( 'NONE',  ( 5.606460214450851964, 6.499623990736163037, 1.199719254218462483 ) ) ;
#187252 = CARTESIAN_POINT ( 'NONE',  ( 4.615648854252428102, 0.4318217149890530848, -1.913582009320368371 ) ) ;
#187254 = CARTESIAN_POINT ( 'NONE',  ( 1.669295836627190610, -0.7230268306642473330, -1.882186858670406693 ) ) ;
#187255 = CARTESIAN_POINT ( 'NONE',  ( -0.1108833634137010304, 6.948331553507800962, -2.491992042620773340 ) ) ;
#187256 = CARTESIAN_POINT ( 'NONE',  ( -0.1114211809780316365, -0.4883405756051837354, -2.144353428667714390 ) ) ;
#187257 = CARTESIAN_POINT ( 'NONE',  ( -11.86145016429273014, 19.00000000000000000, -1.180000000000002158 ) ) ;
#187258 = CARTESIAN_POINT ( 'NONE',  ( 2.249088872875557144, -1.499603784168266563, -1.117866018216478574 ) ) ;
#187259 = CARTESIAN_POINT ( 'NONE',  ( 1.364683531249990311, 5.113541667008084879, 0.7879004041258500513 ) ) ;
#187260 = CARTESIAN_POINT ( 'NONE',  ( 3.937747632521654495, -1.925297015496162611, 0.5883167919090799280 ) ) ;
#187261 = CARTESIAN_POINT ( 'NONE',  ( -6.970863535720637216, 11.28442455831609337, 0.7998128361456481317 ) ) ;
#187262 = B_SPLINE_CURVE_WITH_KNOTS ( 'NONE', 3,
 ( #166410, #52662, #118790, #1750, #72086, #182652 ),
 .UNSPECIFIED., .F., .F.,
 ( 4, 2, 4 ),
 ( 0.000000000000000000, 0.0005369603738926351233, 0.001073920747785270247 ),
 .UNSPECIFIED. ) ;
#187264 = CARTESIAN_POINT ( 'NONE',  ( 4.007494584968971374, -2.025512140874039524, 0.6163414799803969002 ) ) ;
#187263 = CARTESIAN_POINT ( 'NONE',  ( -4.392478581147607031, 7.108013530438723748, 1.082531754730560403 ) ) ;
#187265 = DIRECTION ( 'NONE',  ( 0.000000000000000000, 0.000000000000000000, -1.000000000000000000 ) ) ;
#187266 = CARTESIAN_POINT ( 'NONE',  ( 5.793440749948310042, -1.873300974885267589, 0.8818263447485861217 ) ) ;
#187268 = CARTESIAN_POINT ( 'NONE',  ( 6.720655732516639169, 2.430015300743305406, 2.455394564723146100 ) ) ;
#187267 = CARTESIAN_POINT ( 'NONE',  ( 1.013356050919094198, -2.038958350640528661, 0.4616950316734638737 ) ) ;
#187270 = ORIENTED_EDGE ( 'NONE', *, *, #88956, .F. ) ;
#187269 = CARTESIAN_POINT ( 'NONE',  ( 6.036143291503483610, 0.8974207610169572247, -1.589712159477923992 ) ) ;
#187271 = CARTESIAN_POINT ( 'NONE',  ( 7.239163954692881653, 10.53310948286200599, -1.199719254218441611 ) ) ;
#187272 = DIRECTION ( 'NONE',  ( 1.000000000000000000, -1.084202172485501594E-14, 0.000000000000000000 ) ) ;
#187273 = CARTESIAN_POINT ( 'NONE',  ( -9.420034542028389524, 2.999999999999999556, 6.906487091023606695 ) ) ;
#187274 = CARTESIAN_POINT ( 'NONE',  ( 7.253248993186724114, 9.485209796849769504, 1.443375672974076540 ) ) ;
#187275 = CARTESIAN_POINT ( 'NONE',  ( 0.6823417656249934904, 12.75520833367473017, 1.181850606188764807 ) ) ;
#187276 = CARTESIAN_POINT ( 'NONE',  ( 5.953752735127215701, -1.388294428863137586, -1.315342447896154843 ) ) ;
#187277 = CARTESIAN_POINT ( 'NONE',  ( -7.374745490829552885, 10.69128794168811680, -1.199719254218446718 ) ) ;
#187278 = TOROIDAL_SURFACE ( 'NONE', #80129, 10.92000000000000171, 0.08000000000000000167 ) ;
#187279 = CARTESIAN_POINT ( 'NONE',  ( 4.819033534653518025, 7.709623992816043270, -1.199719254218452047 ) ) ;
#187280 = CIRCLE ( 'NONE', #45532, 0.08000000000000020983 ) ;
#187281 = DIRECTION ( 'NONE',  ( -1.224646799147353207E-16, 1.000000000000000000, 0.000000000000000000 ) ) ;
#187282 = CARTESIAN_POINT ( 'NONE',  ( 0.4019237886466884846, 9.926335450315368902, -1.499999999999994449 ) ) ;
#187283 = CARTESIAN_POINT ( 'NONE',  ( 3.277320446201373638, 4.846626492033466072, 1.599625672291267398 ) ) ;
#187284 = VERTEX_POINT ( 'NONE', #122125 ) ;
#187285 = CARTESIAN_POINT ( 'NONE',  ( 6.398064575937244314, -0.9530261711272209890, -1.777004751544956962 ) ) ;
#187286 = CARTESIAN_POINT ( 'NONE',  ( 0.04773460823432121303, -1.936894771697717621, 0.8635138731061947626 ) ) ;
#187287 = DIRECTION ( 'NONE',  ( 0.7806247497458018714, 0.000000000000000000, -0.6250000000674432732 ) ) ;
#187288 = PRODUCT_DEFINITION_CONTEXT ( 'detailed design', #40891, 'design' ) ;
#187289 = CARTESIAN_POINT ( 'NONE',  ( -0.1399997263889819488, 4.088450529495776919, -2.555104583160577203 ) ) ;
#187290 = CARTESIAN_POINT ( 'NONE',  ( -4.229780737783618072, 6.918199379847403740, 1.082531754730560403 ) ) ;
#187291 = CARTESIAN_POINT ( 'NONE',  ( 8.703971430293332645, 12.13808852110884118, -1.082531754730543083 ) ) ;
#187292 = CARTESIAN_POINT ( 'NONE',  ( 3.889471302351163562, -1.821405649934451532, 0.7496272025103620784 ) ) ;
#187293 = EDGE_CURVE ( 'NONE', #149924, #59046, #146863, .T. ) ;
#187294 = CARTESIAN_POINT ( 'NONE',  ( 5.026970340808907700, -1.727993218758390404, 1.039010492973009514 ) ) ;
#187295 = CARTESIAN_POINT ( 'NONE',  ( -5.533699252672048985, 9.607732894759390518, -0.7998128361456231517 ) ) ;
#187296 = CARTESIAN_POINT ( 'NONE',  ( -10.96027417533446346, -7.850147675656140578, 0.3662874062585462220 ) ) ;
#187297 = CARTESIAN_POINT ( 'NONE',  ( 4.962908505822443139, 0.2168217322565080263, -2.180687389885840322 ) ) ;
#187298 = CARTESIAN_POINT ( 'NONE',  ( 3.258729403965909821, -1.459781800624770032, 1.257100956980856443 ) ) ;
#187299 = CARTESIAN_POINT ( 'NONE',  ( -8.019811557683421910, 9.315200557840817908, 1.199719254218462483 ) ) ;
#187300 = ADVANCED_FACE ( 'NONE', ( #86333 ), #50309, .T. ) ;
#187301 = CARTESIAN_POINT ( 'NONE',  ( -0.02948999725182251813, 4.092753722544117956, -2.481335295887850290 ) ) ;
#187302 = CARTESIAN_POINT ( 'NONE',  ( 0.4697016844467936103, 0.2121168557088908557, -2.196667960996725011 ) ) ;
#187303 = DIRECTION ( 'NONE',  ( 0.000000000000000000, -1.000000000000000000, 0.000000000000000000 ) ) ;
#187304 = LINE ( 'NONE', #84751, #191438 ) ;
#187305 =( BOUNDED_SURFACE ( )  B_SPLINE_SURFACE ( 1, 2, ( 
 ( #115203, #32823, #34936, #184387, #133557, #53334, #99956, #83691, #50141, #118401, #180145, #149779, #116263, #98898, #67416, #19755, #164951, #131440, #18686, #199566, #51210, #15482, #66352, #85836, #182254, #49085, #68495, #31771, #16544, #36006, #97841, #197444, #82625, #213669, #117332, #148710, #183330, #101008, #280, #201689, #163906, #167097, #65293, #132496, #151914, #84768, #2418, #198496, #147653, #81567, #134622, #200625, #52274, #102087, #69556, #135666, #24019, #107491, #205975, #22941, #104231, #106408, #91191, #72774, #171347, #170277, #21862, #186528, #38158, #123767, #136733, #8845, #7765, #173517, #73854, #25091, #122704, #41381, #87970, #154044, #5609, #71692, #137805, #207042, #157252, #204891, #203824, #55468, #121624, #20808, #120550, #187593, #119467, #39218, #105309, #138873, #89057, #155114, #57607, #74923, #185455, #6698, #156188, #4546, #54410, #56542, #188667, #189728, #40297, #37077, #172431, #90121, #139949, #141035, #103156, #169217, #86905, #152972, #70619, #202757, #208106, #9912, #111756, #44576, #176688, #108553, #159367, #178836, #143168, #142091, #161520, #146349, #191851, #62928, #58672, #75987, #59734, #92274, #110690, #125892, #160435, #78112, #109634, #80250, #190786, #60802, #158321, #43513, #46707, #61871, #144240, #175640, #26160, #124821, #126960, #210234, #209163, #28301, #10967, #93331, #193990, #27226, #30450, #128036, #77041, #192920, #174584, #94397, #177761, #12041, #45639, #145298, #42449, #29377, #14156, #79183, #95472, #13104, #211303, #195067, #129096, #112822, #96535, #162582, #1102, #35752, #197189, #47784, #48827, #65045, #52018, #132236, #179892, #100753, #64002, #31515, #19494, #150594, #85569, #181993, #149516, #67161, #97590, #113898, #84505, #81319, #163649, #180942, #33626, #15229, #49882, #212361, #101826, #200370, #198244, #116007, #99698, #114942, #68233, #32562, #98639, #199303, #130153, #147395, #29, #165768, #183071, #133297, #213422, #131201, #134366, #167894, #83434, #164698, #16284, #17352, #18431, #118144, #82371, #50948, #2156, #184129, #117073, #34684, #196143, #166835, #148460, #66093, #87709, #185189, #154851, #152708, #155919, #4290, #6435, #168954, #57345, #172171, #72510, #204631, #139689, #119203, #170015, #73587, #56282, #205711, #71433, #120286, #138608, #3229, #21603, #88793, #37895, #201430, #36813, #137545, #38965, #69296, #105050, #106147, #153781, #203563, #5351, #135407, #186261, #23763, #53070, #55215, #107225, #151659, #103973, #188399, #41116, #121361, #187336, #102895, #24829, #173249, #20557, #86641, #171085, #189474, #22681, #54149, #122441, #40035, #70362, #89868, #136476, #7503, #202498, #123509, #141838, #77848, #140766, #45375, #10709, #176432, #156995, #109367, #209964, #78906, #177498, #208900, #75724, #143971, #62658, #44306, #142899, #207844, #59469, #158062, #9648, #95194, #108297, #194798, #193730, #145028, #111490, #211032, #94136, #12832, #125628, #191587, #43248, #175375, #26958, #178565, #128816, #28042, #93065, #159106, #76777, #206778, #92002, #60532, #90929, #126692, #192654, #110428, #160175, #11775, #29111, #46435, #8582, #61604, #127774, #190526, #25892, #161245, #112553, #74662, #58412, #124566, #42182, #174318, #114689, #182810, #30173, #98374, #180681, #31251, #16023, #18163, #179630, #195875, #83171, #82109, #148202, #79981, #130939, #150337, #32307, #113626, #133038, #117888, #163383, #34427, #96262, #47514, #97327, #63732, #214202, #14957, #131981, #49617, #81055, #51768, #162314, #164437, #129891, #147139, #84251, #33362, #115742, #213165, #212096, #13899, #65832, #181731, #197989, #99444, #196932, #64795, #165500, #48570, #1905, #17093, #149255, #828, #146084, #66898, #199037, #50685, #116810, #100500, #166576, #67964, #134108, #200117, #4040, #104794, #86392, #89615, #203314, #151403, #152460, #85320, #52818, #88541, #153533, #2976, #56032, #205463, #70109, #139428, #204375, #20307, #170840, #19240, #138358, #103718, #54964, #35493, #202243, #154603, #171913, #122185, #87465, #168703, #22431, #155666, #137296, #21359, #136222, #53894, #36559, #102647, #188151, #201180, #73326 ),
 ( #72250, #101571, #69044, #57096, #39782, #183881, #5102, #121116, #38714, #135161, #118956, #105888, #184935, #120029, #186005, #71178, #37640, #187081, #167638, #169769, #23510, #6182, #7249, #158864, #174074, #193494, #91757, #157810, #110181, #210798, #24576, #125375, #10461, #93890, #126444, #206530, #124320, #45136, #160998, #208655, #190279, #74419, #43004, #143726, #111246, #8334, #142646, #127523, #177251, #76534, #44062, #12590, #175131, #28863, #191338, #59217, #156744, #192407, #41936, #94950, #108049, #176192, #140518, #78663, #209719, #27792, #159930, #144791, #90683, #109117, #26718, #58162, #11533, #25646, #123261, #9408, #77603, #75479, #189226, #61364, #40866, #106971, #172995, #141591, #207597, #92820, #60285, #198785, #196691, #31010, #49376, #128585, #80812, #213964, #163137, #112313, #96019, #48330, #164193, #194551, #15779, #16840, #212922, #114440, #64556, #46195, #97085, #82922, #178328, #146902, #17900, #62421, #14721, #99195, #166311, #130699, #180440, #162072, #150074, #83986, #29936, #13662, #32057, #100243, #98144, #179390, #81865, #147950, #79734, #50434, #115494, #65584, #145849, #33118, #131731, #211857, #47267, #63493, #113382, #129649, #116553, #197736, #195634, #165246, #181489, #148995, #570, #66637, #132782, #182545, #34171, #70913, #183621, #117630, #88267, #85058, #51504, #184675, #185739, #35228, #53628, #89348, #105609, #204106, #135955, #119760, #37372, #52559, #71983, #36297, #102373, #203050, #1646, #101304, #3769, #103448, #186817, #4833, #151144, #2711, #138093, #39510, #87193, #68785, #167384, #201970, #22152, #55758, #18974, #21090, #5910, #121914, #169508, #137023, #171640, #153258, #187883, #168443, #134904, #200911, #54691, #120843, #67704, #38445, #170570, #152202, #104525, #69844, #133852, #20042, #154335, #118691, #86129, #23237, #199861, #74155, #26458, #109924, #57895, #140249, #123000, #30481, #178869, #205189, #155397, #124058, #6979, #91490, #206270, #157551, #173812, #188957, #126183, #108852, #9147, #56830, #92567, #191080, #73060, #190024, #40597, #41676, #8069, #43811, #75221, #106702, #76281, #172727, #24305, #139159, #90410, #156480, #107787, #25391, #141332, #174878, #42747, #207346, #158607, #10206, #192147, #58967, #142389, #125122, #208398, #60032, #122638, #54348, #38096, #170215, #185393, #204824, #103093, #169152, #121559, #7701, #35947, #136673, #21800, #105244, #137742, #3429, #135603, #56476, #172365, #5547, #201624, #85772, #120487, #155045, #188601, #19694, #153980, #138805, #40232, #87908, #55405, #23955, #186459, #106343, #202698, #70554, #168095, #203762, #53273, #90059, #119404, #187530, #151853, #156119, #6631, #39161, #171284, #134560, #102026, #152905, #200563, #22876, #52210, #104167, #20745, #88992, #118337, #4483, #71629, #184322, #72710, #69496, #37011, #86840, #177414, #111410, #212013, #193648, #196851, #96182, #44227, #45290, #192572, #160093, #195791, #46354, #110349, #163295, #98295, #29032, #32222, #97241, #127688, #63656, #126609, #31168, #210952, #162233, #139880, #95115, #47429, #64711, #14876, #194714, #61522, #129811, #48488, #30093, #128740, #161164, #12750, #143890, #209884, #80968, #94052, #180597, #179547, #130854, #147060, #114606, #79893, #213080, #78824, #144945, #62578, #112473, #178482, #164357, #73784, #13820, #146003, #113544, #208822, #176352, #77770, #60452, #27959, #11696, #18077, #183796, #84164, #150252, #102551, #3952, #82025, #51683, #52730, #115656, #165414, #17010, #85227, #20216, #35405, #103631, #1820, #67878, #100415, #168614, #15941, #134024, #166485, #83086, #200031, #70019, #149165, #181651, #68955, #117804, #101483, #65748, #116722, #136135, #167553, #99363, #118864, #148117, #742, #86304, #214120, #33278, #66808, #49532, #19154, #132950, #151316, #2884, #198955, #37551, #131894, #135076, #50597, #182722, #202151, #201089, #184850, #34341, #197902, #36478, #152374, #53812, #119941, #185917, #109060, #95967, #143672, #212870, #179338, #210746, #110127, #11478, #27739, #26663, #126391, #127468, #125325, #176139, #193439, #78612, #45083, #111192, #211804, #113331, #191285, #160947, #162021 ) ),
 .UNSPECIFIED., .F., .F., .T. ) 
 B_SPLINE_SURFACE_WITH_KNOTS ( ( 2, 2 ),
 ( 3, 2, 2, 2, 2, 2, 2, 2, 2, 2, 2, 2, 2, 2, 2, 2, 2, 2, 2, 2, 2, 2, 2, 2, 2, 2, 2, 2, 2, 2, 2, 2, 2, 2, 2, 2, 2, 2, 2, 2, 2, 2, 2, 2, 2, 2, 2, 2, 2, 2, 2, 2, 2, 2, 2, 2, 2, 2, 2, 2, 2, 2, 2, 2, 2, 2, 2, 2, 2, 2, 2, 2, 2, 2, 2, 2, 2, 2, 2, 2, 2, 2, 2, 2, 2, 2, 2, 2, 2, 2, 2, 2, 2, 2, 2, 2, 2, 2, 2, 2, 2, 2, 2, 2, 2, 2, 2, 2, 2, 2, 2, 2, 2, 2, 2, 2, 2, 2, 2, 2, 2, 2, 2, 2, 2, 2, 2, 2, 2, 2, 2, 2, 2, 2, 2, 2, 2, 2, 2, 2, 2, 2, 2, 2, 2, 2, 2, 2, 2, 2, 2, 2, 2, 2, 2, 2, 2, 2, 2, 2, 2, 2, 2, 2, 2, 2, 2, 2, 2, 2, 2, 2, 2, 2, 2, 2, 2, 2, 2, 2, 2, 2, 2, 2, 2, 2, 2, 2, 2, 2, 2, 2, 2, 2, 2, 2, 2, 2, 2, 2, 2, 2, 2, 2, 2, 2, 2, 2, 2, 2, 2, 2, 2, 2, 2, 2, 2, 2, 2, 2, 2, 2, 2, 2, 2, 2, 2, 2, 2, 2, 2, 2, 2, 2, 2, 2, 2, 2, 2, 2, 3 ),
 ( 0.000000000000000000, 1.000000000000000000 ),
 ( 0.000000000000000000, 0.004166666666666666609, 0.008333333333333333218, 0.01250000000000000069, 0.01666666666666666644, 0.02083333333333333218, 0.02500000000000000139, 0.02916666666666666713, 0.03333333333333333287, 0.03749999999999999861, 0.04166666666666666435, 0.04583333333333333010, 0.05000000000000000278, 0.05416666666666666852, 0.05833333333333333426, 0.06250000000000000000, 0.06666666666666666574, 0.07083333333333333148, 0.07499999999999999722, 0.07916666666666666297, 0.08333333333333332871, 0.08749999999999999445, 0.09166666666666666019, 0.09583333333333333981, 0.1000000000000000056, 0.1041666666666666713, 0.1083333333333333370, 0.1125000000000000028, 0.1166666666666666685, 0.1208333333333333343, 0.1250000000000000000, 0.1291666666666666796, 0.1333333333333333315, 0.1375000000000000111, 0.1416666666666666630, 0.1458333333333333426, 0.1499999999999999944, 0.1541666666666666741, 0.1583333333333333259, 0.1625000000000000056, 0.1666666666666666574, 0.1708333333333333370, 0.1749999999999999889, 0.1791666666666666685, 0.1833333333333333204, 0.1875000000000000000, 0.1916666666666666796, 0.1958333333333333315, 0.2000000000000000111, 0.2041666666666666630, 0.2083333333333333426, 0.2124999999999999944, 0.2166666666666666741, 0.2208333333333333259, 0.2250000000000000056, 0.2291666666666666574, 0.2333333333333333370, 0.2374999999999999889, 0.2416666666666666685, 0.2458333333333333204, 0.2500000000000000000, 0.2541666666666666519, 0.2583333333333333592, 0.2625000000000000111, 0.2666666666666666630, 0.2708333333333333148, 0.2750000000000000222, 0.2791666666666666741, 0.2833333333333333259, 0.2874999999999999778, 0.2916666666666666852, 0.2958333333333333370, 0.2999999999999999889, 0.3041666666666666408, 0.3083333333333333481, 0.3125000000000000000, 0.3166666666666666519, 0.3208333333333333592, 0.3250000000000000111, 0.3291666666666666630, 0.3333333333333333148, 0.3375000000000000222, 0.3416666666666666741, 0.3458333333333333259, 0.3499999999999999778, 0.3541666666666666852, 0.3583333333333333370, 0.3624999999999999889, 0.3666666666666666408, 0.3708333333333333481, 0.3750000000000000000, 0.3791666666666666519, 0.3833333333333333592, 0.3875000000000000111, 0.3916666666666666630, 0.3958333333333333148, 0.4000000000000000222, 0.4041666666666666741, 0.4083333333333333259, 0.4124999999999999778, 0.4166666666666666852, 0.4208333333333333370, 0.4249999999999999889, 0.4291666666666666408, 0.4333333333333333481, 0.4375000000000000000, 0.4416666666666666519, 0.4458333333333333592, 0.4500000000000000111, 0.4541666666666666630, 0.4583333333333333148, 0.4625000000000000222, 0.4666666666666666741, 0.4708333333333333259, 0.4749999999999999778, 0.4791666666666666852, 0.4833333333333333370, 0.4874999999999999889, 0.4916666666666666408, 0.4958333333333333481, 0.5000000000000000000, 0.5041666666666666519, 0.5083333333333333037, 0.5124999999999999556, 0.5166666666666667185, 0.5208333333333333703, 0.5250000000000000222, 0.5291666666666666741, 0.5333333333333333259, 0.5374999999999999778, 0.5416666666666666297, 0.5458333333333332815, 0.5500000000000000444, 0.5541666666666666963, 0.5583333333333333481, 0.5625000000000000000, 0.5666666666666666519, 0.5708333333333333037, 0.5749999999999999556, 0.5791666666666667185, 0.5833333333333333703, 0.5875000000000000222, 0.5916666666666666741, 0.5958333333333333259, 0.5999999999999999778, 0.6041666666666666297, 0.6083333333333332815, 0.6125000000000000444, 0.6166666666666666963, 0.6208333333333333481, 0.6250000000000000000, 0.6291666666666666519, 0.6333333333333333037, 0.6374999999999999556, 0.6416666666666667185, 0.6458333333333333703, 0.6500000000000000222, 0.6541666666666666741, 0.6583333333333333259, 0.6624999999999999778, 0.6666666666666666297, 0.6708333333333332815, 0.6750000000000000444, 0.6791666666666666963, 0.6833333333333333481, 0.6875000000000000000, 0.6916666666666666519, 0.6958333333333333037, 0.6999999999999999556, 0.7041666666666667185, 0.7083333333333333703, 0.7125000000000000222, 0.7166666666666666741, 0.7208333333333333259, 0.7249999999999999778, 0.7291666666666666297, 0.7333333333333332815, 0.7375000000000000444, 0.7416666666666666963, 0.7458333333333333481, 0.7500000000000000000, 0.7541666666666666519, 0.7583333333333333037, 0.7624999999999999556, 0.7666666666666667185, 0.7708333333333333703, 0.7750000000000000222, 0.7791666666666666741, 0.7833333333333333259, 0.7874999999999999778, 0.7916666666666666297, 0.7958333333333332815, 0.8000000000000000444, 0.8041666666666666963, 0.8083333333333333481, 0.8125000000000000000, 0.8166666666666666519, 0.8208333333333333037, 0.8249999999999999556, 0.8291666666666667185, 0.8333333333333333703, 0.8375000000000000222, 0.8416666666666666741, 0.8458333333333333259, 0.8499999999999999778, 0.8541666666666666297, 0.8583333333333332815, 0.8625000000000000444, 0.8666666666666666963, 0.8708333333333333481, 0.8750000000000000000, 0.8791666666666666519, 0.8833333333333333037, 0.8874999999999999556, 0.8916666666666667185, 0.8958333333333333703, 0.9000000000000000222, 0.9041666666666666741, 0.9083333333333333259, 0.9124999999999999778, 0.9166666666666666297, 0.9208333333333332815, 0.9250000000000000444, 0.9291666666666666963, 0.9333333333333333481, 0.9375000000000000000, 0.9416666666666666519, 0.9458333333333333037, 0.9499999999999999556, 0.9541666666666667185, 0.9583333333333333703, 0.9625000000000000222, 0.9666666666666666741, 0.9708333333333333259, 0.9749999999999999778, 0.9791666666666666297, 0.9833333333333332815, 0.9875000000000000444, 0.9916666666666666963, 0.9958333333333333481, 1.000000000000000000 ),
 .UNSPECIFIED. ) 
 GEOMETRIC_REPRESENTATION_ITEM ( )  RATIONAL_B_SPLINE_SURFACE ( (
 ( 1.000000000000000000, 0.8660254037844387076, 1.000000000000000000, 0.8660254037844387076, 1.000000000000000000, 0.8660254037844387076, 1.000000000000000000, 0.8660254037844387076, 1.000000000000000000, 0.8660254037844387076, 1.000000000000000000, 0.8660254037844387076, 1.000000000000000000, 0.8660254037844387076, 1.000000000000000000, 0.8660254037844387076, 1.000000000000000000, 0.8660254037844387076, 1.000000000000000000, 0.8660254037844387076, 1.000000000000000000, 0.8660254037844387076, 1.000000000000000000, 0.8660254037844387076, 1.000000000000000000, 0.8660254037844387076, 1.000000000000000000, 0.8660254037844387076, 1.000000000000000000, 0.8660254037844387076, 1.000000000000000000, 0.8660254037844387076, 1.000000000000000000, 0.8660254037844387076, 1.000000000000000000, 0.8660254037844387076, 1.000000000000000000, 0.8660254037844387076, 1.000000000000000000, 0.8660254037844387076, 1.000000000000000000, 0.8660254037844387076, 1.000000000000000000, 0.8660254037844387076, 1.000000000000000000, 0.8660254037844387076, 1.000000000000000000, 0.8660254037844387076, 1.000000000000000000, 0.8660254037844387076, 1.000000000000000000, 0.8660254037844387076, 1.000000000000000000, 0.8660254037844387076, 1.000000000000000000, 0.8660254037844387076, 1.000000000000000000, 0.8660254037844387076, 1.000000000000000000, 0.8660254037844387076, 1.000000000000000000, 0.8660254037844387076, 1.000000000000000000, 0.8660254037844387076, 1.000000000000000000, 0.8660254037844387076, 1.000000000000000000, 0.8660254037844387076, 1.000000000000000000, 0.8660254037844387076, 1.000000000000000000, 0.8660254037844387076, 1.000000000000000000, 0.8660254037844387076, 1.000000000000000000, 0.8660254037844387076, 1.000000000000000000, 0.8660254037844387076, 1.000000000000000000, 0.8660254037844387076, 1.000000000000000000, 0.8660254037844387076, 1.000000000000000000, 0.8660254037844387076, 1.000000000000000000, 0.8660254037844387076, 1.000000000000000000, 0.8660254037844387076, 1.000000000000000000, 0.8660254037844387076, 1.000000000000000000, 0.8660254037844387076, 1.000000000000000000, 0.8660254037844387076, 1.000000000000000000, 0.8660254037844387076, 1.000000000000000000, 0.8660254037844387076, 1.000000000000000000, 0.8660254037844387076, 1.000000000000000000, 0.8660254037844387076, 1.000000000000000000, 0.8660254037844387076, 1.000000000000000000, 0.8660254037844387076, 1.000000000000000000, 0.8660254037844387076, 1.000000000000000000, 0.8660254037844387076, 1.000000000000000000, 0.8660254037844387076, 1.000000000000000000, 0.8660254037844387076, 1.000000000000000000, 0.8660254037844387076, 1.000000000000000000, 0.8660254037844387076, 1.000000000000000000, 0.8660254037844387076, 1.000000000000000000, 0.8660254037844387076, 1.000000000000000000, 0.8660254037844387076, 1.000000000000000000, 0.8660254037844387076, 1.000000000000000000, 0.8660254037844387076, 1.000000000000000000, 0.8660254037844387076, 1.000000000000000000, 0.8660254037844387076, 1.000000000000000000, 0.8660254037844387076, 1.000000000000000000, 0.8660254037844387076, 1.000000000000000000, 0.8660254037844387076, 1.000000000000000000, 0.8660254037844387076, 1.000000000000000000, 0.8660254037844387076, 1.000000000000000000, 0.8660254037844387076, 1.000000000000000000, 0.8660254037844387076, 1.000000000000000000, 0.8660254037844387076, 1.000000000000000000, 0.8660254037844387076, 1.000000000000000000, 0.8660254037844387076, 1.000000000000000000, 0.8660254037844387076, 1.000000000000000000, 0.8660254037844387076, 1.000000000000000000, 0.8660254037844387076, 1.000000000000000000, 0.8660254037844387076, 1.000000000000000000, 0.8660254037844387076, 1.000000000000000000, 0.8660254037844387076, 1.000000000000000000, 0.8660254037844387076, 1.000000000000000000, 0.8660254037844387076, 1.000000000000000000, 0.8660254037844387076, 1.000000000000000000, 0.8660254037844387076, 1.000000000000000000, 0.8660254037844387076, 1.000000000000000000, 0.8660254037844387076, 1.000000000000000000, 0.8660254037844387076, 1.000000000000000000, 0.8660254037844387076, 1.000000000000000000, 0.8660254037844387076, 1.000000000000000000, 0.8660254037844387076, 1.000000000000000000, 0.8660254037844387076, 1.000000000000000000, 0.8660254037844387076, 1.000000000000000000, 0.8660254037844387076, 1.000000000000000000, 0.8660254037844387076, 1.000000000000000000, 0.8660254037844387076, 1.000000000000000000, 0.8660254037844387076, 1.000000000000000000, 0.8660254037844387076, 1.000000000000000000, 0.8660254037844387076, 1.000000000000000000, 0.8660254037844387076, 1.000000000000000000, 0.8660254037844387076, 1.000000000000000000, 0.8660254037844387076, 1.000000000000000000, 0.8660254037844387076, 1.000000000000000000, 0.8660254037844387076, 1.000000000000000000, 0.8660254037844387076, 1.000000000000000000, 0.8660254037844387076, 1.000000000000000000, 0.8660254037844387076, 1.000000000000000000, 0.8660254037844387076, 1.000000000000000000, 0.8660254037844387076, 1.000000000000000000, 0.8660254037844387076, 1.000000000000000000, 0.8660254037844387076, 1.000000000000000000, 0.8660254037844387076, 1.000000000000000000, 0.8660254037844387076, 1.000000000000000000, 0.8660254037844387076, 1.000000000000000000, 0.8660254037844387076, 1.000000000000000000, 0.8660254037844387076, 1.000000000000000000, 0.8660254037844387076, 1.000000000000000000, 0.8660254037844387076, 1.000000000000000000, 0.8660254037844387076, 1.000000000000000000, 0.8660254037844387076, 1.000000000000000000, 0.8660254037844387076, 1.000000000000000000, 0.8660254037844387076, 1.000000000000000000, 0.8660254037844387076, 1.000000000000000000, 0.8660254037844387076, 1.000000000000000000, 0.8660254037844387076, 1.000000000000000000, 0.8660254037844387076, 1.000000000000000000, 0.8660254037844387076, 1.000000000000000000, 0.8660254037844387076, 1.000000000000000000, 0.8660254037844387076, 1.000000000000000000, 0.8660254037844387076, 1.000000000000000000, 0.8660254037844387076, 1.000000000000000000, 0.8660254037844387076, 1.000000000000000000, 0.8660254037844387076, 1.000000000000000000, 0.8660254037844387076, 1.000000000000000000, 0.8660254037844387076, 1.000000000000000000, 0.8660254037844387076, 1.000000000000000000, 0.8660254037844387076, 1.000000000000000000, 0.8660254037844387076, 1.000000000000000000, 0.8660254037844387076, 1.000000000000000000, 0.8660254037844387076, 1.000000000000000000, 0.8660254037844387076, 1.000000000000000000, 0.8660254037844387076, 1.000000000000000000, 0.8660254037844387076, 1.000000000000000000, 0.8660254037844387076, 1.000000000000000000, 0.8660254037844387076, 1.000000000000000000, 0.8660254037844387076, 1.000000000000000000, 0.8660254037844387076, 1.000000000000000000, 0.8660254037844387076, 1.000000000000000000, 0.8660254037844387076, 1.000000000000000000, 0.8660254037844387076, 1.000000000000000000, 0.8660254037844387076, 1.000000000000000000, 0.8660254037844387076, 1.000000000000000000, 0.8660254037844387076, 1.000000000000000000, 0.8660254037844387076, 1.000000000000000000, 0.8660254037844387076, 1.000000000000000000, 0.8660254037844387076, 1.000000000000000000, 0.8660254037844387076, 1.000000000000000000, 0.8660254037844387076, 1.000000000000000000, 0.8660254037844387076, 1.000000000000000000, 0.8660254037844387076, 1.000000000000000000, 0.8660254037844387076, 1.000000000000000000, 0.8660254037844387076, 1.000000000000000000, 0.8660254037844387076, 1.000000000000000000, 0.8660254037844387076, 1.000000000000000000, 0.8660254037844387076, 1.000000000000000000, 0.8660254037844387076, 1.000000000000000000, 0.8660254037844387076, 1.000000000000000000, 0.8660254037844387076, 1.000000000000000000, 0.8660254037844387076, 1.000000000000000000, 0.8660254037844387076, 1.000000000000000000, 0.8660254037844387076, 1.000000000000000000, 0.8660254037844387076, 1.000000000000000000, 0.8660254037844387076, 1.000000000000000000, 0.8660254037844387076, 1.000000000000000000, 0.8660254037844387076, 1.000000000000000000, 0.8660254037844387076, 1.000000000000000000, 0.8660254037844387076, 1.000000000000000000, 0.8660254037844387076, 1.000000000000000000, 0.8660254037844387076, 1.000000000000000000, 0.8660254037844387076, 1.000000000000000000, 0.8660254037844387076, 1.000000000000000000, 0.8660254037844387076, 1.000000000000000000, 0.8660254037844387076, 1.000000000000000000, 0.8660254037844387076, 1.000000000000000000, 0.8660254037844387076, 1.000000000000000000, 0.8660254037844387076, 1.000000000000000000, 0.8660254037844387076, 1.000000000000000000, 0.8660254037844387076, 1.000000000000000000, 0.8660254037844387076, 1.000000000000000000, 0.8660254037844387076, 1.000000000000000000, 0.8660254037844387076, 1.000000000000000000, 0.8660254037844387076, 1.000000000000000000, 0.8660254037844387076, 1.000000000000000000, 0.8660254037844387076, 1.000000000000000000, 0.8660254037844387076, 1.000000000000000000, 0.8660254037844387076, 1.000000000000000000, 0.8660254037844387076, 1.000000000000000000, 0.8660254037844387076, 1.000000000000000000, 0.8660254037844387076, 1.000000000000000000, 0.8660254037844387076, 1.000000000000000000, 0.8660254037844387076, 1.000000000000000000, 0.8660254037844387076, 1.000000000000000000, 0.8660254037844387076, 1.000000000000000000, 0.8660254037844387076, 1.000000000000000000, 0.8660254037844387076, 1.000000000000000000, 0.8660254037844387076, 1.000000000000000000, 0.8660254037844387076, 1.000000000000000000, 0.8660254037844387076, 1.000000000000000000, 0.8660254037844387076, 1.000000000000000000, 0.8660254037844387076, 1.000000000000000000, 0.8660254037844387076, 1.000000000000000000, 0.8660254037844387076, 1.000000000000000000, 0.8660254037844387076, 1.000000000000000000, 0.8660254037844387076, 1.000000000000000000, 0.8660254037844387076, 1.000000000000000000, 0.8660254037844387076, 1.000000000000000000, 0.8660254037844387076, 1.000000000000000000, 0.8660254037844387076, 1.000000000000000000, 0.8660254037844387076, 1.000000000000000000, 0.8660254037844387076, 1.000000000000000000, 0.8660254037844387076, 1.000000000000000000, 0.8660254037844387076, 1.000000000000000000, 0.8660254037844387076, 1.000000000000000000, 0.8660254037844387076, 1.000000000000000000, 0.8660254037844387076, 1.000000000000000000, 0.8660254037844387076, 1.000000000000000000, 0.8660254037844387076, 1.000000000000000000, 0.8660254037844387076, 1.000000000000000000, 0.8660254037844387076, 1.000000000000000000, 0.8660254037844387076, 1.000000000000000000, 0.8660254037844387076, 1.000000000000000000, 0.8660254037844387076, 1.000000000000000000, 0.8660254037844387076, 1.000000000000000000, 0.8660254037844387076, 1.000000000000000000, 0.8660254037844387076, 1.000000000000000000, 0.8660254037844387076, 1.000000000000000000, 0.8660254037844387076, 1.000000000000000000, 0.8660254037844387076, 1.000000000000000000, 0.8660254037844387076, 1.000000000000000000),
 ( 1.000000000000000000, 0.8660254037844387076, 1.000000000000000000, 0.8660254037844387076, 1.000000000000000000, 0.8660254037844387076, 1.000000000000000000, 0.8660254037844387076, 1.000000000000000000, 0.8660254037844387076, 1.000000000000000000, 0.8660254037844387076, 1.000000000000000000, 0.8660254037844387076, 1.000000000000000000, 0.8660254037844387076, 1.000000000000000000, 0.8660254037844387076, 1.000000000000000000, 0.8660254037844387076, 1.000000000000000000, 0.8660254037844387076, 1.000000000000000000, 0.8660254037844387076, 1.000000000000000000, 0.8660254037844387076, 1.000000000000000000, 0.8660254037844387076, 1.000000000000000000, 0.8660254037844387076, 1.000000000000000000, 0.8660254037844387076, 1.000000000000000000, 0.8660254037844387076, 1.000000000000000000, 0.8660254037844387076, 1.000000000000000000, 0.8660254037844387076, 1.000000000000000000, 0.8660254037844387076, 1.000000000000000000, 0.8660254037844387076, 1.000000000000000000, 0.8660254037844387076, 1.000000000000000000, 0.8660254037844387076, 1.000000000000000000, 0.8660254037844387076, 1.000000000000000000, 0.8660254037844387076, 1.000000000000000000, 0.8660254037844387076, 1.000000000000000000, 0.8660254037844387076, 1.000000000000000000, 0.8660254037844387076, 1.000000000000000000, 0.8660254037844387076, 1.000000000000000000, 0.8660254037844387076, 1.000000000000000000, 0.8660254037844387076, 1.000000000000000000, 0.8660254037844387076, 1.000000000000000000, 0.8660254037844387076, 1.000000000000000000, 0.8660254037844387076, 1.000000000000000000, 0.8660254037844387076, 1.000000000000000000, 0.8660254037844387076, 1.000000000000000000, 0.8660254037844387076, 1.000000000000000000, 0.8660254037844387076, 1.000000000000000000, 0.8660254037844387076, 1.000000000000000000, 0.8660254037844387076, 1.000000000000000000, 0.8660254037844387076, 1.000000000000000000, 0.8660254037844387076, 1.000000000000000000, 0.8660254037844387076, 1.000000000000000000, 0.8660254037844387076, 1.000000000000000000, 0.8660254037844387076, 1.000000000000000000, 0.8660254037844387076, 1.000000000000000000, 0.8660254037844387076, 1.000000000000000000, 0.8660254037844387076, 1.000000000000000000, 0.8660254037844387076, 1.000000000000000000, 0.8660254037844387076, 1.000000000000000000, 0.8660254037844387076, 1.000000000000000000, 0.8660254037844387076, 1.000000000000000000, 0.8660254037844387076, 1.000000000000000000, 0.8660254037844387076, 1.000000000000000000, 0.8660254037844387076, 1.000000000000000000, 0.8660254037844387076, 1.000000000000000000, 0.8660254037844387076, 1.000000000000000000, 0.8660254037844387076, 1.000000000000000000, 0.8660254037844387076, 1.000000000000000000, 0.8660254037844387076, 1.000000000000000000, 0.8660254037844387076, 1.000000000000000000, 0.8660254037844387076, 1.000000000000000000, 0.8660254037844387076, 1.000000000000000000, 0.8660254037844387076, 1.000000000000000000, 0.8660254037844387076, 1.000000000000000000, 0.8660254037844387076, 1.000000000000000000, 0.8660254037844387076, 1.000000000000000000, 0.8660254037844387076, 1.000000000000000000, 0.8660254037844387076, 1.000000000000000000, 0.8660254037844387076, 1.000000000000000000, 0.8660254037844387076, 1.000000000000000000, 0.8660254037844387076, 1.000000000000000000, 0.8660254037844387076, 1.000000000000000000, 0.8660254037844387076, 1.000000000000000000, 0.8660254037844387076, 1.000000000000000000, 0.8660254037844387076, 1.000000000000000000, 0.8660254037844387076, 1.000000000000000000, 0.8660254037844387076, 1.000000000000000000, 0.8660254037844387076, 1.000000000000000000, 0.8660254037844387076, 1.000000000000000000, 0.8660254037844387076, 1.000000000000000000, 0.8660254037844387076, 1.000000000000000000, 0.8660254037844387076, 1.000000000000000000, 0.8660254037844387076, 1.000000000000000000, 0.8660254037844387076, 1.000000000000000000, 0.8660254037844387076, 1.000000000000000000, 0.8660254037844387076, 1.000000000000000000, 0.8660254037844387076, 1.000000000000000000, 0.8660254037844387076, 1.000000000000000000, 0.8660254037844387076, 1.000000000000000000, 0.8660254037844387076, 1.000000000000000000, 0.8660254037844387076, 1.000000000000000000, 0.8660254037844387076, 1.000000000000000000, 0.8660254037844387076, 1.000000000000000000, 0.8660254037844387076, 1.000000000000000000, 0.8660254037844387076, 1.000000000000000000, 0.8660254037844387076, 1.000000000000000000, 0.8660254037844387076, 1.000000000000000000, 0.8660254037844387076, 1.000000000000000000, 0.8660254037844387076, 1.000000000000000000, 0.8660254037844387076, 1.000000000000000000, 0.8660254037844387076, 1.000000000000000000, 0.8660254037844387076, 1.000000000000000000, 0.8660254037844387076, 1.000000000000000000, 0.8660254037844387076, 1.000000000000000000, 0.8660254037844387076, 1.000000000000000000, 0.8660254037844387076, 1.000000000000000000, 0.8660254037844387076, 1.000000000000000000, 0.8660254037844387076, 1.000000000000000000, 0.8660254037844387076, 1.000000000000000000, 0.8660254037844387076, 1.000000000000000000, 0.8660254037844387076, 1.000000000000000000, 0.8660254037844387076, 1.000000000000000000, 0.8660254037844387076, 1.000000000000000000, 0.8660254037844387076, 1.000000000000000000, 0.8660254037844387076, 1.000000000000000000, 0.8660254037844387076, 1.000000000000000000, 0.8660254037844387076, 1.000000000000000000, 0.8660254037844387076, 1.000000000000000000, 0.8660254037844387076, 1.000000000000000000, 0.8660254037844387076, 1.000000000000000000, 0.8660254037844387076, 1.000000000000000000, 0.8660254037844387076, 1.000000000000000000, 0.8660254037844387076, 1.000000000000000000, 0.8660254037844387076, 1.000000000000000000, 0.8660254037844387076, 1.000000000000000000, 0.8660254037844387076, 1.000000000000000000, 0.8660254037844387076, 1.000000000000000000, 0.8660254037844387076, 1.000000000000000000, 0.8660254037844387076, 1.000000000000000000, 0.8660254037844387076, 1.000000000000000000, 0.8660254037844387076, 1.000000000000000000, 0.8660254037844387076, 1.000000000000000000, 0.8660254037844387076, 1.000000000000000000, 0.8660254037844387076, 1.000000000000000000, 0.8660254037844387076, 1.000000000000000000, 0.8660254037844387076, 1.000000000000000000, 0.8660254037844387076, 1.000000000000000000, 0.8660254037844387076, 1.000000000000000000, 0.8660254037844387076, 1.000000000000000000, 0.8660254037844387076, 1.000000000000000000, 0.8660254037844387076, 1.000000000000000000, 0.8660254037844387076, 1.000000000000000000, 0.8660254037844387076, 1.000000000000000000, 0.8660254037844387076, 1.000000000000000000, 0.8660254037844387076, 1.000000000000000000, 0.8660254037844387076, 1.000000000000000000, 0.8660254037844387076, 1.000000000000000000, 0.8660254037844387076, 1.000000000000000000, 0.8660254037844387076, 1.000000000000000000, 0.8660254037844387076, 1.000000000000000000, 0.8660254037844387076, 1.000000000000000000, 0.8660254037844387076, 1.000000000000000000, 0.8660254037844387076, 1.000000000000000000, 0.8660254037844387076, 1.000000000000000000, 0.8660254037844387076, 1.000000000000000000, 0.8660254037844387076, 1.000000000000000000, 0.8660254037844387076, 1.000000000000000000, 0.8660254037844387076, 1.000000000000000000, 0.8660254037844387076, 1.000000000000000000, 0.8660254037844387076, 1.000000000000000000, 0.8660254037844387076, 1.000000000000000000, 0.8660254037844387076, 1.000000000000000000, 0.8660254037844387076, 1.000000000000000000, 0.8660254037844387076, 1.000000000000000000, 0.8660254037844387076, 1.000000000000000000, 0.8660254037844387076, 1.000000000000000000, 0.8660254037844387076, 1.000000000000000000, 0.8660254037844387076, 1.000000000000000000, 0.8660254037844387076, 1.000000000000000000, 0.8660254037844387076, 1.000000000000000000, 0.8660254037844387076, 1.000000000000000000, 0.8660254037844387076, 1.000000000000000000, 0.8660254037844387076, 1.000000000000000000, 0.8660254037844387076, 1.000000000000000000, 0.8660254037844387076, 1.000000000000000000, 0.8660254037844387076, 1.000000000000000000, 0.8660254037844387076, 1.000000000000000000, 0.8660254037844387076, 1.000000000000000000, 0.8660254037844387076, 1.000000000000000000, 0.8660254037844387076, 1.000000000000000000, 0.8660254037844387076, 1.000000000000000000, 0.8660254037844387076, 1.000000000000000000, 0.8660254037844387076, 1.000000000000000000, 0.8660254037844387076, 1.000000000000000000, 0.8660254037844387076, 1.000000000000000000, 0.8660254037844387076, 1.000000000000000000, 0.8660254037844387076, 1.000000000000000000, 0.8660254037844387076, 1.000000000000000000, 0.8660254037844387076, 1.000000000000000000, 0.8660254037844387076, 1.000000000000000000, 0.8660254037844387076, 1.000000000000000000, 0.8660254037844387076, 1.000000000000000000, 0.8660254037844387076, 1.000000000000000000, 0.8660254037844387076, 1.000000000000000000, 0.8660254037844387076, 1.000000000000000000, 0.8660254037844387076, 1.000000000000000000, 0.8660254037844387076, 1.000000000000000000, 0.8660254037844387076, 1.000000000000000000, 0.8660254037844387076, 1.000000000000000000, 0.8660254037844387076, 1.000000000000000000, 0.8660254037844387076, 1.000000000000000000, 0.8660254037844387076, 1.000000000000000000, 0.8660254037844387076, 1.000000000000000000, 0.8660254037844387076, 1.000000000000000000, 0.8660254037844387076, 1.000000000000000000, 0.8660254037844387076, 1.000000000000000000, 0.8660254037844387076, 1.000000000000000000, 0.8660254037844387076, 1.000000000000000000, 0.8660254037844387076, 1.000000000000000000, 0.8660254037844387076, 1.000000000000000000, 0.8660254037844387076, 1.000000000000000000, 0.8660254037844387076, 1.000000000000000000, 0.8660254037844387076, 1.000000000000000000, 0.8660254037844387076, 1.000000000000000000, 0.8660254037844387076, 1.000000000000000000, 0.8660254037844387076, 1.000000000000000000, 0.8660254037844387076, 1.000000000000000000, 0.8660254037844387076, 1.000000000000000000, 0.8660254037844387076, 1.000000000000000000, 0.8660254037844387076, 1.000000000000000000, 0.8660254037844387076, 1.000000000000000000, 0.8660254037844387076, 1.000000000000000000, 0.8660254037844387076, 1.000000000000000000, 0.8660254037844387076, 1.000000000000000000, 0.8660254037844387076, 1.000000000000000000, 0.8660254037844387076, 1.000000000000000000, 0.8660254037844387076, 1.000000000000000000, 0.8660254037844387076, 1.000000000000000000, 0.8660254037844387076, 1.000000000000000000, 0.8660254037844387076, 1.000000000000000000, 0.8660254037844387076, 1.000000000000000000, 0.8660254037844387076, 1.000000000000000000, 0.8660254037844387076, 1.000000000000000000, 0.8660254037844387076, 1.000000000000000000, 0.8660254037844387076, 1.000000000000000000, 0.8660254037844387076, 1.000000000000000000, 0.8660254037844387076, 1.000000000000000000, 0.8660254037844387076, 1.000000000000000000, 0.8660254037844387076, 1.000000000000000000) ) ) 
 REPRESENTATION_ITEM ( '' )  SURFACE ( )  );
#187306 = ORIENTED_EDGE ( 'NONE', *, *, #182547, .T. ) ;
#187307 = CARTESIAN_POINT ( 'NONE',  ( 5.750066545971570520, 5.881034856487848295, -0.7216878364870458196 ) ) ;
#187308 = CARTESIAN_POINT ( 'NONE',  ( 5.260591308972474067, -0.6599101888420509932, -1.855755260766891235 ) ) ;
#187309 = EDGE_LOOP ( 'NONE', ( #57748, #25066, #134338, #163281 ) ) ;
#187311 = CARTESIAN_POINT ( 'NONE',  ( 4.090493406365951934, -1.157184705539246794, 1.647087716845529126 ) ) ;
#187310 = CARTESIAN_POINT ( 'NONE',  ( 0.9076408456279178028, -0.8746481411591797706, -1.734042483418346547 ) ) ;
#187312 = CARTESIAN_POINT ( 'NONE',  ( 5.659591354751080772, -0.5502123075824224552, -2.231479479524396403 ) ) ;
#187313 = CARTESIAN_POINT ( 'NONE',  ( 3.713571355222999415, 0.4562380391235145161, -1.803994140785330602 ) ) ;
#187314 = CARTESIAN_POINT ( 'NONE',  ( 7.472478939787284169, 8.746922180287201698, 1.199719254218452935 ) ) ;
#187315 = DIRECTION ( 'NONE',  ( 0.000000000000000000, 1.000000000000000000, 0.000000000000000000 ) ) ;
#187316 =( LENGTH_UNIT ( ) NAMED_UNIT ( * ) SI_UNIT ( .MILLI., .METRE. ) );
#187317 = CARTESIAN_POINT ( 'NONE',  ( -5.208303565944065738, 9.228104593576741621, -0.7998128361456231517 ) ) ;
#187318 = CARTESIAN_POINT ( 'NONE',  ( -5.492461627311929995, 5.580495784718250363, 0.000000000000000000 ) ) ;
#187319 = CARTESIAN_POINT ( 'NONE',  ( 6.532766951017621615, -1.867387138063754337, 0.9404246163645290091 ) ) ;
#187320 = CARTESIAN_POINT ( 'NONE',  ( 4.500943810056890371, 8.194925511800951412, -0.7216878364870207285 ) ) ;
#187321 = EDGE_LOOP ( 'NONE', ( #191925, #52735, #5906, #116487 ) ) ;
#187322 = CARTESIAN_POINT ( 'NONE',  ( -0.01856135223283512589, 6.487495393664096888, 3.100011470320014340 ) ) ;
#187323 = CARTESIAN_POINT ( 'NONE',  ( -11.04536101718726293, 12.59542727035991661, 1.099999999999998757 ) ) ;
#187324 = CARTESIAN_POINT ( 'NONE',  ( 0.1701549220758866166, -1.195335944658926230, 1.380069390326914336 ) ) ;
#187325 = CARTESIAN_POINT ( 'NONE',  ( -6.437424008390261854, 6.404749519410410485, 0.7998128361456341429 ) ) ;
#187326 = CARTESIAN_POINT ( 'NONE',  ( 2.179902339641195397, 1.341075392948913425, 1.099452185880249067 ) ) ;
#187327 = CARTESIAN_POINT ( 'NONE',  ( -10.38813158755799471, 2.629643693813620065, -6.007251501586706510 ) ) ;
#187328 = CARTESIAN_POINT ( 'NONE',  ( 6.509000000000048303, 2.074227158855263209, 2.209070705210983032 ) ) ;
#187329 = CARTESIAN_POINT ( 'NONE',  ( -6.826694039680798021, 7.923230120171105284, -1.199719254218446718 ) ) ;
#187330 = CARTESIAN_POINT ( 'NONE',  ( -5.862481816454102379, 6.029744924107142801, -0.3769115147483664274 ) ) ;
#187331 = CARTESIAN_POINT ( 'NONE',  ( 6.578989008465588206, 2.022637127319019790, 0.7894149679951308896 ) ) ;
#187332 = CARTESIAN_POINT ( 'NONE',  ( 6.076747101522134820, -1.735163100867884500, -0.5679748894881069265 ) ) ;
#187333 = CARTESIAN_POINT ( 'NONE',  ( 2.992962298452766845, 0.2353761085502041883, 1.947492218917420637 ) ) ;
#187334 = CARTESIAN_POINT ( 'NONE',  ( -1.225000000000038058, -0.6666666659838712539, 0.7072540797572637317 ) ) ;
#187335 = CARTESIAN_POINT ( 'NONE',  ( -9.854078719034067291, 10.39084668182823634, 0.7998128361456462443 ) ) ;
#187336 = CARTESIAN_POINT ( 'NONE',  ( 6.089583550832340819, 10.25626457594641749, 1.040834085586084257E-14 ) ) ;
#187337 = CARTESIAN_POINT ( 'NONE',  ( 3.756581929197760683, 2.110411401290826383, 0.2062832702387565331 ) ) ;
#187338 = CARTESIAN_POINT ( 'NONE',  ( 7.693325821111733021, 7.940244644243982464, -0.7998128361456341429 ) ) ;
#187339 = CARTESIAN_POINT ( 'NONE',  ( -7.974166903131914452, 12.45494515362926435, -0.7998128361456281477 ) ) ;
#187340 = CIRCLE ( 'NONE', #166634, 0.07999999999999998779 ) ;
#187341 = CARTESIAN_POINT ( 'NONE',  ( 1.745070579777140418, -0.2997347613497360896, -2.048299739058518920 ) ) ;
#187342 = CARTESIAN_POINT ( 'NONE',  ( -1.364683531250014514, -0.9072916663252470482, 0.7879004041258379498 ) ) ;
#187344 = ORIENTED_EDGE ( 'NONE', *, *, #49372, .F. ) ;
#187343 = CARTESIAN_POINT ( 'NONE',  ( 4.160924129468469346, 0.5925846814045959698, 2.140718581676650079 ) ) ;
#187345 = CARTESIAN_POINT ( 'NONE',  ( 2.075183622135381434, -0.9789826713841279782, 2.079913408810558195 ) ) ;
#187347 = CARTESIAN_POINT ( 'NONE',  ( 6.297729475711208558, -1.489980986158835119, -1.426453875638087343 ) ) ;
#187346 = CARTESIAN_POINT ( 'NONE',  ( 8.405692050792682224, 12.75046512599275772, -0.7216878364870328300 ) ) ;
#187349 = CARTESIAN_POINT ( 'NONE',  ( 2.520459450608881991, -4.091624429771669291, -2.338646429533238535 ) ) ;
#187348 = CARTESIAN_POINT ( 'NONE',  ( 7.078765600110826561, 8.391552967285011988, -1.082531754730548412 ) ) ;
#187350 = DIRECTION ( 'NONE',  ( 0.000000000000000000, 1.000000000000000000, 0.000000000000000000 ) ) ;
#187351 = ORIENTED_EDGE ( 'NONE', *, *, #104398, .F. ) ;
#187352 = CARTESIAN_POINT ( 'NONE',  ( -5.711861010086065171, 6.121870493066576380, -0.7247779672692231667 ) ) ;
#187353 = CARTESIAN_POINT ( 'NONE',  ( 2.548957913124219044, 0.2380835140640499836, 1.897471792728817386 ) ) ;
#187354 = CARTESIAN_POINT ( 'NONE',  ( 0.9311234436981545848, -1.153130369558482027, -3.474999999999999201 ) ) ;
#187355 = CARTESIAN_POINT ( 'NONE',  ( 4.172648073627690302, -1.609630772656017950, -0.6200716988599298540 ) ) ;
#187356 = CARTESIAN_POINT ( 'NONE',  ( 2.079314900164643820, 1.561883299538203929, 1.275554356156020086 ) ) ;
#187357 = CARTESIAN_POINT ( 'NONE',  ( 4.272342533241332063, 2.053246469231550630, -1.033699615426456830 ) ) ;
#187358 = CARTESIAN_POINT ( 'NONE',  ( 4.042437229998629533, 2.251021955006918596, 0.2269351218320627694 ) ) ;
#187359 = CARTESIAN_POINT ( 'NONE',  ( 6.252575686221216955, 0.6590897193336446858, 2.000345064990595390 ) ) ;
#187360 = CARTESIAN_POINT ( 'NONE',  ( -5.099275172515603138, 8.002885897026576600, 1.082531754730549967 ) ) ;
#187361 = EDGE_LOOP ( 'NONE', ( #143180, #151118, #87411, #24872 ) ) ;
#187362 = CARTESIAN_POINT ( 'NONE',  ( 4.217836599137672060, -0.9083132443464863037, -1.518676986326646938 ) ) ;
#187364 = CARTESIAN_POINT ( 'NONE',  ( 0.7797068561936998377, 1.543341569868655450, 1.695032692825575005 ) ) ;
#187363 = CARTESIAN_POINT ( 'NONE',  ( 6.851666526859736983, 9.086973262793417661, -1.599625672291269396 ) ) ;
#187365 = CARTESIAN_POINT ( 'NONE',  ( 6.175717916360309090, -0.9808100270635997653, 1.557957644481674730 ) ) ;
#187366 = CARTESIAN_POINT ( 'NONE',  ( -3.164938793786285842, 5.779846795137578930, -1.199719254218452935 ) ) ;
#187367 = CARTESIAN_POINT ( 'NONE',  ( 5.261759291836726860, 1.077959533075742993, 1.907929976554381346 ) ) ;
#187368 = CARTESIAN_POINT ( 'NONE',  ( -5.143339171537843590, 7.093924681584509173, 1.599625672291263179 ) ) ;
#187369 = CARTESIAN_POINT ( 'NONE',  ( -2.449219305563052895, 6.009172956465517856, 1.040834085586084257E-14 ) ) ;
#187370 = CARTESIAN_POINT ( 'NONE',  ( -3.058251533181919335, 15.44822376919687024, 11.56640689338974148 ) ) ;
#187371 = CARTESIAN_POINT ( 'NONE',  ( 5.969205681473694902, 1.824102622056431811, 0.9793482939001868504 ) ) ;
#187372 = CARTESIAN_POINT ( 'NONE',  ( 1.165250339122084533, 1.861343190080061882, -0.7762330495894869120 ) ) ;
#187373 = CARTESIAN_POINT ( 'NONE',  ( 1.499999999999987121, -1.214583332650518432, 0.8660254037844524744 ) ) ;
#187374 = CARTESIAN_POINT ( 'NONE',  ( 4.775960602080351336, 1.110526314841601359, 1.574030653434669746 ) ) ;
#187375 = CARTESIAN_POINT ( 'NONE',  ( -0.6823417656250039265, 10.81770833367473550, -1.181850606188755259 ) ) ;
#187376 = CARTESIAN_POINT ( 'NONE',  ( 0.7740458967449159733, 0.4260312260581029520, -2.180030009307607042 ) ) ;
#187378 = EDGE_LOOP ( 'NONE', ( #162917, #91034, #3175, #71258, #121910 ) ) ;
#187377 = CARTESIAN_POINT ( 'NONE',  ( 3.984117037569365305, 5.741498858621315371, 1.599625672291261402 ) ) ;
#187380 = CARTESIAN_POINT ( 'NONE',  ( 1.423205080756922314, 7.980384757729337863, 10.65537363484301459 ) ) ;
#187379 = DIRECTION ( 'NONE',  ( 0.000000000000000000, 0.000000000000000000, 1.000000000000000000 ) ) ;
#187381 = CARTESIAN_POINT ( 'NONE',  ( 10.56588178375152864, 11.22128359066528169, -0.7998128361456281477 ) ) ;
#187382 = DIRECTION ( 'NONE',  ( -0.7592566023653004592, -0.6507913734559639396, -0.000000000000000000 ) ) ;
#187383 = CARTESIAN_POINT ( 'NONE',  ( 11.82917762496792946, 7.768082351849152190, 1.754661222088528483 ) ) ;
#187385 = CARTESIAN_POINT ( 'NONE',  ( 2.875390130891414042, -0.1950805366632331617, 1.952157403750237163 ) ) ;
#187384 = AXIS2_PLACEMENT_3D ( 'NONE', #107990, #189166, #206473 ) ;
#187387 = CARTESIAN_POINT ( 'NONE',  ( 1.364683531249986537, 2.717708333674754062, -0.7879004041258239610 ) ) ;
#187386 = CARTESIAN_POINT ( 'NONE',  ( 6.498435699651741615, 6.475929825882159818, -0.7998128361456281477 ) ) ;
#187388 = CARTESIAN_POINT ( 'NONE',  ( 0.000000000000000000, 4.400000000000001243, 0.000000000000000000 ) ) ;
#187389 = CARTESIAN_POINT ( 'NONE',  ( 6.883263157960391787, -0.001104538646235289417, 1.946037152736757925 ) ) ;
#187390 = CARTESIAN_POINT ( 'NONE',  ( -8.565000355531095622, 11.01558638625153286, -1.599625672291263179 ) ) ;
#187391 = CARTESIAN_POINT ( 'NONE',  ( -4.080641047588914994, 5.783833860318930320, -1.443375672974051449 ) ) ;
#187392 = CARTESIAN_POINT ( 'NONE',  ( 0.2689492781585648418, -1.474829822998312778, 1.715830925988118816 ) ) ;
#187394 = ORIENTED_EDGE ( 'NONE', *, *, #198353, .T. ) ;
#187393 = CARTESIAN_POINT ( 'NONE',  ( -4.869349725602420520, 8.832658446511480577, 1.040834085586084257E-14 ) ) ;
#187395 = CARTESIAN_POINT ( 'NONE',  ( -0.6823417656250212460, 5.301041667008086655, 1.181850606188767472 ) ) ;
#187396 = CARTESIAN_POINT ( 'NONE',  ( 1.141631569582121974, 0.7634220068381203372, -1.707866752806507460 ) ) ;
#187397 = CARTESIAN_POINT ( 'NONE',  ( 6.837244271306878396, -1.062160112102826126, 1.370476690187643731 ) ) ;
#187399 = CARTESIAN_POINT ( 'NONE',  ( 3.685266855566126321, 1.588411730319793769, 1.510178839762461811 ) ) ;
#187398 = CARTESIAN_POINT ( 'NONE',  ( 0.6801582343750004478, 2.057291667008069425, -1.178068619123876282 ) ) ;
#187400 = CARTESIAN_POINT ( 'NONE',  ( 5.333197341169245043, 0.1633263742753125747, 2.301865194068336784 ) ) ;
#187401 = CARTESIAN_POINT ( 'NONE',  ( 0.5497720567373615141, 0.6472090466588500401, -1.956683156177397853 ) ) ;
#187402 = CARTESIAN_POINT ( 'NONE',  ( 2.519391418834667995, -1.118305101016278558, -1.587446049422422956 ) ) ;
#187403 = CARTESIAN_POINT ( 'NONE',  ( -5.300874872818844175, 7.207439989753867238, 1.443375672974064550 ) ) ;
#187404 = EDGE_CURVE ( 'NONE', #182455, #13289, #15397, .T. ) ;
#187405 = PRESENTATION_STYLE_ASSIGNMENT (( #138684 ) ) ;
#187406 = CARTESIAN_POINT ( 'NONE',  ( 5.072158865288243668, 6.050511776658669127, 1.082531754730549078 ) ) ;
#187407 = CARTESIAN_POINT ( 'NONE',  ( -1.360316468750006669, 0.1614583336747227316, 0.7853790794158981292 ) ) ;
#187408 = CARTESIAN_POINT ( 'NONE',  ( 3.586564705785996843, -0.5826563296015655480, 1.930417576838711957 ) ) ;
#187409 = CARTESIAN_POINT ( 'NONE',  ( -5.233084104750526322, 5.207612331738130429, 0.000000000000000000 ) ) ;
#187410 = CARTESIAN_POINT ( 'NONE',  ( -6.794571259104023930, 7.956029886156682274, 1.199719254218452047 ) ) ;
#187411 = CARTESIAN_POINT ( 'NONE',  ( 8.615316546479974136, 12.13862083994696839, 1.199719254218450271 ) ) ;
#187413 = CARTESIAN_POINT ( 'NONE',  ( 0.000000000000000000, 13.49999999999999822, -1.500000000000000222 ) ) ;
#187412 = CARTESIAN_POINT ( 'NONE',  ( 0.7151340513122245168, -0.2707656271505008982, 1.805370379145049275 ) ) ;
#187414 = CARTESIAN_POINT ( 'NONE',  ( -7.110325215724114578, 7.260077271291732082, 0.000000000000000000 ) ) ;
#187415 = CARTESIAN_POINT ( 'NONE',  ( -4.118644803501354978, 8.027112380718707030, 0.7998128361456350310 ) ) ;
#187416 = CARTESIAN_POINT ( 'NONE',  ( -10.78913822082115281, 5.463154562124156399, 6.589184675844935057 ) ) ;
#187417 = VERTEX_POINT ( 'NONE', #212526 ) ;
#187418 = CARTESIAN_POINT ( 'NONE',  ( 6.578986920187222864, -0.09832028258810160404, -2.058664976587327722 ) ) ;
#187419 = CARTESIAN_POINT ( 'NONE',  ( -7.444835747235459600, 8.818634805597074688, 1.082531754730549078 ) ) ;
#187420 = UNCERTAINTY_MEASURE_WITH_UNIT (LENGTH_MEASURE( 1.000000000000000082E-05 ), #37613, 'distance_accuracy_value', 'NONE');
#187421 = CARTESIAN_POINT ( 'NONE',  ( -0.7500000000000006661, 11.73958333401613174, -1.299038105676657340 ) ) ;
#187422 = FACE_OUTER_BOUND ( 'NONE', #91949, .T. ) ;
#187423 = CARTESIAN_POINT ( 'NONE',  ( 2.969872605471105764, 6.605953636083951253, 0.1972538285620730192 ) ) ;
#187424 = CARTESIAN_POINT ( 'NONE',  ( 5.250651393837939551, 1.990147761501987800, 0.3430726210427292311 ) ) ;
#187426 = VERTEX_POINT ( 'NONE', #81479 ) ;
#187425 = CARTESIAN_POINT ( 'NONE',  ( 5.742908703533418091, 2.140221812536883927, 0.5945068574613203705 ) ) ;
#187427 = CARTESIAN_POINT ( 'NONE',  ( -5.354544322754380303, 5.211666229493680191, 0.7998128361456281477 ) ) ;
#187428 = CARTESIAN_POINT ( 'NONE',  ( 4.808338034340912337, 8.761478140039733020, 1.040834085586084257E-14 ) ) ;
#187429 = CARTESIAN_POINT ( 'NONE',  ( 4.979397702276197712, 1.923710689106904015, -0.7398180773239333430 ) ) ;
#187430 = CARTESIAN_POINT ( 'NONE',  ( 3.516250148862578584, -1.862017090670412767, 0.7743150488077471527 ) ) ;
#187431 = EDGE_LOOP ( 'NONE', ( #144217, #53097, #14862 ) ) ;
#187432 = DIRECTION ( 'NONE',  ( 0.000000000000000000, 0.000000000000000000, -1.000000000000000000 ) ) ;
#187433 = CARTESIAN_POINT ( 'NONE',  ( 4.379447312414087357, 5.068108938359919158, -1.199719254218452047 ) ) ;
#187434 =( GEOMETRIC_REPRESENTATION_CONTEXT ( 3 ) GLOBAL_UNCERTAINTY_ASSIGNED_CONTEXT ( ( #140288 ) ) GLOBAL_UNIT_ASSIGNED_CONTEXT ( ( #112870, #213467, #192969 ) ) REPRESENTATION_CONTEXT ( 'NONE', 'WORKASPACE' ) );
#187436 = ORIENTED_EDGE ( 'NONE', *, *, #92993, .T. ) ;
#187435 = CARTESIAN_POINT ( 'NONE',  ( -5.986807348886189040, 9.142303119412650503, -1.199719254218452047 ) ) ;
#187437 = CARTESIAN_POINT ( 'NONE',  ( 5.441225816562971218, 7.512442699629209741, -1.249814574298679926 ) ) ;
#187438 = CARTESIAN_POINT ( 'NONE',  ( 4.270861128529729989, -2.010896307770511537, 0.1455111863851859810 ) ) ;
#187439 = CARTESIAN_POINT ( 'NONE',  ( 3.943160212656390051, 0.6185462545997171269, -1.734258544408360470 ) ) ;
#187440 = VECTOR ( 'NONE', #53837, 1000.000000000000227 ) ;
#187441 = CARTESIAN_POINT ( 'NONE',  ( 7.006746397889299871, 6.052176462752766106, 2.500000000000000444 ) ) ;
#187442 = CARTESIAN_POINT ( 'NONE',  ( 2.473609491499198398, 0.1116694970143172483, -2.305109432965181337 ) ) ;
#187443 = CARTESIAN_POINT ( 'NONE',  ( 5.086243903782109221, 5.962981304947771122, -1.199719254218452047 ) ) ;
#187444 = CARTESIAN_POINT ( 'NONE',  ( 3.567792053227138105, 2.109782723108716063, -0.4697668898906853796 ) ) ;
#187445 = CARTESIAN_POINT ( 'NONE',  ( 9.433775957010412938, 9.900493459467314850, 0.000000000000000000 ) ) ;
#187446 = CARTESIAN_POINT ( 'NONE',  ( -4.388035272317281077, 8.271124917678806199, 0.7998128361456481317 ) ) ;
#187447 = ADVANCED_FACE ( 'NONE', ( #66252 ), #70727, .T. ) ;
#187448 = CARTESIAN_POINT ( 'NONE',  ( 3.075839645193487293, 1.666627022722726670, -1.582919517265988674 ) ) ;
#187449 = DIRECTION ( 'NONE',  ( -0.000000000000000000, 1.000000000000000000, 0.000000000000000000 ) ) ;
#187450 = CARTESIAN_POINT ( 'NONE',  ( 2.236979667955760309, -1.672073921526989748, 0.8388852543278202401 ) ) ;
#187451 = CARTESIAN_POINT ( 'NONE',  ( 0.6496080044469240145, 0.6224236735355732630, -1.870565628188630702 ) ) ;
#187453 = CARTESIAN_POINT ( 'NONE',  ( -7.099629715411508890, 8.311931418515415615, 1.199719254218452047 ) ) ;
#187452 = CARTESIAN_POINT ( 'NONE',  ( -1.364683531250010295, 5.280208333674758059, 0.7879004041258379498 ) ) ;
#187455 = CARTESIAN_POINT ( 'NONE',  ( 1.647397727484143592, -1.863059487452220386, 1.182652941231487453 ) ) ;
#187454 = CARTESIAN_POINT ( 'NONE',  ( -6.573005544526917099, 6.562927978236513304, -0.7998128361456291469 ) ) ;
#187456 = ORIENTED_EDGE ( 'NONE', *, *, #172795, .F. ) ;
#187457 = CARTESIAN_POINT ( 'NONE',  ( -2.788906526875773208E-15, 10.18750000000000000, -1.499999999999998446 ) ) ;
#187458 = CARTESIAN_POINT ( 'NONE',  ( 6.030679399980265920, 5.930214142932100252, -0.7998128361456281477 ) ) ;
#187459 = CARTESIAN_POINT ( 'NONE',  ( -5.949330478298285207, 5.835307067636438028, 0.7998128361456341429 ) ) ;
#187460 = CARTESIAN_POINT ( 'NONE',  ( 11.95359438122010864, 13.60421899708691562, 1.059536798430457338 ) ) ;
#187461 = CARTESIAN_POINT ( 'NONE',  ( 5.875845355493965805, 1.173799634058709129, 1.583810875030462695 ) ) ;
#187462 = CARTESIAN_POINT ( 'NONE',  ( 5.496783081331708232, -0.5556612750647730303, -2.239684525637525514 ) ) ;
#187463 = CARTESIAN_POINT ( 'NONE',  ( 6.742638014206057129, -1.825417518414352180, -0.3614582840437295941 ) ) ;
#187464 = CARTESIAN_POINT ( 'NONE',  ( 3.133693747638730098, 1.960048766001153631, -0.6424893143618380931 ) ) ;
#187465 = CARTESIAN_POINT ( 'NONE',  ( 5.477130870240836558, 9.333810415348903433, -0.7216878364870267237 ) ) ;
#187466 = CARTESIAN_POINT ( 'NONE',  ( 5.110497557708379546, 4.926945003606695295, -0.7998128361456481317 ) ) ;
#187467 = CARTESIAN_POINT ( 'NONE',  ( 7.253248993186731219, 8.524840582548424806, 1.082531754730558626 ) ) ;
#187468 = CARTESIAN_POINT ( 'NONE',  ( -1.364683531249997417, 3.821875000341416584, 1.214306433183764966E-14 ) ) ;
#187469 = CARTESIAN_POINT ( 'NONE',  ( -9.906966810501817378, 3.509494795930026001, -6.775981647894812276 ) ) ;
#187470 = CARTESIAN_POINT ( 'NONE',  ( 5.517805330637495231, 6.500156309574290248, -1.082531754730543083 ) ) ;
#187471 = CARTESIAN_POINT ( 'NONE',  ( 6.426262541905297887, 1.110578645885337501, 1.865513821534901417 ) ) ;
#187473 = CARTESIAN_POINT ( 'NONE',  ( 5.337399561049260832, 0.7408347518493042516, -1.685818907712175019 ) ) ;
#187472 = CARTESIAN_POINT ( 'NONE',  ( 6.727182134110222478, 0.005875948494733079785, 1.810970247402940547 ) ) ;
#187474 = DIRECTION ( 'NONE',  ( -1.000000000000000000, 2.168404344971003504E-14, -0.000000000000000000 ) ) ;
#187475 = CARTESIAN_POINT ( 'NONE',  ( 0.3585786437626807821, 3.975028841772350052, 0.9637995837462361992 ) ) ;
#187476 = CARTESIAN_POINT ( 'NONE',  ( 0.5087955169046609605, 1.624258005607306599, 0.9276666955444977658 ) ) ;
#187477 = EDGE_CURVE ( 'NONE', #107724, #184758, #120563, .T. ) ;
#187478 = CARTESIAN_POINT ( 'NONE',  ( -5.283800884368243800, 6.573997454655339467, 1.390413726763789937 ) ) ;
#187479 = CARTESIAN_POINT ( 'NONE',  ( 0.04469781632471583888, 2.590841079414101245, 2.082512688130889966 ) ) ;
#187480 = CARTESIAN_POINT ( 'NONE',  ( 6.367678427751853221, 6.924687757192571347, 0.8275186136274095272 ) ) ;
#187481 = AXIS2_PLACEMENT_3D ( 'NONE', #59143, #157734, #25570 ) ;
#187482 = CARTESIAN_POINT ( 'NONE',  ( 0.1527893875182678718, 0.3269112364552365091, 1.883972597190447518 ) ) ;
#187483 = CARTESIAN_POINT ( 'NONE',  ( 2.412676795855304590, 1.579722209848779313, 0.7981720169879211735 ) ) ;
#187484 = CARTESIAN_POINT ( 'NONE',  ( 0.08246951281144777879, -1.249137507218839094, 1.448023666807838117 ) ) ;
#187486 = CARTESIAN_POINT ( 'NONE',  ( 4.728101222851567975, 1.910784947378706855, 0.1365434035073622987 ) ) ;
#187485 = CARTESIAN_POINT ( 'NONE',  ( -7.994504133552415404, 12.47867192245318435, -0.7998128361456281477 ) ) ;
#187487 = DIRECTION ( 'NONE',  ( -0.7592566023652995710, -0.6507913734559650498, 0.000000000000000000 ) ) ;
#187488 = CARTESIAN_POINT ( 'NONE',  ( 5.283641479639247684, -1.870778298764510961, 0.6161543930274359093 ) ) ;
#187489 = CARTESIAN_POINT ( 'NONE',  ( -0.2046613956954954905, -0.1581703332043625232, -2.086340352340488646 ) ) ;
#187490 = CARTESIAN_POINT ( 'NONE',  ( -0.7500000000000179856, 11.04166666666666430, 1.299038105676658228 ) ) ;
#187491 = CARTESIAN_POINT ( 'NONE',  ( 3.291731440620565330, -0.7593194595177065187, 1.709801165022284408 ) ) ;
#187493 = ORIENTED_EDGE ( 'NONE', *, *, #153604, .F. ) ;
#187492 = CARTESIAN_POINT ( 'NONE',  ( 6.393153111415212031, 1.496800677787715639, -0.8570667202875602575 ) ) ;
#187495 = CARTESIAN_POINT ( 'NONE',  ( 2.738383840280320669, 6.138605547061593448, 0.7216878364870338292 ) ) ;
#187494 = CARTESIAN_POINT ( 'NONE',  ( 1.928631425534212074, 1.268998755960360603, -1.805353087401928569 ) ) ;
#187496 = CARTESIAN_POINT ( 'NONE',  ( -1.364683531249997417, 3.821875000341416584, 1.214306433183764966E-14 ) ) ;
#187497 = CARTESIAN_POINT ( 'NONE',  ( 0.2212323960570794501, -1.841704181501323312, -0.9290775759197547057 ) ) ;
#187498 = CARTESIAN_POINT ( 'NONE',  ( 7.182068686937156166, 9.402166106225269715, 1.599625672291281386 ) ) ;
#187499 = CARTESIAN_POINT ( 'NONE',  ( -9.992522908471816123, 11.61669713376064372, 1.199719254218462483 ) ) ;
#187500 = CARTESIAN_POINT ( 'NONE',  ( -3.314994193297896796, 6.393354490853021765, -0.7784788408506218005 ) ) ;
#187501 = CARTESIAN_POINT ( 'NONE',  ( -3.419936744200066325, -0.02828022925090156736, -0.3125692937056851473 ) ) ;
#187502 = VECTOR ( 'NONE', #63846, 1000.000000000000114 ) ;
#187503 = CARTESIAN_POINT ( 'NONE',  ( -7.806953216197586087, -6.479141885268315804, -7.749822179018686974 ) ) ;
#187504 = ORIENTED_EDGE ( 'NONE', *, *, #95474, .T. ) ;
#187505 = CARTESIAN_POINT ( 'NONE',  ( 3.033707436314789785, 1.966763487489433970, -0.6469820378900912328 ) ) ;
#187506 = CARTESIAN_POINT ( 'NONE',  ( 1.499999999999990896, 4.525000000000021672, 1.214306433183764966E-14 ) ) ;
#187507 = CARTESIAN_POINT ( 'NONE',  ( 3.635557746758808495, 7.393234471193928847, -0.7998128361456291469 ) ) ;
#187508 = CARTESIAN_POINT ( 'NONE',  ( -5.873358954868365345, 7.276917811852929852, 1.275545277584020365 ) ) ;
#187509 = CARTESIAN_POINT ( 'NONE',  ( 1.453777360798803819, -1.464386276593489189, -1.391179603160071387 ) ) ;
#187510 = CARTESIAN_POINT ( 'NONE',  ( -1.201851678989727383E-14, 3.946875000341423689, -1.575800808251660134 ) ) ;
#187511 = VERTEX_POINT ( 'NONE', #131352 ) ;
#187512 = EDGE_CURVE ( 'NONE', #31691, #182472, #98443, .T. ) ;
#187514 = CARTESIAN_POINT ( 'NONE',  ( 9.734391104931955141, 10.45913716528321125, 0.7216878364870438212 ) ) ;
#187513 = CARTESIAN_POINT ( 'NONE',  ( 0.07499057489264349119, 0.002531239327734773146, -1.955573237620360505 ) ) ;
#187515 = CARTESIAN_POINT ( 'NONE',  ( 4.973982425466109802, 1.752763018817087293, 0.9961474888594208377 ) ) ;
#187516 = CARTESIAN_POINT ( 'NONE',  ( 5.471877088563796399, -0.8550440501978623375, 1.714365851762880144 ) ) ;
#187517 = CARTESIAN_POINT ( 'NONE',  ( 6.539320575229256249, 7.052319431262985105, 2.701414634427783845 ) ) ;
#187518 = CARTESIAN_POINT ( 'NONE',  ( 3.404031855413204966, -0.8899279105200922357, -2.002928011436304612 ) ) ;
#187519 = CARTESIAN_POINT ( 'NONE',  ( -1.500000000000013101, 1.910416667349488451, -0.8660254037844313801 ) ) ;
#187520 = CARTESIAN_POINT ( 'NONE',  ( 2.285291272251275707, 0.09004542135446562401, -1.910373438827176251 ) ) ;
#187521 = CARTESIAN_POINT ( 'NONE',  ( -5.799137018343247796, 7.788745826199009237, -1.599625672291256295 ) ) ;
#187522 = CARTESIAN_POINT ( 'NONE',  ( 4.650083499362867911, 6.448183387388563226, 1.443375672974062551 ) ) ;
#187523 = CARTESIAN_POINT ( 'NONE',  ( 0.7027501817156033281, 1.864177386631181044, 0.7691025790682111118 ) ) ;
#187524 = CARTESIAN_POINT ( 'NONE',  ( 0.6823417656249934904, 11.00520833367472839, 1.181850606188764807 ) ) ;
#187526 = CARTESIAN_POINT ( 'NONE',  ( -5.271087860662956537, 9.371629280740593870, 0.000000000000000000 ) ) ;
#187525 = CARTESIAN_POINT ( 'NONE',  ( 6.075747529084263299, -1.173811750163206158, 1.850510016281024850 ) ) ;
#187528 = ORIENTED_EDGE ( 'NONE', *, *, #38982, .T. ) ;
#187527 = CARTESIAN_POINT ( 'NONE',  ( 3.082691909922595563, -0.1251556739016151387, -1.720276473149193297 ) ) ;
#187529 = FILL_AREA_STYLE ('',( #151852 ) ) ;
#187530 = CARTESIAN_POINT ( 'NONE',  ( 6.286176778230493589, 10.48562334124426698, 0.7998128361456462443 ) ) ;
#187531 = CARTESIAN_POINT ( 'NONE',  ( 5.009901455449552010, 5.803638771901306725, -1.199719254218452047 ) ) ;
#187532 = FACE_OUTER_BOUND ( 'NONE', #102536, .T. ) ;
#187533 = CARTESIAN_POINT ( 'NONE',  ( 0.4144086874100678664, 0.7473079093508437909, 1.814158889769983185 ) ) ;
#187534 = EDGE_CURVE ( 'NONE', #111607, #103797, #74476, .T. ) ;
#187535 = CARTESIAN_POINT ( 'NONE',  ( 7.334597915313080918, 9.580116872663850813, 1.040834085586084257E-14 ) ) ;
#187536 = CARTESIAN_POINT ( 'NONE',  ( 4.808338034340912337, 8.761478140039733020, 1.040834085586084257E-14 ) ) ;
#187537 = DIRECTION ( 'NONE',  ( -1.000000000000000000, 8.673617379884035472E-16, 0.000000000000000000 ) ) ;
#187538 = ORIENTED_EDGE ( 'NONE', *, *, #14569, .F. ) ;
#187539 = EDGE_LOOP ( 'NONE', ( #186652, #33466, #83141, #174267 ) ) ;
#187540 = CARTESIAN_POINT ( 'NONE',  ( 3.756361958294622383, 1.803085962505234008, 0.1738922897399265421 ) ) ;
#187541 = ORIENTED_EDGE ( 'NONE', *, *, #127328, .F. ) ;
#187542 = CARTESIAN_POINT ( 'NONE',  ( 10.05067194643221207, 10.62020544712608938, 0.7998128361456462443 ) ) ;
#187543 = CARTESIAN_POINT ( 'NONE',  ( 3.250922972226694352, 7.014770244231638863, 0.7998128361456281477 ) ) ;
#187544 = CARTESIAN_POINT ( 'NONE',  ( 4.424329001689049079, -0.7786147893445326540, -1.635752125832173220 ) ) ;
#187545 = CARTESIAN_POINT ( 'NONE',  ( 6.278834536460164983, 9.379038488295265097, -1.082531754730548412 ) ) ;
#187546 = CARTESIAN_POINT ( 'NONE',  ( 11.01135777277262306, 13.40000000000000036, -1.400000000000001910 ) ) ;
#187547 = CARTESIAN_POINT ( 'NONE',  ( 5.463439706979909438, 6.248932391672394893, 1.002290858133829010 ) ) ;
#187549 = CARTESIAN_POINT ( 'NONE',  ( -1.364683531250014514, 14.58854166700806232, -0.7879004041258335089 ) ) ;
#187548 = CARTESIAN_POINT ( 'NONE',  ( 4.932013296703669170, 1.071099452130529039, 1.521725064211083112 ) ) ;
#187550 = CARTESIAN_POINT ( 'NONE',  ( 2.864735742032016752, -0.1435939464786405995, -1.910298799178041351 ) ) ;
#187551 = CARTESIAN_POINT ( 'NONE',  ( 4.734293507696039960, 8.204026701335402905, 0.7038455069194777813 ) ) ;
#187552 = CARTESIAN_POINT ( 'NONE',  ( -10.50660484223216606, 5.359830900411396648, 5.105327592218940502 ) ) ;
#187553 = CARTESIAN_POINT ( 'NONE',  ( -0.7499999999999972244, 5.639583334016151639, -1.299038105676652899 ) ) ;
#187554 = CARTESIAN_POINT ( 'NONE',  ( 6.471393748265540147, 5.229711127717882491, 2.420000000000010587 ) ) ;
#187555 = CARTESIAN_POINT ( 'NONE',  ( 6.805829924380108586, 8.963220883242035697, 1.443375672974076540 ) ) ;
#187556 = EDGE_CURVE ( 'NONE', #117552, #183165, #52330, .T. ) ;
#187557 = CARTESIAN_POINT ( 'NONE',  ( -4.925689880466507908, 4.641059703499347044, -0.7998128361456221525 ) ) ;
#187558 = CARTESIAN_POINT ( 'NONE',  ( -1.416652131158606664, 8.000043606524071649, 10.86080395187257608 ) ) ;
#187559 = CARTESIAN_POINT ( 'NONE',  ( 1.798888674052185888, 1.738860765912113138, 1.160333176109765274 ) ) ;
#187560 = CARTESIAN_POINT ( 'NONE',  ( 5.123001941117305336, 7.070197912760590064, 1.599625672291268286 ) ) ;
#187561 = CARTESIAN_POINT ( 'NONE',  ( 6.475613818078473471, 1.843275991838376981, -0.5597920731088936730 ) ) ;
#187562 = CARTESIAN_POINT ( 'NONE',  ( -5.687809136132860210, 6.594531066031826150, -1.199719254218446718 ) ) ;
#187563 = EDGE_CURVE ( 'NONE', #156117, #52075, #40314, .T. ) ;
#187564 = CARTESIAN_POINT ( 'NONE',  ( 2.537895388257872753, 0.8626947210231518115, -1.608888323311054691 ) ) ;
#187565 = CARTESIAN_POINT ( 'NONE',  ( 11.15656239214823664, 9.703780284206802165, -5.826040129427457970 ) ) ;
#187566 = CARTESIAN_POINT ( 'NONE',  ( 1.346085547170269070, -0.8884179423524626307, 1.757888261374307870 ) ) ;
#187567 = CARTESIAN_POINT ( 'NONE',  ( 4.106929586529986409, -0.3288250506029398168, 1.913867117139455676 ) ) ;
#187568 = ORIENTED_EDGE ( 'NONE', *, *, #79933, .F. ) ;
#187569 = DIRECTION ( 'NONE',  ( -0.7408284471490506062, -1.804614770759877281E-12, 0.6716942845482062330 ) ) ;
#187571 = CARTESIAN_POINT ( 'NONE',  ( 6.280112003059028503, -1.032894792506684034, -1.547752956576850858 ) ) ;
#187570 = CARTESIAN_POINT ( 'NONE',  ( -4.980641328173854632, 6.904110530993182948, 1.599625672291263179 ) ) ;
#187573 = CARTESIAN_POINT ( 'NONE',  ( 4.219064148821600746, 1.637239594409030330, -1.347683705884415106 ) ) ;
#187572 = CARTESIAN_POINT ( 'NONE',  ( 7.842465510862060896, 8.114240948952696542, 0.000000000000000000 ) ) ;
#187574 = CARTESIAN_POINT ( 'NONE',  ( 6.594971855056625643, -6.631671885544809797, 6.818239715405312040 ) ) ;
#187575 = CARTESIAN_POINT ( 'NONE',  ( 8.075853055234393452, 12.57357899774884658, 0.7998128361456462443 ) ) ;
#187576 = CARTESIAN_POINT ( 'NONE',  ( -7.110325215724114578, 7.260077271291732082, 0.000000000000000000 ) ) ;
#187577 = CYLINDRICAL_SURFACE ( 'NONE', #166982, 0.5000000000000000000 ) ;
#187578 = CARTESIAN_POINT ( 'NONE',  ( 5.956828388357757298, 8.042995434541133193, 1.599625672291269396 ) ) ;
#187579 = CARTESIAN_POINT ( 'NONE',  ( 11.94980361058169116, 12.70000000000000107, -1.099999999999998535 ) ) ;
#187580 = CARTESIAN_POINT ( 'NONE',  ( 4.107882937833263526, -1.820653182827164596, 0.1363937739093170898 ) ) ;
#187581 = CARTESIAN_POINT ( 'NONE',  ( 5.314433026432511475, 5.302519407033794430, 1.040834085586084257E-14 ) ) ;
#187582 = CARTESIAN_POINT ( 'NONE',  ( -8.785320351975364872, 12.23299559640450518, 1.082531754730560403 ) ) ;
#187583 = CIRCLE ( 'NONE', #56170, 0.8300000000000008482 ) ;
#187584 = CARTESIAN_POINT ( 'NONE',  ( -5.137161949866410282, 7.898551110135567654, 1.241398918778359173 ) ) ;
#187585 = DIRECTION ( 'NONE',  ( 0.000000000000000000, -1.000000000000000000, 0.000000000000000000 ) ) ;
#187586 = CARTESIAN_POINT ( 'NONE',  ( 4.276139911362797363, -1.077190196239918851, 1.529178877381555335 ) ) ;
#187587 = CARTESIAN_POINT ( 'NONE',  ( 8.535021395002688749, 9.916278701380017324, 1.199719254218462483 ) ) ;
#187588 = STYLED_ITEM ( 'NONE', ( #142236 ), #51527 ) ;
#187589 = CARTESIAN_POINT ( 'NONE',  ( 1.980962579895541920, -0.09440724433935901438, -1.924309447538669060 ) ) ;
#187590 = CARTESIAN_POINT ( 'NONE',  ( 6.895372015613538963, -1.753720159772365284, 0.8792710811909019153 ) ) ;
#187591 = CARTESIAN_POINT ( 'NONE',  ( -0.6823417656250003738, 8.463541667008064096, 1.181850606188754593 ) ) ;
#187592 = CARTESIAN_POINT ( 'NONE',  ( -7.562750758324527922, 7.717630727667075696, 1.040834085586084257E-14 ) ) ;
#187593 = CARTESIAN_POINT ( 'NONE',  ( 3.337278367258157630, 7.045241861776501580, 0.7998128361456341429 ) ) ;
#187594 = CARTESIAN_POINT ( 'NONE',  ( -5.451787166026575981, 5.533042246551999277, 0.000000000000000000 ) ) ;
#187595 = CARTESIAN_POINT ( 'NONE',  ( 1.318125747981816698, 1.040119728068724880, -1.844044674895953806 ) ) ;
#187596 = CARTESIAN_POINT ( 'NONE',  ( 10.22692794340986921, 10.82583744360002243, 0.000000000000000000 ) ) ;
#187597 = CARTESIAN_POINT ( 'NONE',  ( -1.500085555261173376, 4.450186320795536332, -0.08157497973213596876 ) ) ;
#187598 = CARTESIAN_POINT ( 'NONE',  ( 4.768459183169745152, -0.8803848081004579385, -1.873848736155204087 ) ) ;
#187600 = CARTESIAN_POINT ( 'NONE',  ( 1.364683531249990311, 2.696875000341415696, 1.214306433183764966E-14 ) ) ;
#187599 = CARTESIAN_POINT ( 'NONE',  ( 0.7668492355173107677, 1.774547462407764842, -0.4907661837717376407 ) ) ;
#187601 = CARTESIAN_POINT ( 'NONE',  ( 5.168667805954368255, 1.541955118739355424, 1.704926945024546336 ) ) ;
#187602 = CARTESIAN_POINT ( 'NONE',  ( 7.307481608085759639, 7.627742752295940676, 1.040834085586084257E-14 ) ) ;
#187604 = CARTESIAN_POINT ( 'NONE',  ( -1.201851678989727383E-14, 4.618750000682821266, -1.732050807568863648 ) ) ;
#187603 = CARTESIAN_POINT ( 'NONE',  ( 4.760321332173959696, 4.726332107057286791, 0.000000000000000000 ) ) ;
#187605 = CARTESIAN_POINT ( 'NONE',  ( 1.148812421071528256, -1.804313360470580108, 1.413740901141118611 ) ) ;
#187606 = CARTESIAN_POINT ( 'NONE',  ( 5.017088295346122884, 4.896660802193717466, 0.1179097395585339686 ) ) ;
#187607 = CARTESIAN_POINT ( 'NONE',  ( -5.966470118465691641, 9.118576350588734059, -1.199719254218452047 ) ) ;
#187608 = CARTESIAN_POINT ( 'NONE',  ( 4.751864635371732426, 0.7446896046985322926, 1.793680106537680174 ) ) ;
#187609 = ORIENTED_EDGE ( 'NONE', *, *, #208563, .T. ) ;
#187610 = CARTESIAN_POINT ( 'NONE',  ( 8.609064354553323639, 10.10662517080946543, -1.082531754730543083 ) ) ;
#187611 = VERTEX_POINT ( 'NONE', #186422 ) ;
#187612 = CARTESIAN_POINT ( 'NONE',  ( 0.01783784634934187929, -0.5327901187049766119, 1.941387642157591742 ) ) ;
#187613 = CARTESIAN_POINT ( 'NONE',  ( 6.175017591530616023, 1.752142144017948100, -0.9981200475188132248 ) ) ;
#187615 = CARTESIAN_POINT ( 'NONE',  ( -4.517335436343488553, 8.499999999999996447, 0.7749999999999996891 ) ) ;
#187614 = CARTESIAN_POINT ( 'NONE',  ( -8.154339323615371171, 11.60081407993821045, 1.199719254218453823 ) ) ;
#187616 = CARTESIAN_POINT ( 'NONE',  ( 1.642778471875000035, -2.413541666188709911, -2.845375778867859751 ) ) ;
#187618 = CARTESIAN_POINT ( 'NONE',  ( 0.8304726968981954727, 0.1242609525908405232, 1.765545458023538572 ) ) ;
#187617 = CARTESIAN_POINT ( 'NONE',  ( 2.818400364232038768, 1.968743758771305918, 0.7038092692753412649 ) ) ;
#187619 = CARTESIAN_POINT ( 'NONE',  ( -0.1588445005388229581, -6.630981418884854151, -9.484513308955760280 ) ) ;
#187621 = CARTESIAN_POINT ( 'NONE',  ( 4.541174964560028116, -1.770302748489580358, -1.456204954804733998 ) ) ;
#187620 = FACE_OUTER_BOUND ( 'NONE', #159446, .T. ) ;
#187622 = CARTESIAN_POINT ( 'NONE',  ( 2.360927591450364904, 1.706848764895356085, -0.3387292939842252437 ) ) ;
#187623 = CARTESIAN_POINT ( 'NONE',  ( 2.869522067586683711, 6.499526178826442013, 0.7998128361456362523 ) ) ;
#187624 = VECTOR ( 'NONE', #101231, 1000.000000000000000 ) ;
#187625 = CARTESIAN_POINT ( 'NONE',  ( 6.062430963966053632, 7.101866208495718702, -1.199719254218452047 ) ) ;
#187626 = CARTESIAN_POINT ( 'NONE',  ( 2.125947893326819660, 0.3012468308378027371, -1.707275946889510676 ) ) ;
#187627 = CARTESIAN_POINT ( 'NONE',  ( 1.360316468749955598, 1.526041667008097180, 0.7853790794158861388 ) ) ;
#187628 = CARTESIAN_POINT ( 'NONE',  ( 2.014367633873125563, 2.165423841567072127, -0.1585431616079237827 ) ) ;
#187629 = CARTESIAN_POINT ( 'NONE',  ( 5.823390672269506574, 6.752709524857930745, -1.199719254218446718 ) ) ;
#187630 = CARTESIAN_POINT ( 'NONE',  ( 4.417204035549080920, -1.841734835922325120, 0.8216704330437707426 ) ) ;
#187631 = CARTESIAN_POINT ( 'NONE',  ( 3.250000000000002665, 1.855058607017213327E-13, 2.052068128417948056 ) ) ;
#187632 = CARTESIAN_POINT ( 'NONE',  ( -0.7500000000000215383, 2.972916667349487341, 1.299038105676671107 ) ) ;
#187633 = CARTESIAN_POINT ( 'NONE',  ( 1.272347295514785870, -1.224129819625971782, 1.487435282370595857 ) ) ;
#187634 = CARTESIAN_POINT ( 'NONE',  ( -1.402160292154681736E-14, 14.17187500034139624, 1.575800808251682339 ) ) ;
#187635 = CARTESIAN_POINT ( 'NONE',  ( 4.078556047614148028, 1.049247773278503049, 1.958029639119197585 ) ) ;
#187636 = ORIENTED_EDGE ( 'NONE', *, *, #55665, .T. ) ;
#187637 = CARTESIAN_POINT ( 'NONE',  ( -0.1106856583841242386, 6.948332279000682732, -2.591999772403537516 ) ) ;
#187638 = CARTESIAN_POINT ( 'NONE',  ( -0.7500000000000249800, -0.05833333333331303105, 1.299038105676659116 ) ) ;
#187639 = CARTESIAN_POINT ( 'NONE',  ( 6.089583550832340819, 10.25626457594641749, 1.040834085586084257E-14 ) ) ;
#187640 = CARTESIAN_POINT ( 'NONE',  ( -3.285556943750000070, -1.509374999522042238, 0.000000000000000000 ) ) ;
#187641 = CARTESIAN_POINT ( 'NONE',  ( 0.3115808214643934204, 1.843292235811417878, -1.239274738845694390 ) ) ;
#187642 = CARTESIAN_POINT ( 'NONE',  ( 5.336364984333265227, -1.091323163865608459, 1.630109012322231266 ) ) ;
#187643 = CARTESIAN_POINT ( 'NONE',  ( 9.897088948295946764, 10.64895131587453569, 0.7216878364870438212 ) ) ;
#187644 = CARTESIAN_POINT ( 'NONE',  ( -1.315349297999210076, 4.153791881628437821, -0.4023297572127273458 ) ) ;
#187645 = CARTESIAN_POINT ( 'NONE',  ( 0.4390364970160881564, 0.3691015439823107092, 2.129678967336546602 ) ) ;
#187646 = VECTOR ( 'NONE', #49677, 1000.000000000000000 ) ;
#187648 = AXIS2_PLACEMENT_3D ( 'NONE', #93069, #156998, #174321 ) ;
#187647 = CARTESIAN_POINT ( 'NONE',  ( -4.882344714696960075, 5.829061934302122161, 1.082531754730549078 ) ) ;
#187649 = CARTESIAN_POINT ( 'NONE',  ( 3.754389245258652252, -2.060177385294372776, -0.1042076536686628307 ) ) ;
#187650 = CARTESIAN_POINT ( 'NONE',  ( -5.422371370461663176, 8.413518134592214537, -1.199719254218446718 ) ) ;
#187651 = CARTESIAN_POINT ( 'NONE',  ( -1.500000000000013101, 2.910416667349485120, -0.8660254037844313801 ) ) ;
#187652 = CARTESIAN_POINT ( 'NONE',  ( -1.364683531250010295, 5.092708333674757171, 0.7879004041258379498 ) ) ;
#187653 = CARTESIAN_POINT ( 'NONE',  ( 5.044154037833219029, 1.865456107639616556, 0.1390639465682907416 ) ) ;
#187654 = CARTESIAN_POINT ( 'NONE',  ( 3.885211248783075888, -0.5490618756427265712, -1.644986201639383028 ) ) ;
#187655 = CARTESIAN_POINT ( 'NONE',  ( 2.946521060880839205, -1.424341091986385921, -0.9998927444686573907 ) ) ;
#187656 = CARTESIAN_POINT ( 'NONE',  ( 0.3458147113889240565, 0.7113776200376471515, -2.179290858394256070 ) ) ;
#187657 = CARTESIAN_POINT ( 'NONE',  ( -1.364683531250012516, 3.801041667008087099, -0.7879004041258300672 ) ) ;
#187658 = CARTESIAN_POINT ( 'NONE',  ( 5.073812392315714348, -1.160337598488449196, 1.738990438290926921 ) ) ;
#187659 = CARTESIAN_POINT ( 'NONE',  ( 6.351511478899689145, 1.936555568076937295, -0.1455203235936879114 ) ) ;
#187660 = LINE ( 'NONE', #101076, #42816 ) ;
#187661 = CARTESIAN_POINT ( 'NONE',  ( 1.055314813143366726, -1.277040974352643854, 1.560502084637045650 ) ) ;
#187662 = CARTESIAN_POINT ( 'NONE',  ( 0.6684183810189650021, 2.117893379942568988, -0.1100008709709817956 ) ) ;
#187663 = CARTESIAN_POINT ( 'NONE',  ( 6.328750030911493241, 0.7691242348151774433, -1.864167186630163009 ) ) ;
#187664 = CARTESIAN_POINT ( 'NONE',  ( -8.636707547105197946, 10.03491254549959777, -1.199719254218446718 ) ) ;
#187665 = CARTESIAN_POINT ( 'NONE',  ( 4.794779880727245036, 8.745660294157122649, -0.7998128361456281477 ) ) ;
#187666 = CARTESIAN_POINT ( 'NONE',  ( 2.069135417989849568, -1.637292086295978111, 1.347470637625711731 ) ) ;
#187667 = CARTESIAN_POINT ( 'NONE',  ( 0.7662865668233912464, -4.140281660848650347, -0.6727527331043390291 ) ) ;
#187668 = CARTESIAN_POINT ( 'NONE',  ( 4.898959864523320107, 1.516061528642864253, -1.016892643307308441 ) ) ;
#187669 = EDGE_LOOP ( 'NONE', ( #199404, #840, #102211, #174708 ) ) ;
#187670 = CARTESIAN_POINT ( 'NONE',  ( -3.133342898089680695, 6.669667457830990465, 0.7216878364870338292 ) ) ;
#187671 = CARTESIAN_POINT ( 'NONE',  ( 0.01181297548617449289, -7.619382996155831478, -9.500232605409566489 ) ) ;
#187672 = CARTESIAN_POINT ( 'NONE',  ( 3.285556943750000070, -0.7218749995220423710, 0.000000000000000000 ) ) ;
#187673 = CARTESIAN_POINT ( 'NONE',  ( -7.718669524881690336, 7.899535955317097624, 0.7998128361456462443 ) ) ;
#187674 = CARTESIAN_POINT ( 'NONE',  ( 2.672133692126318127, 2.009681031688851593, -0.2020390005853574256 ) ) ;
#187675 = CARTESIAN_POINT ( 'NONE',  ( 5.825267882404531861, -0.05969703229705652925, 2.206138628428089277 ) ) ;
#187677 = EDGE_CURVE ( 'NONE', #179385, #51705, #153789, .T. ) ;
#187676 = CIRCLE ( 'NONE', #869, 10.86343145750506878 ) ;
#187678 = CARTESIAN_POINT ( 'NONE',  ( -4.309512724297390740, 6.121127159803966933, 1.599625672291270506 ) ) ;
#187679 = CARTESIAN_POINT ( 'NONE',  ( 3.397144026274971029, -1.643366908016094641, 0.8731178804023755902 ) ) ;
#187680 = CARTESIAN_POINT ( 'NONE',  ( 3.891353782322113375, 4.498666486585943147, -1.199719254218446718 ) ) ;
#187681 = CARTESIAN_POINT ( 'NONE',  ( 1.673491136019439323E-15, 15.00041888085534758, 11.67999951260719982 ) ) ;
#187682 = ORIENTED_EDGE ( 'NONE', *, *, #56195, .T. ) ;
#187683 = CARTESIAN_POINT ( 'NONE',  ( -3.405069135326500351, 7.124331091189553433, 1.040834085586084257E-14 ) ) ;
#187684 = CARTESIAN_POINT ( 'NONE',  ( -8.727698198895085469, 11.20540053684285553, -1.599625672291263179 ) ) ;
#187685 = CARTESIAN_POINT ( 'NONE',  ( 5.285714101943871590, 1.228958891529348785, 1.350286652578087665 ) ) ;
#187687 = CARTESIAN_POINT ( 'NONE',  ( -4.695925055628692668, 7.055611427533158064, -1.405632220554285272 ) ) ;
#187686 = CARTESIAN_POINT ( 'NONE',  ( -5.503684012504701961, 5.385662534202396934, 0.000000000000000000 ) ) ;
#187688 = CARTESIAN_POINT ( 'NONE',  ( 1.364683531249986537, -0.6364583329919177856, 0.7879004041258500513 ) ) ;
#187689 = CARTESIAN_POINT ( 'NONE',  ( 6.854846703925610463, -0.8643618726141141240, 1.819651424301058640 ) ) ;
#187690 = CARTESIAN_POINT ( 'NONE',  ( -0.02397475188680147154, -0.1303385410800334265, -1.711279094490937069 ) ) ;
#187691 = CARTESIAN_POINT ( 'NONE',  ( 5.461655971716653291, 0.4551397948197592469, -2.262217722918384410 ) ) ;
#187692 = CARTESIAN_POINT ( 'NONE',  ( 3.542423274920540432, 7.354853930707762721, -1.734723475976807094E-15 ) ) ;
#187693 = CARTESIAN_POINT ( 'NONE',  ( 6.591117433763723277, 1.884315261875910474, -1.059023293578951863 ) ) ;
#187694 = CARTESIAN_POINT ( 'NONE',  ( 4.971035877704902184, 8.951292290631053916, 1.040834085586084257E-14 ) ) ;
#187695 = ADVANCED_FACE ( 'NONE', ( #52175 ), #190845, .T. ) ;
#187696 = EDGE_CURVE ( 'NONE', #195818, #10241, #99761, .T. ) ;
#187697 = CARTESIAN_POINT ( 'NONE',  ( 6.151801744867631427, -0.3282927394851458125, -2.274731023314037870 ) ) ;
#187698 = DIRECTION ( 'NONE',  ( 0.9998476951563912696, -0.000000000000000000, -0.01745240643728004568 ) ) ;
#187699 = CARTESIAN_POINT ( 'NONE',  ( -5.264308783856126439, 9.363720357799287797, -0.7998128361456362523 ) ) ;
#187700 = CARTESIAN_POINT ( 'NONE',  ( 6.139502064137229986, -1.356240498024411600, -1.288626068300227523 ) ) ;
#187702 = CARTESIAN_POINT ( 'NONE',  ( -3.474632506852224356, 7.275764701294714420, -0.7998128361456481317 ) ) ;
#187701 = CARTESIAN_POINT ( 'NONE',  ( 3.533378866418676711, -0.1359047358975660202, 1.907598245988059826 ) ) ;
#187703 = CARTESIAN_POINT ( 'NONE',  ( 5.250674450588199704, 0.6379336648693231249, 2.112661011922472021 ) ) ;
#187704 = CARTESIAN_POINT ( 'NONE',  ( 4.803976500543080341, -1.135498674831243227, -1.786957999583696610 ) ) ;
#187705 = CARTESIAN_POINT ( 'NONE',  ( -0.6125000000000123679, 1.770833334016133520, -1.060881119635941339 ) ) ;
#187706 = CARTESIAN_POINT ( 'NONE',  ( 6.983263157960372780, 1.247263239625576059, 2.158450195331083510 ) ) ;
#187707 = CARTESIAN_POINT ( 'NONE',  ( 3.079110283634975964, 6.606396074300548982, 0.7216878364870257245 ) ) ;
#187708 = CARTESIAN_POINT ( 'NONE',  ( -5.655159470231558849, 6.730679149092498648, 1.082531754730549078 ) ) ;
#187709 = CARTESIAN_POINT ( 'NONE',  ( 5.619825546450978315, -0.5151785252428126016, 2.056841324599982368 ) ) ;
#187710 = CARTESIAN_POINT ( 'NONE',  ( 2.661487998672926292, -2.007448288467659214, -1.137923995292255741 ) ) ;
#187711 = CARTESIAN_POINT ( 'NONE',  ( 3.736726379466179804, -1.890069333072645241, -0.5255722985574098338 ) ) ;
#187712 = CARTESIAN_POINT ( 'NONE',  ( -5.971440312176176768, 5.931378217152456500, 0.000000000000000000 ) ) ;
#187713 = CARTESIAN_POINT ( 'NONE',  ( 0.2390249890181182224, -0.1369461163322066299, -1.930431041017650395 ) ) ;
#187714 = CARTESIAN_POINT ( 'NONE',  ( 7.854620613934385709, 15.31793777779468968, 9.015191429226655728 ) ) ;
#187715 = CARTESIAN_POINT ( 'NONE',  ( 4.390861645979372341, 6.216034235099629157, -1.599625672291269396 ) ) ;
#187716 = VERTEX_POINT ( 'NONE', #37569 ) ;
#187717 = CARTESIAN_POINT ( 'NONE',  ( 5.612517632836664383, 1.944729323200470095, 0.5331731267440716904 ) ) ;
#187718 = CARTESIAN_POINT ( 'NONE',  ( -7.960608749518247151, 12.43912730774665576, 0.000000000000000000 ) ) ;
#187719 = CARTESIAN_POINT ( 'NONE',  ( 0.09336763325077861164, -1.840659761701424646, -0.04852334659839750014 ) ) ;
#187720 = CARTESIAN_POINT ( 'NONE',  ( 2.969727409235598969, 6.579374545918310169, -0.3541450170054856184 ) ) ;
#187721 = CARTESIAN_POINT ( 'NONE',  ( 3.625983508040203862, 2.119313185944927902, -0.4706255054970372997 ) ) ;
#187722 = CARTESIAN_POINT ( 'NONE',  ( 6.066347387471824781, 6.042103138330730872, -0.7998128361456481317 ) ) ;
#187723 = CARTESIAN_POINT ( 'NONE',  ( 0.8441712343106638761, -1.349783269286155774, -1.635521010841307410 ) ) ;
#187724 = CARTESIAN_POINT ( 'NONE',  ( 0.7499999999999885647, 1.847916667349486231, -1.299038105676652899 ) ) ;
#187725 = CARTESIAN_POINT ( 'NONE',  ( -0.8988756482332411757, 14.48154074969179739, -11.99999999996309974 ) ) ;
#187726 = CARTESIAN_POINT ( 'NONE',  ( 5.703612580814390043, 7.410739916031705121, 1.319003781635886163 ) ) ;
#187727 = CARTESIAN_POINT ( 'NONE',  ( 0.8607048193125128588, -1.494471031236654257, 1.419199468611084480 ) ) ;
#187729 = CARTESIAN_POINT ( 'NONE',  ( 4.337593226613512876, 3.996631841756838277, -0.04457646079592735011 ) ) ;
#187728 = CARTESIAN_POINT ( 'NONE',  ( -8.455481356417053007, 13.01647868246193518, 0.7998128361456341429 ) ) ;
#187730 = CARTESIAN_POINT ( 'NONE',  ( -1.364683531250014514, 1.238541667008091096, -0.7879004041258289570 ) ) ;
#187731 =( BOUNDED_CURVE ( )  B_SPLINE_CURVE ( 2, ( #76617, #176272, #204460, #9489, #157896, #11612, #107051, #8413, #188229 ),
 .UNSPECIFIED., .F., .T. ) 
 B_SPLINE_CURVE_WITH_KNOTS ( ( 3, 2, 2, 2, 3 ),
 ( 0.3660714285714286031, 0.3690476190476190688, 0.3750000000000000000, 0.3809523809523809312, 0.3839285714285713969 ),
 .UNSPECIFIED. ) 
 CURVE ( )  GEOMETRIC_REPRESENTATION_ITEM ( )  RATIONAL_B_SPLINE_CURVE ( ( 0.9330127018922194093, 0.9330127018922199644, 1.000000000000000000, 0.8660254037844387076, 1.000000000000000000, 0.8660254037844387076, 1.000000000000000000, 0.9330127018922199644, 0.9330127018922194093 ) ) 
 REPRESENTATION_ITEM ( '' )  );
#187732 = EDGE_LOOP ( 'NONE', ( #110849, #78244, #65371, #188686 ) ) ;
#187733 = CARTESIAN_POINT ( 'NONE',  ( 3.070860992347378637, -1.446505282863861375, 1.250851760459831041 ) ) ;
#187734 = VECTOR ( 'NONE', #56178, 1000.000000000000000 ) ;
#187735 = B_SPLINE_CURVE_WITH_KNOTS ( 'NONE', 3,
 ( #184620, #84999, #168389, #70854, #19985, #136968 ),
 .UNSPECIFIED., .F., .F.,
 ( 4, 2, 4 ),
 ( 1.226634733346699349E-18, 0.0009740587311750446408, 0.001948117462350088197 ),
 .UNSPECIFIED. ) ;
#187736 = CARTESIAN_POINT ( 'NONE',  ( 5.700005536890629720, -1.770032025875327042, 0.003423177859356376761 ) ) ;
#187737 = CARTESIAN_POINT ( 'NONE',  ( 6.444921918449731280, 8.612437886315108315, 1.599625672291268286 ) ) ;
#187738 = CARTESIAN_POINT ( 'NONE',  ( -5.739179097286464248, 5.590130456455974617, -0.7998128361456221525 ) ) ;
#187739 = CARTESIAN_POINT ( 'NONE',  ( 0.7557781591117664899, 0.7332364915693561080, -1.656728582389139781 ) ) ;
#187741 = CARTESIAN_POINT ( 'NONE',  ( 1.112342557844925750, 1.847186106069747646, 0.5076494344821417259 ) ) ;
#187740 = CARTESIAN_POINT ( 'NONE',  ( 5.899206235721897507, 6.055031161196562373, 0.000000000000000000 ) ) ;
#187742 = CARTESIAN_POINT ( 'NONE',  ( 1.768117254402020277, -2.054967671486531255, 0.2513356459030794410 ) ) ;
#187743 = CARTESIAN_POINT ( 'NONE',  ( -1.364683531250000748, 0.07187500034142035865, 0.000000000000000000 ) ) ;
#187744 = CARTESIAN_POINT ( 'NONE',  ( 6.332864056472936376, 0.1854757364097951722, 1.861418627818342664 ) ) ;
#187745 = CARTESIAN_POINT ( 'NONE',  ( 2.437895498511342574, 0.8609710149188254391, -1.609920059450341778 ) ) ;
#187747 = CARTESIAN_POINT ( 'NONE',  ( 6.326190869690321961, 6.855918622363850190, 0.6739092513716876676 ) ) ;
#187746 = CARTESIAN_POINT ( 'NONE',  ( 6.621690180768193379, -2.141820631849135292, 0.5315211216728524812 ) ) ;
#187748 = CARTESIAN_POINT ( 'NONE',  ( -0.6823417656250003738, 0.2177083336747515085, -1.181850606188749264 ) ) ;
#187749 = CARTESIAN_POINT ( 'NONE',  ( 3.684078386338876854, -1.226296459201616340, -1.658441301575198645 ) ) ;
#187750 = CARTESIAN_POINT ( 'NONE',  ( -6.527360889975461156, 9.702672574024962415, 1.199719254218452047 ) ) ;
#187751 = CARTESIAN_POINT ( 'NONE',  ( 8.971744963941056028, 11.49012176272984931, 1.599625672291281386 ) ) ;
#187752 = DIRECTION ( 'NONE',  ( 1.039099362110107450E-15, 1.000000000000000000, -4.583713267641621330E-32 ) ) ;
#187753 = CARTESIAN_POINT ( 'NONE',  ( 0.8784639925019832596, -1.201575844224999301, 1.796657101444131932 ) ) ;
#187754 = CARTESIAN_POINT ( 'NONE',  ( 6.320769956279724155, -1.466918727022302971, 1.461273828345016845 ) ) ;
#187755 = CARTESIAN_POINT ( 'NONE',  ( 1.364683531249988757, 0.9468750003414211358, 0.000000000000000000 ) ) ;
#187756 = CARTESIAN_POINT ( 'NONE',  ( 3.954491917119377753, 0.7739500986865335275, 2.018479124525011770 ) ) ;
#187757 = CARTESIAN_POINT ( 'NONE',  ( 4.406902263202909786, -0.4446603063312704607, -1.969940172527106625 ) ) ;
#187758 = CARTESIAN_POINT ( 'NONE',  ( 6.620655732516611103, 6.033324165176342291, 2.868629481857593255 ) ) ;
#187759 = EDGE_CURVE ( 'NONE', #44750, #12260, #204744, .T. ) ;
#187762 = CARTESIAN_POINT ( 'NONE',  ( 5.151735183512854199, 8.954182114166247430, -0.7216878364870257245 ) ) ;
#187761 = CARTESIAN_POINT ( 'NONE',  ( 2.960183410750786059, -4.109567543049581495, -1.425552035297093623 ) ) ;
#187760 = CARTESIAN_POINT ( 'NONE',  ( 0.3878679656440350287, 3.999999999999961808, -1.007084189318423473 ) ) ;
#187763 = CARTESIAN_POINT ( 'NONE',  ( -5.932574734431526942, 9.079031735882207244, 1.199719254218454489 ) ) ;
#187764 = CARTESIAN_POINT ( 'NONE',  ( 2.114470590943520634, 1.957170936680457052, 0.4852650170619755565 ) ) ;
#187765 = CARTESIAN_POINT ( 'NONE',  ( -8.199983978166823562, 8.461069484149769337, -0.7998128361456291469 ) ) ;
#187766 = CARTESIAN_POINT ( 'NONE',  ( -5.413783410558481002, 5.210502155273325720, -0.7998128361456221525 ) ) ;
#187767 = DIRECTION ( 'NONE',  ( 0.6507913734559641616, -0.7592566023653004592, 0.000000000000000000 ) ) ;
#187768 = CARTESIAN_POINT ( 'NONE',  ( 5.642805672956042962, 1.844803604357934779, 0.5037821151940986564 ) ) ;
#187769 = CARTESIAN_POINT ( 'NONE',  ( -1.123270288250315163, 3.047697346350006331, -0.7749999999993613109 ) ) ;
#187770 = CARTESIAN_POINT ( 'NONE',  ( 5.788968402910812827, 6.816513227226497662, 1.082531754730558626 ) ) ;
#187772 = CARTESIAN_POINT ( 'NONE',  ( 4.886342304379579282, -0.6820123065829878373, -1.897693145932321857 ) ) ;
#187771 = CARTESIAN_POINT ( 'NONE',  ( -7.985389288324697965, 10.33937347451072775, -1.443375672974058777 ) ) ;
#187773 = CARTESIAN_POINT ( 'NONE',  ( -0.7500000000000215383, 4.441666666666691299, 1.299038105676671107 ) ) ;
#187774 = CARTESIAN_POINT ( 'NONE',  ( -1.364683531250000748, 14.67187500034139447, 0.000000000000000000 ) ) ;
#187775 = CARTESIAN_POINT ( 'NONE',  ( 6.792093547228882144, -0.7321312287554645470, 1.560492760358098918 ) ) ;
#187776 = CARTESIAN_POINT ( 'NONE',  ( 5.091969210384201361, 8.098325291160362482, 1.199719254218452047 ) ) ;
#187777 = AXIS2_PLACEMENT_3D ( 'NONE', #119473, #185461, #85841 ) ;
#187778 = CARTESIAN_POINT ( 'NONE',  ( 7.592202833972727660, 11.80139437303613015, -0.7216878364870267237 ) ) ;
#187779 = CARTESIAN_POINT ( 'NONE',  ( -11.48243876534946040, 11.29999999999999893, -3.200000000000001510 ) ) ;
#187780 = CARTESIAN_POINT ( 'NONE',  ( 5.272658424858247095, -1.760895560629770262, -0.6313210838888929644 ) ) ;
#187781 = DIRECTION ( 'NONE',  ( -0.000000000000000000, -1.000000000000000000, -0.000000000000000000 ) ) ;
#187783 =( BOUNDED_CURVE ( )  B_SPLINE_CURVE ( 2, ( #14030, #198123, #49754, #130027, #147269, #80116, #115881 ),
 .UNSPECIFIED., .F., .T. ) 
 B_SPLINE_CURVE_WITH_KNOTS ( ( 3, 2, 2, 3 ),
 ( 0.4249999999999998224, 0.4333333333333331261, 0.4416666666666663743, 0.4499999999999996780 ),
 .UNSPECIFIED. ) 
 CURVE ( )  GEOMETRIC_REPRESENTATION_ITEM ( )  RATIONAL_B_SPLINE_CURVE ( ( 1.000000000000002665, 0.8660254037844360431, 1.000000000000000000, 0.8660254037844387076, 1.000000000000000000, 0.8660254037844440367, 0.9999999999999946709 ) ) 
 REPRESENTATION_ITEM ( '' )  );
#187782 = CARTESIAN_POINT ( 'NONE',  ( 1.938418878558012315, -1.110983660290700170, 1.746734030103759938 ) ) ;
#187784 = CARTESIAN_POINT ( 'NONE',  ( -6.224601922005509991, 10.27613631906616476, 0.7216878364870267237 ) ) ;
#187785 = ORIENTED_EDGE ( 'NONE', *, *, #72377, .T. ) ;
#187786 = CARTESIAN_POINT ( 'NONE',  ( 4.927462483923885195, 4.713404084191450849, -0.7998128361456481317 ) ) ;
#187787 = CARTESIAN_POINT ( 'NONE',  ( 0.6324356828835416833, 0.5880426346329314935, 1.928746166857209676 ) ) ;
#187788 = CARTESIAN_POINT ( 'NONE',  ( 1.458926887072587553, -1.529292093677349307, 0.9708203095366783053 ) ) ;
#187789 = CARTESIAN_POINT ( 'NONE',  ( 5.045042557616584489, 5.058506870073687267, 0.000000000000000000 ) ) ;
#187790 = CARTESIAN_POINT ( 'NONE',  ( 0.000000000000000000, 2.999999999999999112, 0.000000000000000000 ) ) ;
#187791 = CARTESIAN_POINT ( 'NONE',  ( 8.392133896734668141, 9.853539636687704828, 1.082531754730558626 ) ) ;
#187792 = CARTESIAN_POINT ( 'NONE',  ( 8.209625708274705502, 9.536650400197368427, 1.199719254218462483 ) ) ;
#187793 = AXIS2_PLACEMENT_3D ( 'NONE', #129487, #213804, #195469 ) ;
#187795 = CARTESIAN_POINT ( 'NONE',  ( 5.624599552000627334, 0.3785363404739845450, 1.877648607602548925 ) ) ;
#187794 = CARTESIAN_POINT ( 'NONE',  ( -5.368138756007025947, 8.350246751061767725, 1.199719254218452047 ) ) ;
#187796 = DIRECTION ( 'NONE',  ( 0.000000000000000000, 0.000000000000000000, -1.000000000000000000 ) ) ;
#187797 = DIRECTION ( 'NONE',  ( 0.000000000000000000, 1.000000000000000000, 0.000000000000000000 ) ) ;
#187798 = CARTESIAN_POINT ( 'NONE',  ( -10.98997987423604172, -6.893137084989842123, 0.4694063952341877011 ) ) ;
#187800 = ORIENTED_EDGE ( 'NONE', *, *, #200712, .F. ) ;
#187799 = CARTESIAN_POINT ( 'NONE',  ( 4.121315508874254796, 5.831287398485176077, -1.443375672974051449 ) ) ;
#187801 = ADVANCED_FACE ( 'NONE', ( #134042 ), #51701, .F. ) ;
#187802 = CARTESIAN_POINT ( 'NONE',  ( -6.371969008742801144, 10.37778824360119145, 0.7216878364870458196 ) ) ;
#187803 = CARTESIAN_POINT ( 'NONE',  ( 2.975616057669258741, 2.053088362031017855, -0.6768339029224537118 ) ) ;
#187804 = CARTESIAN_POINT ( 'NONE',  ( -7.431277594066160397, 7.842447745931541370, -0.7216878364870338292 ) ) ;
#187805 = CARTESIAN_POINT ( 'NONE',  ( 7.024532985656141371, 7.367912369453226695, 0.7216878364870328300 ) ) ;
#187806 = CARTESIAN_POINT ( 'NONE',  ( 1.125412309253082332, 1.872817075645373697, 0.9946839901537675166 ) ) ;
#187807 = EDGE_CURVE ( 'NONE', #64278, #76973, #19562, .T. ) ;
#187808 = CARTESIAN_POINT ( 'NONE',  ( 5.702125722003772879, -1.825762228975034596, 0.002264948092654816680 ) ) ;
#187809 = CIRCLE ( 'NONE', #66719, 2.650000000000000799 ) ;
#187810 = CARTESIAN_POINT ( 'NONE',  ( 1.862511354659317053, -1.396895987378836690, 1.391268958170795100 ) ) ;
#187811 = CARTESIAN_POINT ( 'NONE',  ( 4.078302138561982204, 0.9061299177482335931, 1.684124486321957104 ) ) ;
#187812 = CARTESIAN_POINT ( 'NONE',  ( -11.55950211276791073, 9.799999999999998934, -3.221476510067115662 ) ) ;
#187813 = CARTESIAN_POINT ( 'NONE',  ( 4.932068866601894364, 1.132370341068598796, 1.611282302955379553 ) ) ;
#187814 = CARTESIAN_POINT ( 'NONE',  ( 0.6912261618599843116, -0.6995774015170745930, 1.811736774657431548 ) ) ;
#187815 = ORIENTED_EDGE ( 'NONE', *, *, #102432, .T. ) ;
#187816 = CARTESIAN_POINT ( 'NONE',  ( -5.529746549527323474, 7.544733289238903851, -1.599625672291271394 ) ) ;
#187817 = CARTESIAN_POINT ( 'NONE',  ( -3.471769853551161411, 6.208092708188416076, 1.199719254218452935 ) ) ;
#187819 = CARTESIAN_POINT ( 'NONE',  ( 6.712695452097489301, 7.964471127936110229, -1.082531754730548412 ) ) ;
#187818 = CARTESIAN_POINT ( 'NONE',  ( 6.584456157731144899, 10.83361595066169514, -0.7998128361456291469 ) ) ;
#187821 = ORIENTED_EDGE ( 'NONE', *, *, #75342, .T. ) ;
#187820 = CARTESIAN_POINT ( 'NONE',  ( 5.303337639526568559, 1.684534858470821961, -0.9050978215178404618 ) ) ;
#187822 = AXIS2_PLACEMENT_3D ( 'NONE', #92350, #56618, #154120 ) ;
#187823 = CARTESIAN_POINT ( 'NONE',  ( 1.220068447022312652, -2.152735442661047216, 0.4846846590640523367 ) ) ;
#187824 = CARTESIAN_POINT ( 'NONE',  ( 9.333041836227131682, 4.446947634373626279, -7.472413793103381607 ) ) ;
#187825 = CARTESIAN_POINT ( 'NONE',  ( 5.760407631487725055, 2.010880845746499279, 0.09660876809274536459 ) ) ;
#187826 = CARTESIAN_POINT ( 'NONE',  ( 0.07680821025393863577, 5.725641208404781857, -2.404836704152548688 ) ) ;
#187827 = CARTESIAN_POINT ( 'NONE',  ( 11.04536101718726293, 12.69999999999999929, 1.099999999999996758 ) ) ;
#187828 = CARTESIAN_POINT ( 'NONE',  ( -2.298420387838187473, 5.509269730139584986, -0.7346435760097105305 ) ) ;
#187829 = CARTESIAN_POINT ( 'NONE',  ( 3.139188941651628539, -0.1496422021231707811, -2.064996656166856237 ) ) ;
#187830 = CARTESIAN_POINT ( 'NONE',  ( -6.063521013809733518, 8.097193820909906137, 1.599625672291283607 ) ) ;
#187831 = CARTESIAN_POINT ( 'NONE',  ( -4.945771867956824330, 7.989995641179508112, -1.012621479200847441 ) ) ;
#187833 = CARTESIAN_POINT ( 'NONE',  ( 0.7081719773709761467, -2.151164098719647200, 0.2130325561137471624 ) ) ;
#187832 = CARTESIAN_POINT ( 'NONE',  ( -4.205000198532790279, 8.057583998263570635, 0.7998128361456341429 ) ) ;
#187834 = CARTESIAN_POINT ( 'NONE',  ( -11.63182876714490632, 8.359486921846603025, 2.963400241755523634 ) ) ;
#187835 = CARTESIAN_POINT ( 'NONE',  ( 3.933273961740286317, 7.602920365423422311, 0.7216878364870257245 ) ) ;
#187836 = FACE_OUTER_BOUND ( 'NONE', #73946, .T. ) ;
#187837 = CARTESIAN_POINT ( 'NONE',  ( -8.012344526598182026E-15, 12.60937500034139802, -1.575800808251669460 ) ) ;
#187839 = CARTESIAN_POINT ( 'NONE',  ( -7.767895665986912057, 8.027242796598338614, -0.7998128361456362523 ) ) ;
#187838 = CARTESIAN_POINT ( 'NONE',  ( 6.925078400183547700, 0.5992389604297322370, 1.809181922849491198 ) ) ;
#187840 = CARTESIAN_POINT ( 'NONE',  ( 5.063005163341266268, -0.9570555141230531193, 1.445894719807367723 ) ) ;
#187841 = EDGE_CURVE ( 'NONE', #181174, #116397, #195387, .T. ) ;
#187842 = CARTESIAN_POINT ( 'NONE',  ( -3.415764635639130020, 6.072476943965863683, 1.199719254218462483 ) ) ;
#187843 = CARTESIAN_POINT ( 'NONE',  ( 1.973570569994816060, -0.2575147360633044391, 2.054139978358980656 ) ) ;
#187844 = CARTESIAN_POINT ( 'NONE',  ( 5.114917985578482096, 0.1569784262732084601, 2.111484538518786813 ) ) ;
#187845 = CARTESIAN_POINT ( 'NONE',  ( 7.610204295972345712, 7.772993188256215547, 0.7998128361456341429 ) ) ;
#187846 = CARTESIAN_POINT ( 'NONE',  ( 0.000000000000000000, 1.000000000000000888, -12.00000000000000178 ) ) ;
#187847 = CARTESIAN_POINT ( 'NONE',  ( 1.674589265674136129, 1.326639880153294371, -1.455732889183375178 ) ) ;
#187848 = CARTESIAN_POINT ( 'NONE',  ( 5.870433092755101612, 6.171306251675328092, 0.8628692295504901688 ) ) ;
#187849 = DIRECTION ( 'NONE',  ( 3.330669073875478989E-16, -3.540251991789410786E-16, -1.000000000000000000 ) ) ;
#187850 = CARTESIAN_POINT ( 'NONE',  ( 5.015721488424509822, -1.223180480392561886, -1.938471153541870384 ) ) ;
#187851 = CARTESIAN_POINT ( 'NONE',  ( 1.453431991042982041, 0.5316948868413253759, -1.746555546766684675 ) ) ;
#187852 = CARTESIAN_POINT ( 'NONE',  ( 5.204350862799327793, 7.165104988056252289, -1.599625672291281386 ) ) ;
#187853 = CARTESIAN_POINT ( 'NONE',  ( 4.758548728272192108, 7.535095368750792666, -1.082531754730549078 ) ) ;
#187854 = CARTESIAN_POINT ( 'NONE',  ( -6.320072162264675164, 10.52516795595079557, 0.7998128361456481317 ) ) ;
#187855 = CARTESIAN_POINT ( 'NONE',  ( 3.076434440837049866, 0.9091080936043660632, 1.796352098325330715 ) ) ;
#187856 = CARTESIAN_POINT ( 'NONE',  ( 3.502741298630154709, 0.4721981695934416856, 1.903977903881831191 ) ) ;
#187857 = CARTESIAN_POINT ( 'NONE',  ( -9.481229494658258261, 9.955855920056455588, -0.7998128361456291469 ) ) ;
#187858 = CARTESIAN_POINT ( 'NONE',  ( -6.749261541504576911, 6.768559974710451677, 1.040834085586084257E-14 ) ) ;
#187859 = CARTESIAN_POINT ( 'NONE',  ( 10.99999999999737632, 1.347111479061767535E-15, 0.4330127018937080519 ) ) ;
#187861 = CARTESIAN_POINT ( 'NONE',  ( 4.557331473417879586, 0.3865553534455662965, -1.726927170965624647 ) ) ;
#187860 = CARTESIAN_POINT ( 'NONE',  ( 6.597611690090901426, -2.090214587215084130, 0.04977907537380765746 ) ) ;
#187862 = CARTESIAN_POINT ( 'NONE',  ( 4.902486209380604087, 4.845403771096273182, 0.6282069583892326836 ) ) ;
#187863 = CARTESIAN_POINT ( 'NONE',  ( 0.2346725361867564585, 0.3788711812165134196, 2.158297013397599162 ) ) ;
#187864 = CARTESIAN_POINT ( 'NONE',  ( 5.349435159262297290, 1.738085940734758639, -0.09086515553361101949 ) ) ;
#187865 = CARTESIAN_POINT ( 'NONE',  ( 8.209625708274705502, 9.536650400197368427, 1.199719254218462483 ) ) ;
#187866 = CARTESIAN_POINT ( 'NONE',  ( 6.399114681295562157, -1.079681622539971464, -2.029393132690388235 ) ) ;
#187867 = CARTESIAN_POINT ( 'NONE',  ( 7.204675194429079505E-15, -1.443749999044083854, -3.475000000000000089 ) ) ;
#187868 = CARTESIAN_POINT ( 'NONE',  ( 5.940742354060237318, 1.035569694170878519, 1.390440122839208703 ) ) ;
#187869 = CARTESIAN_POINT ( 'NONE',  ( 1.963769682107346037, 0.3752889857368995608, -2.174583152744386627 ) ) ;
#187870 = CIRCLE ( 'NONE', #94539, 1.829047314007942848 ) ;
#187871 = CARTESIAN_POINT ( 'NONE',  ( 6.074718851800529507, 1.462630930118626660, -1.604749943717192373 ) ) ;
#187872 = CARTESIAN_POINT ( 'NONE',  ( 0.000000000000000000, 0.000000000000000000, 0.000000000000000000 ) ) ;
#187873 = EDGE_CURVE ( 'NONE', #189704, #45344, #22649, .T. ) ;
#187874 = CARTESIAN_POINT ( 'NONE',  ( 1.112693368687894369, 2.042276985739148731, 0.5586806735067056939 ) ) ;
#187875 = CARTESIAN_POINT ( 'NONE',  ( 3.437500000000002665, 1.451031289060976448, -1.451031289061255780 ) ) ;
#187876 = CARTESIAN_POINT ( 'NONE',  ( 6.727182134110194944, 2.413774403037728167, 2.569658639860139093 ) ) ;
#187877 = CARTESIAN_POINT ( 'NONE',  ( 4.823225626762606133, -0.09501261394700975804, 1.924175346943966414 ) ) ;
#187878 = CARTESIAN_POINT ( 'NONE',  ( 0.7861345822535183991, 2.139302153856616151, -0.5977261144227277168 ) ) ;
#187879 = ORIENTED_EDGE ( 'NONE', *, *, #173196, .T. ) ;
#187881 = CARTESIAN_POINT ( 'NONE',  ( -1.500000000000011324, 4.670833333333353821, 0.8660254037844403729 ) ) ;
#187880 = CARTESIAN_POINT ( 'NONE',  ( 1.593750267980385882, -0.7671775610453807070, 2.160330554385545110 ) ) ;
#187882 = CARTESIAN_POINT ( 'NONE',  ( 4.039439701867726384, 6.800097854565950506, 1.199719254218462483 ) ) ;
#187883 = CARTESIAN_POINT ( 'NONE',  ( 5.307127064745490230, 8.279066444590018392, -1.199719254218452935 ) ) ;
#187884 = CARTESIAN_POINT ( 'NONE',  ( 3.563320577568354075, -1.815308083731239419, 1.279909030408127091 ) ) ;
#187885 = CARTESIAN_POINT ( 'NONE',  ( -8.676855123066022912, 10.18571440074093282, -1.082531754730543971 ) ) ;
#187886 = CARTESIAN_POINT ( 'NONE',  ( 5.938108093105483931, 8.911247961056314892, -1.082531754730537088 ) ) ;
#187887 = CARTESIAN_POINT ( 'NONE',  ( -9.449669878600625239, 10.12696240122997082, -0.7216878364870267237 ) ) ;
#187888 = CARTESIAN_POINT ( 'NONE',  ( 7.187230829020129441, 8.518095734345896730, 1.082531754730549967 ) ) ;
#187889 = ORIENTED_EDGE ( 'NONE', *, *, #5202, .F. ) ;
#187890 = CARTESIAN_POINT ( 'NONE',  ( 1.283827520628720187, 1.646837967535810021, -1.163270716046126196 ) ) ;
#187892 = CARTESIAN_POINT ( 'NONE',  ( 6.215292634054179643, -1.767141628190834757, -1.063693359622622125 ) ) ;
#187891 = CARTESIAN_POINT ( 'NONE',  ( 7.079328764629950754, 11.41096732537697633, 0.7998128361456462443 ) ) ;
#187893 =( NAMED_UNIT ( * ) SI_UNIT ( $, .STERADIAN. ) SOLID_ANGLE_UNIT ( ) );
#187894 = CARTESIAN_POINT ( 'NONE',  ( 7.499068361690118145, 7.921536974826172361, -0.7216878364870317197 ) ) ;
#187895 = CARTESIAN_POINT ( 'NONE',  ( 0.2218712608162629052, 1.761692264604281633, 0.5354471447000588302 ) ) ;
#187896 = CARTESIAN_POINT ( 'NONE',  ( -1.364683531250000748, 2.259375000341422357, 1.214306433183764966E-14 ) ) ;
#187897 = CARTESIAN_POINT ( 'NONE',  ( 1.211743588231738888, -0.7890745783359112142, -1.584151303567796543 ) ) ;
#187898 = CARTESIAN_POINT ( 'NONE',  ( 0.2467204944939948574, 1.994070950632735428, -0.2986300710981006357 ) ) ;
#187899 = CARTESIAN_POINT ( 'NONE',  ( 6.603062865972897377, -0.3679811349713958957, 1.707173594542527040 ) ) ;
#187900 = CARTESIAN_POINT ( 'NONE',  ( 4.300488954165425426, 1.772315894223834176, -1.453880271152303116 ) ) ;
#187901 = CARTESIAN_POINT ( 'NONE',  ( 3.820104440490858622, 1.748809976318686177, 0.5759312369505511509 ) ) ;
#187902 = CARTESIAN_POINT ( 'NONE',  ( 8.015895134177609904, 10.37496362800581018, 1.599625672291281386 ) ) ;
#187903 = CARTESIAN_POINT ( 'NONE',  ( 3.434410497111122673, 1.780829521046650932, 0.4009754434649847044 ) ) ;
#187904 = CARTESIAN_POINT ( 'NONE',  ( 4.236954046275762664, 2.015912997090345549, -0.05229627655192746472 ) ) ;
#187905 = CARTESIAN_POINT ( 'NONE',  ( -8.805130697071332335, 12.36007068230351358, 1.199719254218462483 ) ) ;
#187907 = CARTESIAN_POINT ( 'NONE',  ( -6.095272577795516789, 9.268845886473535245, 1.199719254218452047 ) ) ;
#187906 = CARTESIAN_POINT ( 'NONE',  ( 3.784249319668216760, -1.117672106238891461, 1.967118024168002410 ) ) ;
#187908 = CARTESIAN_POINT ( 'NONE',  ( 5.438542061945497608, 2.074265116652589391, 0.3630613376124564584 ) ) ;
#187909 = CARTESIAN_POINT ( 'NONE',  ( 7.825489347732291989, 14.97139610117899444, 9.977962224420885207 ) ) ;
#187910 = CARTESIAN_POINT ( 'NONE',  ( 3.385274849524767316, 0.04804411014160993310, 2.069964801482151895 ) ) ;
#187911 = CARTESIAN_POINT ( 'NONE',  ( 10.53876547652418338, 11.18964789890005918, 0.7998128361456462443 ) ) ;
#187912 = CARTESIAN_POINT ( 'NONE',  ( 1.360316468749975582, 2.317708333674725285, -0.7853790794158961308 ) ) ;
#187913 = CARTESIAN_POINT ( 'NONE',  ( 6.287751673603878544, 2.029294879081492198, -0.6150919484220889188 ) ) ;
#187915 = CARTESIAN_POINT ( 'NONE',  ( 1.014139625077722595, -0.8655271193952519537, -1.721200913303379654 ) ) ;
#187914 = CARTESIAN_POINT ( 'NONE',  ( -9.612894607289142357, 11.17379744904754801, -1.199719254218441611 ) ) ;
#187916 = CARTESIAN_POINT ( 'NONE',  ( 9.586610838029415049, -7.161464053357574855, -0.003376046620562692113 ) ) ;
#187917 = CARTESIAN_POINT ( 'NONE',  ( 9.610031953988080744, 10.10612545594124967, -0.7998128361456281477 ) ) ;
#187918 = CARTESIAN_POINT ( 'NONE',  ( 4.001064729364292916, 6.721640380016713934, -1.082531754730548412 ) ) ;
#187919 = CARTESIAN_POINT ( 'NONE',  ( 5.290189798603822879, 6.367883502209223501, 1.128355864069837455 ) ) ;
#187920 = CARTESIAN_POINT ( 'NONE',  ( 1.150222622689962781, 3.233395032273045810, -0.7749999999993620881 ) ) ;
#187921 = CARTESIAN_POINT ( 'NONE',  ( -5.091250377131585125, 5.898545847196970726, 1.199719254218450271 ) ) ;
#187922 = CARTESIAN_POINT ( 'NONE',  ( 0.9146621208586953600, -2.221583675102642097, 0.007239306818007660779 ) ) ;
#187923 = VECTOR ( 'NONE', #126068, 1000.000000000000114 ) ;
#187924 = CARTESIAN_POINT ( 'NONE',  ( 2.503073473877976518, 1.692030140557040152, -1.253631523096561784 ) ) ;
#187925 = CARTESIAN_POINT ( 'NONE',  ( -3.492107083971660586, 6.231819477012331632, 1.199719254218452935 ) ) ;
#187926 = CARTESIAN_POINT ( 'NONE',  ( 8.586391356156291010, 8.911878091804165791, 0.7998128361456481317 ) ) ;
#187927 = CARTESIAN_POINT ( 'NONE',  ( 0.1329588055935396196, 0.006246367379872731426, -1.846049620084761367 ) ) ;
#187928 = CARTESIAN_POINT ( 'NONE',  ( 7.800018446563675489, 7.994443030612759848, -0.7998128361456281477 ) ) ;
#187929 = CARTESIAN_POINT ( 'NONE',  ( 11.96212011828584387, 9.771875549500522951, 0.9569185076417748848 ) ) ;
#187930 = CARTESIAN_POINT ( 'NONE',  ( -5.777182853198894463, 9.754147405458438058, 0.7216878364870267237 ) ) ;
#187931 = CARTESIAN_POINT ( 'NONE',  ( -9.653042183249972652, 10.36423008998754192, -0.7216878364870267237 ) ) ;
#187932 = CARTESIAN_POINT ( 'NONE',  ( -1.812896364438562946, 2.514517768406681952, 2.499891510452760368 ) ) ;
#187933 = CARTESIAN_POINT ( 'NONE',  ( -8.086512275908061653, 8.398962174839683215, 0.000000000000000000 ) ) ;
#187935 = CARTESIAN_POINT ( 'NONE',  ( 3.666413850373055006, -0.7928392042928497085, -1.794698522912529182 ) ) ;
#187934 = CARTESIAN_POINT ( 'NONE',  ( -1.225000000000005640, -1.000000000000000888, -1.908195823574487804E-14 ) ) ;
#187936 = CARTESIAN_POINT ( 'NONE',  ( 1.692469166403000491, -2.151312531270420436, -0.2117842694067117448 ) ) ;
#187937 = CARTESIAN_POINT ( 'NONE',  ( 1.733694375844633706, 1.821329977863223926, 0.2691589665217360983 ) ) ;
#187939 = CARTESIAN_POINT ( 'NONE',  ( -4.869203491162207520, 6.719169366249152731, -1.250126817991310757 ) ) ;
#187938 = CARTESIAN_POINT ( 'NONE',  ( -3.800028193580205382, 7.655393002477360653, -0.7998128361456481317 ) ) ;
#187940 = CARTESIAN_POINT ( 'NONE',  ( 3.696946667989671642, -0.5033324012985186391, 1.665945954428204923 ) ) ;
#187941 = CARTESIAN_POINT ( 'NONE',  ( 6.819388077993785657, 7.058300300521964665, 1.040834085586084257E-14 ) ) ;
#187942 = CARTESIAN_POINT ( 'NONE',  ( -11.78039045457385292, 4.728130269440308453, 4.968650233931813709 ) ) ;
#187943 = ADVANCED_FACE ( 'NONE', ( #7472 ), #73551, .F. ) ;
#187944 = CARTESIAN_POINT ( 'NONE',  ( 0.7433210806352362754, -1.853469564684958382, 1.112228649290482263 ) ) ;
#187945 = STYLED_ITEM ( 'NONE', ( #144519 ), #84085 ) ;
#187946 = CARTESIAN_POINT ( 'NONE',  ( 3.497422563753574298, 1.966343570655813666, 0.4444343670074250574 ) ) ;
#187947 = CARTESIAN_POINT ( 'NONE',  ( -10.97010717055062656, 12.30000000000000249, -1.696399592028410952 ) ) ;
#187949 = AXIS2_PLACEMENT_3D ( 'NONE', #193733, #81058, #197992 ) ;
#187948 = CARTESIAN_POINT ( 'NONE',  ( 0.1280963075596490419, -1.331634228802502928, -1.703589906866372017 ) ) ;
#187950 = CARTESIAN_POINT ( 'NONE',  ( 2.237131214483905950, -1.761753319436863086, 0.8849394531919276830 ) ) ;
#187951 = CARTESIAN_POINT ( 'NONE',  ( 6.609000000000036401, 0.5823242425131782696, 2.053003180352876100 ) ) ;
#187952 = CARTESIAN_POINT ( 'NONE',  ( 2.278764488077251738, 1.774667200368160280, -0.7891824313753895703 ) ) ;
#187955 = ORIENTED_EDGE ( 'NONE', *, *, #16995, .F. ) ;
#187954 = CARTESIAN_POINT ( 'NONE',  ( -3.987506576194992824, 7.666191748953863794, 0.7216878364870338292 ) ) ;
#187953 = CARTESIAN_POINT ( 'NONE',  ( 2.889785579457926801, 6.440540434672812786, -0.3822207396134719715 ) ) ;
#187956 = CARTESIAN_POINT ( 'NONE',  ( -4.407809337774280856, 7.196175756495025055, 1.082531754730549967 ) ) ;
#187957 = CARTESIAN_POINT ( 'NONE',  ( -0.1108833634137009749, 4.092508091048022933, -2.451885048449681914 ) ) ;
#187958 = CARTESIAN_POINT ( 'NONE',  ( 5.520104819419390907, 6.469152373191302985, 1.199719254218452935 ) ) ;
#187959 = CARTESIAN_POINT ( 'NONE',  ( -5.468734858265826837, 7.473552982767158070, 1.599625672291263179 ) ) ;
#187960 = CARTESIAN_POINT ( 'NONE',  ( -5.257529707049291900, 9.355811434857983500, 0.7998128361456291469 ) ) ;
#187961 = CARTESIAN_POINT ( 'NONE',  ( 5.508889292638126989, 1.751971812537992834, -1.501964572959401778 ) ) ;
#187962 = CARTESIAN_POINT ( 'NONE',  ( -10.49167311136684511, 5.343773310534622567, 5.730690286876297002 ) ) ;
#187963 = EDGE_CURVE ( 'NONE', #187284, #168636, #204595, .T. ) ;
#187964 = CARTESIAN_POINT ( 'NONE',  ( 4.153139481255548660, 1.659551801668930793, -1.045809187271130591 ) ) ;
#187965 = CARTESIAN_POINT ( 'NONE',  ( 7.313733799568044702, 10.62010763521636214, 1.199719254218460707 ) ) ;
#187966 = CARTESIAN_POINT ( 'NONE',  ( 0.4928148368598186946, -2.006445878461552645, 0.2004378712678403507 ) ) ;
#187967 = ORIENTED_EDGE ( 'NONE', *, *, #190385, .F. ) ;
#187968 = CARTESIAN_POINT ( 'NONE',  ( 2.624332661740484962, 2.101919520188862744, 0.2543673568942694252 ) ) ;
#187969 = CARTESIAN_POINT ( 'NONE',  ( 1.499999999999987121, 1.035416667349484232, 0.8660254037844524744 ) ) ;
#187971 = CARTESIAN_POINT ( 'NONE',  ( -6.287230548435221777, 8.358188277972981695, -1.599625672291263179 ) ) ;
#187970 = PRESENTATION_STYLE_ASSIGNMENT (( #8158 ) ) ;
#187972 = CARTESIAN_POINT ( 'NONE',  ( 2.941158370608713213, 0.6622022323767087215, -1.718108305994885177 ) ) ;
#187973 = VERTEX_POINT ( 'NONE', #57312 ) ;
#187974 = CARTESIAN_POINT ( 'NONE',  ( -9.982881178363895103, 10.54111621771303753, 1.040834085586084257E-14 ) ) ;
#187975 = CARTESIAN_POINT ( 'NONE',  ( 9.348381460497192208, 13.52536904890506264, 7.450314784081288444 ) ) ;
#187976 = CARTESIAN_POINT ( 'NONE',  ( 3.674183785563363447, 2.104178206457421485, -0.2630699042918820396 ) ) ;
#187977 = CARTESIAN_POINT ( 'NONE',  ( 0.6382991350510487383, -1.580419255802448575, 0.9442637585924051891 ) ) ;
#187978 = FACE_BOUND ( 'NONE', #105255, .T. ) ;
#187979 = CARTESIAN_POINT ( 'NONE',  ( 5.601490020740366838, 9.686822124172440596, 1.040834085586084257E-14 ) ) ;
#187980 = CARTESIAN_POINT ( 'NONE',  ( 5.742760583840166966, 8.857581893525663830, 1.199719254218452047 ) ) ;
#187981 = ORIENTED_EDGE ( 'NONE', *, *, #165987, .T. ) ;
#187982 = CARTESIAN_POINT ( 'NONE',  ( 3.848945901207713849, -1.686846252213095365, 1.183521113291643223 ) ) ;
#187984 = CARTESIAN_POINT ( 'NONE',  ( 1.628196140939692338, 0.1813696128579282696, 1.832309401408799276 ) ) ;
#187983 = CARTESIAN_POINT ( 'NONE',  ( -8.037286134802835491, 8.271255333558444889, -0.7998128361456291469 ) ) ;
#187985 = CARTESIAN_POINT ( 'NONE',  ( 0.6823417656249917140, 4.592708333674755394, 1.181850606188765695 ) ) ;
#187986 = DIRECTION ( 'NONE',  ( 0.000000000000000000, 0.000000000000000000, 1.000000000000000000 ) ) ;
#187987 = CARTESIAN_POINT ( 'NONE',  ( -9.499701791763566661, -9.918130724412307586, 0.07530116296179305280 ) ) ;
#187988 = FACE_OUTER_BOUND ( 'NONE', #36936, .T. ) ;
#187989 = CARTESIAN_POINT ( 'NONE',  ( 1.541937560865791479, -1.600244427420342896, -1.519961040588948986 ) ) ;
#187990 = CARTESIAN_POINT ( 'NONE',  ( 4.042437229998629533, 2.251021955006918596, 0.2269351218320627694 ) ) ;
#187991 = CARTESIAN_POINT ( 'NONE',  ( -7.863365906246061243, 10.19701286208565705, -1.443375672974059665 ) ) ;
#187992 = CARTESIAN_POINT ( 'NONE',  ( 3.375094514129430845, -1.600109896321648462, -0.8493348278759412784 ) ) ;
#187993 = CARTESIAN_POINT ( 'NONE',  ( 3.766719225569253204, -0.1932013629946625344, -1.905979854919868988 ) ) ;
#187994 = CARTESIAN_POINT ( 'NONE',  ( 5.811005889236001032, -1.634438611397070806, 1.270752202701043609 ) ) ;
#187995 = CARTESIAN_POINT ( 'NONE',  ( 0.6823417656249899377, 3.738541667008085767, -1.181850606188754593 ) ) ;
#187996 = CARTESIAN_POINT ( 'NONE',  ( 3.309407512850143451, -0.3859909667141645517, 1.933149248684182808 ) ) ;
#187997 = CARTESIAN_POINT ( 'NONE',  ( 1.202032481184050816, -1.926566264184792709, -0.002868833312720530347 ) ) ;
#187998 = CARTESIAN_POINT ( 'NONE',  ( 4.082764389539480732, -0.1829629792115642917, -1.861669828791753467 ) ) ;
#187999 = CARTESIAN_POINT ( 'NONE',  ( 3.229449743806306561, 0.05664919459314603917, 2.307159798345681523 ) ) ;
#188000 = CARTESIAN_POINT ( 'NONE',  ( 3.754231824312683763, -1.858861104869345082, -0.09317703841194531489 ) ) ;
#188001 = CARTESIAN_POINT ( 'NONE',  ( 1.364683531249988535, 4.905208333674756283, -0.7879004041258300672 ) ) ;
#188002 = CARTESIAN_POINT ( 'NONE',  ( 5.722423353419669567, 8.833855124701747386, 1.199719254218451159 ) ) ;
#188003 = CARTESIAN_POINT ( 'NONE',  ( 0.8914058518391498875, 1.856551077915175707, -0.9943519572734434986 ) ) ;
#188004 = CARTESIAN_POINT ( 'NONE',  ( 2.670593071767634719, 6.059516317130127838, -0.7216878364870267237 ) ) ;
#188006 = DIRECTION ( 'NONE',  ( -0.000000000000000000, -8.546850786086437571E-32, -1.000000000000000000 ) ) ;
#188005 = CARTESIAN_POINT ( 'NONE',  ( 0.6823417656249899377, 5.238541667008086655, -1.181850606188754593 ) ) ;
#188007 = CARTESIAN_POINT ( 'NONE',  ( 6.925078400183550364, -0.007619068086212391067, 2.144148427808051594 ) ) ;
#188008 = CARTESIAN_POINT ( 'NONE',  ( 6.966220764712146796, 6.002124920821316323, -2.500000000000000444 ) ) ;
#188009 = CARTESIAN_POINT ( 'NONE',  ( 0.5803392809272100994, 0.9991348162329892757, 1.755301537792392175 ) ) ;
#188010 = CARTESIAN_POINT ( 'NONE',  ( 1.364683531249986537, 0.3635416670080869328, 0.7879004041258500513 ) ) ;
#188011 = CARTESIAN_POINT ( 'NONE',  ( -3.877268743828284681, 5.546566172598190292, 1.443375672974064550 ) ) ;
#188012 = CARTESIAN_POINT ( 'NONE',  ( 3.988069740714122791, 7.804498464141805592, 0.7998128361456321445 ) ) ;
#188013 = EDGE_LOOP ( 'NONE', ( #37278, #93181, #122539, #186420 ) ) ;
#188014 = CARTESIAN_POINT ( 'NONE',  ( 0.8257154465432202661, -2.052837714267462754, 0.6772920067378007669 ) ) ;
#188015 = EDGE_CURVE ( 'NONE', #179471, #64456, #178074, .T. ) ;
#188018 = CARTESIAN_POINT ( 'NONE',  ( 4.039966587192267866, 4.776011108888172707, 1.082531754730560403 ) ) ;
#188017 = CARTESIAN_POINT ( 'NONE',  ( 6.925078400183590333, 2.970608243536181359, 2.408862486266015512 ) ) ;
#188016 = CARTESIAN_POINT ( 'NONE',  ( 6.574778147984297938, 6.635272358928617997, -0.7998128361456481317 ) ) ;
#188019 = LINE ( 'NONE', #38586, #155167 ) ;
#188020 = CARTESIAN_POINT ( 'NONE',  ( 5.559779856078610472, 1.205038519190555268, 1.616695979245158066 ) ) ;
#188021 = CARTESIAN_POINT ( 'NONE',  ( -8.514157279702033065, 9.995900250149611921, -1.082531754730543971 ) ) ;
#188022 = CARTESIAN_POINT ( 'NONE',  ( 0.3983070667218471805, -0.7439898890007863308, -2.061537379893277677 ) ) ;
#188023 = CARTESIAN_POINT ( 'NONE',  ( -2.937463097380563013E-12, -7.034525084947490292, -10.67552547708197608 ) ) ;
#188025 = CARTESIAN_POINT ( 'NONE',  ( -1.364683531250014514, 10.83854166700806942, -0.7879004041258335089 ) ) ;
#188024 = CARTESIAN_POINT ( 'NONE',  ( 0.9016947886714383742, 1.851236229948808543, 1.300475659685183416 ) ) ;
#188026 = CARTESIAN_POINT ( 'NONE',  ( -7.960608749518247151, 12.43912730774665576, 0.000000000000000000 ) ) ;
#188028 = CARTESIAN_POINT ( 'NONE',  ( 1.352997864604365885, 0.1391545085356447886, -1.910588907247000368 ) ) ;
#188027 = CARTESIAN_POINT ( 'NONE',  ( -6.385527161912131433, 6.552129231760014605, 0.7216878364870317197 ) ) ;
#188029 = CARTESIAN_POINT ( 'NONE',  ( 1.364683531249988757, 2.446875000341415696, 1.214306433183764966E-14 ) ) ;
#188030 = CARTESIAN_POINT ( 'NONE',  ( -6.661184041420952440, -7.246166700180828535, 6.773376349083140013 ) ) ;
#188031 = CARTESIAN_POINT ( 'NONE',  ( 0.7500000000000006661, 9.416666666666669627, -1.299038105676657340 ) ) ;
#188032 = CARTESIAN_POINT ( 'NONE',  ( 2.701417116451056533, -0.5414251306648624196, 1.637772108618321454 ) ) ;
#188033 = CARTESIAN_POINT ( 'NONE',  ( 4.095444919779759552, 6.935713618788495793, 1.199719254218451159 ) ) ;
#188034 = CARTESIAN_POINT ( 'NONE',  ( 2.459888865612788855, 0.7521488021439284299, 1.602074255657309099 ) ) ;
#188035 = COLOUR_RGB ( '', 0.66274510, 0.83137255, 0.94901961) ;
#188036 = CARTESIAN_POINT ( 'NONE',  ( 5.719807747550186505, -2.154180246964752410, 0.4782370604126117142 ) ) ;
#188037 = ORIENTED_EDGE ( 'NONE', *, *, #200653, .T. ) ;
#188038 = CARTESIAN_POINT ( 'NONE',  ( 4.095966777872499520, 1.322572826423114911, 1.526597406435834081 ) ) ;
#188039 = CARTESIAN_POINT ( 'NONE',  ( -5.101610940492132151, 9.173906207207963348, -0.7998128361456362523 ) ) ;
#188041 = CARTESIAN_POINT ( 'NONE',  ( 4.112907772398490813, 0.1017678201147946826, 2.013986186455194449 ) ) ;
#188040 = CARTESIAN_POINT ( 'NONE',  ( 4.319064098534145302, 1.638436671179326787, -1.346072318137331969 ) ) ;
#188042 = ORIENTED_EDGE ( 'NONE', *, *, #158186, .T. ) ;
#188043 = CARTESIAN_POINT ( 'NONE',  ( 4.227110032410640095, 8.153655147779589996, 0.7998128361456271485 ) ) ;
#188044 = ORIENTED_EDGE ( 'NONE', *, *, #88762, .T. ) ;
#188045 = CARTESIAN_POINT ( 'NONE',  ( 1.498681428038322272, 1.531199225506232553, -1.074333469806128427 ) ) ;
#188047 = AXIS2_PLACEMENT_3D ( 'NONE', #202577, #20632, #109188 ) ;
#188046 = CARTESIAN_POINT ( 'NONE',  ( -10.91877977293360047, -9.985078020775008056, 0.1443118549625500291 ) ) ;
#188048 = CARTESIAN_POINT ( 'NONE',  ( 6.006502151196043471, -1.803439199047681907, -0.1703578026433834602 ) ) ;
#188049 = CARTESIAN_POINT ( 'NONE',  ( -4.776550190716183586, 4.467063398790632966, 1.214306433183764966E-14 ) ) ;
#188050 = CARTESIAN_POINT ( 'NONE',  ( 1.419999999999990603, 6.280000000000042881, 2.580000000000000515 ) ) ;
#188051 = SURFACE_STYLE_FILL_AREA ( #75391 ) ;
#188052 = CARTESIAN_POINT ( 'NONE',  ( -0.6823417656250212460, 2.613541667008084879, 1.181850606188767472 ) ) ;
#188053 = LINE ( 'NONE', #26628, #205626 ) ;
#188054 = ORIENTED_EDGE ( 'NONE', *, *, #140722, .F. ) ;
#188055 = ADVANCED_FACE ( 'NONE', ( #122406 ), #146607, .F. ) ;
#188056 = CARTESIAN_POINT ( 'NONE',  ( 7.512626515748113576, 7.937354821227203594, 0.7216878364870267237 ) ) ;
#188057 = CARTESIAN_POINT ( 'NONE',  ( -3.797692425603673705, 6.484372692295976570, 1.082531754730549967 ) ) ;
#188058 = CARTESIAN_POINT ( 'NONE',  ( -5.424143973919053785, 8.485862515284315677, 1.199719254218454489 ) ) ;
#188059 = CARTESIAN_POINT ( 'NONE',  ( 4.236665939827915395, 1.302216991916404387, -1.673619383358643908 ) ) ;
#188061 = CARTESIAN_POINT ( 'NONE',  ( -10.16814981310353616, 6.288261174334121684, -5.589887627215723853 ) ) ;
#188060 = CARTESIAN_POINT ( 'NONE',  ( 2.044581833100483692, 2.972657967446784788, -11.47952151275210930 ) ) ;
#188062 = CARTESIAN_POINT ( 'NONE',  ( 5.747334165637288272, -1.552519754122901663, -1.214743736649764649 ) ) ;
#188063 = CARTESIAN_POINT ( 'NONE',  ( -1.364683531250000748, 1.509375000341421691, 0.000000000000000000 ) ) ;
#188064 = CARTESIAN_POINT ( 'NONE',  ( 0.4221356392010866543, -2.003110517487953324, 0.2016333174496009462 ) ) ;
#188065 = ORIENTED_EDGE ( 'NONE', *, *, #40506, .F. ) ;
#188066 = CARTESIAN_POINT ( 'NONE',  ( 0.5095558700928676243, -2.008984845895735116, 0.6684745883070477568 ) ) ;
#188068 = ADVANCED_FACE ( 'NONE', ( #210998 ), #185002, .T. ) ;
#188067 = CARTESIAN_POINT ( 'NONE',  ( 8.809690371089201832, 13.28836970969089393, 8.148114100277203065 ) ) ;
#188069 = CARTESIAN_POINT ( 'NONE',  ( 1.732962091629593804, -1.965256999408044436, -0.6514315320021792921 ) ) ;
#188070 = EDGE_LOOP ( 'NONE', ( #31850, #2144, #204296, #142841, #154599, #178916, #200538 ) ) ;
#188071 = CARTESIAN_POINT ( 'NONE',  ( 4.206772801990143584, 8.129928378955675328, 0.7998128361456271485 ) ) ;
#188072 = CARTESIAN_POINT ( 'NONE',  ( 4.603875680292229156, 7.528882839386387360, 1.199719254218452047 ) ) ;
#188074 = CARTESIAN_POINT ( 'NONE',  ( 5.301401758143367893, 6.143722458377430584, 1.199719254218462483 ) ) ;
#188073 = CARTESIAN_POINT ( 'NONE',  ( 4.224618542793646014, 0.1023655851960032920, 2.088258538514795593 ) ) ;
#188075 = CARTESIAN_POINT ( 'NONE',  ( 7.201315867513990554, 8.430565262634994284, -1.199719254218452047 ) ) ;
#188078 = ORIENTED_EDGE ( 'NONE', *, *, #174801, .F. ) ;
#188077 = CARTESIAN_POINT ( 'NONE',  ( 1.435880962511564718, -1.006192904286895340, -1.506089461148002018 ) ) ;
#188076 = CARTESIAN_POINT ( 'NONE',  ( 3.082817581614716307, -0.1327354176642106531, -1.820802398864965088 ) ) ;
#188079 = CARTESIAN_POINT ( 'NONE',  ( 9.499562802171208631, -9.415754203682769941, -0.1226201807150868461 ) ) ;
#188080 = CARTESIAN_POINT ( 'NONE',  ( 3.719872605471109761, 6.605953636083950364, -2.500000000000002220 ) ) ;
#188081 = CARTESIAN_POINT ( 'NONE',  ( 4.067547972739316897, 0.2730280005818259137, -2.189760481282684967 ) ) ;
#188082 = CARTESIAN_POINT ( 'NONE',  ( 8.121497709785879593, 9.433834401960398353, -1.199719254218445830 ) ) ;
#188083 = CARTESIAN_POINT ( 'NONE',  ( -0.6823417656250003738, 9.963541667008065872, 1.181850606188754593 ) ) ;
#188084 = CARTESIAN_POINT ( 'NONE',  ( 2.314975094136799694, 1.534822137071165660, -1.140449143091977646 ) ) ;
#188085 = CARTESIAN_POINT ( 'NONE',  ( 8.284195553149872993, 9.623648552551724578, -1.199719254218445830 ) ) ;
#188086 = CARTESIAN_POINT ( 'NONE',  ( 5.969205681473694902, 1.824102622056431811, 0.9793482939001868504 ) ) ;
#188087 = CARTESIAN_POINT ( 'NONE',  ( -1.360316468750056851, 0.6510416670080610979, -0.7853790794158981292 ) ) ;
#188088 = CARTESIAN_POINT ( 'NONE',  ( 6.128506746050899068, 0.2130254606748181456, 2.181202035047181020 ) ) ;
#188089 = DIRECTION ( 'NONE',  ( 1.779758311459934189E-16, 0.000000000000000000, -1.000000000000000000 ) ) ;
#188090 = FACE_OUTER_BOUND ( 'NONE', #175653, .T. ) ;
#188091 = ORIENTED_EDGE ( 'NONE', *, *, #89116, .T. ) ;
#188092 = CARTESIAN_POINT ( 'NONE',  ( 1.404019654741015755, -1.209281689291617834, 1.481605035838507334 ) ) ;
#188093 = CARTESIAN_POINT ( 'NONE',  ( 5.435893244436359240, 5.306573304789342416, -0.7998128361456481317 ) ) ;
#188094 = CARTESIAN_POINT ( 'NONE',  ( 4.647606103345025552, 8.407977806742819027, 0.6343139517084724899 ) ) ;
#188095 = CARTESIAN_POINT ( 'NONE',  ( -0.2409995289980003397, 0.7158067089181943121, -2.082568332340509087 ) ) ;
#188096 = AXIS2_PLACEMENT_3D ( 'NONE', #164963, #196406, #62142 ) ;
#188097 = EDGE_CURVE ( 'NONE', #94442, #205391, #133156, .T. ) ;
#188098 = CARTESIAN_POINT ( 'NONE',  ( -8.690413276679693766, 9.241163032322203819, 1.040834085586084257E-14 ) ) ;
#188099 = CARTESIAN_POINT ( 'NONE',  ( 3.223806664999388172, 6.983134552466421674, -0.7998128361456362523 ) ) ;
#188100 = CARTESIAN_POINT ( 'NONE',  ( 5.418829850390409320, -1.503349927839289002, 1.423607673449282851 ) ) ;
#188101 = CARTESIAN_POINT ( 'NONE',  ( 4.160710321027959679, -1.426769435979913236, 1.294678423299196579 ) ) ;
#188102 = CARTESIAN_POINT ( 'NONE',  ( 1.054314798682391530, -1.277026470193865171, 1.560515422851154854 ) ) ;
#188103 = AXIS2_PLACEMENT_3D ( 'NONE', #156391, #159581, #42658 ) ;
#188104 = CARTESIAN_POINT ( 'NONE',  ( -8.188234707649510113, 11.64035869464474082, -1.199719254218446718 ) ) ;
#188105 = CARTESIAN_POINT ( 'NONE',  ( 4.598150373690133463, 5.393538853173795111, -1.199719254218452047 ) ) ;
#188106 = SURFACE_SIDE_STYLE ('',( #150296 ) ) ;
#188107 = CARTESIAN_POINT ( 'NONE',  ( 1.095947417326826212, -2.191629467406099430, 0.003159298377679311057 ) ) ;
#188108 = CARTESIAN_POINT ( 'NONE',  ( 5.707590141996651489, -0.4392596013848491521, 1.771934311310577659 ) ) ;
#188109 = CARTESIAN_POINT ( 'NONE',  ( -4.303823697334223652, 7.108545849276850959, -1.199719254218452047 ) ) ;
#188110 = CARTESIAN_POINT ( 'NONE',  ( 5.722950238744200391, 7.770137593325314285, 1.443375672974065660 ) ) ;
#188111 = CARTESIAN_POINT ( 'NONE',  ( 10.39640486358069360, 11.02356051713265650, 0.7998128361456462443 ) ) ;
#188112 = CARTESIAN_POINT ( 'NONE',  ( -4.769436176957319695, 8.786368983084006601, 0.7998128361456281477 ) ) ;
#188113 = CARTESIAN_POINT ( 'NONE',  ( 4.385172619016207918, 7.203452924572514959, 1.199719254218462483 ) ) ;
#188114 = CARTESIAN_POINT ( 'NONE',  ( 3.770049233051776749, 6.556085317605844232, 1.199719254218451159 ) ) ;
#188115 = ORIENTED_EDGE ( 'NONE', *, *, #178239, .T. ) ;
#188117 = CARTESIAN_POINT ( 'NONE',  ( 6.222908185483853494, 1.488938611106488841, -1.355157726057078404 ) ) ;
#188116 = CARTESIAN_POINT ( 'NONE',  ( 2.577489280727011778, -0.9446877197298314544, 1.580272903027237774 ) ) ;
#188118 = CARTESIAN_POINT ( 'NONE',  ( 2.232162068744643069, -2.100961912546659871, -0.9323289839222002051 ) ) ;
#188120 = CARTESIAN_POINT ( 'NONE',  ( 6.807479307002794577, -1.573682814073861902, -1.171087784426767753 ) ) ;
#188119 = CARTESIAN_POINT ( 'NONE',  ( 2.901081683644312736, 6.328419697652925002, 0.7216878364870338292 ) ) ;
#188121 = CARTESIAN_POINT ( 'NONE',  ( -5.096975683733680818, 8.033889833409558534, -1.199719254218452047 ) ) ;
#188122 = CARTESIAN_POINT ( 'NONE',  ( 11.24798771954521293, -6.442483420751878853, -0.4630894006630673077 ) ) ;
#188123 = CARTESIAN_POINT ( 'NONE',  ( 3.656429697474584017, 1.903630103707624865, 0.1825790434749063051 ) ) ;
#188124 = CARTESIAN_POINT ( 'NONE',  ( -8.272446282632566650, 12.80293776304669962, 0.7998128361456481317 ) ) ;
#188125 = CARTESIAN_POINT ( 'NONE',  ( 0.2036857628631080219, -1.599406074100502506, -1.314310892166506095 ) ) ;
#188126 = CARTESIAN_POINT ( 'NONE',  ( -2.959422669532919326, 6.674686557755516780, 0.7998128361456352531 ) ) ;
#188128 = CARTESIAN_POINT ( 'NONE',  ( 0.9537216069140028729, 1.868711056098860235, -0.08788249432020722729 ) ) ;
#188127 = CARTESIAN_POINT ( 'NONE',  ( 2.155913254374627552, 0.8966022695893551830, 1.888892756932699646 ) ) ;
#188129 = CARTESIAN_POINT ( 'NONE',  ( 2.003279617838377824, 1.993765885540278004, 0.2985825316763612847 ) ) ;
#188130 = CARTESIAN_POINT ( 'NONE',  ( 8.920901888112002354, 9.510066412326583674, 0.7216878364870438212 ) ) ;
#188131 = ORIENTED_EDGE ( 'NONE', *, *, #72841, .T. ) ;
#188132 = CARTESIAN_POINT ( 'NONE',  ( -0.6823417656250212460, 3.863541667008085767, 1.181850606188767472 ) ) ;
#188133 = CARTESIAN_POINT ( 'NONE',  ( 3.649730646487856056, 0.6304092353721781894, 1.622436561192377891 ) ) ;
#188134 = CARTESIAN_POINT ( 'NONE',  ( 5.169736645512481132, 4.925780929386339935, 0.7998128361456341429 ) ) ;
#188136 = CARTESIAN_POINT ( 'NONE',  ( 0.4139252888115696472, 3.006731736636585328, -1.957985015624248204 ) ) ;
#188135 = CARTESIAN_POINT ( 'NONE',  ( 1.333449616921239089, 8.249651149236392200, 11.01993490927446828 ) ) ;
#188137 = CARTESIAN_POINT ( 'NONE',  ( 2.613528241349000858, -1.706151288242565567, 0.2525731233022251443 ) ) ;
#188138 = CARTESIAN_POINT ( 'NONE',  ( 3.070069520051089906, -1.303570237086741024, 1.761582097007891923 ) ) ;
#188139 = CARTESIAN_POINT ( 'NONE',  ( 5.321004863918796346, 2.037934703285459115, 0.8473243778325880715 ) ) ;
#188140 = CARTESIAN_POINT ( 'NONE',  ( -10.48363756508902611, 5.078564944783316548, -7.119907325005036647 ) ) ;
#188141 = CARTESIAN_POINT ( 'NONE',  ( 3.186559800492471783, 1.209906992153013894, -1.802498320862821579 ) ) ;
#188142 = CARTESIAN_POINT ( 'NONE',  ( 2.297230901563730665, 1.410920830412419003, 1.158640757216542028 ) ) ;
#188144 = EDGE_CURVE ( 'NONE', #116165, #94694, #79034, .T. ) ;
#188143 = CARTESIAN_POINT ( 'NONE',  ( 0.3737810522974581717, -1.925036204310347943, 0.3769080146646397456 ) ) ;
#188145 = CARTESIAN_POINT ( 'NONE',  ( 4.100857973768299303, 1.937344669444723166, 0.8546590867991187279 ) ) ;
#188146 = CARTESIAN_POINT ( 'NONE',  ( 1.836970198721030181E-16, 13.49999999999999822, 1.500000000000000222 ) ) ;
#188147 = VERTEX_POINT ( 'NONE', #164403 ) ;
#188149 = CARTESIAN_POINT ( 'NONE',  ( -0.6823417656250003738, 2.030208333674753174, -1.181850606188749264 ) ) ;
#188148 = CARTESIAN_POINT ( 'NONE',  ( 5.038769576086907342, -1.967128976631225434, 1.176836258767649745 ) ) ;
#188150 = CARTESIAN_POINT ( 'NONE',  ( 0.07755575628183573877, -0.002876890934064984216, -2.188974970840869005 ) ) ;
#188151 = CARTESIAN_POINT ( 'NONE',  ( 10.16199982864259788, 11.81442020729326536, 1.199719254218452047 ) ) ;
#188152 = CARTESIAN_POINT ( 'NONE',  ( 0.2410938523699951708, 2.030451451530786766, 0.6113826261911479154 ) ) ;
#188153 = CARTESIAN_POINT ( 'NONE',  ( -5.341549334104202629, 7.254893527920112994, 1.443375672974064550 ) ) ;
#188154 = CARTESIAN_POINT ( 'NONE',  ( 4.039966587192259873, 5.736380323189513852, 1.443375672974062551 ) ) ;
#188155 = CARTESIAN_POINT ( 'NONE',  ( -5.382223794500843539, 7.302347065049529462, -1.443375672974051449 ) ) ;
#188156 = ORIENTED_EDGE ( 'NONE', *, *, #208257, .T. ) ;
#188157 = CARTESIAN_POINT ( 'NONE',  ( 5.678361341766085424, 1.528739221709461082, 1.314999087022615587 ) ) ;
#188159 = CARTESIAN_POINT ( 'NONE',  ( 3.080982041725123910, 1.940567726598545040, 0.6991345639211270502 ) ) ;
#188158 = CARTESIAN_POINT ( 'NONE',  ( 4.286349120214771879, 8.152491073559232859, -0.7998128361456221525 ) ) ;
#188161 = CARTESIAN_POINT ( 'NONE',  ( -0.2409995289980003397, 2.873648158547074338, -2.488896373646624749 ) ) ;
#188160 = CARTESIAN_POINT ( 'NONE',  ( 5.996449078994045223, 10.21788403546024782, 0.7998128361456331437 ) ) ;
#188162 = CARTESIAN_POINT ( 'NONE',  ( 7.635176783151273128, 8.936736330878529699, 1.199719254218452935 ) ) ;
#188163 = CARTESIAN_POINT ( 'NONE',  ( -3.285556943749998737, -1.830208332855373987, 1.896917185911908499 ) ) ;
#188164 = DIRECTION ( 'NONE',  ( -1.000000000000000000, -3.451266460341925773E-31, -8.638326563840809144E-31 ) ) ;
#188165 = CARTESIAN_POINT ( 'NONE',  ( 6.281208295753298643, 1.508423295503196648, 1.589913042345507455 ) ) ;
#188166 = CARTESIAN_POINT ( 'NONE',  ( 3.270157880292836605, 1.821742160604752137, -0.8647241845514613834 ) ) ;
#188167 = CARTESIAN_POINT ( 'NONE',  ( 3.737712173649463399, 1.832726675769575486, 0.1767833568970395008 ) ) ;
#188168 = CARTESIAN_POINT ( 'NONE',  ( 4.819033534653518025, 7.709623992816043270, -1.199719254218452047 ) ) ;
#188169 = CARTESIAN_POINT ( 'NONE',  ( 2.250000000000001776, 1.285947368876626068E-13, 2.052068128417949389 ) ) ;
#188170 = CARTESIAN_POINT ( 'NONE',  ( 0.5160737793865723955, 1.194803229551535173, -1.244154219207161960 ) ) ;
#188171 = CARTESIAN_POINT ( 'NONE',  ( 0.02903434592765696126, -5.609732095436333665, 10.94445979172680516 ) ) ;
#188172 = CARTESIAN_POINT ( 'NONE',  ( 1.196342457394595993, 2.030139636617489085, 1.078195451733245047 ) ) ;
#188173 = CARTESIAN_POINT ( 'NONE',  ( -6.364663046611467756, 9.512858423433634414, 1.199719254218452047 ) ) ;
#188174 = CARTESIAN_POINT ( 'NONE',  ( 0.3689490567273964738, -1.476270946665221517, 1.714425361395756964 ) ) ;
#188175 = CARTESIAN_POINT ( 'NONE',  ( 1.787856894401329333, 1.453325235529376869, 1.524497383921459726 ) ) ;
#188176 = CARTESIAN_POINT ( 'NONE',  ( -4.990283058281743678, 7.979691447040783814, -1.199719254218453823 ) ) ;
#188177 = CARTESIAN_POINT ( 'NONE',  ( 8.046927864910717432, 9.346836249606042202, 1.199719254218462483 ) ) ;
#188178 = CARTESIAN_POINT ( 'NONE',  ( 6.658462837642799670, 6.940830530104329377, 0.7216878364870328300 ) ) ;
#188179 = CARTESIAN_POINT ( 'NONE',  ( -6.307567778855718288, 8.381915046796901692, -1.599625672291263179 ) ) ;
#188180 = CARTESIAN_POINT ( 'NONE',  ( 7.741342523278707866, 8.133913820021057006, 0.7216878364870458196 ) ) ;
#188181 = CARTESIAN_POINT ( 'NONE',  ( 4.715454802112915011, 7.044561259014620269, 1.385117731104364536 ) ) ;
#188182 = CARTESIAN_POINT ( 'NONE',  ( -5.220052836461385404, 6.048815383081766583, -1.199719254218446718 ) ) ;
#188183 = CARTESIAN_POINT ( 'NONE',  ( 3.797323596237450971, -0.2205154750010793197, -2.210469098741683514 ) ) ;
#188184 = CARTESIAN_POINT ( 'NONE',  ( 2.220887445055406584, 0.001640320231081903845, 2.191629467496846839 ) ) ;
#188185 = CARTESIAN_POINT ( 'NONE',  ( -5.117312914154178216, 8.057616602233474978, -1.199719254218452047 ) ) ;
#188186 = CARTESIAN_POINT ( 'NONE',  ( 0.6278963055918493907, -2.094311335337955882, 0.6960538111202837497 ) ) ;
#188187 = CARTESIAN_POINT ( 'NONE',  ( -4.797606254389363833, 6.690569611577942943, 1.599625672291263179 ) ) ;
#188188 = CARTESIAN_POINT ( 'NONE',  ( 5.248475795274027078, -1.946838731704622072, -0.2419367024937419397 ) ) ;
#188189 = DIRECTION ( 'NONE',  ( 0.000000000000000000, 0.000000000000000000, -1.000000000000000000 ) ) ;
#188190 = CARTESIAN_POINT ( 'NONE',  ( -1.402160292154681736E-14, 2.196875000341423689, -1.575800808251660134 ) ) ;
#188191 = CARTESIAN_POINT ( 'NONE',  ( -3.797692425603673705, 6.484372692295976570, 1.082531754730549967 ) ) ;
#188192 = CARTESIAN_POINT ( 'NONE',  ( -6.412643469583822586, 6.583764924043652655, 1.040834085586084257E-14 ) ) ;
#188193 = CARTESIAN_POINT ( 'NONE',  ( 4.799148092389167175, -0.2621723519393297508, -2.104289960152181393 ) ) ;
#188194 = CARTESIAN_POINT ( 'NONE',  ( -5.659602779061863487, 5.567567761852417085, 0.7998128361456281477 ) ) ;
#188195 = EDGE_LOOP ( 'NONE', ( #109708, #24141 ) ) ;
#188196 = CARTESIAN_POINT ( 'NONE',  ( 5.893488898593548520, 1.633865717575968324, 1.415524914074948404 ) ) ;
#188197 = CARTESIAN_POINT ( 'NONE',  ( 6.440286661691305703, 7.472421512516709718, 1.199719254218462483 ) ) ;
#188198 = CARTESIAN_POINT ( 'NONE',  ( 5.231922985772964552, 1.814955821992572993, 0.3091130605668013231 ) ) ;
#188199 = CARTESIAN_POINT ( 'NONE',  ( -5.887541547804238995, 6.014758725225416214, 0.2650624260464862214 ) ) ;
#188200 = CARTESIAN_POINT ( 'NONE',  ( 1.364683531249988757, 1.696875000341414808, 0.000000000000000000 ) ) ;
#188201 = CARTESIAN_POINT ( 'NONE',  ( 6.580030513128129144, -1.708294420148011472, -0.3314369902002142765 ) ) ;
#188202 = CARTESIAN_POINT ( 'NONE',  ( 6.827182134110196365, 4.700652535171166768, 2.373648650996477372 ) ) ;
#188203 = CARTESIAN_POINT ( 'NONE',  ( 0.000000000000000000, 15.50000000000019362, 0.000000000000000000 ) ) ;
#188204 = EDGE_CURVE ( 'NONE', #115124, #142909, #67329, .T. ) ;
#188205 = CARTESIAN_POINT ( 'NONE',  ( 3.977527890101069996, 2.036293384626610248, -0.7259696361804208742 ) ) ;
#188206 = CARTESIAN_POINT ( 'NONE',  ( -3.276266675996675204, 6.974061555304760240, -0.7998128361456281477 ) ) ;
#188207 = CARTESIAN_POINT ( 'NONE',  ( -8.825994812371996900, 9.399341490629888440, 0.7216878364870438212 ) ) ;
#188208 = CARTESIAN_POINT ( 'NONE',  ( 2.975616057669258741, 2.053088362031017855, -0.6768339029224537118 ) ) ;
#188209 = CARTESIAN_POINT ( 'NONE',  ( 5.413337677306027551, -0.2920802625693446619, 1.949502277767001690 ) ) ;
#188210 = CARTESIAN_POINT ( 'NONE',  ( 4.042145929572971141, 1.632826047920731050, -0.5835893337435077433 ) ) ;
#188211 = CARTESIAN_POINT ( 'NONE',  ( 1.294752383181968503, 1.788903229852260246, -1.265732775075766092 ) ) ;
#188212 = CARTESIAN_POINT ( 'NONE',  ( 1.431196836673795936, 2.224535207900823153, 0.6132342015414853353 ) ) ;
#188213 = CARTESIAN_POINT ( 'NONE',  ( 3.884101140911602634, -1.018864849042991461, 1.791236251998897133 ) ) ;
#188214 = CARTESIAN_POINT ( 'NONE',  ( 5.812047917624927784, 1.301047364602755829, -1.442011890679588904 ) ) ;
#188215 = CARTESIAN_POINT ( 'NONE',  ( -7.443063143778079649, 10.66702885350765584, 1.082531754730549967 ) ) ;
#188216 = CARTESIAN_POINT ( 'NONE',  ( -5.818384198920079520, 6.817144982608731141, 1.199719254218452935 ) ) ;
#188217 = CARTESIAN_POINT ( 'NONE',  ( -11.86145016429273014, 13.40000000000000036, -1.100000000000002087 ) ) ;
#188219 = ORIENTED_EDGE ( 'NONE', *, *, #91556, .T. ) ;
#188218 = CARTESIAN_POINT ( 'NONE',  ( -3.923105346307911745, 5.670318552149568703, -1.599625672291283607 ) ) ;
#188220 = CARTESIAN_POINT ( 'NONE',  ( -8.175203438916030407, 8.640084888264587093, 0.7216878364870578100 ) ) ;
#188221 = CARTESIAN_POINT ( 'NONE',  ( 3.030518406005321186, 1.227118389542980026, -1.833929004854919054 ) ) ;
#188222 = CARTESIAN_POINT ( 'NONE',  ( 3.285556943750000514, -0.3135416661887098777, 1.896917185911906500 ) ) ;
#188223 = EDGE_LOOP ( 'NONE', ( #80522, #129901 ) ) ;
#188224 = CARTESIAN_POINT ( 'NONE',  ( 0.2329586101569866563, 0.008238550247445517935, -1.845944905557160398 ) ) ;
#188225 = CARTESIAN_POINT ( 'NONE',  ( -0.1291982275798392032, 1.351143144720265532, -2.329141727150272789 ) ) ;
#188226 = CARTESIAN_POINT ( 'NONE',  ( -1.201851678989727383E-14, 5.118750000682815937, -1.732050807568863648 ) ) ;
#188227 = CARTESIAN_POINT ( 'NONE',  ( 4.492266506575326446, 7.256230230409263626, -1.267781117195718288 ) ) ;
#188229 = CARTESIAN_POINT ( 'NONE',  ( -3.602337597214539753E-15, 12.59375000068279782, 1.500000000000001554 ) ) ;
#188228 = CARTESIAN_POINT ( 'NONE',  ( -5.946407990378149933, 7.222024315256661886, -1.239984355232233826 ) ) ;
#188230 = CARTESIAN_POINT ( 'NONE',  ( 6.527308116070499544, -1.206667617865687214, -1.390688675169844624 ) ) ;
#188231 = ORIENTED_EDGE ( 'NONE', *, *, #133268, .F. ) ;
#188232 = CARTESIAN_POINT ( 'NONE',  ( 1.850533416564412725, 0.6455992098736047513, 1.957236905219070566 ) ) ;
#188233 = CARTESIAN_POINT ( 'NONE',  ( -1.360316468750006669, 1.119791667008071201, -0.7853790794158921340 ) ) ;
#188234 = CARTESIAN_POINT ( 'NONE',  ( -7.555971681517696936, 7.709721804725773175, 0.7998128361456462443 ) ) ;
#188235 = SURFACE_SIDE_STYLE ('',( #26805 ) ) ;
#188236 = FILL_AREA_STYLE_COLOUR ( '', #189227 ) ;
#188237 = CARTESIAN_POINT ( 'NONE',  ( 5.508690485854129903, 5.321227076451600091, 1.040834085586084257E-14 ) ) ;
#188238 = CARTESIAN_POINT ( 'NONE',  ( 1.375931059888847896, 1.226954981729235561, 1.655701539656707411 ) ) ;
#188240 = CARTESIAN_POINT ( 'NONE',  ( 5.302248432823610358, 1.390444127666954355, -1.207098008268410183 ) ) ;
#188239 = CARTESIAN_POINT ( 'NONE',  ( -1.500000000000001110, 12.52083333333333215, 0.8660254037844418162 ) ) ;
#188241 = CARTESIAN_POINT ( 'NONE',  ( 5.198661835836162481, 8.152523677529138979, 1.199719254218462483 ) ) ;
#188242 = CARTESIAN_POINT ( 'NONE',  ( -6.629010762438975135, 6.698543742459062145, -0.7998128361456362523 ) ) ;
#188243 = CARTESIAN_POINT ( 'NONE',  ( -0.2409995289980245703, 0.2355275985303668385, -2.034371242098035548 ) ) ;
#188244 = CARTESIAN_POINT ( 'NONE',  ( 4.670673364294657404, -1.443042178620690841, 1.669811033208345341 ) ) ;
#188245 = CARTESIAN_POINT ( 'NONE',  ( 0.1811626231076196580, -0.1537715369321658587, -2.127283700313627346 ) ) ;
#188246 = CARTESIAN_POINT ( 'NONE',  ( -5.436456409399874623, 5.444880020495701523, 0.000000000000000000 ) ) ;
#188247 = CARTESIAN_POINT ( 'NONE',  ( 0.4219365929402639215, -1.902980170924161385, 0.1897552588234762416 ) ) ;
#188248 = CARTESIAN_POINT ( 'NONE',  ( 1.007046422456716384, -0.04465021774549028655, 2.016188868504041665 ) ) ;
#188249 = CARTESIAN_POINT ( 'NONE',  ( -6.783773228136968036, -6.684699857435323800, 6.634380643896202301 ) ) ;
#188250 = CARTESIAN_POINT ( 'NONE',  ( 1.406082690172899108, 0.4493768194517386849, 2.253890741632145200 ) ) ;
#188251 = CARTESIAN_POINT ( 'NONE',  ( 6.825078400183573812, 0.002648415797040087893, 1.855566311045192540 ) ) ;
#188252 = CARTESIAN_POINT ( 'NONE',  ( -1.332267629550188046E-16, 4.000000000000003553, 2.400000000000007461 ) ) ;
#188253 = CARTESIAN_POINT ( 'NONE',  ( -10.99999999999731237, 3.761581922631320025E-34, -0.4330127018938148553 ) ) ;
#188254 = TOROIDAL_SURFACE ( 'NONE', #177763, 2.149999999999999911, 0.1000000000000000056 ) ;
#188255 = CARTESIAN_POINT ( 'NONE',  ( 1.358040219746913024, 0.7549631825471068147, 1.711723683848711985 ) ) ;
#188256 = CARTESIAN_POINT ( 'NONE',  ( 2.413296319342159713, -1.879803466158457059, 0.7303082167480907660 ) ) ;
#188258 = CARTESIAN_POINT ( 'NONE',  ( 11.48243876534946217, 13.79999999999998295, 3.199999999999997957 ) ) ;
#188257 = CARTESIAN_POINT ( 'NONE',  ( 1.364683531249986537, 0.3635416670080869328, 0.7879004041258500513 ) ) ;
#188260 = CARTESIAN_POINT ( 'NONE',  ( 5.461587592249073531, 0.4120570304669196604, -2.065184316587692415 ) ) ;
#188259 = CARTESIAN_POINT ( 'NONE',  ( -9.691380875670077444, 10.20103253123691189, 0.7998128361456462443 ) ) ;
#188261 = CIRCLE ( 'NONE', #181451, 2.650000000000008349 ) ;
#188262 = CARTESIAN_POINT ( 'NONE',  ( 8.457588896826466751, 8.761608555919362828, 1.040834085586084257E-14 ) ) ;
#188264 = CARTESIAN_POINT ( 'NONE',  ( -8.688077508258798431, 9.030511935923748013, -0.7998128361456291469 ) ) ;
#188263 = CARTESIAN_POINT ( 'NONE',  ( 4.549643065837591038, 7.465611455855944101, -1.199719254218452047 ) ) ;
#188265 = SURFACE_STYLE_USAGE ( .BOTH. , #122307 ) ;
#188266 = CARTESIAN_POINT ( 'NONE',  ( 4.605726162909654420, 1.499404818428259345, 1.353488595782571524 ) ) ;
#188267 = CARTESIAN_POINT ( 'NONE',  ( -1.001543065824772872E-14, 4.821875000341419693, 1.575800808251672791 ) ) ;
#188268 = CARTESIAN_POINT ( 'NONE',  ( 6.320769014966518107, -1.461346085113580440, 1.455966316998691168 ) ) ;
#188269 = CARTESIAN_POINT ( 'NONE',  ( 9.571693261567961741, 11.22969222899322617, 1.082531754730548412 ) ) ;
#188270 = CARTESIAN_POINT ( 'NONE',  ( 4.798204600472657511, -2.160985683756014630, -0.05834674948757002932 ) ) ;
#188271 = CARTESIAN_POINT ( 'NONE',  ( 7.038618024149998043, 8.240751112043669835, -1.199719254218452047 ) ) ;
#188272 = CARTESIAN_POINT ( 'NONE',  ( 0.6823417656249882723, -0.01145833299191073573, -1.181850606188749264 ) ) ;
#188274 = CARTESIAN_POINT ( 'NONE',  ( -9.496893780459334522, -9.200036371099116650, 0.2463816395386524416 ) ) ;
#188273 = CARTESIAN_POINT ( 'NONE',  ( 5.397027666691686321, 8.454226823519094935, 1.199719254218451159 ) ) ;
#188275 = CARTESIAN_POINT ( 'NONE',  ( 6.277061933002769045, 10.26706332190449622, 0.7216878364870438212 ) ) ;
#188277 = CARTESIAN_POINT ( 'NONE',  ( -0.08202876420372198774, -7.861065518611666469, 10.99977341864973468 ) ) ;
#188276 = CARTESIAN_POINT ( 'NONE',  ( 1.662788154211870983, -0.7805772603099859763, -2.026187018951190133 ) ) ;
#188279 = CARTESIAN_POINT ( 'NONE',  ( 1.751249726499287673, 1.836263021919124050, -0.1365115386888632321 ) ) ;
#188278 = CARTESIAN_POINT ( 'NONE',  ( -6.073689629242176480, 6.188318776978391611, -0.7216878364870278340 ) ) ;
#188280 = CARTESIAN_POINT ( 'NONE',  ( -1.201851678989727383E-14, 2.821875000341418804, 1.575800808251672791 ) ) ;
#188281 = CARTESIAN_POINT ( 'NONE',  ( 3.755584314896889264, 2.174856280799509545, -0.2696606696684644700 ) ) ;
#188282 = DIRECTION ( 'NONE',  ( 0.000000000000000000, 0.000000000000000000, -1.000000000000000000 ) ) ;
#188283 = CARTESIAN_POINT ( 'NONE',  ( 3.573342120354418672, 0.05797898436993471211, -2.261936065680466346 ) ) ;
#188284 = CARTESIAN_POINT ( 'NONE',  ( -5.181187258716735577, 9.196468901811520880, 0.7998128361456481317 ) ) ;
#188285 = CARTESIAN_POINT ( 'NONE',  ( -1.806654366501805775, 9.001999999999998892, 2.420000000000000373 ) ) ;
#188286 = CARTESIAN_POINT ( 'NONE',  ( 6.011645680221167076, 7.072102904328817274, -1.053258377668888857 ) ) ;
#188287 = CARTESIAN_POINT ( 'NONE',  ( -0.7500000000000006661, 13.95833333333333570, -1.299038105676657340 ) ) ;
#188288 = CARTESIAN_POINT ( 'NONE',  ( 5.641601317062233001, 7.675230518029648508, -1.443375672974078761 ) ) ;
#188289 = CARTESIAN_POINT ( 'NONE',  ( 5.395664931544272847, -0.6364340197690997458, 1.651504472441939875 ) ) ;
#188290 = CARTESIAN_POINT ( 'NONE',  ( 3.422524054001755633, -0.8179560535927836717, -1.839607883820688405 ) ) ;
#188291 = CARTESIAN_POINT ( 'NONE',  ( 9.271078113646423091, 9.710679308875986848, 1.040834085586084257E-14 ) ) ;
#188292 = CARTESIAN_POINT ( 'NONE',  ( 1.694499644457616583, -2.095784359944006248, -0.2068371402374687973 ) ) ;
#188294 = CARTESIAN_POINT ( 'NONE',  ( -1.500000000000001332, 0.6500000000000255573, 0.000000000000000000 ) ) ;
#188293 = CARTESIAN_POINT ( 'NONE',  ( 1.364683531249996529, 11.21354166700806232, 0.7879004041258405033 ) ) ;
#188295 = CARTESIAN_POINT ( 'NONE',  ( 0.9769314595147912117, 1.818477718279483568, 0.7569839642056105378 ) ) ;
#188296 = CARTESIAN_POINT ( 'NONE',  ( -5.320648938720212051, 5.172121614787156929, 0.000000000000000000 ) ) ;
#188297 = CARTESIAN_POINT ( 'NONE',  ( 3.686041076052345211, 7.355199913248151589, -0.03413285989870468856 ) ) ;
#188299 = ORIENTED_EDGE ( 'NONE', *, *, #52780, .F. ) ;
#188298 = CARTESIAN_POINT ( 'NONE',  ( 5.414259967653319627, -1.811767230315189048, 0.008324397547932599339 ) ) ;
#188300 = CARTESIAN_POINT ( 'NONE',  ( 5.992340707560147806, 8.974519344586754599, 1.082531754730558626 ) ) ;
#188301 = CARTESIAN_POINT ( 'NONE',  ( 5.366025703835962446, 0.9229158262306772498, 1.627043297953718382 ) ) ;
#188302 = ORIENTED_EDGE ( 'NONE', *, *, #136490, .F. ) ;
#188303 = CARTESIAN_POINT ( 'NONE',  ( 4.381733404717279790, -1.982624999272283084, 0.5960583376443122638 ) ) ;
#188304 = CARTESIAN_POINT ( 'NONE',  ( 1.224999999999986988, 1.645833333333327930, -0.7072540797572998139 ) ) ;
#188305 = SHAPE_REPRESENTATION ( 'drip tip', ( #200407 ), #152191 ) ;
#188306 = CARTESIAN_POINT ( 'NONE',  ( -3.946832114909637479, 7.618738210787614484, 0.7216878364870338292 ) ) ;
#188307 = CARTESIAN_POINT ( 'NONE',  ( 3.251336881620926267, -0.9471318103815578038, 0.9360613127407988454 ) ) ;
#188308 = CARTESIAN_POINT ( 'NONE',  ( 8.209625708274705502, 9.536650400197368427, 1.199719254218462483 ) ) ;
#188309 = CARTESIAN_POINT ( 'NONE',  ( -9.677822722056413696, 10.18521468535430685, 1.040834085586084257E-14 ) ) ;
#188310 = CARTESIAN_POINT ( 'NONE',  ( 9.452953479610789245, 4.518459255872631530, 7.393264888175490768 ) ) ;
#188311 = DIRECTION ( 'NONE',  ( -1.000000000000000000, 8.673617379884035472E-16, 0.000000000000000000 ) ) ;
#188312 = CARTESIAN_POINT ( 'NONE',  ( 1.364683531249986537, -0.3864583329919166199, 0.7879004041258500513 ) ) ;
#188314 = CIRCLE ( 'NONE', #29241, 6.200000000000000178 ) ;
#188313 = CARTESIAN_POINT ( 'NONE',  ( -0.7500000000000215383, 1.191666666666688190, 1.299038105676659116 ) ) ;
#188316 = CARTESIAN_POINT ( 'NONE',  ( 4.286349120214771879, 8.152491073559232859, -0.7998128361456221525 ) ) ;
#188315 = CARTESIAN_POINT ( 'NONE',  ( 4.703538834289092030, -1.515240342570793430, -1.246145567450624991 ) ) ;
#188317 = CARTESIAN_POINT ( 'NONE',  ( 1.651720012567552853, -0.2930234437087535504, -1.994564656426714988 ) ) ;
#188318 = LINE ( 'NONE', #154772, #121119 ) ;
#188319 = CARTESIAN_POINT ( 'NONE',  ( 0.4861908890553789386, -2.175720422541329580, -0.2624175912114696252 ) ) ;
#188320 = CARTESIAN_POINT ( 'NONE',  ( 0.000000000000000000, 3.499999999999989342, 0.000000000000000000 ) ) ;
#188321 = CARTESIAN_POINT ( 'NONE',  ( 1.756895065592100291, -1.601674646019658255, -0.9660157589584242865 ) ) ;
#188322 = CARTESIAN_POINT ( 'NONE',  ( 0.6823417656249917140, 4.592708333674755394, 1.181850606188765695 ) ) ;
#188323 = CARTESIAN_POINT ( 'NONE',  ( 3.726818050638240898, 1.420666359685630598, -1.426677609031762994 ) ) ;
#188324 = CARTESIAN_POINT ( 'NONE',  ( -7.160677686311960777, 11.50587440067263678, -0.7998128361456291469 ) ) ;
#188326 = CARTESIAN_POINT ( 'NONE',  ( 3.532911237611217281, -1.729578172696862426, 1.220892919093808482 ) ) ;
#188325 = CARTESIAN_POINT ( 'NONE',  ( -3.958617665510266725, 7.562211676496538360, -0.7216878364870267237 ) ) ;
#188328 = EDGE_CURVE ( 'NONE', #197566, #114098, #167704, .T. ) ;
#188327 = CARTESIAN_POINT ( 'NONE',  ( 0.000000000000000000, 0.5000000000000004441, 0.000000000000000000 ) ) ;
#188329 = CARTESIAN_POINT ( 'NONE',  ( 4.598136200040512378, 0.8882050449813773119, -1.870312673664726644 ) ) ;
#188330 = CARTESIAN_POINT ( 'NONE',  ( 5.559725510055676168, 8.644040974110419384, 1.199719254218451159 ) ) ;
#188332 = CARTESIAN_POINT ( 'NONE',  ( 6.720655732516641834, 7.051887106169240305, 2.771889904330120391 ) ) ;
#188331 = CARTESIAN_POINT ( 'NONE',  ( 1.277023361749257457, 1.930420895987930097, -0.8034254789068133729 ) ) ;
#188334 = ORIENTED_EDGE ( 'NONE', *, *, #1599, .T. ) ;
#188333 = CARTESIAN_POINT ( 'NONE',  ( 6.071303273277399271, 0.1315155018670917386, -1.820917815106848359 ) ) ;
#188335 = CARTESIAN_POINT ( 'NONE',  ( 8.776205506747620788, 9.133327934160710981, -0.7998128361456221525 ) ) ;
#188336 = CARTESIAN_POINT ( 'NONE',  ( -6.071028223004627300, 5.977287769793835359, -0.4191162096944526239 ) ) ;
#188337 = CARTESIAN_POINT ( 'NONE',  ( 0.000000000000000000, 0.06698729810653621108, 0.000000000000000000 ) ) ;
#188338 = CARTESIAN_POINT ( 'NONE',  ( -10.39851513827935747, 3.504673854002353206, 5.419231829292963099 ) ) ;
#188339 = CARTESIAN_POINT ( 'NONE',  ( 6.765155463094746580, 9.876136559377135526, 1.082531754730558626 ) ) ;
#188340 = DIRECTION ( 'NONE',  ( 1.000000000000000000, -0.000000000000000000, -0.000000000000000000 ) ) ;
#188341 = CARTESIAN_POINT ( 'NONE',  ( 5.848291733227988232, 0.9385554955868085081, -1.666026892748099009 ) ) ;
#188342 = CARTESIAN_POINT ( 'NONE',  ( -6.997979842947967377, 11.31606025008131233, -0.7998128361456291469 ) ) ;
#188343 = CARTESIAN_POINT ( 'NONE',  ( 6.518772930072240790, 6.499656594706071822, -0.7998128361456281477 ) ) ;
#188344 = CARTESIAN_POINT ( 'NONE',  ( -6.953912913643675253, -8.144978210217285408, 6.511381374296902891 ) ) ;
#188345 = CARTESIAN_POINT ( 'NONE',  ( -0.4019237886466871523, 12.22991455036742892, -1.499999999999998668 ) ) ;
#188346 = CARTESIAN_POINT ( 'NONE',  ( 4.871457266011829823, 4.577788319968905562, -0.7998128361456221525 ) ) ;
#188347 = ORIENTED_EDGE ( 'NONE', *, *, #66268, .F. ) ;
#188348 = CARTESIAN_POINT ( 'NONE',  ( 6.327749939939702806, 0.7691082200134463642, -1.864175038933603146 ) ) ;
#188349 = CARTESIAN_POINT ( 'NONE',  ( -4.100072327556957497, 7.608104560092542101, -0.6936436459203108029 ) ) ;
#188350 = CARTESIAN_POINT ( 'NONE',  ( 1.873515663034563961, 3.299988112486734071, -0.3999999999999993006 ) ) ;
#188351 = CARTESIAN_POINT ( 'NONE',  ( 0.1394461523057137220, 5.725876337386284654, -2.313825101289856967 ) ) ;
#188352 = EDGE_CURVE ( 'NONE', #193389, #72609, #160908, .T. ) ;
#188353 = CARTESIAN_POINT ( 'NONE',  ( -4.934804725694224459, 6.780358151441803649, -1.443375672974053447 ) ) ;
#188354 = CARTESIAN_POINT ( 'NONE',  ( 3.358669367883368118, 4.941533567329135401, -1.599625672291262513 ) ) ;
#188355 = CARTESIAN_POINT ( 'NONE',  ( 3.379706166375577414, -1.899257087701329949, 0.5209217831910922802 ) ) ;
#188356 = CARTESIAN_POINT ( 'NONE',  ( 4.025017672583341977, -1.753021876717888006, 0.9963191169995513352 ) ) ;
#188357 = CARTESIAN_POINT ( 'NONE',  ( -5.194745412330402878, 9.212286747694129474, 0.000000000000000000 ) ) ;
#188358 = CARTESIAN_POINT ( 'NONE',  ( -1.115562610750309283E-14, 10.31250000000000000, 1.500000000000001554 ) ) ;
#188359 = CARTESIAN_POINT ( 'NONE',  ( 5.156268285673103691, -1.588865937562380148, 1.509524371192130676 ) ) ;
#188360 = CARTESIAN_POINT ( 'NONE',  ( 1.237941840314000785, 1.374772708486753370, 1.500000000000001332 ) ) ;
#188361 = CARTESIAN_POINT ( 'NONE',  ( 2.678635733147361808, -1.842946530311468045, -0.5607992601908852182 ) ) ;
#188362 = CARTESIAN_POINT ( 'NONE',  ( -8.646349277213090545, 11.11049346154719508, 1.599625672291269396 ) ) ;
#188363 = CARTESIAN_POINT ( 'NONE',  ( -0.1298852118744101003, 4.098067735550426249, -2.281510303361510061 ) ) ;
#188364 = CARTESIAN_POINT ( 'NONE',  ( 0.1331565106231363538, 0.2470099659030860484, -1.980838409567912572 ) ) ;
#188365 = CARTESIAN_POINT ( 'NONE',  ( 1.364683531250000748, 13.00520833367473550, -0.7879004041258355073 ) ) ;
#188366 = CARTESIAN_POINT ( 'NONE',  ( 5.834086172582112262, 5.700855377634248100, 1.040834085586084257E-14 ) ) ;
#188367 = CARTESIAN_POINT ( 'NONE',  ( -4.952636518945700672, 6.537114055553894687, -2.442608363190702292 ) ) ;
#188368 = CARTESIAN_POINT ( 'NONE',  ( 3.906157654512984134, 7.571284673658201569, -0.7216878364870338292 ) ) ;
#188369 = VERTEX_POINT ( 'NONE', #99407 ) ;
#188370 = VERTEX_POINT ( 'NONE', #789 ) ;
#188372 = CARTESIAN_POINT ( 'NONE',  ( 3.035794076406534536, -1.939542403429166395, 0.5389024948808174287 ) ) ;
#188371 = CARTESIAN_POINT ( 'NONE',  ( 6.374545129912787544, -0.09763137639631430664, -1.838803627010993313 ) ) ;
#188373 = CARTESIAN_POINT ( 'NONE',  ( 5.817770776407988009, -1.817369610395104695, 1.406990027747441419 ) ) ;
#188375 = CARTESIAN_POINT ( 'NONE',  ( 3.063170293922971243, 1.569483505267080359, 0.9996245905467721071 ) ) ;
#188374 = CARTESIAN_POINT ( 'NONE',  ( 0.4170821662628897974, 3.033599471985628959, -0.4170821662629418114 ) ) ;
#188376 = CARTESIAN_POINT ( 'NONE',  ( -3.285556943749998737, -0.7802083328553744979, 1.896917185911908499 ) ) ;
#188377 = CARTESIAN_POINT ( 'NONE',  ( 0.000000000000000000, 4.446947634372835800, 0.000000000000000000 ) ) ;
#188378 =( NAMED_UNIT ( * ) PLANE_ANGLE_UNIT ( ) SI_UNIT ( $, .RADIAN. ) );
#188379 = CARTESIAN_POINT ( 'NONE',  ( -5.693534442735004752, 8.729875052244421951, 1.199719254218452047 ) ) ;
#188380 = CARTESIAN_POINT ( 'NONE',  ( -5.207740401424942434, 6.208690235484773723, 1.082531754730549078 ) ) ;
#188381 = CARTESIAN_POINT ( 'NONE',  ( 6.040588761503070003, -1.765850204961866954, 1.119074740713212002 ) ) ;
#188382 = CARTESIAN_POINT ( 'NONE',  ( 4.351804120306567825, 8.020929207092235558, 1.040834085586084257E-14 ) ) ;
#188383 = VERTEX_POINT ( 'NONE', #163345 ) ;
#188384 = FACE_OUTER_BOUND ( 'NONE', #141246, .T. ) ;
#188385 = CARTESIAN_POINT ( 'NONE',  ( 0.09999999999999592548, -9.919999999999998153, 10.91954211494236660 ) ) ;
#188386 = CARTESIAN_POINT ( 'NONE',  ( 0.3635304476994546952, 1.806310985241452949, -0.2645042207462811046 ) ) ;
#188387 = CARTESIAN_POINT ( 'NONE',  ( -5.545448523189368650, 6.428443684264421698, -1.199719254218446718 ) ) ;
#188388 =( BOUNDED_SURFACE ( )  B_SPLINE_SURFACE ( 1, 2, ( 
 ( #36582, #5126, #71201, #187101, #38735, #104817, #70134, #170862, #202266, #208408, #174889, #60042, #120054, #22453, #186028, #136246, #108863, #72272, #88565, #92578, #37665, #138381, #204399, #158620, #168727, #10217, #76291, #126195, #192158, #43820, #109936, #61111, #175945, #27541, #159678, #143472, #31825, #180203, #161830, #44890, #178073, #29691, #47018, #95774, #112072, #13418, #162890, #148764, #110996, #145612, #12343, #177001, #32878, #213725, #196450, #65348, #28617, #129405, #131495, #211608, #128345, #79493, #96842, #195386, #333, #193243, #144545, #113133, #15538, #45952, #63244, #98955, #66406, #97901, #48093, #114205, #130460, #194311, #81622, #94706, #115258, #160747, #179140, #78423, #165006, #30763, #14473, #80562, #163960, #147706, #210552, #82681, #146661, #16600, #197499, #62188, #49142, #212674, #64315, #181251, #199621, #104287, #53388, #50198, #167152, #86961, #18739, #119524, #117391, #169276, #183387, #170335, #120609, #4603, #1411, #69615, #154100, #34993, #116317, #51267, #101065, #102144, #84823, #182308, #88028, #150911, #5669, #2473, #21919, #68550, #132551, #20862, #198550, #38214, #134677, #33937, #200680, #135724, #100011, #151971, #185511, #133619, #70678, #166076, #52329, #83749, #67471, #118459, #202816, #19810, #184445, #36063, #17664, #201747, #149841, #168211, #3544, #153030, #136788, #85896, #37134, #103216, #54465, #186586, #89115, #8901, #58729, #206032, #137864, #204953, #90183, #39276, #109688, #159424, #27282, #93388, #56601, #125950, #26216, #73916, #174639, #156246, #191906, #42506, #55528, #71748, #122765, #24078, #189787, #105371, #7824, #57667, #173580, #158375, #6753, #172491, #74982, #141090, #188724, #43569, #41437, #91251, #203884, #157311, #72829, #121683, #187650, #140009, #171408, #175691, #22998, #155170, #138932, #107546, #123825, #59793, #40362, #25150, #106465, #124880, #108612, #207101, #190844, #92333, #9968, #76045, #142147, #208161, #14211, #195129, #31570, #15285, #131255, #146406, #79242, #98695, #194048, #78169, #61932, #45700, #128090, #209216, #177820, #176745, #179947, #212418, #113951, #28359, #111818, #160493, #127019, #162637, #46767, #29436, #64060, #12100, #95527, #144298, #94455, #11024, #161577, #47840, #210291, #13164, #130203, #97645, #32617, #145360, #211360, #65098, #112879, #196197, #163704, #62985, #77101, #129154, #178893, #30507, #96588, #80306, #81371, #147452, #180998, #143226, #213475, #44631, #60857, #197242, #48881, #114999, #192978, #110747, #100808, #185247, #183130, #99752, #133354, #68290, #166894, #186319, #164753, #116058, #18486, #201486, #17405, #67218, #70417, #37954, #52072, #84562, #118199, #150652, #132290, #49937, #136533, #165822, #184186, #182048, #198296, #36870, #33678, #83489, #1156, #149572, #2214, #4348, #199360, #53131, #152767, #202553, #16343, #120343, #82424, #51007, #54204, #119261, #134423, #102953, #34736, #148513, #135464, #80, #66145, #117128, #200426, #35808, #101885, #167950, #19553, #85630, #169012, #151717, #3287, #69354, #20610, #86698, #75784, #7561, #157051, #107282, #24883, #41174, #39022, #140823, #5412, #25953, #59523, #171144, #71491, #158116, #89923, #56338, #155974, #74719, #58469, #125683, #207900, #88853, #141891, #108352, #191641, #90988, #55271, #57399, #154909, #22736, #104026, #8639, #21660, #138666, #124623, #204688, #206836, #6493, #190581, #72568, #170074, #92059, #42239, #187390, #173303, #87766, #122499, #153842, #188460, #40091, #73647, #106203, #137603, #203620, #172229, #121418, #23818, #105105, #139746, #205770, #174374, #123564, #9708, #189527, #147198, #144028, #194860, #109425, #62717, #96323, #44364, #129950, #15022, #94192, #208958, #126749, #160232, #113689, #145090, #95258, #111548, #27016, #112615, #81113, #210023, #128879, #146143, #47574, #110487, #11831, #176486, #45433, #127833, #60591, #46493, #30239, #177557, #175430, #28096, #61665, #10762, #77908, #211094, #192708, #76836, #195938, #193785, #142956, #29168, #161308, #12891, #97385, #78970, #80039, #31308, #178627, #213224, #162378, #13956, #43305, #93124, #212157, #131001, #163442, #64854 ),
 ( #63793, #179691, #159163, #200176, #166633, #3035, #201238, #102705, #117947, #50744, #70171, #165561, #49679, #33427, #17155, #99504, #180743, #149315, #148261, #151462, #183940, #85380, #214261, #83230, #132039, #98435, #134166, #18227, #894, #35552, #198050, #66961, #115806, #65894, #196993, #133101, #19298, #181793, #199098, #101632, #69104, #4101, #116871, #182872, #36619, #84310, #167698, #135226, #34488, #48628, #100562, #150396, #1964, #68028, #51829, #52879, #119015, #152517, #114744, #184996, #16084, #32369, #168762, #20368, #86452, #164499, #82167, #22489, #57153, #104852, #153592, #121173, #138417, #88600, #140579, #136282, #21418, #154657, #205519, #137355, #187142, #156803, #206590, #122247, #6241, #188206, #72312, #103780, #169831, #8390, #155725, #204437, #202303, #203370, #56090, #87527, #74472, #53954, #120092, #186067, #38770, #37704, #5164, #23565, #71238, #89675, #55024, #170897, #7309, #39844, #173053, #105950, #171974, #189281, #73385, #139491, #123318, #40920, #107027, #24633, #90740, #52506, #34121, #87139, #18919, #168393, #118639, #36241, #184624, #50380, #152149, #16787, #37319, #70858, #182492, #82870, #169455, #101250, #67652, #167333, #86074, #69794, #136972, #4780, #100192, #153210, #119707, #203000, #102319, #66587, #68732, #166258, #17847, #115446, #19989, #33066, #150021, #135903, #1591, #3718, #83932, #201921, #133798, #181437, #103394, #53574, #198734, #185690, #99144, #199807, #165193, #51452, #117572, #85003, #183567, #148948, #519, #35173, #132730, #151095, #116502, #2658, #134853, #21041, #200859, #174825, #105552, #158551, #155346, #206213, #120788, #74100, #107732, #55704, #141277, #26401, #171586, #5858, #138040, #23180, #125068, #156423, #106646, #122944, #38390, #124002, #92513, #6929, #140192, #157497, #58913, #121859, #89295, #187830, #56778, #139107, #71929, #57840, #73007, #104471, #10148, #205135, #76223, #188900, #142333, #39456, #54639, #91436, #186765, #170518, #40543, #22100, #172674, #189970, #88213, #41619, #173758, #24251, #207286, #154284, #90354, #204053, #8009, #25335, #191026, #9091, #75168, #42693, #108798, #13011, #79088, #78025, #45552, #110603, #160350, #145206, #158232, #55641, #177675, #93243, #176604, #28216, #92182, #186699, #105490, #174493, #191764, #26070, #39395, #9823, #159277, #211212, #38328, #75899, #154216, #104404, #29285, #144149, #126870, #210141, #170453, #59644, #61785, #142003, #121797, #208018, #27137, #125802, #120726, #22038, #71865, #43420, #11952, #187765, #109544, #95379, #88149, #10876, #175548, #76951, #143076, #127951, #5788, #111668, #137974, #209069, #203993, #161428, #60706, #192828, #44486, #94309, #193904, #18339, #166745, #47688, #100667, #67070, #34599, #198155, #14067, #16194, #113800, #130063, #84420, #49788, #194976, #97497, #17262, #163554, #115914, #179802, #99607, #31421, #150509, #50857, #149423, #146259, #214369, #62837, #15137, #46612, #196056, #81225, #32473, #147307, #48738, #33535, #83338, #128999, #112734, #213333, #178744, #133206, #30357, #181900, #80154, #82275, #64958, #131110, #96444, #165673, #162495, #197097, #1006, #114851, #199210, #180851, #116982, #98545, #212272, #182982, #63907, #164609, #65999, #148370, #132149, #200282, #69208, #135328, #186172, #36724, #51933, #172080, #52982, #23673, #119118, #39951, #201342, #89783, #38874, #106058, #122352, #185097, #2070, #102810, #153696, #68141, #21513, #55127, #3138, #88705, #188309, #168866, #167807, #85485, #20469, #72418, #103881, #54061, #70274, #118057, #134274, #86555, #187247, #19406, #104959, #6346, #152619, #4206, #136390, #202406, #120196, #151571, #5265, #203473, #37806, #184042, #169929, #87625, #35659, #101738, #71342, #137458, #121272, #171000, #56191, #22598, #154763, #138519, #204543, #209876, #126602, #139597, #111404, #206695, #108211, #59384, #123422, #174234, #75643, #43167, #27952, #90842, #42096, #92978, #159024, #74576, #127680, #125539, #155830, #9566, #25808, #156905, #8494, #192564, #57260, #77761, #177406, #140679, #189384, #61515, #141750, #124479, #7414, #58323, #190436, #207757, #91917, #157977, #191501 ) ),
 .UNSPECIFIED., .F., .F., .F. ) 
 B_SPLINE_SURFACE_WITH_KNOTS ( ( 2, 2 ),
 ( 3, 2, 2, 2, 2, 2, 2, 2, 2, 2, 2, 2, 2, 2, 2, 2, 2, 2, 2, 2, 2, 2, 2, 2, 2, 2, 2, 2, 2, 2, 2, 2, 2, 2, 2, 2, 2, 2, 2, 2, 2, 2, 2, 2, 2, 2, 2, 2, 2, 2, 2, 2, 2, 2, 2, 2, 2, 2, 2, 2, 2, 2, 2, 2, 2, 2, 2, 2, 2, 2, 2, 2, 2, 2, 2, 2, 2, 2, 2, 2, 2, 2, 2, 2, 2, 2, 2, 2, 2, 2, 2, 2, 2, 2, 2, 2, 2, 2, 2, 2, 2, 2, 2, 2, 2, 2, 2, 2, 2, 2, 2, 2, 2, 2, 2, 2, 2, 2, 2, 2, 2, 2, 2, 2, 2, 2, 2, 2, 2, 2, 2, 2, 2, 2, 2, 2, 2, 2, 2, 2, 2, 2, 2, 2, 2, 2, 2, 2, 2, 2, 2, 2, 2, 2, 2, 2, 2, 2, 2, 2, 2, 2, 2, 2, 2, 2, 2, 2, 2, 2, 2, 2, 2, 2, 2, 2, 2, 2, 2, 2, 2, 2, 2, 2, 2, 2, 2, 2, 2, 2, 2, 2, 2, 2, 2, 2, 2, 2, 2, 2, 2, 2, 2, 2, 2, 2, 2, 2, 2, 2, 2, 2, 2, 2, 2, 2, 2, 2, 2, 2, 2, 2, 2, 2, 2, 2, 2, 2, 2, 2, 2, 2, 2, 2, 2, 2, 2, 2, 2, 2, 3 ),
 ( 0.000000000000000000, 1.000000000000000000 ),
 ( 0.000000000000000000, 0.004166666666666666609, 0.008333333333333333218, 0.01250000000000000069, 0.01666666666666666644, 0.02083333333333333218, 0.02500000000000000139, 0.02916666666666666713, 0.03333333333333333287, 0.03749999999999999861, 0.04166666666666666435, 0.04583333333333333010, 0.05000000000000000278, 0.05416666666666666852, 0.05833333333333333426, 0.06250000000000000000, 0.06666666666666666574, 0.07083333333333333148, 0.07499999999999999722, 0.07916666666666666297, 0.08333333333333332871, 0.08749999999999999445, 0.09166666666666666019, 0.09583333333333333981, 0.1000000000000000056, 0.1041666666666666713, 0.1083333333333333370, 0.1125000000000000028, 0.1166666666666666685, 0.1208333333333333343, 0.1250000000000000000, 0.1291666666666666796, 0.1333333333333333315, 0.1375000000000000111, 0.1416666666666666630, 0.1458333333333333426, 0.1499999999999999944, 0.1541666666666666741, 0.1583333333333333259, 0.1625000000000000056, 0.1666666666666666574, 0.1708333333333333370, 0.1749999999999999889, 0.1791666666666666685, 0.1833333333333333204, 0.1875000000000000000, 0.1916666666666666796, 0.1958333333333333315, 0.2000000000000000111, 0.2041666666666666630, 0.2083333333333333426, 0.2124999999999999944, 0.2166666666666666741, 0.2208333333333333259, 0.2250000000000000056, 0.2291666666666666574, 0.2333333333333333370, 0.2374999999999999889, 0.2416666666666666685, 0.2458333333333333204, 0.2500000000000000000, 0.2541666666666666519, 0.2583333333333333592, 0.2625000000000000111, 0.2666666666666666630, 0.2708333333333333148, 0.2750000000000000222, 0.2791666666666666741, 0.2833333333333333259, 0.2874999999999999778, 0.2916666666666666852, 0.2958333333333333370, 0.2999999999999999889, 0.3041666666666666408, 0.3083333333333333481, 0.3125000000000000000, 0.3166666666666666519, 0.3208333333333333592, 0.3250000000000000111, 0.3291666666666666630, 0.3333333333333333148, 0.3375000000000000222, 0.3416666666666666741, 0.3458333333333333259, 0.3499999999999999778, 0.3541666666666666852, 0.3583333333333333370, 0.3624999999999999889, 0.3666666666666666408, 0.3708333333333333481, 0.3750000000000000000, 0.3791666666666666519, 0.3833333333333333592, 0.3875000000000000111, 0.3916666666666666630, 0.3958333333333333148, 0.4000000000000000222, 0.4041666666666666741, 0.4083333333333333259, 0.4124999999999999778, 0.4166666666666666852, 0.4208333333333333370, 0.4249999999999999889, 0.4291666666666666408, 0.4333333333333333481, 0.4375000000000000000, 0.4416666666666666519, 0.4458333333333333592, 0.4500000000000000111, 0.4541666666666666630, 0.4583333333333333148, 0.4625000000000000222, 0.4666666666666666741, 0.4708333333333333259, 0.4749999999999999778, 0.4791666666666666852, 0.4833333333333333370, 0.4874999999999999889, 0.4916666666666666408, 0.4958333333333333481, 0.5000000000000000000, 0.5041666666666666519, 0.5083333333333333037, 0.5124999999999999556, 0.5166666666666667185, 0.5208333333333333703, 0.5250000000000000222, 0.5291666666666666741, 0.5333333333333333259, 0.5374999999999999778, 0.5416666666666666297, 0.5458333333333332815, 0.5500000000000000444, 0.5541666666666666963, 0.5583333333333333481, 0.5625000000000000000, 0.5666666666666666519, 0.5708333333333333037, 0.5749999999999999556, 0.5791666666666667185, 0.5833333333333333703, 0.5875000000000000222, 0.5916666666666666741, 0.5958333333333333259, 0.5999999999999999778, 0.6041666666666666297, 0.6083333333333332815, 0.6125000000000000444, 0.6166666666666666963, 0.6208333333333333481, 0.6250000000000000000, 0.6291666666666666519, 0.6333333333333333037, 0.6374999999999999556, 0.6416666666666667185, 0.6458333333333333703, 0.6500000000000000222, 0.6541666666666666741, 0.6583333333333333259, 0.6624999999999999778, 0.6666666666666666297, 0.6708333333333332815, 0.6750000000000000444, 0.6791666666666666963, 0.6833333333333333481, 0.6875000000000000000, 0.6916666666666666519, 0.6958333333333333037, 0.6999999999999999556, 0.7041666666666667185, 0.7083333333333333703, 0.7125000000000000222, 0.7166666666666666741, 0.7208333333333333259, 0.7249999999999999778, 0.7291666666666666297, 0.7333333333333332815, 0.7375000000000000444, 0.7416666666666666963, 0.7458333333333333481, 0.7500000000000000000, 0.7541666666666666519, 0.7583333333333333037, 0.7624999999999999556, 0.7666666666666667185, 0.7708333333333333703, 0.7750000000000000222, 0.7791666666666666741, 0.7833333333333333259, 0.7874999999999999778, 0.7916666666666666297, 0.7958333333333332815, 0.8000000000000000444, 0.8041666666666666963, 0.8083333333333333481, 0.8125000000000000000, 0.8166666666666666519, 0.8208333333333333037, 0.8249999999999999556, 0.8291666666666667185, 0.8333333333333333703, 0.8375000000000000222, 0.8416666666666666741, 0.8458333333333333259, 0.8499999999999999778, 0.8541666666666666297, 0.8583333333333332815, 0.8625000000000000444, 0.8666666666666666963, 0.8708333333333333481, 0.8750000000000000000, 0.8791666666666666519, 0.8833333333333333037, 0.8874999999999999556, 0.8916666666666667185, 0.8958333333333333703, 0.9000000000000000222, 0.9041666666666666741, 0.9083333333333333259, 0.9124999999999999778, 0.9166666666666666297, 0.9208333333333332815, 0.9250000000000000444, 0.9291666666666666963, 0.9333333333333333481, 0.9375000000000000000, 0.9416666666666666519, 0.9458333333333333037, 0.9499999999999999556, 0.9541666666666667185, 0.9583333333333333703, 0.9625000000000000222, 0.9666666666666666741, 0.9708333333333333259, 0.9749999999999999778, 0.9791666666666666297, 0.9833333333333332815, 0.9875000000000000444, 0.9916666666666666963, 0.9958333333333333481, 1.000000000000000000 ),
 .UNSPECIFIED. ) 
 GEOMETRIC_REPRESENTATION_ITEM ( )  RATIONAL_B_SPLINE_SURFACE ( (
 ( 1.000000000000000000, 0.8660254037844387076, 1.000000000000000000, 0.8660254037844387076, 1.000000000000000000, 0.8660254037844387076, 1.000000000000000000, 0.8660254037844387076, 1.000000000000000000, 0.8660254037844387076, 1.000000000000000000, 0.8660254037844387076, 1.000000000000000000, 0.8660254037844387076, 1.000000000000000000, 0.8660254037844387076, 1.000000000000000000, 0.8660254037844387076, 1.000000000000000000, 0.8660254037844387076, 1.000000000000000000, 0.8660254037844387076, 1.000000000000000000, 0.8660254037844387076, 1.000000000000000000, 0.8660254037844387076, 1.000000000000000000, 0.8660254037844387076, 1.000000000000000000, 0.8660254037844387076, 1.000000000000000000, 0.8660254037844387076, 1.000000000000000000, 0.8660254037844387076, 1.000000000000000000, 0.8660254037844387076, 1.000000000000000000, 0.8660254037844387076, 1.000000000000000000, 0.8660254037844387076, 1.000000000000000000, 0.8660254037844387076, 1.000000000000000000, 0.8660254037844387076, 1.000000000000000000, 0.8660254037844387076, 1.000000000000000000, 0.8660254037844387076, 1.000000000000000000, 0.8660254037844387076, 1.000000000000000000, 0.8660254037844387076, 1.000000000000000000, 0.8660254037844387076, 1.000000000000000000, 0.8660254037844387076, 1.000000000000000000, 0.8660254037844387076, 1.000000000000000000, 0.8660254037844387076, 1.000000000000000000, 0.8660254037844387076, 1.000000000000000000, 0.8660254037844387076, 1.000000000000000000, 0.8660254037844387076, 1.000000000000000000, 0.8660254037844387076, 1.000000000000000000, 0.8660254037844387076, 1.000000000000000000, 0.8660254037844387076, 1.000000000000000000, 0.8660254037844387076, 1.000000000000000000, 0.8660254037844387076, 1.000000000000000000, 0.8660254037844387076, 1.000000000000000000, 0.8660254037844387076, 1.000000000000000000, 0.8660254037844387076, 1.000000000000000000, 0.8660254037844387076, 1.000000000000000000, 0.8660254037844387076, 1.000000000000000000, 0.8660254037844387076, 1.000000000000000000, 0.8660254037844387076, 1.000000000000000000, 0.8660254037844387076, 1.000000000000000000, 0.8660254037844387076, 1.000000000000000000, 0.8660254037844387076, 1.000000000000000000, 0.8660254037844387076, 1.000000000000000000, 0.8660254037844387076, 1.000000000000000000, 0.8660254037844387076, 1.000000000000000000, 0.8660254037844387076, 1.000000000000000000, 0.8660254037844387076, 1.000000000000000000, 0.8660254037844387076, 1.000000000000000000, 0.8660254037844387076, 1.000000000000000000, 0.8660254037844387076, 1.000000000000000000, 0.8660254037844387076, 1.000000000000000000, 0.8660254037844387076, 1.000000000000000000, 0.8660254037844387076, 1.000000000000000000, 0.8660254037844387076, 1.000000000000000000, 0.8660254037844387076, 1.000000000000000000, 0.8660254037844387076, 1.000000000000000000, 0.8660254037844387076, 1.000000000000000000, 0.8660254037844387076, 1.000000000000000000, 0.8660254037844387076, 1.000000000000000000, 0.8660254037844387076, 1.000000000000000000, 0.8660254037844387076, 1.000000000000000000, 0.8660254037844387076, 1.000000000000000000, 0.8660254037844387076, 1.000000000000000000, 0.8660254037844387076, 1.000000000000000000, 0.8660254037844387076, 1.000000000000000000, 0.8660254037844387076, 1.000000000000000000, 0.8660254037844387076, 1.000000000000000000, 0.8660254037844387076, 1.000000000000000000, 0.8660254037844387076, 1.000000000000000000, 0.8660254037844387076, 1.000000000000000000, 0.8660254037844387076, 1.000000000000000000, 0.8660254037844387076, 1.000000000000000000, 0.8660254037844387076, 1.000000000000000000, 0.8660254037844387076, 1.000000000000000000, 0.8660254037844387076, 1.000000000000000000, 0.8660254037844387076, 1.000000000000000000, 0.8660254037844387076, 1.000000000000000000, 0.8660254037844387076, 1.000000000000000000, 0.8660254037844387076, 1.000000000000000000, 0.8660254037844387076, 1.000000000000000000, 0.8660254037844387076, 1.000000000000000000, 0.8660254037844387076, 1.000000000000000000, 0.8660254037844387076, 1.000000000000000000, 0.8660254037844387076, 1.000000000000000000, 0.8660254037844387076, 1.000000000000000000, 0.8660254037844387076, 1.000000000000000000, 0.8660254037844387076, 1.000000000000000000, 0.8660254037844387076, 1.000000000000000000, 0.8660254037844387076, 1.000000000000000000, 0.8660254037844387076, 1.000000000000000000, 0.8660254037844387076, 1.000000000000000000, 0.8660254037844387076, 1.000000000000000000, 0.8660254037844387076, 1.000000000000000000, 0.8660254037844387076, 1.000000000000000000, 0.8660254037844387076, 1.000000000000000000, 0.8660254037844387076, 1.000000000000000000, 0.8660254037844387076, 1.000000000000000000, 0.8660254037844387076, 1.000000000000000000, 0.8660254037844387076, 1.000000000000000000, 0.8660254037844387076, 1.000000000000000000, 0.8660254037844387076, 1.000000000000000000, 0.8660254037844387076, 1.000000000000000000, 0.8660254037844387076, 1.000000000000000000, 0.8660254037844387076, 1.000000000000000000, 0.8660254037844387076, 1.000000000000000000, 0.8660254037844387076, 1.000000000000000000, 0.8660254037844387076, 1.000000000000000000, 0.8660254037844387076, 1.000000000000000000, 0.8660254037844387076, 1.000000000000000000, 0.8660254037844387076, 1.000000000000000000, 0.8660254037844387076, 1.000000000000000000, 0.8660254037844387076, 1.000000000000000000, 0.8660254037844387076, 1.000000000000000000, 0.8660254037844387076, 1.000000000000000000, 0.8660254037844387076, 1.000000000000000000, 0.8660254037844387076, 1.000000000000000000, 0.8660254037844387076, 1.000000000000000000, 0.8660254037844387076, 1.000000000000000000, 0.8660254037844387076, 1.000000000000000000, 0.8660254037844387076, 1.000000000000000000, 0.8660254037844387076, 1.000000000000000000, 0.8660254037844387076, 1.000000000000000000, 0.8660254037844387076, 1.000000000000000000, 0.8660254037844387076, 1.000000000000000000, 0.8660254037844387076, 1.000000000000000000, 0.8660254037844387076, 1.000000000000000000, 0.8660254037844387076, 1.000000000000000000, 0.8660254037844387076, 1.000000000000000000, 0.8660254037844387076, 1.000000000000000000, 0.8660254037844387076, 1.000000000000000000, 0.8660254037844387076, 1.000000000000000000, 0.8660254037844387076, 1.000000000000000000, 0.8660254037844387076, 1.000000000000000000, 0.8660254037844387076, 1.000000000000000000, 0.8660254037844387076, 1.000000000000000000, 0.8660254037844387076, 1.000000000000000000, 0.8660254037844387076, 1.000000000000000000, 0.8660254037844387076, 1.000000000000000000, 0.8660254037844387076, 1.000000000000000000, 0.8660254037844387076, 1.000000000000000000, 0.8660254037844387076, 1.000000000000000000, 0.8660254037844387076, 1.000000000000000000, 0.8660254037844387076, 1.000000000000000000, 0.8660254037844387076, 1.000000000000000000, 0.8660254037844387076, 1.000000000000000000, 0.8660254037844387076, 1.000000000000000000, 0.8660254037844387076, 1.000000000000000000, 0.8660254037844387076, 1.000000000000000000, 0.8660254037844387076, 1.000000000000000000, 0.8660254037844387076, 1.000000000000000000, 0.8660254037844387076, 1.000000000000000000, 0.8660254037844387076, 1.000000000000000000, 0.8660254037844387076, 1.000000000000000000, 0.8660254037844387076, 1.000000000000000000, 0.8660254037844387076, 1.000000000000000000, 0.8660254037844387076, 1.000000000000000000, 0.8660254037844387076, 1.000000000000000000, 0.8660254037844387076, 1.000000000000000000, 0.8660254037844387076, 1.000000000000000000, 0.8660254037844387076, 1.000000000000000000, 0.8660254037844387076, 1.000000000000000000, 0.8660254037844387076, 1.000000000000000000, 0.8660254037844387076, 1.000000000000000000, 0.8660254037844387076, 1.000000000000000000, 0.8660254037844387076, 1.000000000000000000, 0.8660254037844387076, 1.000000000000000000, 0.8660254037844387076, 1.000000000000000000, 0.8660254037844387076, 1.000000000000000000, 0.8660254037844387076, 1.000000000000000000, 0.8660254037844387076, 1.000000000000000000, 0.8660254037844387076, 1.000000000000000000, 0.8660254037844387076, 1.000000000000000000, 0.8660254037844387076, 1.000000000000000000, 0.8660254037844387076, 1.000000000000000000, 0.8660254037844387076, 1.000000000000000000, 0.8660254037844387076, 1.000000000000000000, 0.8660254037844387076, 1.000000000000000000, 0.8660254037844387076, 1.000000000000000000, 0.8660254037844387076, 1.000000000000000000, 0.8660254037844387076, 1.000000000000000000, 0.8660254037844387076, 1.000000000000000000, 0.8660254037844387076, 1.000000000000000000, 0.8660254037844387076, 1.000000000000000000, 0.8660254037844387076, 1.000000000000000000, 0.8660254037844387076, 1.000000000000000000, 0.8660254037844387076, 1.000000000000000000, 0.8660254037844387076, 1.000000000000000000, 0.8660254037844387076, 1.000000000000000000, 0.8660254037844387076, 1.000000000000000000, 0.8660254037844387076, 1.000000000000000000, 0.8660254037844387076, 1.000000000000000000, 0.8660254037844387076, 1.000000000000000000, 0.8660254037844387076, 1.000000000000000000, 0.8660254037844387076, 1.000000000000000000, 0.8660254037844387076, 1.000000000000000000, 0.8660254037844387076, 1.000000000000000000, 0.8660254037844387076, 1.000000000000000000, 0.8660254037844387076, 1.000000000000000000, 0.8660254037844387076, 1.000000000000000000, 0.8660254037844387076, 1.000000000000000000, 0.8660254037844387076, 1.000000000000000000, 0.8660254037844387076, 1.000000000000000000, 0.8660254037844387076, 1.000000000000000000, 0.8660254037844387076, 1.000000000000000000, 0.8660254037844387076, 1.000000000000000000, 0.8660254037844387076, 1.000000000000000000, 0.8660254037844387076, 1.000000000000000000, 0.8660254037844387076, 1.000000000000000000, 0.8660254037844387076, 1.000000000000000000, 0.8660254037844387076, 1.000000000000000000, 0.8660254037844387076, 1.000000000000000000, 0.8660254037844387076, 1.000000000000000000, 0.8660254037844387076, 1.000000000000000000, 0.8660254037844387076, 1.000000000000000000, 0.8660254037844387076, 1.000000000000000000, 0.8660254037844387076, 1.000000000000000000, 0.8660254037844387076, 1.000000000000000000, 0.8660254037844387076, 1.000000000000000000, 0.8660254037844387076, 1.000000000000000000, 0.8660254037844387076, 1.000000000000000000, 0.8660254037844387076, 1.000000000000000000, 0.8660254037844387076, 1.000000000000000000, 0.8660254037844387076, 1.000000000000000000, 0.8660254037844387076, 1.000000000000000000, 0.8660254037844387076, 1.000000000000000000, 0.8660254037844387076, 1.000000000000000000, 0.8660254037844387076, 1.000000000000000000, 0.8660254037844387076, 1.000000000000000000, 0.8660254037844387076, 1.000000000000000000, 0.8660254037844387076, 1.000000000000000000, 0.8660254037844387076, 1.000000000000000000, 0.8660254037844387076, 1.000000000000000000, 0.8660254037844387076, 1.000000000000000000, 0.8660254037844387076, 1.000000000000000000),
 ( 1.000000000000000000, 0.8660254037844387076, 1.000000000000000000, 0.8660254037844387076, 1.000000000000000000, 0.8660254037844387076, 1.000000000000000000, 0.8660254037844387076, 1.000000000000000000, 0.8660254037844387076, 1.000000000000000000, 0.8660254037844387076, 1.000000000000000000, 0.8660254037844387076, 1.000000000000000000, 0.8660254037844387076, 1.000000000000000000, 0.8660254037844387076, 1.000000000000000000, 0.8660254037844387076, 1.000000000000000000, 0.8660254037844387076, 1.000000000000000000, 0.8660254037844387076, 1.000000000000000000, 0.8660254037844387076, 1.000000000000000000, 0.8660254037844387076, 1.000000000000000000, 0.8660254037844387076, 1.000000000000000000, 0.8660254037844387076, 1.000000000000000000, 0.8660254037844387076, 1.000000000000000000, 0.8660254037844387076, 1.000000000000000000, 0.8660254037844387076, 1.000000000000000000, 0.8660254037844387076, 1.000000000000000000, 0.8660254037844387076, 1.000000000000000000, 0.8660254037844387076, 1.000000000000000000, 0.8660254037844387076, 1.000000000000000000, 0.8660254037844387076, 1.000000000000000000, 0.8660254037844387076, 1.000000000000000000, 0.8660254037844387076, 1.000000000000000000, 0.8660254037844387076, 1.000000000000000000, 0.8660254037844387076, 1.000000000000000000, 0.8660254037844387076, 1.000000000000000000, 0.8660254037844387076, 1.000000000000000000, 0.8660254037844387076, 1.000000000000000000, 0.8660254037844387076, 1.000000000000000000, 0.8660254037844387076, 1.000000000000000000, 0.8660254037844387076, 1.000000000000000000, 0.8660254037844387076, 1.000000000000000000, 0.8660254037844387076, 1.000000000000000000, 0.8660254037844387076, 1.000000000000000000, 0.8660254037844387076, 1.000000000000000000, 0.8660254037844387076, 1.000000000000000000, 0.8660254037844387076, 1.000000000000000000, 0.8660254037844387076, 1.000000000000000000, 0.8660254037844387076, 1.000000000000000000, 0.8660254037844387076, 1.000000000000000000, 0.8660254037844387076, 1.000000000000000000, 0.8660254037844387076, 1.000000000000000000, 0.8660254037844387076, 1.000000000000000000, 0.8660254037844387076, 1.000000000000000000, 0.8660254037844387076, 1.000000000000000000, 0.8660254037844387076, 1.000000000000000000, 0.8660254037844387076, 1.000000000000000000, 0.8660254037844387076, 1.000000000000000000, 0.8660254037844387076, 1.000000000000000000, 0.8660254037844387076, 1.000000000000000000, 0.8660254037844387076, 1.000000000000000000, 0.8660254037844387076, 1.000000000000000000, 0.8660254037844387076, 1.000000000000000000, 0.8660254037844387076, 1.000000000000000000, 0.8660254037844387076, 1.000000000000000000, 0.8660254037844387076, 1.000000000000000000, 0.8660254037844387076, 1.000000000000000000, 0.8660254037844387076, 1.000000000000000000, 0.8660254037844387076, 1.000000000000000000, 0.8660254037844387076, 1.000000000000000000, 0.8660254037844387076, 1.000000000000000000, 0.8660254037844387076, 1.000000000000000000, 0.8660254037844387076, 1.000000000000000000, 0.8660254037844387076, 1.000000000000000000, 0.8660254037844387076, 1.000000000000000000, 0.8660254037844387076, 1.000000000000000000, 0.8660254037844387076, 1.000000000000000000, 0.8660254037844387076, 1.000000000000000000, 0.8660254037844387076, 1.000000000000000000, 0.8660254037844387076, 1.000000000000000000, 0.8660254037844387076, 1.000000000000000000, 0.8660254037844387076, 1.000000000000000000, 0.8660254037844387076, 1.000000000000000000, 0.8660254037844387076, 1.000000000000000000, 0.8660254037844387076, 1.000000000000000000, 0.8660254037844387076, 1.000000000000000000, 0.8660254037844387076, 1.000000000000000000, 0.8660254037844387076, 1.000000000000000000, 0.8660254037844387076, 1.000000000000000000, 0.8660254037844387076, 1.000000000000000000, 0.8660254037844387076, 1.000000000000000000, 0.8660254037844387076, 1.000000000000000000, 0.8660254037844387076, 1.000000000000000000, 0.8660254037844387076, 1.000000000000000000, 0.8660254037844387076, 1.000000000000000000, 0.8660254037844387076, 1.000000000000000000, 0.8660254037844387076, 1.000000000000000000, 0.8660254037844387076, 1.000000000000000000, 0.8660254037844387076, 1.000000000000000000, 0.8660254037844387076, 1.000000000000000000, 0.8660254037844387076, 1.000000000000000000, 0.8660254037844387076, 1.000000000000000000, 0.8660254037844387076, 1.000000000000000000, 0.8660254037844387076, 1.000000000000000000, 0.8660254037844387076, 1.000000000000000000, 0.8660254037844387076, 1.000000000000000000, 0.8660254037844387076, 1.000000000000000000, 0.8660254037844387076, 1.000000000000000000, 0.8660254037844387076, 1.000000000000000000, 0.8660254037844387076, 1.000000000000000000, 0.8660254037844387076, 1.000000000000000000, 0.8660254037844387076, 1.000000000000000000, 0.8660254037844387076, 1.000000000000000000, 0.8660254037844387076, 1.000000000000000000, 0.8660254037844387076, 1.000000000000000000, 0.8660254037844387076, 1.000000000000000000, 0.8660254037844387076, 1.000000000000000000, 0.8660254037844387076, 1.000000000000000000, 0.8660254037844387076, 1.000000000000000000, 0.8660254037844387076, 1.000000000000000000, 0.8660254037844387076, 1.000000000000000000, 0.8660254037844387076, 1.000000000000000000, 0.8660254037844387076, 1.000000000000000000, 0.8660254037844387076, 1.000000000000000000, 0.8660254037844387076, 1.000000000000000000, 0.8660254037844387076, 1.000000000000000000, 0.8660254037844387076, 1.000000000000000000, 0.8660254037844387076, 1.000000000000000000, 0.8660254037844387076, 1.000000000000000000, 0.8660254037844387076, 1.000000000000000000, 0.8660254037844387076, 1.000000000000000000, 0.8660254037844387076, 1.000000000000000000, 0.8660254037844387076, 1.000000000000000000, 0.8660254037844387076, 1.000000000000000000, 0.8660254037844387076, 1.000000000000000000, 0.8660254037844387076, 1.000000000000000000, 0.8660254037844387076, 1.000000000000000000, 0.8660254037844387076, 1.000000000000000000, 0.8660254037844387076, 1.000000000000000000, 0.8660254037844387076, 1.000000000000000000, 0.8660254037844387076, 1.000000000000000000, 0.8660254037844387076, 1.000000000000000000, 0.8660254037844387076, 1.000000000000000000, 0.8660254037844387076, 1.000000000000000000, 0.8660254037844387076, 1.000000000000000000, 0.8660254037844387076, 1.000000000000000000, 0.8660254037844387076, 1.000000000000000000, 0.8660254037844387076, 1.000000000000000000, 0.8660254037844387076, 1.000000000000000000, 0.8660254037844387076, 1.000000000000000000, 0.8660254037844387076, 1.000000000000000000, 0.8660254037844387076, 1.000000000000000000, 0.8660254037844387076, 1.000000000000000000, 0.8660254037844387076, 1.000000000000000000, 0.8660254037844387076, 1.000000000000000000, 0.8660254037844387076, 1.000000000000000000, 0.8660254037844387076, 1.000000000000000000, 0.8660254037844387076, 1.000000000000000000, 0.8660254037844387076, 1.000000000000000000, 0.8660254037844387076, 1.000000000000000000, 0.8660254037844387076, 1.000000000000000000, 0.8660254037844387076, 1.000000000000000000, 0.8660254037844387076, 1.000000000000000000, 0.8660254037844387076, 1.000000000000000000, 0.8660254037844387076, 1.000000000000000000, 0.8660254037844387076, 1.000000000000000000, 0.8660254037844387076, 1.000000000000000000, 0.8660254037844387076, 1.000000000000000000, 0.8660254037844387076, 1.000000000000000000, 0.8660254037844387076, 1.000000000000000000, 0.8660254037844387076, 1.000000000000000000, 0.8660254037844387076, 1.000000000000000000, 0.8660254037844387076, 1.000000000000000000, 0.8660254037844387076, 1.000000000000000000, 0.8660254037844387076, 1.000000000000000000, 0.8660254037844387076, 1.000000000000000000, 0.8660254037844387076, 1.000000000000000000, 0.8660254037844387076, 1.000000000000000000, 0.8660254037844387076, 1.000000000000000000, 0.8660254037844387076, 1.000000000000000000, 0.8660254037844387076, 1.000000000000000000, 0.8660254037844387076, 1.000000000000000000, 0.8660254037844387076, 1.000000000000000000, 0.8660254037844387076, 1.000000000000000000, 0.8660254037844387076, 1.000000000000000000, 0.8660254037844387076, 1.000000000000000000, 0.8660254037844387076, 1.000000000000000000, 0.8660254037844387076, 1.000000000000000000, 0.8660254037844387076, 1.000000000000000000, 0.8660254037844387076, 1.000000000000000000, 0.8660254037844387076, 1.000000000000000000, 0.8660254037844387076, 1.000000000000000000, 0.8660254037844387076, 1.000000000000000000, 0.8660254037844387076, 1.000000000000000000, 0.8660254037844387076, 1.000000000000000000, 0.8660254037844387076, 1.000000000000000000, 0.8660254037844387076, 1.000000000000000000, 0.8660254037844387076, 1.000000000000000000, 0.8660254037844387076, 1.000000000000000000, 0.8660254037844387076, 1.000000000000000000, 0.8660254037844387076, 1.000000000000000000, 0.8660254037844387076, 1.000000000000000000, 0.8660254037844387076, 1.000000000000000000, 0.8660254037844387076, 1.000000000000000000, 0.8660254037844387076, 1.000000000000000000, 0.8660254037844387076, 1.000000000000000000, 0.8660254037844387076, 1.000000000000000000, 0.8660254037844387076, 1.000000000000000000, 0.8660254037844387076, 1.000000000000000000, 0.8660254037844387076, 1.000000000000000000, 0.8660254037844387076, 1.000000000000000000, 0.8660254037844387076, 1.000000000000000000, 0.8660254037844387076, 1.000000000000000000, 0.8660254037844387076, 1.000000000000000000, 0.8660254037844387076, 1.000000000000000000, 0.8660254037844387076, 1.000000000000000000, 0.8660254037844387076, 1.000000000000000000, 0.8660254037844387076, 1.000000000000000000, 0.8660254037844387076, 1.000000000000000000, 0.8660254037844387076, 1.000000000000000000, 0.8660254037844387076, 1.000000000000000000, 0.8660254037844387076, 1.000000000000000000, 0.8660254037844387076, 1.000000000000000000, 0.8660254037844387076, 1.000000000000000000, 0.8660254037844387076, 1.000000000000000000, 0.8660254037844387076, 1.000000000000000000, 0.8660254037844387076, 1.000000000000000000, 0.8660254037844387076, 1.000000000000000000, 0.8660254037844387076, 1.000000000000000000, 0.8660254037844387076, 1.000000000000000000, 0.8660254037844387076, 1.000000000000000000, 0.8660254037844387076, 1.000000000000000000, 0.8660254037844387076, 1.000000000000000000, 0.8660254037844387076, 1.000000000000000000, 0.8660254037844387076, 1.000000000000000000, 0.8660254037844387076, 1.000000000000000000, 0.8660254037844387076, 1.000000000000000000, 0.8660254037844387076, 1.000000000000000000, 0.8660254037844387076, 1.000000000000000000, 0.8660254037844387076, 1.000000000000000000, 0.8660254037844387076, 1.000000000000000000, 0.8660254037844387076, 1.000000000000000000, 0.8660254037844387076, 1.000000000000000000, 0.8660254037844387076, 1.000000000000000000, 0.8660254037844387076, 1.000000000000000000, 0.8660254037844387076, 1.000000000000000000, 0.8660254037844387076, 1.000000000000000000) ) ) 
 REPRESENTATION_ITEM ( '' )  SURFACE ( )  );
#188389 = CARTESIAN_POINT ( 'NONE',  ( 2.109626794357027268, 0.001117226762978317921, 1.734343004219033757 ) ) ;
#188390 = CARTESIAN_POINT ( 'NONE',  ( -3.098866152801546647, 14.55178984617735694, 11.55550500168035555 ) ) ;
#188391 = CARTESIAN_POINT ( 'NONE',  ( 1.499999999999990896, 5.556250000682820378, 1.214306433183764966E-14 ) ) ;
#188392 = CARTESIAN_POINT ( 'NONE',  ( -4.882907879216086933, 8.848476292394087395, -0.7998128361456281477 ) ) ;
#188393 = CARTESIAN_POINT ( 'NONE',  ( 6.773846765307952822, -7.473374494058216300, -6.773846765307982132 ) ) ;
#188394 = CARTESIAN_POINT ( 'NONE',  ( 6.860228214211484321, -2.170771502548960452, 0.04436455139915015944 ) ) ;
#188395 = CARTESIAN_POINT ( 'NONE',  ( 5.918537399722813674, 1.222626809077583587, -1.356019982345892050 ) ) ;
#188396 = CARTESIAN_POINT ( 'NONE',  ( 3.098438489093110704, 1.946378968836332213, 0.2448508753878294586 ) ) ;
#188397 = CARTESIAN_POINT ( 'NONE',  ( -4.036671995544492297, 7.285761072467114019, 0.7944190476826870073 ) ) ;
#188398 = CARTESIAN_POINT ( 'NONE',  ( -7.831806290188425557, 12.28885777186185990, -0.7998128361456281477 ) ) ;
#188399 = CARTESIAN_POINT ( 'NONE',  ( 7.100719765255169236, 9.307259030929609267, -1.599625672291262513 ) ) ;
#188400 = CARTESIAN_POINT ( 'NONE',  ( 3.264422710156249963, 2.120667954687505574, -0.001943060928578931989 ) ) ;
#188401 = CARTESIAN_POINT ( 'NONE',  ( -2.318081078256692518, 5.648252324700675508, 1.040834085586084257E-14 ) ) ;
#188402 = TOROIDAL_SURFACE ( 'NONE', #1602, 0.8300000000000010703, 0.08000000000000000167 ) ;
#188403 = CARTESIAN_POINT ( 'NONE',  ( 0.4366703603831034175, -8.283751815806033036, -10.40709768291843673 ) ) ;
#188404 = CARTESIAN_POINT ( 'NONE',  ( 1.815371668717490339, -1.773540675419151169, -1.067758146248848128 ) ) ;
#188406 = CARTESIAN_POINT ( 'NONE',  ( -1.364683531250000748, -0.6781249996585803075, 0.000000000000000000 ) ) ;
#188405 = CARTESIAN_POINT ( 'NONE',  ( 6.827182134110225675, 7.053278108740402175, 2.409100297097351184 ) ) ;
#188409 = VERTEX_POINT ( 'NONE', #149214 ) ;
#188408 = CARTESIAN_POINT ( 'NONE',  ( 4.178555957833706813, 1.047420865545487523, 1.958865958838784005 ) ) ;
#188407 = AXIS2_PLACEMENT_3D ( 'NONE', #147364, #213390, #15196 ) ;
#188410 = CARTESIAN_POINT ( 'NONE',  ( 1.688534781859708067, 1.914194972067848832, 1.272504748915660899 ) ) ;
#188412 = CARTESIAN_POINT ( 'NONE',  ( 6.719587945281444874, 0.3584770237896938716, -2.031047634367310284 ) ) ;
#188411 = CARTESIAN_POINT ( 'NONE',  ( 9.408995418203963013, 12.00024729270324286, 1.443375672974076540 ) ) ;
#188414 = CARTESIAN_POINT ( 'NONE',  ( 3.285556943749998737, -3.755208332855373587, -1.896917185911906500 ) ) ;
#188413 = CARTESIAN_POINT ( 'NONE',  ( 3.607351389687783794, 6.366271167014519783, 1.199719254218451159 ) ) ;
#188415 = CARTESIAN_POINT ( 'NONE',  ( 0.4999999999999900080, 3.949999999999995293, -0.4000000000000339950 ) ) ;
#188416 = CARTESIAN_POINT ( 'NONE',  ( 6.198766299729112639, 1.534709720371667308, 1.016988835930050739 ) ) ;
#188417 = ORIENTED_EDGE ( 'NONE', *, *, #118518, .T. ) ;
#188418 = DIRECTION ( 'NONE',  ( 0.000000000000000000, 0.000000000000000000, -1.000000000000000000 ) ) ;
#188419 = CARTESIAN_POINT ( 'NONE',  ( 3.304848191199673213, -0.3775801424153284458, -1.874573493127674961 ) ) ;
#188420 = CARTESIAN_POINT ( 'NONE',  ( -0.1104750535120268828, 7.629137130509074716, -2.703481013110929254 ) ) ;
#188421 = CARTESIAN_POINT ( 'NONE',  ( 3.539825753290166688, 0.7759033148657649148, -1.540472896381483769 ) ) ;
#188422 = CARTESIAN_POINT ( 'NONE',  ( 1.938685741270998797, -1.555697844595272716, 1.282991390469834458 ) ) ;
#188423 = CARTESIAN_POINT ( 'NONE',  ( 4.377739380128500279, -0.5030580445687399260, -2.242836179151234344 ) ) ;
#188424 = AXIS2_PLACEMENT_3D ( 'NONE', #47772, #67150, #146337 ) ;
#188425 = CARTESIAN_POINT ( 'NONE',  ( 3.286655449121218542, -2.228332854187901280, -0.3904065581350114611 ) ) ;
#188426 = CARTESIAN_POINT ( 'NONE',  ( 6.481095854277318935, -0.1012916397761880333, -2.103764601514758414 ) ) ;
#188427 = CARTESIAN_POINT ( 'NONE',  ( -6.156811154381562012, 6.355570232966157640, 0.7216878364870257245 ) ) ;
#188428 = EDGE_LOOP ( 'NONE', ( #93075, #7195, #42192, #127072 ) ) ;
#188429 = CARTESIAN_POINT ( 'NONE',  ( 4.815556489234497306, -1.735627832820924477, 0.3447801454335273630 ) ) ;
#188431 = CARTESIAN_POINT ( 'NONE',  ( 0.6215105264332577706, -2.174887359234744633, 0.7243307227927602288 ) ) ;
#188430 = CARTESIAN_POINT ( 'NONE',  ( 5.189738938980948291, 9.276722205444929870, 0.000000000000000000 ) ) ;
#188432 = CARTESIAN_POINT ( 'NONE',  ( 5.929618730664214077, 0.9035273275350870215, -1.604119651413847603 ) ) ;
#188433 = CARTESIAN_POINT ( 'NONE',  ( -3.785751206713858785, 5.439795712631356750, 1.599625672291267398 ) ) ;
#188434 = UNCERTAINTY_MEASURE_WITH_UNIT (LENGTH_MEASURE( 1.000000000000000082E-05 ), #137934, 'distance_accuracy_value', 'NONE');
#188435 = CARTESIAN_POINT ( 'NONE',  ( 5.595707529797693702, -2.191629465999441084, -0.002916574791289594515 ) ) ;
#188436 = CARTESIAN_POINT ( 'NONE',  ( -3.297657676621885692, 4.870353260857385180, 1.599625672291267398 ) ) ;
#188437 = CARTESIAN_POINT ( 'NONE',  ( -4.337327078093950128, 15.44737643973769359, 11.15018912635215464 ) ) ;
#188438 = CARTESIAN_POINT ( 'NONE',  ( 5.670397268163976712, -0.9275489576153757021, -1.851018422006404096 ) ) ;
#188439 = CARTESIAN_POINT ( 'NONE',  ( -0.1531117392989979065, -1.803405091603600185, -0.9023890051431044945 ) ) ;
#188440 = CARTESIAN_POINT ( 'NONE',  ( -0.6823417656249969321, 5.717708333674756283, -1.181850606188749264 ) ) ;
#188441 = CARTESIAN_POINT ( 'NONE',  ( 4.547439623722833169, -1.490282656903282099, -1.220848939070565686 ) ) ;
#188442 = CARTESIAN_POINT ( 'NONE',  ( -0.6823417656250003738, 10.15104166700806587, 1.181850606188754593 ) ) ;
#188444 = CARTESIAN_POINT ( 'NONE',  ( -4.609409038966253647, 4.479991421656468908, -0.7216878364870207285 ) ) ;
#188443 = CIRCLE ( 'NONE', #95096, 11.09999999999999964 ) ;
#188445 = CARTESIAN_POINT ( 'NONE',  ( 1.266231527720959926, 0.6383494478915030523, -2.127751457625071563 ) ) ;
#188447 = ORIENTED_EDGE ( 'NONE', *, *, #86344, .T. ) ;
#188446 = CARTESIAN_POINT ( 'NONE',  ( -0.4019237886466871523, 13.22991455036742714, -1.499999999999998668 ) ) ;
#188449 = CARTESIAN_POINT ( 'NONE',  ( 0.000000000000000000, 0.2000000000000057288, 0.000000000000000000 ) ) ;
#188448 = CARTESIAN_POINT ( 'NONE',  ( 6.720655732516622294, 7.629137130509072051, 2.773739711112707340 ) ) ;
#188450 = CARTESIAN_POINT ( 'NONE',  ( 4.539282502477016479, 4.190251095844947926, 0.7998128361456341429 ) ) ;
#188451 = CARTESIAN_POINT ( 'NONE',  ( 0.000000000000000000, 12.30000000000000071, 0.000000000000000000 ) ) ;
#188452 = LINE ( 'NONE', #140815, #100998 ) ;
#188453 = CARTESIAN_POINT ( 'NONE',  ( 10.19631792989279084, 10.81030520795681582, -6.241902085265002675 ) ) ;
#188454 = CARTESIAN_POINT ( 'NONE',  ( 10.52076401408022299, 11.37657222595619189, 0.000000000000000000 ) ) ;
#188455 = CARTESIAN_POINT ( 'NONE',  ( 1.416376618315864144, 0.7919773292732554815, 1.795081228748253377 ) ) ;
#188456 = CARTESIAN_POINT ( 'NONE',  ( -1.402160292154681736E-14, 2.509375000341417028, -1.575800808251660134 ) ) ;
#188457 = EDGE_CURVE ( 'NONE', #150697, #66179, #166534, .T. ) ;
#188458 = CARTESIAN_POINT ( 'NONE',  ( 1.499999999999990896, 3.775000000000021227, 1.214306433183764966E-14 ) ) ;
#188459 = CARTESIAN_POINT ( 'NONE',  ( 6.250445965835445428, -1.952298026214387194, -0.1936728439068043650 ) ) ;
#188460 = CARTESIAN_POINT ( 'NONE',  ( -9.158696461231359720, 10.64389961198009615, 1.199719254218462483 ) ) ;
#188461 = CARTESIAN_POINT ( 'NONE',  ( -5.544921637864841379, 5.571422787038166291, -0.7216878364870197293 ) ) ;
#188462 = CARTESIAN_POINT ( 'NONE',  ( 0.5501786683353731000, 0.7064523498505774768, -2.149447411369388217 ) ) ;
#188464 = EDGE_LOOP ( 'NONE', ( #195303, #44144, #98848, #24762 ) ) ;
#188463 = CARTESIAN_POINT ( 'NONE',  ( -6.891622154448065807, 6.934647356477856128, 1.040834085586084257E-14 ) ) ;
#188465 = CARTESIAN_POINT ( 'NONE',  ( 1.499999999999987121, -1.214583332650518432, 0.8660254037844524744 ) ) ;
#188466 = CARTESIAN_POINT ( 'NONE',  ( 1.950266909631480861, 0.5821006739541793040, 1.777759251391328732 ) ) ;
#188467 = CARTESIAN_POINT ( 'NONE',  ( 7.214646527853999024E-05, -1.701284277595259464, 0.3348680416483724720 ) ) ;
#188469 = CARTESIAN_POINT ( 'NONE',  ( 4.616832073239669043, -0.1072513232249286408, 2.189039617437993357 ) ) ;
#188468 = CARTESIAN_POINT ( 'NONE',  ( 0.6801582343749970061, 2.223958333674731946, 1.178068619123799898 ) ) ;
#188470 = CARTESIAN_POINT ( 'NONE',  ( 4.050101169753547836, 0.7808133845815302676, -2.171591319759837546 ) ) ;
#188471 = B_SPLINE_CURVE_WITH_KNOTS ( 'NONE', 3,
 ( #57378, #39000, #123542, #7539, #204666, #73623, #43284 ),
 .UNSPECIFIED., .F., .F.,
 ( 4, 3, 4 ),
 ( 3.315837474970997266E-05, 0.0009000000035470257127, 0.001929259801299054245 ),
 .UNSPECIFIED. ) ;
#188472 = CARTESIAN_POINT ( 'NONE',  ( 6.555941810938458403, 2.055592219362284201, -0.1468124517445909549 ) ) ;
#188473 = CARTESIAN_POINT ( 'NONE',  ( 2.449080105735270685, 0.5175099976203160201, -1.871664248846743872 ) ) ;
#188474 = CARTESIAN_POINT ( 'NONE',  ( -4.392478580703220281, 8.068382744221649361, 1.040834085586084257E-14 ) ) ;
#188476 = EDGE_CURVE ( 'NONE', #2895, #109653, #109321, .T. ) ;
#188475 = AXIS2_PLACEMENT_3D ( 'NONE', #84486, #34667, #120266 ) ;
#188477 = CARTESIAN_POINT ( 'NONE',  ( -15.75000000000000000, 13.40000000000000036, -1.400000000000001910 ) ) ;
#188478 = CARTESIAN_POINT ( 'NONE',  ( 5.185831674374465905, 2.043064739972153543, -0.5678235988075125418 ) ) ;
#188479 = CARTESIAN_POINT ( 'NONE',  ( -1.360316468750007779, 0.1406250003413919702, -1.734723475976807094E-15 ) ) ;
#188480 = CARTESIAN_POINT ( 'NONE',  ( 3.533827422916273164, -1.646839391163470223, 1.163268690995450383 ) ) ;
#188481 = CARTESIAN_POINT ( 'NONE',  ( -3.917943204224913156, 7.514758138330285497, -0.7216878364870257245 ) ) ;
#188482 = CARTESIAN_POINT ( 'NONE',  ( -5.759181390754928742, 9.941071732514568993, 0.000000000000000000 ) ) ;
#188483 = CARTESIAN_POINT ( 'NONE',  ( 8.886479618753304166, 12.45497775759917758, -1.199719254218446718 ) ) ;
#188484 = CARTESIAN_POINT ( 'NONE',  ( 1.119449510670032177, -1.781678707675336870, 0.3977030049751931196 ) ) ;
#188485 = CARTESIAN_POINT ( 'NONE',  ( -6.099189001301292379, 8.209082816308541197, 1.599625672291263179 ) ) ;
#188486 = DIRECTION ( 'NONE',  ( 1.000000000000000000, 3.451266460341927087E-31, 0.000000000000000000 ) ) ;
#188487 = CARTESIAN_POINT ( 'NONE',  ( -10.47051000334347570, 4.046481986658133856, 7.152373939818348347 ) ) ;
#188488 = EDGE_LOOP ( 'NONE', ( #189956, #98734 ) ) ;
#188489 = CARTESIAN_POINT ( 'NONE',  ( 5.858293207932864455, 0.8329246649354884457, 1.885258002110825615 ) ) ;
#188490 = CARTESIAN_POINT ( 'NONE',  ( -6.956742217143487395, 8.249192353823097790, 1.082531754730549078 ) ) ;
#188491 = CARTESIAN_POINT ( 'NONE',  ( -4.440459003675619520, 5.139289244831666714, 1.199719254218462483 ) ) ;
#188492 = CARTESIAN_POINT ( 'NONE',  ( -8.622095623286845978, 12.14652976288826913, 1.199719254218462483 ) ) ;
#188493 = CARTESIAN_POINT ( 'NONE',  ( 5.145178147197468022, 0.1505999202349363186, 2.014131245181075336 ) ) ;
#188495 = ORIENTED_EDGE ( 'NONE', *, *, #117200, .F. ) ;
#188494 = CARTESIAN_POINT ( 'NONE',  ( 5.865950696152278709, 0.6470421894613547220, -2.124994868043238672 ) ) ;
#188496 = CARTESIAN_POINT ( 'NONE',  ( -4.842197138736131556, 5.678260079060780008, 1.199719254218452935 ) ) ;
#188497 = CARTESIAN_POINT ( 'NONE',  ( 5.738125327081736060, 7.717565519727259904, 1.599625672291267398 ) ) ;
#188498 = CARTESIAN_POINT ( 'NONE',  ( 4.575106920794588916, 0.002012451770977418796, -2.061077815012714254 ) ) ;
#188499 = CARTESIAN_POINT ( 'NONE',  ( 4.201796189063250253, 1.844709454618495670, 0.8146275914719460776 ) ) ;
#188500 = ORIENTED_EDGE ( 'NONE', *, *, #89525, .F. ) ;
#188501 = DIRECTION ( 'NONE',  ( 0.000000000000000000, 1.000000000000000000, -8.546850786086437571E-32 ) ) ;
#188502 = CARTESIAN_POINT ( 'NONE',  ( 4.403700966340357681, 4.032072637018845107, -0.7998128361456211532 ) ) ;
#188504 = ORIENTED_EDGE ( 'NONE', *, *, #95474, .F. ) ;
#188503 = CARTESIAN_POINT ( 'NONE',  ( -6.474900878978163021, 9.711745571186627402, -1.199719254218452047 ) ) ;
#188505 = CARTESIAN_POINT ( 'NONE',  ( 5.061762083669725243, 7.855803969722688684, -1.119403510469544782 ) ) ;
#188506 = CARTESIAN_POINT ( 'NONE',  ( 4.552111140598270822, 1.802141083034415781, -0.9039717811075360654 ) ) ;
#188507 = CARTESIAN_POINT ( 'NONE',  ( 3.450948914068392881, 0.4461466885457600062, -1.786139022923169506 ) ) ;
#188508 = EDGE_CURVE ( 'NONE', #130707, #23166, #180646, .T. ) ;
#188509 = CARTESIAN_POINT ( 'NONE',  ( -3.197497122698730099, 6.431928158754200986, 0.6077543439236172684 ) ) ;
#188510 = CARTESIAN_POINT ( 'NONE',  ( 1.682680061667326088, -1.231660274741898320, 1.951365989292063174 ) ) ;
#188511 = CARTESIAN_POINT ( 'NONE',  ( 5.585032934186686226, 5.480569609498057382, 0.000000000000000000 ) ) ;
#188512 = CARTESIAN_POINT ( 'NONE',  ( 4.165412764819938829, 0.2691229397190370576, -2.144731622849817221 ) ) ;
#188513 = CARTESIAN_POINT ( 'NONE',  ( 8.769426429940780920, 9.125419011219408461, 0.7998128361456462443 ) ) ;
#188514 = CARTESIAN_POINT ( 'NONE',  ( -6.112028321662274166, 6.025121218227761588, 0.7998128361456341429 ) ) ;
#188515 = CARTESIAN_POINT ( 'NONE',  ( 3.216491754421717530, -1.877423419238280822, -1.325616196499669108 ) ) ;
#188516 = LINE ( 'NONE', #40147, #11077 ) ;
#188517 = CARTESIAN_POINT ( 'NONE',  ( 2.026040307571222332, 1.079255042350239391, -1.527726335390042767 ) ) ;
#188518 = CARTESIAN_POINT ( 'NONE',  ( 0.1749903794560749015, 0.004523422195312763391, -1.955468523092759536 ) ) ;
#188521 = EDGE_CURVE ( 'NONE', #146898, #109724, #83999, .T. ) ;
#188520 = CARTESIAN_POINT ( 'NONE',  ( -8.072954122294394352, 8.383144328957069291, -0.7998128361456362523 ) ) ;
#188519 = CARTESIAN_POINT ( 'NONE',  ( -1.201851678989727383E-14, 4.196875000341417028, -1.575800808251660134 ) ) ;
#188523 = CARTESIAN_POINT ( 'NONE',  ( 1.524350002934187653, -1.228176919886795782, -1.833354347511229498 ) ) ;
#188522 = CARTESIAN_POINT ( 'NONE',  ( -5.494078562035765501, 7.432844293840273231, -1.599625672291256295 ) ) ;
#188524 = CARTESIAN_POINT ( 'NONE',  ( -1.874158809982179319, 3.299964346911585356, 0.3999999999999993006 ) ) ;
#188525 = CARTESIAN_POINT ( 'NONE',  ( 4.157546660884947620, 8.002221537674429896, 1.040834085586084257E-14 ) ) ;
#188526 = CARTESIAN_POINT ( 'NONE',  ( -4.415151579544611238, 8.302760609444034046, -0.7998128361456281477 ) ) ;
#188527 = CARTESIAN_POINT ( 'NONE',  ( -7.720982915750198572, -5.743759731405759794, 7.834948807407328353 ) ) ;
#188528 = CARTESIAN_POINT ( 'NONE',  ( 5.805538644497215017, -0.4794378417142564075, 1.912156289036368806 ) ) ;
#188529 = ADVANCED_FACE ( 'NONE', ( #17055 ), #195838, .F. ) ;
#188530 = CARTESIAN_POINT ( 'NONE',  ( 5.795647523915807398, 1.743732541305573758, 1.511695197786174782 ) ) ;
#188531 = CARTESIAN_POINT ( 'NONE',  ( 0.6605093422152423788, -0.6574743052488278838, -1.848563176889833626 ) ) ;
#188532 = CARTESIAN_POINT ( 'NONE',  ( 3.450102088163331082, -0.8403066601648312428, 1.883826651212586745 ) ) ;
#188533 = CARTESIAN_POINT ( 'NONE',  ( 6.263503779833467178, 9.290876262238963790, -1.082531754730537088 ) ) ;
#188534 = CARTESIAN_POINT ( 'NONE',  ( 6.587282531393223728, 8.778525268082516320, 1.599625672291268286 ) ) ;
#188535 = CARTESIAN_POINT ( 'NONE',  ( 6.765155463094746580, 9.876136559377135526, 1.082531754730558626 ) ) ;
#188536 = CARTESIAN_POINT ( 'NONE',  ( 0.6823417656249899377, 2.905208333674754062, 1.181850606188765695 ) ) ;
#188537 = CARTESIAN_POINT ( 'NONE',  ( -11.06299035296667732, 12.34316295623905191, -0.9087041361035911313 ) ) ;
#188538 = CARTESIAN_POINT ( 'NONE',  ( 5.463572716182834910, 5.476515711742504067, 0.7216878364870317197 ) ) ;
#188539 = CARTESIAN_POINT ( 'NONE',  ( 5.846172790272405884, -0.9815748167120906809, 1.936718618010783377 ) ) ;
#188541 = CARTESIAN_POINT ( 'NONE',  ( 5.003375819710620398, -1.831856422778654681, 0.1858995714831001289 ) ) ;
#188540 = CARTESIAN_POINT ( 'NONE',  ( 2.679285714285720044, 0.4970443252110459120, -0.09999999999999592548 ) ) ;
#188542 = AXIS2_PLACEMENT_3D ( 'NONE', #111928, #177929, #80418 ) ;
#188543 = CARTESIAN_POINT ( 'NONE',  ( 6.620655732516647518, 7.053381450551401421, 2.424417106520880161 ) ) ;
#188544 = CARTESIAN_POINT ( 'NONE',  ( 0.3999999999999901412, 3.964661556059753789, 0.9099571394228996857 ) ) ;
#188545 = CARTESIAN_POINT ( 'NONE',  ( 0.3505827959322353471, -1.506356567903786470, 1.108807183729618062 ) ) ;
#188546 = CARTESIAN_POINT ( 'NONE',  ( 0.7380304622728722785, -1.600708836854593198, -1.599060815671312641 ) ) ;
#188547 = CARTESIAN_POINT ( 'NONE',  ( -4.074449998555902397, 7.717048951691181102, 0.6760625908293280695 ) ) ;
#188548 = DIRECTION ( 'NONE',  ( 0.000000000000000000, -7.254698431504949604E-17, 1.000000000000000000 ) ) ;
#188549 = CARTESIAN_POINT ( 'NONE',  ( 6.578229047358968629, 6.784305542873760864, 0.2988042929856441488 ) ) ;
#188550 = CARTESIAN_POINT ( 'NONE',  ( -1.310129046446498746, 3.547233999020424466, -0.4142140226951010473 ) ) ;
#188551 = CARTESIAN_POINT ( 'NONE',  ( 1.656752475421595872, -1.515787608549432175, -0.9133899773908128461 ) ) ;
#188552 = CARTESIAN_POINT ( 'NONE',  ( 6.621754286443582771, -0.4424289334611238300, 1.971349943050800801 ) ) ;
#188553 = B_SPLINE_CURVE_WITH_KNOTS ( 'NONE', 3,
 ( #70316, #51976, #71386, #35705, #100713, #54103, #38916, #84461, #169970, #165722 ),
 .UNSPECIFIED., .F., .F.,
 ( 4, 3, 3, 4 ),
 ( 3.588344277745669791E-16, 3.125155930788468421E-05, 5.676974391825271470E-05, 8.229510585278265896E-05 ),
 .UNSPECIFIED. ) ;
#188555 = CARTESIAN_POINT ( 'NONE',  ( 3.620622283765279725, 0.2843237153829519248, 1.894267977526209012 ) ) ;
#188554 = CARTESIAN_POINT ( 'NONE',  ( -10.50487009249003378, 11.15010328419353947, 0.7998128361456462443 ) ) ;
#188556 = CARTESIAN_POINT ( 'NONE',  ( 5.756345505848640798, 6.148709499980903992, 0.8262799378709930753 ) ) ;
#188557 = CARTESIAN_POINT ( 'NONE',  ( 3.912524032909367566, 0.7067130192578415793, 1.838586846604377323 ) ) ;
#188558 = CARTESIAN_POINT ( 'NONE',  ( -0.01710467543277957581, -1.380256469788909035, 1.610041658517608054 ) ) ;
#188559 = CARTESIAN_POINT ( 'NONE',  ( -3.918470089549458635, 4.530302178351167441, -1.199719254218452047 ) ) ;
#188560 = CARTESIAN_POINT ( 'NONE',  ( 2.606148294764852213, -0.7140300644919925777, -1.729217693616967644 ) ) ;
#188562 = ORIENTED_EDGE ( 'NONE', *, *, #106488, .T. ) ;
#188561 = CARTESIAN_POINT ( 'NONE',  ( 6.217413168894407427, -0.2034119912461933299, 1.712789424573582409 ) ) ;
#188564 = CARTESIAN_POINT ( 'NONE',  ( 2.684151225825664788, 5.114964949229812596, -1.082531754730543083 ) ) ;
#188563 = CARTESIAN_POINT ( 'NONE',  ( 2.157103830005083100, -1.704838622333640030, 1.401371054633032909 ) ) ;
#188565 = CARTESIAN_POINT ( 'NONE',  ( -1.364683531250012516, 3.342708333674756727, 0.7879004041258379498 ) ) ;
#188566 = CARTESIAN_POINT ( 'NONE',  ( 6.338335788673861160, -1.050647824335379399, 1.656640365463659670 ) ) ;
#188567 = CARTESIAN_POINT ( 'NONE',  ( 8.209625708274705502, 9.536650400197368427, 1.199719254218462483 ) ) ;
#188569 = CARTESIAN_POINT ( 'NONE',  ( -7.664865541497347223, -5.787795860784272328, 7.047292192038678849 ) ) ;
#188568 =( GEOMETRIC_REPRESENTATION_CONTEXT ( 3 ) GLOBAL_UNCERTAINTY_ASSIGNED_CONTEXT ( ( #116084 ) ) GLOBAL_UNIT_ASSIGNED_CONTEXT ( ( #11767, #51759, #66887 ) ) REPRESENTATION_CONTEXT ( 'NONE', 'WORKASPACE' ) );
#188570 = CARTESIAN_POINT ( 'NONE',  ( 1.249999999999997558, -1.500000000000001332, 1.734723475976807094E-15 ) ) ;
#188571 = CARTESIAN_POINT ( 'NONE',  ( -4.011515005667116718, 5.867910776320241162, 1.537733183400939119 ) ) ;
#188572 = DIRECTION ( 'NONE',  ( -0.000000000000000000, -1.000000000000000000, -0.000000000000000000 ) ) ;
#188573 = ORIENTED_EDGE ( 'NONE', *, *, #22230, .F. ) ;
#188574 = CARTESIAN_POINT ( 'NONE',  ( 2.594261239525695206, 0.9781076984213372683, -1.824767828009652426 ) ) ;
#188575 = CARTESIAN_POINT ( 'NONE',  ( -1.201851678989727383E-14, 3.587500000000020339, -1.732050807568863648 ) ) ;
#188576 = CARTESIAN_POINT ( 'NONE',  ( 6.335737856287750880, 6.286115675290828264, -0.7998128361456281477 ) ) ;
#188577 = CARTESIAN_POINT ( 'NONE',  ( -6.279577920751266973, 6.982973266031838655, 0.9645283542769074181 ) ) ;
#188578 = CARTESIAN_POINT ( 'NONE',  ( 0.3463606850301796380, 1.036194208456611809, -1.733443346147050868 ) ) ;
#188579 = CARTESIAN_POINT ( 'NONE',  ( 1.499999999999999112, 7.438721522839136568, 4.195160983902605167 ) ) ;
#188580 = CARTESIAN_POINT ( 'NONE',  ( -1.364683531249997417, 4.259375000341424133, 1.214306433183764966E-14 ) ) ;
#188582 = CARTESIAN_POINT ( 'NONE',  ( 9.761507412159302177, 10.49077285704843199, -0.7216878364870257245 ) ) ;
#188581 = CARTESIAN_POINT ( 'NONE',  ( 0.07459516483346650961, 6.948550711820903558, -2.350542341214032493 ) ) ;
#188583 = CARTESIAN_POINT ( 'NONE',  ( 5.817732461567613811, -1.591073081590413052, 1.238133459405404757 ) ) ;
#188584 = CARTESIAN_POINT ( 'NONE',  ( 5.823430154129352054, -1.392497453891910375, -1.315930268783272794 ) ) ;
#188585 = DIRECTION ( 'NONE',  ( 0.000000000000000000, 1.000000000000000000, 0.000000000000000000 ) ) ;
#188586 = CARTESIAN_POINT ( 'NONE',  ( 4.036819321710017228, -1.906298169312226953, 1.081085072550565407 ) ) ;
#188587 =( BOUNDED_CURVE ( )  B_SPLINE_CURVE ( 3, ( #43079, #206603, #108117, #208728 ),
 .UNSPECIFIED., .F., .T. ) 
 B_SPLINE_CURVE_WITH_KNOTS ( ( 4, 4 ),
 ( 0.000000000000000000, 0.5000000000000006661 ),
 .UNSPECIFIED. ) 
 CURVE ( )  GEOMETRIC_REPRESENTATION_ITEM ( )  RATIONAL_B_SPLINE_CURVE ( ( 1.000000000000000000, 0.3333333333333324822, 0.3333333333333333703, 1.000000000000000888 ) ) 
 REPRESENTATION_ITEM ( '' )  );
#188588 = CARTESIAN_POINT ( 'NONE',  ( 1.499999999999989120, 2.535416667349483344, 0.8660254037844524744 ) ) ;
#188589 = CARTESIAN_POINT ( 'NONE',  ( 2.566550162062298579, 0.6480892470011965223, 1.799338185917313870 ) ) ;
#188590 = CARTESIAN_POINT ( 'NONE',  ( -6.013204822860843457, 6.974159367214481264, -1.199719254218446718 ) ) ;
#188591 = CARTESIAN_POINT ( 'NONE',  ( 3.660338285565247762, 7.214219066560688454, 1.040834085586084257E-14 ) ) ;
#188593 = CARTESIAN_POINT ( 'NONE',  ( 0.1402502066264778580, 0.7743353953559418690, 1.862009890338502505 ) ) ;
#188592 = DIRECTION ( 'NONE',  ( 0.000000000000000000, -1.000000000000000000, 0.000000000000000000 ) ) ;
#188595 = EDGE_CURVE ( 'NONE', #140029, #127623, #39682, .T. ) ;
#188594 = CARTESIAN_POINT ( 'NONE',  ( -1.364683531250014514, 10.90104166700806942, -0.7879004041258335089 ) ) ;
#188597 = CARTESIAN_POINT ( 'NONE',  ( -5.094831863685302942, 9.165997284266655498, 0.7998128361456291469 ) ) ;
#188596 = CARTESIAN_POINT ( 'NONE',  ( 5.864808805604324604, 0.1626094438406736342, -2.185560445749204828 ) ) ;
#188599 = ORIENTED_EDGE ( 'NONE', *, *, #75356, .T. ) ;
#188598 = CARTESIAN_POINT ( 'NONE',  ( 3.188212539307228699, -1.698978696193183202, -0.2961410920078124676 ) ) ;
#188600 = CARTESIAN_POINT ( 'NONE',  ( 6.293239850429793947, -0.1054838202379469042, -2.118119863012501991 ) ) ;
#188601 = CARTESIAN_POINT ( 'NONE',  ( 7.633404179693907388, 8.864391950186421454, -1.199719254218441611 ) ) ;
#188602 = CARTESIAN_POINT ( 'NONE',  ( 5.983225862332436584, 5.874851682342960402, 0.7998128361456341429 ) ) ;
#188603 = CARTESIAN_POINT ( 'NONE',  ( 0.5023040531197673353, 1.956348610274569744, 0.1481081594910879096 ) ) ;
#188604 = CARTESIAN_POINT ( 'NONE',  ( 6.844216539294127877, -8.074889850123396329, -6.588752024304540988 ) ) ;
#188605 = CARTESIAN_POINT ( 'NONE',  ( 4.333802657862601215, 8.207853534148366492, 0.7998128361456462443 ) ) ;
#188606 = CYLINDRICAL_SURFACE ( 'NONE', #113158, 0.07999999999999993228 ) ;
#188607 = VERTEX_POINT ( 'NONE', #96227 ) ;
#188608 = ORIENTED_EDGE ( 'NONE', *, *, #9331, .T. ) ;
#188609 = CARTESIAN_POINT ( 'NONE',  ( 2.894932696777189118, -0.1353093493836102779, -1.806485987321084341 ) ) ;
#188610 = CIRCLE ( 'NONE', #26103, 0.07999999999999998779 ) ;
#188611 = EDGE_LOOP ( 'NONE', ( #183878, #73253, #115117, #57518 ) ) ;
#188612 = CARTESIAN_POINT ( 'NONE',  ( 8.367353357928214663, 12.91366268422496688, 1.040834085586084257E-14 ) ) ;
#188613 = CARTESIAN_POINT ( 'NONE',  ( 3.386504508363381571, 7.172948703057747011, -0.7998128361456362523 ) ) ;
#188614 = CARTESIAN_POINT ( 'NONE',  ( 3.422321195131371674, -0.7368491698513750521, -1.655029553552778809 ) ) ;
#188615 = CARTESIAN_POINT ( 'NONE',  ( 7.200788982189461507, 8.533913579710086239, -1.082531754730548412 ) ) ;
#188616 =( NAMED_UNIT ( * ) SI_UNIT ( $, .STERADIAN. ) SOLID_ANGLE_UNIT ( ) );
#188617 = CARTESIAN_POINT ( 'NONE',  ( 5.881923755780003482, 5.983360633994940336, 0.1790317558759656202 ) ) ;
#188619 = CARTESIAN_POINT ( 'NONE',  ( -1.364683531250010295, 14.38020833367473372, 0.7879004041258445001 ) ) ;
#188618 = CARTESIAN_POINT ( 'NONE',  ( 5.178104514100493994, -0.9952990805809349695, -1.572330789729664779 ) ) ;
#188620 = CARTESIAN_POINT ( 'NONE',  ( 2.741684679331716890, 1.906140283219289966, -0.1903247725174895544 ) ) ;
#188621 = CARTESIAN_POINT ( 'NONE',  ( 1.342497868159111984, 0.3520595052693386018, 1.791136884925909056 ) ) ;
#188622 = DIRECTION ( 'NONE',  ( -1.000000000000000000, 1.016547956922408957E-15, 1.479114432388267300E-31 ) ) ;
#188623 = CARTESIAN_POINT ( 'NONE',  ( -10.60630588279735242, 5.715763139788331948, 4.896273837757428637 ) ) ;
#188624 = AXIS2_PLACEMENT_3D ( 'NONE', #23683, #61523, #89794 ) ;
#188625 = CARTESIAN_POINT ( 'NONE',  ( 5.015976829175539109, 7.901154160799176651, 1.084432410706299477 ) ) ;
#188626 = CARTESIAN_POINT ( 'NONE',  ( -11.49966000274969602, 9.857671544352443860, 3.429881629453267244 ) ) ;
#188627 = DIRECTION ( 'NONE',  ( 0.000000000000000000, 1.000000000000000000, 0.000000000000000000 ) ) ;
#188628 = DIRECTION ( 'NONE',  ( -0.7806247334443685570, 0.000000000000000000, -0.6250000204279265725 ) ) ;
#188629 = CARTESIAN_POINT ( 'NONE',  ( 7.971831135155394321, 8.402817200543854170, -0.7216878364870267237 ) ) ;
#188630 = CARTESIAN_POINT ( 'NONE',  ( -3.632695093457760649, 6.325562478087638496, -1.199719254218452047 ) ) ;
#188631 = AXIS2_PLACEMENT_3D ( 'NONE', #179369, #97066, #163119 ) ;
#188632 = CARTESIAN_POINT ( 'NONE',  ( 1.359446872921949101, 2.059443214669457234, -0.3588360909314599612 ) ) ;
#188633 = CARTESIAN_POINT ( 'NONE',  ( 0.2701547006425785713, -1.196777392914155635, 1.378664180083796875 ) ) ;
#188634 = CARTESIAN_POINT ( 'NONE',  ( -4.543954038874438162, 8.453030145328826350, 1.040834085586084257E-14 ) ) ;
#188635 = EDGE_CURVE ( 'NONE', #166237, #147669, #63700, .T. ) ;
#188636 = CARTESIAN_POINT ( 'NONE',  ( 1.922601709848625440, 1.702220721529534853, 0.6601445126475160574 ) ) ;
#188637 = CARTESIAN_POINT ( 'NONE',  ( 3.387540773601561916, 1.995160029947869340, -0.9435142334218297178 ) ) ;
#188638 = CARTESIAN_POINT ( 'NONE',  ( -3.294361253650757604, -0.1042918288308124219, 0.000000000000000000 ) ) ;
#188639 = CARTESIAN_POINT ( 'NONE',  ( 1.002048865836258518, -0.8573748960705518396, 1.709468765625526521 ) ) ;
#188640 = CARTESIAN_POINT ( 'NONE',  ( 1.170285302187854981, -0.8824026946198880728, -1.760880109839728647 ) ) ;
#188641 = CARTESIAN_POINT ( 'NONE',  ( 3.544416897000971289, -1.586007893901800969, 1.120530928797113246 ) ) ;
#188642 = EDGE_LOOP ( 'NONE', ( #14790, #7784, #176915, #59564 ) ) ;
#188643 = LINE ( 'NONE', #20785, #19312 ) ;
#188645 = CARTESIAN_POINT ( 'NONE',  ( 6.860206125033806224, -1.860540838789390694, 0.04523802485481390190 ) ) ;
#188644 = CARTESIAN_POINT ( 'NONE',  ( -4.034433228518296666, 6.864533312316751790, -1.199719254218450271 ) ) ;
#188646 = CARTESIAN_POINT ( 'NONE',  ( 5.411639590510088027, 6.342609606130419131, -1.199719254218452047 ) ) ;
#188647 = CARTESIAN_POINT ( 'NONE',  ( 0.1738264060025629942, -9.190401220100138602, -9.624818503329224839 ) ) ;
#188648 = CARTESIAN_POINT ( 'NONE',  ( 10.26082332744404368, 10.86538205830655279, -0.7998128361456281477 ) ) ;
#188649 = CARTESIAN_POINT ( 'NONE',  ( -6.798487682609798632, 6.896266815991691779, 0.7998128361456341429 ) ) ;
#188650 = CARTESIAN_POINT ( 'NONE',  ( 2.700927432832851860, 1.852951201923001223, 1.169960570980829839 ) ) ;
#188651 = CARTESIAN_POINT ( 'NONE',  ( 4.202664430556261266, 4.005456045178151570, 0.7216878364870317197 ) ) ;
#188652 = CARTESIAN_POINT ( 'NONE',  ( 6.526270840131753737, 8.707344961610770540, -1.599625672291283607 ) ) ;
#188653 = DIRECTION ( 'NONE',  ( -1.124869321039521280E-29, -7.437565543542506798E-15, 1.000000000000000000 ) ) ;
#188655 = CARTESIAN_POINT ( 'NONE',  ( 5.999232488047272049, -0.2420365156972601739, 2.001857322483958423 ) ) ;
#188654 = CARTESIAN_POINT ( 'NONE',  ( 3.914527900857078357, 1.289819402409349669, -1.292354223553587644 ) ) ;
#188656 = DIRECTION ( 'NONE',  ( 1.000000000000000000, 0.000000000000000000, 0.000000000000000000 ) ) ;
#188657 = CARTESIAN_POINT ( 'NONE',  ( -10.48008955368359629, 11.32911868882677986, 1.040834085586084257E-14 ) ) ;
#188658 = B_SPLINE_CURVE_WITH_KNOTS ( 'NONE', 3,
 ( #188397, #40033, #19492, #106145, #172169, #68231 ),
 .UNSPECIFIED., .F., .F.,
 ( 4, 2, 4 ),
 ( 0.000000000000000000, 0.01245272936456226325, 0.02490545872912452649 ),
 .UNSPECIFIED. ) ;
#188659 = CARTESIAN_POINT ( 'NONE',  ( -5.435611771797328906, 7.629049766310559200, 1.344574814272103236 ) ) ;
#188660 = CARTESIAN_POINT ( 'NONE',  ( 0.000000000000000000, 6.999999999999999112, -9.999999999999998224 ) ) ;
#188661 = CARTESIAN_POINT ( 'NONE',  ( 4.311305935566238645, -0.3199438451688824125, 1.842931056080451935 ) ) ;
#188662 = CARTESIAN_POINT ( 'NONE',  ( 9.562578416340237197, 10.05076299535211781, 0.7998128361456462443 ) ) ;
#188663 = CARTESIAN_POINT ( 'NONE',  ( 2.508321089405711746, -0.7374124507862482858, -1.779973396525496909 ) ) ;
#188664 = CARTESIAN_POINT ( 'NONE',  ( 6.508651776674191147, 0.6122461511635870490, 1.863871573545019755 ) ) ;
#188665 = CARTESIAN_POINT ( 'NONE',  ( 1.500000000000001332, 14.62500000000000000, 0.000000000000000000 ) ) ;
#188666 = CARTESIAN_POINT ( 'NONE',  ( -5.225778143063529946, 8.184159369294361497, 1.199719254218452047 ) ) ;
#188667 = CARTESIAN_POINT ( 'NONE',  ( 5.118366684358879759, 5.930181538962194132, 1.199719254218462483 ) ) ;
#188668 = EDGE_CURVE ( 'NONE', #151327, #81332, #154803, .T. ) ;
#188669 = CARTESIAN_POINT ( 'NONE',  ( -4.570507181138272479, 7.385989907086349504, 1.082531754730549967 ) ) ;
#188670 = CARTESIAN_POINT ( 'NONE',  ( -0.1408020194050146334, -0.005144001661238749128, -2.100147592658160089 ) ) ;
#188671 = CARTESIAN_POINT ( 'NONE',  ( 9.622536337397022521, 12.24937836509514710, 1.599625672291281386 ) ) ;
#188672 = CARTESIAN_POINT ( 'NONE',  ( -4.121315508874280553, 3.910548969882488901, -0.7216878364870207285 ) ) ;
#188673 = CARTESIAN_POINT ( 'NONE',  ( 5.155165671438199482, 1.724248240607465732, -1.145533019084030268 ) ) ;
#188675 = CARTESIAN_POINT ( 'NONE',  ( -1.364683531250012516, 3.092708333674755838, 0.7879004041258379498 ) ) ;
#188674 = CARTESIAN_POINT ( 'NONE',  ( -0.09456490281532430042, -0.7861721075429689565, -1.663503389917226460 ) ) ;
#188676 = CARTESIAN_POINT ( 'NONE',  ( 4.922631952865072158, -1.624392127635465144, -1.626674183726722678 ) ) ;
#188677 = CARTESIAN_POINT ( 'NONE',  ( 5.327991180490514012, 9.159814110640187579, 1.040834085586084257E-14 ) ) ;
#188679 = DIRECTION ( 'NONE',  ( 0.1669130127894903892, -0.9056625952363863696, -0.3897631457067597394 ) ) ;
#188678 = CARTESIAN_POINT ( 'NONE',  ( 4.909461021924240498, 7.781436054670031410, 1.082531754730549078 ) ) ;
#188680 = CARTESIAN_POINT ( 'NONE',  ( 0.7270408775228944798, 0.1741418271693234987, 2.285704298519490862 ) ) ;
#188681 = CARTESIAN_POINT ( 'NONE',  ( 1.124100812432970948E-16, 3.500000000000003109, -2.025000000000006573 ) ) ;
#188682 = CARTESIAN_POINT ( 'NONE',  ( -5.413448473606448985, 9.537716662508005427, 0.000000000000000000 ) ) ;
#188683 = CARTESIAN_POINT ( 'NONE',  ( 4.769442245286214188, 1.119358777157190010, 1.586704836592154333 ) ) ;
#188684 = VERTEX_POINT ( 'NONE', #63967 ) ;
#188685 = CARTESIAN_POINT ( 'NONE',  ( 8.636180661780656465, 11.09863007687603087, -1.443375672974052559 ) ) ;
#188686 = ORIENTED_EDGE ( 'NONE', *, *, #33483, .F. ) ;
#188687 = CARTESIAN_POINT ( 'NONE',  ( 6.539320575229249144, 0.007148032025052972194, 1.896977914940492393 ) ) ;
#188688 = CARTESIAN_POINT ( 'NONE',  ( 1.101696929656799995, -1.725068445828933594, -0.003817819714259720019 ) ) ;
#188689 = CARTESIAN_POINT ( 'NONE',  ( 5.946499988598237252, -1.422611626450220434, 1.429444749906971790 ) ) ;
#188691 = FILL_AREA_STYLE_COLOUR ( '', #126348 ) ;
#188690 = CARTESIAN_POINT ( 'NONE',  ( -7.994504133552415404, 12.47867192245318435, -0.7998128361456281477 ) ) ;
#188692 = CARTESIAN_POINT ( 'NONE',  ( -3.285556943749998737, -1.567708332855375142, 1.896917185911908499 ) ) ;
#188694 = CARTESIAN_POINT ( 'NONE',  ( 1.779799802231885275, -0.9501279348179264561, 1.492983415055911367 ) ) ;
#188693 = CARTESIAN_POINT ( 'NONE',  ( 2.343796043118621775, 2.090200655756014658, 0.05028463699395351039 ) ) ;
#188695 = DIRECTION ( 'NONE',  ( 1.276756478318932585E-15, -1.000000000000000000, 1.665334536937738262E-16 ) ) ;
#188697 = CARTESIAN_POINT ( 'NONE',  ( 3.908379099077957886, 1.621946506101832775, -1.620046465671644675 ) ) ;
#188696 = DIRECTION ( 'NONE',  ( 0.000000000000000000, 0.000000000000000000, -1.000000000000000000 ) ) ;
#188698 = CARTESIAN_POINT ( 'NONE',  ( 2.378492463385312394, 1.591508763844831531, -0.7045900751257595518 ) ) ;
#188699 = CARTESIAN_POINT ( 'NONE',  ( 2.693266070609028784, 6.293894182352508970, 0.000000000000000000 ) ) ;
#188700 = CARTESIAN_POINT ( 'NONE',  ( 6.574778147984297938, 6.635272358928617109, -0.7998128361456481317 ) ) ;
#188701 = CARTESIAN_POINT ( 'NONE',  ( 2.354500945691032410, -0.7452406562851380256, 1.565668601905329638 ) ) ;
#188702 = CARTESIAN_POINT ( 'NONE',  ( -3.555477883677943599E-14, 2.484375000341469963, 1.570758158831768281 ) ) ;
#188703 = CARTESIAN_POINT ( 'NONE',  ( 1.363465259770980209, -0.4569337200135030197, 1.803945581614458282 ) ) ;
#188704 = CARTESIAN_POINT ( 'NONE',  ( 1.944024895830529731, 1.496304202470769340, 1.573470141065239414 ) ) ;
#188705 = CARTESIAN_POINT ( 'NONE',  ( 3.974511587100456822, 7.788680618259193444, 1.040834085586084257E-14 ) ) ;
#188706 = CARTESIAN_POINT ( 'NONE',  ( 3.221888912838869690, 0.9023448338944944913, -1.803416113280359445 ) ) ;
#188707 = CARTESIAN_POINT ( 'NONE',  ( 2.781250000000002665, 0.7852924748301273183, 1.895863743164028170 ) ) ;
#188708 = CARTESIAN_POINT ( 'NONE',  ( 1.499999999999989120, 2.535416667349483344, 0.8660254037844524744 ) ) ;
#188709 = CARTESIAN_POINT ( 'NONE',  ( 1.026247228566424363, 1.149774913616221417, -1.545494133055951069 ) ) ;
#188710 = CARTESIAN_POINT ( 'NONE',  ( -1.402160292154681736E-14, 14.92187500034139980, 1.575800808251682339 ) ) ;
#188711 = CARTESIAN_POINT ( 'NONE',  ( 4.271885190509593144, 0.4847678284230126922, -2.167736239397171083 ) ) ;
#188712 = VERTEX_POINT ( 'NONE', #211269 ) ;
#188713 = CARTESIAN_POINT ( 'NONE',  ( 0.3282377607281151133, 2.386164550367423587, 1.224999999999977440 ) ) ;
#188714 = CARTESIAN_POINT ( 'NONE',  ( 1.499999999999985123, -0.2041666666666457353, -0.8660254037844323793 ) ) ;
#188715 = CARTESIAN_POINT ( 'NONE',  ( 7.949158136313996259, 8.168439335321471262, 1.040834085586084257E-14 ) ) ;
#188716 = CARTESIAN_POINT ( 'NONE',  ( 1.364683531249986537, -0.3864583329919166199, 0.7879004041258500513 ) ) ;
#188717 = CARTESIAN_POINT ( 'NONE',  ( 0.4170203200158085211, -0.7540967040414385814, -2.089506846138278195 ) ) ;
#188718 = CARTESIAN_POINT ( 'NONE',  ( 4.844172697165038066, -0.9265620464425131653, 1.729294158640543477 ) ) ;
#188719 = CARTESIAN_POINT ( 'NONE',  ( 8.256552361042350796, 12.57646882128404187, 1.040834085586084257E-14 ) ) ;
#188720 = CARTESIAN_POINT ( 'NONE',  ( -1.264548378739724699, 3.911400545389569050, -0.5006372017796719698 ) ) ;
#188721 = CARTESIAN_POINT ( 'NONE',  ( 5.413438844936455219, -0.3396298981525199823, 2.236681904191807568 ) ) ;
#188722 = CARTESIAN_POINT ( 'NONE',  ( -5.153507786970267013, 8.066157280557016307, -1.082531754730549967 ) ) ;
#188723 = CARTESIAN_POINT ( 'NONE',  ( 2.875492298462109630, -0.2048798925258775439, 2.052495523891383566 ) ) ;
#188724 = CARTESIAN_POINT ( 'NONE',  ( -6.891622154448065807, 6.934647356477856128, 1.040834085586084257E-14 ) ) ;
#188725 = AXIS2_PLACEMENT_3D ( 'NONE', #160449, #211316, #12056 ) ;
#188726 = CARTESIAN_POINT ( 'NONE',  ( -1.500000000000013101, 2.202083334016153859, 0.8660254037844403729 ) ) ;
#188727 = CARTESIAN_POINT ( 'NONE',  ( 1.364683531249988535, 5.717708333674752730, -0.7879004041258300672 ) ) ;
#188728 = CARTESIAN_POINT ( 'NONE',  ( 4.464026755505964950, 0.8799173153972823513, 1.650629236088823282 ) ) ;
#188729 = CARTESIAN_POINT ( 'NONE',  ( 3.252318870217449920, 1.690988760736945373, -0.3835568649490900817 ) ) ;
#188730 = CARTESIAN_POINT ( 'NONE',  ( 3.895860127252141591, -0.5505607855701463160, -1.651121638195630181 ) ) ;
#188731 = CARTESIAN_POINT ( 'NONE',  ( 1.083963445724302588, -1.025016635393001252, 2.050507297876194901 ) ) ;
#188732 = CARTESIAN_POINT ( 'NONE',  ( 1.413402608508182556, 1.946665536341249503, 1.039416302365432587 ) ) ;
#188733 = CARTESIAN_POINT ( 'NONE',  ( 4.528904929885309905, -1.910896387970087096, 0.8487916243252179305 ) ) ;
#188734 = CARTESIAN_POINT ( 'NONE',  ( 5.578056150152780113, -1.895089194937165100, -0.4233685073328739557 ) ) ;
#188735 = EDGE_CURVE ( 'NONE', #183890, #203895, #192566, .T. ) ;
#188736 = FACE_OUTER_BOUND ( 'NONE', #15026, .T. ) ;
#188737 = CARTESIAN_POINT ( 'NONE',  ( 0.9146856577476671912, -1.281363086869342194, -1.556907195799726917 ) ) ;
#188738 = CARTESIAN_POINT ( 'NONE',  ( 0.7035762090183244055, 1.867434778015097940, -1.004864118554361863 ) ) ;
#188739 =( NAMED_UNIT ( * ) PLANE_ANGLE_UNIT ( ) SI_UNIT ( $, .RADIAN. ) );
#188740 = CARTESIAN_POINT ( 'NONE',  ( -8.533967624797991647, 12.04371376465130439, -1.199719254218446718 ) ) ;
#188741 = CARTESIAN_POINT ( 'NONE',  ( 6.120616281565444794, 9.228137197546649517, -1.199719254218440723 ) ) ;
#188742 = CARTESIAN_POINT ( 'NONE',  ( 0.000000000000000000, 5.000000000000000888, 0.000000000000000000 ) ) ;
#188743 = CARTESIAN_POINT ( 'NONE',  ( 3.967279163243800255, 0.2216459979678051528, -1.812115712870238537 ) ) ;
#188744 = EDGE_LOOP ( 'NONE', ( #29273, #106868, #161072, #9046 ) ) ;
#188745 = CARTESIAN_POINT ( 'NONE',  ( -7.445362632559989535, 8.715286488521982733, 1.199719254218452047 ) ) ;
#188746 = CARTESIAN_POINT ( 'NONE',  ( -3.383641855062333281, 6.105276709951447778, -1.199719254218452047 ) ) ;
#188747 = CARTESIAN_POINT ( 'NONE',  ( 1.642778471875001811, -1.830208332855375097, 2.845375778867859751 ) ) ;
#188748 = CARTESIAN_POINT ( 'NONE',  ( -7.640183256500752584, 8.872300873127729304, -1.199719254218446718 ) ) ;
#188749 = CARTESIAN_POINT ( 'NONE',  ( 2.127218876063118103, 1.806125448131710387, 0.9042179360667053079 ) ) ;
#188750 = CARTESIAN_POINT ( 'NONE',  ( 5.385833121705805304, 1.478444731487274399, 1.638484004604986000 ) ) ;
#188751 = CARTESIAN_POINT ( 'NONE',  ( -5.469788628470539926, 5.346117919495872783, -0.7998128361456362523 ) ) ;
#188752 = CARTESIAN_POINT ( 'NONE',  ( 2.711566728334329213, 0.5015729494155155566, -1.791976956261555953 ) ) ;
#188753 = CARTESIAN_POINT ( 'NONE',  ( 3.623053363349855172, 5.249981562040033189, 1.599625672291267398 ) ) ;
#188754 = DIRECTION ( 'NONE',  ( 0.000000000000000000, -0.5005768354468324022, 0.8656921114426507913 ) ) ;
#188755 = VERTEX_POINT ( 'NONE', #81287 ) ;
#188756 = CARTESIAN_POINT ( 'NONE',  ( -5.739179097286464248, 5.590130456455974617, -0.7998128361456221525 ) ) ;
#188757 = CARTESIAN_POINT ( 'NONE',  ( -9.833741488613570780, 10.36711991300432345, 0.7998128361456462443 ) ) ;
#188758 = CARTESIAN_POINT ( 'NONE',  ( 5.092344371507952161, -1.812320225013038133, -0.2200062734805732223 ) ) ;
#188759 = CIRCLE ( 'NONE', #36602, 0.08000000000000020983 ) ;
#188761 = CARTESIAN_POINT ( 'NONE',  ( -4.028535363944735437, 7.777154369360758324, -0.5044922354892691363 ) ) ;
#188760 = CARTESIAN_POINT ( 'NONE',  ( -5.901542003698421190, 10.10715911428198055, 0.000000000000000000 ) ) ;
#188762 = CARTESIAN_POINT ( 'NONE',  ( 5.991454128980707949, 7.190850779781567503, -1.201235417510186254 ) ) ;
#188763 = CARTESIAN_POINT ( 'NONE',  ( 0.1570416503036062006, -0.3615154868755916517, -1.700924732364687220 ) ) ;
#188764 = CARTESIAN_POINT ( 'NONE',  ( 0.2337849711155593480, 0.2922425735506446465, 1.715447441342861534 ) ) ;
#188765 = CARTESIAN_POINT ( 'NONE',  ( 5.936188932989287181, 1.142819166849334378, -2.004778302753240649 ) ) ;
#188766 = CARTESIAN_POINT ( 'NONE',  ( 4.583538449871731757, 7.505156070562471804, 1.199719254218451159 ) ) ;
#188767 = CARTESIAN_POINT ( 'NONE',  ( 0.3333698182165916735, -1.885181130612986866, 0.8328085122516776240 ) ) ;
#188768 = CARTESIAN_POINT ( 'NONE',  ( 6.844168616800228477, 6.879284895888727824, -0.7998128361456281477 ) ) ;
#188769 = CARTESIAN_POINT ( 'NONE',  ( 5.712396407272276377, -1.806953704233695612, -1.420304717212710122 ) ) ;
#188770 = CARTESIAN_POINT ( 'NONE',  ( 4.226925616482873238, 3.500738074553327639, 2.444828727306146199 ) ) ;
#188771 = CARTESIAN_POINT ( 'NONE',  ( -4.925354943514475003, 8.968274210734028529, 0.000000000000000000 ) ) ;
#188772 = CARTESIAN_POINT ( 'NONE',  ( 5.770339134078734666, -1.185559297855027561, 1.446973003893243348 ) ) ;
#188773 = AXIS2_PLACEMENT_3D ( 'NONE', #3953, #71093, #184851 ) ;
#188776 = EDGE_CURVE ( 'NONE', #126977, #149611, #53589, .T. ) ;
#188775 = CARTESIAN_POINT ( 'NONE',  ( -5.632486471834530661, 5.535932070087196344, -0.7998128361456362523 ) ) ;
#188774 = CARTESIAN_POINT ( 'NONE',  ( 3.216961742616857745, 1.504763323797538410, -1.180078671740567131 ) ) ;
#188777 = CARTESIAN_POINT ( 'NONE',  ( 5.479209177496175087, -0.05098606815037013545, -2.206463706674952618 ) ) ;
#188778 = CARTESIAN_POINT ( 'NONE',  ( 5.155504860159462410, 2.039786097693491396, -0.5674642188294597434 ) ) ;
#188779 = CARTESIAN_POINT ( 'NONE',  ( 0.6124999999999914957, 0.2291666673494702211, -1.060881119635965764 ) ) ;
#188780 = CARTESIAN_POINT ( 'NONE',  ( -10.72645012907092443, 4.497370833040986504, 5.281782792447082819 ) ) ;
#188781 = CARTESIAN_POINT ( 'NONE',  ( -0.2108831679770961920, 2.882544375557041239, -2.385815782126240236 ) ) ;
#188782 = CARTESIAN_POINT ( 'NONE',  ( 5.411112705185558092, 6.445957923205511086, -1.082531754730548412 ) ) ;
#188783 = AXIS2_PLACEMENT_3D ( 'NONE', #114177, #213696, #52299 ) ;
#188784 = CARTESIAN_POINT ( 'NONE',  ( -3.784134271545645412, 7.428924060196286483, 0.7216878364870338292 ) ) ;
#188785 = CARTESIAN_POINT ( 'NONE',  ( 5.531924462405465981, -2.068776410037334479, 0.4646945096876684556 ) ) ;
#188786 = EDGE_CURVE ( 'NONE', #24495, #198714, #48794, .T. ) ;
#188787 = CARTESIAN_POINT ( 'NONE',  ( 2.028779783278670035, 1.327905328797769569, -1.887045328260747112 ) ) ;
#188788 = CARTESIAN_POINT ( 'NONE',  ( 3.226955236329264398, -1.811681696138227160, -0.7532884077038404236 ) ) ;
#188789 = SURFACE_STYLE_USAGE ( .BOTH. , #141528 ) ;
#188790 = CARTESIAN_POINT ( 'NONE',  ( 6.543808478091840186, 1.418056970388498206, 1.498012503012560170 ) ) ;
#188791 = CARTESIAN_POINT ( 'NONE',  ( 3.714570900464278846, 5.356752022006865843, 1.443375672974062551 ) ) ;
#188792 = CARTESIAN_POINT ( 'NONE',  ( 5.225741863424510747, 5.061396693608882558, 0.7998128361456352531 ) ) ;
#188793 = ORIENTED_EDGE ( 'NONE', *, *, #120455, .T. ) ;
#188794 = CARTESIAN_POINT ( 'NONE',  ( 5.471888747823221877, -0.9023485654677811940, 1.803414228490702209 ) ) ;
#188795 = CARTESIAN_POINT ( 'NONE',  ( -10.14557902172788495, 10.73093036830436553, 1.040834085586084257E-14 ) ) ;
#188796 =( LENGTH_UNIT ( ) NAMED_UNIT ( * ) SI_UNIT ( .MILLI., .METRE. ) );
#188797 = CARTESIAN_POINT ( 'NONE',  ( -0.1408020194049780516, -0.005144001661201014555, -2.100147592658160089 ) ) ;
#188798 = CARTESIAN_POINT ( 'NONE',  ( 1.956167536658510953, -0.7342896127641992399, 2.043222018709658805 ) ) ;
#188799 = DIRECTION ( 'NONE',  ( 0.000000000000000000, 0.000000000000000000, -1.000000000000000000 ) ) ;
#188800 = CARTESIAN_POINT ( 'NONE',  ( 0.9320672075895162223, -2.067649466203642206, 0.4702014512557165515 ) ) ;
#188801 = CARTESIAN_POINT ( 'NONE',  ( -1.499999999999997780, 2.181250000682817713, 1.214306433183764966E-14 ) ) ;
#188802 = CARTESIAN_POINT ( 'NONE',  ( -8.135612300829253130, 14.55183989155882784, -8.805242580674113029 ) ) ;
#188804 = CARTESIAN_POINT ( 'NONE',  ( -8.280982047128215839, -6.442483420143127582, 7.626074736120322051 ) ) ;
#188803 = B_SPLINE_CURVE_WITH_KNOTS ( 'NONE', 3,
 ( #137628, #20634, #37979, #69381, #166919, #135489, #86723 ),
 .UNSPECIFIED., .F., .F.,
 ( 4, 3, 4 ),
 ( 0.0001126021369358736141, 0.001495765174703651314, 0.002006790696433096571 ),
 .UNSPECIFIED. ) ;
#188805 = CARTESIAN_POINT ( 'NONE',  ( 4.930145672075521013, 8.107674077938057167, 1.051636801887654293 ) ) ;
#188806 = CARTESIAN_POINT ( 'NONE',  ( 1.054063116485728813, 2.058546115662110765, -0.09824037785954514712 ) ) ;
#188808 = CARTESIAN_POINT ( 'NONE',  ( 4.332146500830024394, 3.995600397316412700, 0.09403405272452491914 ) ) ;
#188807 = CARTESIAN_POINT ( 'NONE',  ( -9.073431116043565225, 11.60875560684942265, -1.599625672291263179 ) ) ;
#188809 = CARTESIAN_POINT ( 'NONE',  ( -1.364683531250000748, 0.7593750003414210248, 0.000000000000000000 ) ) ;
#188810 = DIRECTION ( 'NONE',  ( -0.8660254037844433705, 0.000000000000000000, -0.4999999999999917843 ) ) ;
#188811 = ORIENTED_EDGE ( 'NONE', *, *, #115920, .F. ) ;
#188812 = EDGE_CURVE ( 'NONE', #74995, #50845, #95065, .T. ) ;
#188813 = CARTESIAN_POINT ( 'NONE',  ( 3.475170734053119048, -1.687717282722025924, -0.8990902037325496643 ) ) ;
#188814 = CARTESIAN_POINT ( 'NONE',  ( 5.014393912088591421, 1.219005865285277546, -1.283338120600298726 ) ) ;
#188815 = CARTESIAN_POINT ( 'NONE',  ( 4.701645408888975197, 8.707279753670952971, 0.000000000000000000 ) ) ;
#188816 = CARTESIAN_POINT ( 'NONE',  ( -3.469997250093771246, 6.135748327496311383, -1.199719254218452935 ) ) ;
#188817 = CARTESIAN_POINT ( 'NONE',  ( 0.5272532902790193488, -0.2650996996472804734, 1.791917353721095285 ) ) ;
#188819 = CARTESIAN_POINT ( 'NONE',  ( 6.151949797202925119, 0.9892698599738621867, 1.640257924793379063 ) ) ;
#188818 = CARTESIAN_POINT ( 'NONE',  ( -6.773846765317315999, -7.246166700180828535, 6.773846765317339091 ) ) ;
#188820 = CARTESIAN_POINT ( 'NONE',  ( 1.363825363374836286, -0.5049007678423790280, 2.007717453658082629 ) ) ;
#188821 = CARTESIAN_POINT ( 'NONE',  ( 0.6823417656249882723, -0.3447916663252489911, 1.181850606188755259 ) ) ;
#188822 = CARTESIAN_POINT ( 'NONE',  ( 5.752782329262380756, -1.473788443143897675, 1.151991621687727507 ) ) ;
#188823 = CARTESIAN_POINT ( 'NONE',  ( 2.279681363911123970, 1.122676072794186908, 1.439608767588994365 ) ) ;
#188825 = CARTESIAN_POINT ( 'NONE',  ( 6.137634773950260580, 6.983624353001562923, 0.9378011681944794509 ) ) ;
#188824 = CARTESIAN_POINT ( 'NONE',  ( 5.901041445831936016, 1.806360628843254768, -1.267562117129708232 ) ) ;
#188826 = CARTESIAN_POINT ( 'NONE',  ( -1.364683531250014514, 0.2802083336747505649, 0.7879004041258379498 ) ) ;
#188827 = CARTESIAN_POINT ( 'NONE',  ( 4.387212324874685265, 0.09821595252585722802, 2.060445151624993976 ) ) ;
#188828 = CARTESIAN_POINT ( 'NONE',  ( -6.852756576703439961, 10.08230087520760954, 1.199719254218453823 ) ) ;
#188829 = CARTESIAN_POINT ( 'NONE',  ( 8.914649696185335870, 10.35917838609310593, -1.199719254218446718 ) ) ;
#188830 = CARTESIAN_POINT ( 'NONE',  ( 3.897079088924235712, 6.634010472798538949, 1.199719254218462483 ) ) ;
#188831 = CARTESIAN_POINT ( 'NONE',  ( 0.3159878724818786511, -2.119942686789745068, 0.4214050671751194410 ) ) ;
#188832 = CARTESIAN_POINT ( 'NONE',  ( 6.461392557816405535, 1.719054114842766268, 1.153505076091146053 ) ) ;
#188833 = CARTESIAN_POINT ( 'NONE',  ( 0.6823417656249882723, -0.3447916663252489911, 1.181850606188755259 ) ) ;
#188834 = CARTESIAN_POINT ( 'NONE',  ( 3.462350783624254191, 0.9684823049558517472, 1.932541222812742987 ) ) ;
#188836 = CARTESIAN_POINT ( 'NONE',  ( 2.611707774152134842, 0.5260268489151798121, -1.889944157703125072 ) ) ;
#188835 = CARTESIAN_POINT ( 'NONE',  ( 4.108072977939541737, -0.7709450260172491243, 1.866947522544240901 ) ) ;
#188837 = DIRECTION ( 'NONE',  ( 0.000000000000000000, 0.000000000000000000, -1.000000000000000000 ) ) ;
#188840 = CARTESIAN_POINT ( 'NONE',  ( 6.155038550924139429, 9.164333495178082600, 1.082531754730558626 ) ) ;
#188839 = CARTESIAN_POINT ( 'NONE',  ( 0.000000000000000000, -4.046874999522043659, -3.793834371823813001 ) ) ;
#188838 = DIRECTION ( 'NONE',  ( -0.1652856342098213693, 0.9636458296411444246, -0.2099223050061321261 ) ) ;
#188841 = CARTESIAN_POINT ( 'NONE',  ( -7.119966945832006289, 8.335658187339330283, 1.199719254218452047 ) ) ;
#188842 = CARTESIAN_POINT ( 'NONE',  ( 2.237517880698642880, 0.5331670712399002587, -1.944730990508992008 ) ) ;
#188844 = FACE_OUTER_BOUND ( 'NONE', #82196, .T. ) ;
#188843 = CARTESIAN_POINT ( 'NONE',  ( -3.958090780185743451, 6.705190779270287393, -1.199719254218452047 ) ) ;
#188845 = CARTESIAN_POINT ( 'NONE',  ( 1.499999999999991118, 5.535416667349481123, 0.8660254037844524744 ) ) ;
#188846 = CARTESIAN_POINT ( 'NONE',  ( 6.011958326525193463, -0.6379227081053112647, 1.803018720113582996 ) ) ;
#188847 = CARTESIAN_POINT ( 'NONE',  ( -3.986493660556410745, 7.309144847462942352, 0.7296485550502177508 ) ) ;
#188848 = CARTESIAN_POINT ( 'NONE',  ( 6.290620086616457662, 6.441404310581745563, 1.040834085586084257E-14 ) ) ;
#188850 = CARTESIAN_POINT ( 'NONE',  ( 3.884388800492278193, -0.6352171928143932611, -1.913798906059568594 ) ) ;
#188849 = CARTESIAN_POINT ( 'NONE',  ( -7.334597914868727919, 10.54048608644677465, -1.082531754730543083 ) ) ;
#188851 = CARTESIAN_POINT ( 'NONE',  ( -0.7499999999999972244, 3.858333333333359594, -1.299038105676652011 ) ) ;
#188852 = CARTESIAN_POINT ( 'NONE',  ( -0.6823417656250003738, 14.46354166700806410, 1.181850606188754593 ) ) ;
#188853 = CARTESIAN_POINT ( 'NONE',  ( 6.721745554788610022, -1.671375598274482677, 0.4255071719459716517 ) ) ;
#188854 = CARTESIAN_POINT ( 'NONE',  ( 5.365994935958575240, 9.482354201918870018, 0.7998128361456341429 ) ) ;
#188855 = CARTESIAN_POINT ( 'NONE',  ( 9.083599731475983319, 11.62061899152058686, 1.443375672974076540 ) ) ;
#188856 = CARTESIAN_POINT ( 'NONE',  ( -0.3000000000000344058, 3.322650755865458994, 0.5865692111442272205 ) ) ;
#188857 = CARTESIAN_POINT ( 'NONE',  ( 4.393722961847310593, -0.7179090532695198146, 1.727491627791829742 ) ) ;
#188858 = CARTESIAN_POINT ( 'NONE',  ( -0.1288028175206907822, -0.008968661790493270836, -2.273875003271644157 ) ) ;
#188859 = CARTESIAN_POINT ( 'NONE',  ( 1.762639944428091576, -0.7413553172891699239, -1.933158369416078770 ) ) ;
#188860 = VERTEX_POINT ( 'NONE', #65014 ) ;
#188861 = CARTESIAN_POINT ( 'NONE',  ( 5.225741863424510747, 5.061396693608882558, 0.7998128361456352531 ) ) ;
#188862 = CARTESIAN_POINT ( 'NONE',  ( 0.9840001696646907270, -2.016598147255070472, 0.002831364411433334727 ) ) ;
#188863 = CARTESIAN_POINT ( 'NONE',  ( -0.2110808730067273986, 0.0005491059566040295322, -1.796958327270286704 ) ) ;
#188864 = CARTESIAN_POINT ( 'NONE',  ( 5.058600711230250013, 5.074324715956299414, -0.7216878364870458196 ) ) ;
#188865 = LINE ( 'NONE', #6890, #66137 ) ;
#188866 = CARTESIAN_POINT ( 'NONE',  ( 8.283668667825342169, 9.726996869626816533, -1.082531754730543083 ) ) ;
#188867 = CARTESIAN_POINT ( 'NONE',  ( 7.293396569147545527, 10.59638086639245280, 1.199719254218460707 ) ) ;
#188869 = CARTESIAN_POINT ( 'NONE',  ( 6.485945863600712791, -1.915068438110486770, 0.05257573307166327897 ) ) ;
#188868 = CARTESIAN_POINT ( 'NONE',  ( -6.392833124043511894, 7.417059051927569868, 1.199719254218450271 ) ) ;
#188870 = CARTESIAN_POINT ( 'NONE',  ( -6.486551268120854807, 6.767445667853342783, -0.2095380678983837508 ) ) ;
#188871 = VECTOR ( 'NONE', #125746, 1000.000000000000000 ) ;
#188872 = CARTESIAN_POINT ( 'NONE',  ( 1.500000000000037748, 8.500000000000000000, 10.64483442802188051 ) ) ;
#188874 = ORIENTED_EDGE ( 'NONE', *, *, #101627, .T. ) ;
#188873 = CARTESIAN_POINT ( 'NONE',  ( 4.419594888374914099, 5.218910793601261311, -1.082531754730548412 ) ) ;
#188875 = CARTESIAN_POINT ( 'NONE',  ( -6.385527162356466668, 10.39360608948380182, 0.000000000000000000 ) ) ;
#188876 = CARTESIAN_POINT ( 'NONE',  ( 2.905317003618158367, 1.825515667692039878, 1.157497049167732550 ) ) ;
#188877 = CARTESIAN_POINT ( 'NONE',  ( -7.105881907338169157, 8.423188659050232729, -1.082531754730549967 ) ) ;
#188878 = CARTESIAN_POINT ( 'NONE',  ( 4.523580528814945545, 5.306540700819438960, 1.199719254218452047 ) ) ;
#188879 = CARTESIAN_POINT ( 'NONE',  ( 0.7738737444688469358, 0.4079195088417564286, -2.080830740624163955 ) ) ;
#188880 = CARTESIAN_POINT ( 'NONE',  ( 6.106453908201667780, -0.6597477751954274883, -1.702385593799011110 ) ) ;
#188881 = CARTESIAN_POINT ( 'NONE',  ( 0.8253839628637716919, -1.873344321310044469, 0.6141440057798281948 ) ) ;
#188882 = CARTESIAN_POINT ( 'NONE',  ( 3.041163856788456687, 0.05134138945498378792, 1.911883771832747048 ) ) ;
#188883 = APPLICATION_CONTEXT ( 'automotive_design' ) ;
#188884 = CARTESIAN_POINT ( 'NONE',  ( -11.44779963594995387, 10.19999999999999041, -3.600000000000078693 ) ) ;
#188885 = CARTESIAN_POINT ( 'NONE',  ( 5.494576857243831824, 1.940090112543988665, 0.3384423684570179724 ) ) ;
#188886 = CARTESIAN_POINT ( 'NONE',  ( 0.1638716437233995460, -1.269140265717118465, 1.469938112931449270 ) ) ;
#188887 = EDGE_LOOP ( 'NONE', ( #19480, #11957, #91578, #178655 ) ) ;
#188888 = CARTESIAN_POINT ( 'NONE',  ( -4.613517410400161722, 8.604463755433990002, -0.7998128361456362523 ) ) ;
#188890 = CARTESIAN_POINT ( 'NONE',  ( 6.082307721193076944, 1.091511717630256673, 1.817998432235830908 ) ) ;
#188889 = CARTESIAN_POINT ( 'NONE',  ( -4.122561227007127016, 6.967349310553715647, 1.199719254218452935 ) ) ;
#188891 = CARTESIAN_POINT ( 'NONE',  ( 5.194182247366861738, 9.073980031987776584, 0.7216878364870317197 ) ) ;
#188893 = ORIENTED_EDGE ( 'NONE', *, *, #195389, .F. ) ;
#188892 = CARTESIAN_POINT ( 'NONE',  ( 5.022078740994724733, -1.902695638548990820, 0.1913334245251183119 ) ) ;
#188894 = CARTESIAN_POINT ( 'NONE',  ( 0.5170026063063514199, 1.520138765826519300, -1.599913083071627273 ) ) ;
#188895 = CARTESIAN_POINT ( 'NONE',  ( 7.720011280421983813, -5.361065518611646041, 7.836017471263537537 ) ) ;
#188896 = CARTESIAN_POINT ( 'NONE',  ( 6.516276865632868898, -2.012592099345715813, 0.05177761937730576691 ) ) ;
#188897 = DIRECTION ( 'NONE',  ( -0.000000000000000000, -0.000000000000000000, -1.000000000000000000 ) ) ;
#188898 = CARTESIAN_POINT ( 'NONE',  ( -0.01716059204523777415, 15.45541796569955650, 11.96980914358345061 ) ) ;
#188899 = CARTESIAN_POINT ( 'NONE',  ( 1.803268859043684058, -1.750145871244257467, 1.105767233283899920 ) ) ;
#188900 = CARTESIAN_POINT ( 'NONE',  ( -7.250913225210214641, 7.353820272367037170, 0.7998128361456341429 ) ) ;
#188901 = STYLED_ITEM ( 'NONE', ( #200306 ), #99019 ) ;
#188902 = CARTESIAN_POINT ( 'NONE',  ( -4.719039639065737646, 8.241789607316443167, 0.6479098462880685805 ) ) ;
#188903 = CARTESIAN_POINT ( 'NONE',  ( 1.024558638192473170, 1.287004556549703693, -1.736669753874709343 ) ) ;
#188904 = CARTESIAN_POINT ( 'NONE',  ( 4.964256800898067645, 8.943383367689749619, 0.7998128361456462443 ) ) ;
#188905 = B_SPLINE_CURVE_WITH_KNOTS ( 'NONE', 3,
 ( #23247, #40608, #155407, #158619, #140260, #123014 ),
 .UNSPECIFIED., .F., .F.,
 ( 4, 2, 4 ),
 ( 0.000000000000000000, 0.0003258677429877275783, 0.0006517354859754551566 ),
 .UNSPECIFIED. ) ;
#188906 = CARTESIAN_POINT ( 'NONE',  ( -10.81324141427316299, 6.418649203030321715, 5.206428076515513759 ) ) ;
#188907 = EDGE_CURVE ( 'NONE', #93282, #109059, #143633, .T. ) ;
#188908 = CARTESIAN_POINT ( 'NONE',  ( 5.397554552016226914, 6.430140077841320689, 1.082531754730549078 ) ) ;
#188909 = DIRECTION ( 'NONE',  ( 8.638326563840814399E-31, 0.000000000000000000, 1.000000000000000000 ) ) ;
#188910 = STYLED_ITEM ( 'NONE', ( #56046 ), #146365 ) ;
#188911 = CARTESIAN_POINT ( 'NONE',  ( 0.1331715793776600543, 0.003733371859311258086, -1.953671397793784736 ) ) ;
#188912 = CARTESIAN_POINT ( 'NONE',  ( 0.6823417656249969321, 12.83854166700806942, -1.181850606188757036 ) ) ;
#188914 = CARTESIAN_POINT ( 'NONE',  ( -7.065734331377342414, 8.272386803808890576, -1.199719254218452047 ) ) ;
#188913 = CARTESIAN_POINT ( 'NONE',  ( 6.925078400183582339, 2.988348447159621113, 2.209593971251204714 ) ) ;
#188915 = EDGE_CURVE ( 'NONE', #105242, #107614, #115973, .T. ) ;
#188916 = CARTESIAN_POINT ( 'NONE',  ( 4.500456895562253479, -1.699381082468238713, 0.3444616058281315119 ) ) ;
#188917 = CARTESIAN_POINT ( 'NONE',  ( -4.172158584703340445, 5.890604320285754980, -1.599625672291256295 ) ) ;
#188918 = CARTESIAN_POINT ( 'NONE',  ( 1.938418878558012315, -1.110983660290700170, 1.746734030103759938 ) ) ;
#188919 = CARTESIAN_POINT ( 'NONE',  ( 3.515340291283968632, -1.955329406025432482, 0.8124583124677657864 ) ) ;
#188920 = CARTESIAN_POINT ( 'NONE',  ( 8.437251666405968464, 8.737881787095446384, 1.040834085586084257E-14 ) ) ;
#188921 = CARTESIAN_POINT ( 'NONE',  ( -0.6823417656250212460, 3.551041667008085323, 1.181850606188767472 ) ) ;
#188922 = CARTESIAN_POINT ( 'NONE',  ( 1.727339394501678838, 0.1499709341525606032, -1.963822474445919175 ) ) ;
#188923 = CARTESIAN_POINT ( 'NONE',  ( 5.769745475479523655, 6.237591007168648005, 1.002400605009654111 ) ) ;
#188924 = CARTESIAN_POINT ( 'NONE',  ( 0.03522015555855115276, -0.09184495783944729430, 1.910282976853895587 ) ) ;
#188925 = CARTESIAN_POINT ( 'NONE',  ( 3.943561162899355654, 0.7735357226616009774, -2.157932208606289759 ) ) ;
#188926 = CARTESIAN_POINT ( 'NONE',  ( 1.840199252755945425, 1.805614550920462635, 0.2691313018618191055 ) ) ;
#188927 = AXIS2_PLACEMENT_3D ( 'NONE', #131950, #33334, #63708 ) ;
#188928 = CARTESIAN_POINT ( 'NONE',  ( 4.529305835417093640, 7.441884687032027657, -1.199719254218450271 ) ) ;
#188929 = CARTESIAN_POINT ( 'NONE',  ( 6.941411460072420603, 7.200660912947041581, 1.040834085586084257E-14 ) ) ;
#188930 = CARTESIAN_POINT ( 'NONE',  ( -7.157815033010924921, 10.43820240756634199, 1.199719254218453823 ) ) ;
#188931 = CARTESIAN_POINT ( 'NONE',  ( 2.847905013607958669, -1.355098151751940483, -1.488992504630684000 ) ) ;
#188932 = CARTESIAN_POINT ( 'NONE',  ( 3.080854412065773928, 1.845568107317007822, 0.6654098317215583203 ) ) ;
#188933 = CARTESIAN_POINT ( 'NONE',  ( -7.296259222448620463, 11.66405285949874759, 0.7998128361456481317 ) ) ;
#188934 = CARTESIAN_POINT ( 'NONE',  ( -6.521635583373313061, 7.567328587812373719, -1.199719254218446718 ) ) ;
#188935 = DIRECTION ( 'NONE',  ( 0.000000000000000000, 0.000000000000000000, 1.000000000000000000 ) ) ;
#188937 = CARTESIAN_POINT ( 'NONE',  ( 4.451851733873055217, 1.769451340447548038, -0.04442182319205205399 ) ) ;
#188936 = CARTESIAN_POINT ( 'NONE',  ( 5.929650942584956397, 1.031255971971676955, -1.818501217082470145 ) ) ;
#188938 = CARTESIAN_POINT ( 'NONE',  ( 4.132297641190314508, 7.622816840561035256, -0.7610026044957002300 ) ) ;
#188939 = CARTESIAN_POINT ( 'NONE',  ( 0.8674257402763450031, 2.111068143204323455, -0.5878430487569612506 ) ) ;
#188940 = CARTESIAN_POINT ( 'NONE',  ( 5.103314706128504241, -1.731452751257630096, 0.1754873227253881951 ) ) ;
#188941 = CARTESIAN_POINT ( 'NONE',  ( 8.101160479365381306, 9.410107633136481908, -1.199719254218446718 ) ) ;
#188942 = CARTESIAN_POINT ( 'NONE',  ( -1.224999999999995204, 3.000000000000002665, -1.387778780781445676E-14 ) ) ;
#188943 = CARTESIAN_POINT ( 'NONE',  ( 6.604150285194997139, -0.1511744057106997885, 2.264526297252217990 ) ) ;
#188944 = CARTESIAN_POINT ( 'NONE',  ( 9.488641820551102057, -8.233137084989836652, -0.4644097342743017665 ) ) ;
#188945 = CARTESIAN_POINT ( 'NONE',  ( 5.747320757027973848, -1.692087196126054849, -0.3772414270737846631 ) ) ;
#188946 = CARTESIAN_POINT ( 'NONE',  ( 2.069229996397306426, -2.018448871333050842, -0.8927042923378907258 ) ) ;
#188947 = CARTESIAN_POINT ( 'NONE',  ( 6.338351057450786641, -1.166998422550720393, 1.830725944502207048 ) ) ;
#188948 = CYLINDRICAL_SURFACE ( 'NONE', #33772, 11.00000000000000000 ) ;
#188949 = CARTESIAN_POINT ( 'NONE',  ( 1.499367237992894841, -0.2534978968403051591, 2.102027841304268119 ) ) ;
#188950 = CARTESIAN_POINT ( 'NONE',  ( 3.031250000000001776, -0.7852924748301450819, -1.895863743164018400 ) ) ;
#188951 = CARTESIAN_POINT ( 'NONE',  ( -0.4909899725977228124, 7.342450396234926124, -1.941297109531795906 ) ) ;
#188952 = CARTESIAN_POINT ( 'NONE',  ( 4.682597122082689189, -1.868462817326870473, -0.4683620393717678465 ) ) ;
#188953 = CARTESIAN_POINT ( 'NONE',  ( 0.8916360836422586589, -0.05999620363036740206, -2.220659203727569420 ) ) ;
#188954 = ORIENTED_EDGE ( 'NONE', *, *, #36264, .F. ) ;
#188955 = CARTESIAN_POINT ( 'NONE',  ( 1.499999999999987121, 4.045833333333359150, -0.8660254037844323793 ) ) ;
#188956 = CARTESIAN_POINT ( 'NONE',  ( 5.657830175604453338, 5.495223381160312393, 0.7998128361456341429 ) ) ;
#188957 = CARTESIAN_POINT ( 'NONE',  ( 6.307567778855705853, 8.381915046796901692, -1.599625672291262513 ) ) ;
#188958 = CARTESIAN_POINT ( 'NONE',  ( 3.352378926113183777, 0.9974692666060747115, -1.984802063203878086 ) ) ;
#188959 = CARTESIAN_POINT ( 'NONE',  ( -7.809133291791416909, 11.09411069285655493, 1.082531754730549967 ) ) ;
#188960 = CARTESIAN_POINT ( 'NONE',  ( 6.697364695470787943, 7.876308901879812474, -1.082531754730543083 ) ) ;
#188961 = CARTESIAN_POINT ( 'NONE',  ( -8.554831740098665094, 11.00372300158037042, 1.443375672974064550 ) ) ;
#188962 = CARTESIAN_POINT ( 'NONE',  ( 7.038091139269835317, 7.383730215335837954, 0.000000000000000000 ) ) ;
#188963 = CARTESIAN_POINT ( 'NONE',  ( 1.776017750421728270, 1.753029812786778940, -0.9963028777105964462 ) ) ;
#188965 = CARTESIAN_POINT ( 'NONE',  ( 0.4091259740910870302, -1.658837074242287102, 1.225595967756993865 ) ) ;
#188964 = CARTESIAN_POINT ( 'NONE',  ( 8.101160479365381306, 9.410107633136481908, -1.199719254218446718 ) ) ;
#188966 = DIRECTION ( 'NONE',  ( 0.000000000000000000, 1.000000000000000000, 0.000000000000000000 ) ) ;
#188967 = CARTESIAN_POINT ( 'NONE',  ( 7.973603738168424826, 8.475161580717541554, 0.000000000000000000 ) ) ;
#188968 = CARTESIAN_POINT ( 'NONE',  ( 6.462468575563847573, -1.595429648854440385, -0.6960047898553810564 ) ) ;
#188969 = CARTESIAN_POINT ( 'NONE',  ( 0.6823417656249899377, 2.842708333674753618, 1.181850606188765695 ) ) ;
#188970 = CARTESIAN_POINT ( 'NONE',  ( 1.123854678948147834, 1.060202766368176786, -1.416847970540972668 ) ) ;
#188971 = CARTESIAN_POINT ( 'NONE',  ( 0.01820432788856435335, -1.842448466851685840, 0.8197770699841927522 ) ) ;
#188972 = CARTESIAN_POINT ( 'NONE',  ( 0.2218712608162629052, 1.761692264604281633, 0.5354471447000588302 ) ) ;
#188973 = CARTESIAN_POINT ( 'NONE',  ( 4.318134875187846333, 1.410584032999320225, -1.806939822960533348 ) ) ;
#188974 = CARTESIAN_POINT ( 'NONE',  ( 2.308333576337255000, 1.644441489820291924, 0.8281405146027611686 ) ) ;
#188975 = EDGE_CURVE ( 'NONE', #60692, #162811, #91667, .T. ) ;
#188976 = CARTESIAN_POINT ( 'NONE',  ( 8.723781775389312543, 12.26516360700784958, -1.199719254218446718 ) ) ;
#188977 = CARTESIAN_POINT ( 'NONE',  ( 11.47453837139429211, 7.808021129890302170, -3.623698920762073783 ) ) ;
#188978 = CARTESIAN_POINT ( 'NONE',  ( 3.328933297416610593, 0.04358344136132231289, 1.825221112333124340 ) ) ;
#188979 = CARTESIAN_POINT ( 'NONE',  ( 4.201796189063250253, 1.844709454618495670, 0.8146275914719460776 ) ) ;
#188980 = CARTESIAN_POINT ( 'NONE',  ( -8.143643823302737061, 12.65266822716189843, 0.000000000000000000 ) ) ;
#188982 = DIRECTION ( 'NONE',  ( 1.000000000000000000, -0.000000000000000000, -0.000000000000000000 ) ) ;
#188981 = CARTESIAN_POINT ( 'NONE',  ( 3.590934319571597033, -0.4389823211032486960, -2.219365549907009960 ) ) ;
#188983 = CARTESIAN_POINT ( 'NONE',  ( 5.069407556592405939, 0.2091588727727889396, -2.095552839448256766 ) ) ;
#188984 = CARTESIAN_POINT ( 'NONE',  ( 7.576886519560940947, 14.99604748842864410, 10.16829559912798686 ) ) ;
#188985 = CARTESIAN_POINT ( 'NONE',  ( 2.805202726412972858, -1.722705984639979704, 1.148039668612794051 ) ) ;
#188986 = CARTESIAN_POINT ( 'NONE',  ( 3.408985558832261731, 6.064568021024562938, 1.199719254218462483 ) ) ;
#188987 = CARTESIAN_POINT ( 'NONE',  ( -1.360316468749995789, 0.9218750003414100114, -6.938893903907228378E-15 ) ) ;
#188988 = CARTESIAN_POINT ( 'NONE',  ( 6.129554906816851556, -0.2598956320666659381, 2.104415924757463419 ) ) ;
#188990 = CIRCLE ( 'NONE', #199330, 2.250000000000000444 ) ;
#188989 = ITEM_DEFINED_TRANSFORMATION ( 'NONE', 'NONE', #211241,  #200407 ) ;
#188992 = CARTESIAN_POINT ( 'NONE',  ( 0.8910897993890665170, 1.699419447932304594, -0.9074141512597186932 ) ) ;
#188991 = CARTESIAN_POINT ( 'NONE',  ( -8.533967624797991647, 12.04371376465130439, -1.199719254218446718 ) ) ;
#188993 = CARTESIAN_POINT ( 'NONE',  ( -5.652823702255029836, 5.559658838911111900, -0.7998128361456362523 ) ) ;
#188994 = CARTESIAN_POINT ( 'NONE',  ( 9.257519960032755790, 9.694861462993381807, 0.7998128361456462443 ) ) ;
#188995 = CARTESIAN_POINT ( 'NONE',  ( 6.021229617800532452, 6.197391773621639288, 0.000000000000000000 ) ) ;
#188996 = CARTESIAN_POINT ( 'NONE',  ( 4.413087178904756769, 7.101426714207548230, 1.094556639780567053 ) ) ;
#188997 = CARTESIAN_POINT ( 'NONE',  ( -1.500000000000015099, 9.510416667349463893, -0.8660254037844309360 ) ) ;
#188998 = CARTESIAN_POINT ( 'NONE',  ( -4.952806187693842510, 4.672695395264567786, 0.7998128361456341429 ) ) ;
#188999 = CARTESIAN_POINT ( 'NONE',  ( 1.020144049103311801, -0.5328101295089396894, 2.156480530197317780 ) ) ;
#189000 = CARTESIAN_POINT ( 'NONE',  ( 2.749164281075014760, -1.751614713500139198, 1.168827980950073009 ) ) ;
#189001 = CARTESIAN_POINT ( 'NONE',  ( -5.004894982100124068, 5.868074229652107121, 1.199719254218452935 ) ) ;
#189002 = CARTESIAN_POINT ( 'NONE',  ( 8.751951852821344247, 10.16936423550178503, -1.199719254218446718 ) ) ;
#189003 = CARTESIAN_POINT ( 'NONE',  ( 5.928513603989616243, -1.181800583780348468, 1.437463819671711995 ) ) ;
#189004 = CARTESIAN_POINT ( 'NONE',  ( 7.263417608619159083, 9.497073181520933716, -1.599625672291262513 ) ) ;
#189005 =( BOUNDED_CURVE ( )  B_SPLINE_CURVE ( 3, ( #8877, #58704, #124854, #91227 ),
 .UNSPECIFIED., .F., .T. ) 
 B_SPLINE_CURVE_WITH_KNOTS ( ( 4, 4 ),
 ( 1.576609981660940907, 1.599396078175049807 ),
 .UNSPECIFIED. ) 
 CURVE ( )  GEOMETRIC_REPRESENTATION_ITEM ( )  RATIONAL_B_SPLINE_CURVE ( ( 1.000000000000000000, 0.9999567332851475587, 0.9999567332851475587, 1.000000000000000000 ) ) 
 REPRESENTATION_ITEM ( '' )  );
#189006 = ADVANCED_FACE ( 'NONE', ( #46669 ), #13067, .F. ) ;
#189007 = CARTESIAN_POINT ( 'NONE',  ( 11.94105721839851952, 10.07301656658867195, 1.187919402540718927 ) ) ;
#189008 = CARTESIAN_POINT ( 'NONE',  ( -7.756673280794142755, 8.222076047114187602, -0.7216878364870338292 ) ) ;
#189009 = CARTESIAN_POINT ( 'NONE',  ( -8.107412671292051343, 10.48173408797264194, 1.443375672974090751 ) ) ;
#189010 = CARTESIAN_POINT ( 'NONE',  ( -0.1049925189658337810, -2.058569791948822392, -0.5088776734372552069 ) ) ;
#189011 = CARTESIAN_POINT ( 'NONE',  ( -6.994027139803241866, 9.253060644560830994, -1.599625672291271394 ) ) ;
#189013 = CARTESIAN_POINT ( 'NONE',  ( 2.892962425504439050, 0.2373818416543191367, 1.947367909387688112 ) ) ;
#189012 = CARTESIAN_POINT ( 'NONE',  ( -0.6125000000000226930, -0.04166666666667595553, -1.060881119635941339 ) ) ;
#189014 = CARTESIAN_POINT ( 'NONE',  ( 2.606508400632711719, -0.8264410288459265175, -1.997682696722333784 ) ) ;
#189015 = CARTESIAN_POINT ( 'NONE',  ( 0.9777802892061361328, -1.796362506263926795, -0.4033719513514140709 ) ) ;
#189017 = CARTESIAN_POINT ( 'NONE',  ( -4.654334680973787108, 6.904393480334801048, -1.215188995478516221 ) ) ;
#189016 = CARTESIAN_POINT ( 'NONE',  ( -4.797606254389363833, 6.690569611577942943, 1.599625672291263179 ) ) ;
#189018 = CARTESIAN_POINT ( 'NONE',  ( -1.364683531250000748, 1.759375000341421913, 0.000000000000000000 ) ) ;
#189019 = CARTESIAN_POINT ( 'NONE',  ( 3.222313301838835020, 0.04370593061932443596, 1.739952058630070519 ) ) ;
#189020 = CARTESIAN_POINT ( 'NONE',  ( 6.534666852106798096, 7.686494751288491578, -1.082531754730543083 ) ) ;
#189021 = CARTESIAN_POINT ( 'NONE',  ( -11.76695491367977375, 4.673720869072629291, 4.995412848167406494 ) ) ;
#189022 = CARTESIAN_POINT ( 'NONE',  ( 0.8663662989462637132, 1.066309655776727539, 1.880320099339624296 ) ) ;
#189023 = COLOUR_RGB ( '', 0.72549020, 0.75294118, 0.79215686) ;
#189024 = CARTESIAN_POINT ( 'NONE',  ( 1.915388525686153143, 0.6297767875703685903, 1.915307412907449436 ) ) ;
#189025 = PLANE ( 'NONE',  #89548 ) ;
#189026 = CARTESIAN_POINT ( 'NONE',  ( 0.2862814217290919894, -1.017545141758866789, 1.907252267444502269 ) ) ;
#189027 = CARTESIAN_POINT ( 'NONE',  ( 2.166812389411576056, -1.801713905456410858, -0.8007201275355458892 ) ) ;
#189028 = AXIS2_PLACEMENT_3D ( 'NONE', #89325, #155372, #6957 ) ;
#189029 = CARTESIAN_POINT ( 'NONE',  ( -0.02319159430947368913, 6.948789054712430691, -2.406029888528108618 ) ) ;
#189033 = ORIENTED_EDGE ( 'NONE', *, *, #64698, .T. ) ;
#189032 = EDGE_CURVE ( 'NONE', #54631, #93709, #119379, .T. ) ;
#189031 = CARTESIAN_POINT ( 'NONE',  ( -5.804299160426249493, 5.944306240018289778, -0.7216878364870338292 ) ) ;
#189030 = PLANE ( 'NONE',  #160288 ) ;
#189034 = CARTESIAN_POINT ( 'NONE',  ( -6.414416072596849538, 7.616478518518682073, -1.082531754730549967 ) ) ;
#189035 = CARTESIAN_POINT ( 'NONE',  ( 7.374709211190586089, 7.568525266002632534, 0.000000000000000000 ) ) ;
#189036 = CARTESIAN_POINT ( 'NONE',  ( -6.629010762438975135, 6.698543742459062145, -0.7998128361456362523 ) ) ;
#189037 = CARTESIAN_POINT ( 'NONE',  ( 2.842449411481930532, 1.120122121419616423, -1.680381219987029606 ) ) ;
#189038 = CARTESIAN_POINT ( 'NONE',  ( -8.636180661780651135, 13.01936850547871138, -0.7216878364870257245 ) ) ;
#189039 = ADVANCED_FACE ( 'NONE', ( #2123 ), #153745, .F. ) ;
#189040 = CARTESIAN_POINT ( 'NONE',  ( 5.298025090176222029, -0.8365315220497183679, 2.150796518170698057 ) ) ;
#189041 = CARTESIAN_POINT ( 'NONE',  ( 4.130316239874070483, 3.817086806095215668, 1.214306433183764966E-14 ) ) ;
#189042 = CARTESIAN_POINT ( 'NONE',  ( 2.957805016080543581, -0.6199431972748243869, 1.861265166911831859 ) ) ;
#189043 = CARTESIAN_POINT ( 'NONE',  ( 7.086107841436786181, 11.41887624831828418, 1.040834085586084257E-14 ) ) ;
#189044 = CARTESIAN_POINT ( 'NONE',  ( 0.05336153386781630759, -1.314994204386025434, 1.528742563917218078 ) ) ;
#189045 = EDGE_LOOP ( 'NONE', ( #39239, #208806, #136578, #93812 ) ) ;
#189046 = CARTESIAN_POINT ( 'NONE',  ( 2.536447107014605962, 0.7179835868570243473, 1.991995636484017673 ) ) ;
#189048 = CARTESIAN_POINT ( 'NONE',  ( -7.203459687562382641, 7.298457811777897319, -0.7998128361456291469 ) ) ;
#189047 = FACE_OUTER_BOUND ( 'NONE', #38134, .T. ) ;
#189049 = CARTESIAN_POINT ( 'NONE',  ( 2.571990918753517708, -1.761868631437716548, -0.5344257538507577454 ) ) ;
#189050 = EDGE_LOOP ( 'NONE', ( #194379, #59375, #84186, #92222 ) ) ;
#189051 = CARTESIAN_POINT ( 'NONE',  ( -2.123823618835070537, 5.629544655282869847, 1.040834085586084257E-14 ) ) ;
#189052 = CARTESIAN_POINT ( 'NONE',  ( 4.094259397040445947, 3.811769539470978962, 2.445515378722424860 ) ) ;
#189053 = CARTESIAN_POINT ( 'NONE',  ( 4.535463010148616192, -0.1012041512906610846, 2.118281909017679432 ) ) ;
#189054 = CARTESIAN_POINT ( 'NONE',  ( 0.3746297210940018885, 1.718982886236510854, -0.6599183738737608440 ) ) ;
#189055 = CARTESIAN_POINT ( 'NONE',  ( -0.7500000000000215383, 5.222916667349482012, 1.299038105676671107 ) ) ;
#189056 = CARTESIAN_POINT ( 'NONE',  ( 6.889514614038635187, 11.18951748302043114, -0.7998128361456291469 ) ) ;
#189057 = CARTESIAN_POINT ( 'NONE',  ( 8.039058738260216330, 8.343599714250547805, -0.7998128361456341429 ) ) ;
#189058 = CARTESIAN_POINT ( 'NONE',  ( 3.884101140911602634, -1.018864849042991461, 1.791236251998897133 ) ) ;
#189060 = CARTESIAN_POINT ( 'NONE',  ( 0.9602180038516641147, -1.664555262390180257, -0.7873027242753791732 ) ) ;
#189059 = CARTESIAN_POINT ( 'NONE',  ( -7.009729113465285266, 8.136771039586342624, -1.199719254218446718 ) ) ;
#189061 = CARTESIAN_POINT ( 'NONE',  ( -1.201851678989727383E-14, 4.946875000341420581, -1.575800808251660134 ) ) ;
#189062 = CARTESIAN_POINT ( 'NONE',  ( 0.000000000000000000, 7.999999999999992895, 0.000000000000000000 ) ) ;
#189063 = CARTESIAN_POINT ( 'NONE',  ( 3.834746474454188013E-15, 13.06250000000000178, 1.500000000000001554 ) ) ;
#189064 = CIRCLE ( 'NONE', #5807, 0.07999999999999983513 ) ;
#189065 =( BOUNDED_CURVE ( )  B_SPLINE_CURVE ( 2, ( #7234, #90667, #201164, #86379, #152447, #193479, #76520 ),
 .UNSPECIFIED., .F., .T. ) 
 B_SPLINE_CURVE_WITH_KNOTS ( ( 3, 2, 2, 3 ),
 ( 0.1999999999999999556, 0.2041666666666666630, 0.2083333333333333981, 0.2125000000000001055 ),
 .UNSPECIFIED. ) 
 CURVE ( )  GEOMETRIC_REPRESENTATION_ITEM ( )  RATIONAL_B_SPLINE_CURVE ( ( 1.000000000000001776, 0.8660254037844369313, 1.000000000000000000, 0.8660254037844387076, 1.000000000000000000, 0.8660254037844351549, 1.000000000000003553 ) ) 
 REPRESENTATION_ITEM ( '' )  );
#189066 = CARTESIAN_POINT ( 'NONE',  ( 1.120068590173186163, -2.152398693614396397, 0.4866647226241942459 ) ) ;
#189067 = CARTESIAN_POINT ( 'NONE',  ( 3.972163192483857408, 1.252710246566196783, 1.883753103390993777 ) ) ;
#189068 = CARTESIAN_POINT ( 'NONE',  ( -7.375272376154081932, 10.58793962461302485, -1.082531754730543971 ) ) ;
#189069 = CARTESIAN_POINT ( 'NONE',  ( 3.568453337068989928, 0.6571482028082703541, 1.688366419454911727 ) ) ;
#189070 = CARTESIAN_POINT ( 'NONE',  ( 4.171028900271775974, 1.708651049203385286, -0.8665242481073615055 ) ) ;
#189072 = EDGE_CURVE ( 'NONE', #191425, #113693, #27236, .T. ) ;
#189071 = CARTESIAN_POINT ( 'NONE',  ( 4.949704645232674061, 1.531818663031824013, 1.392983054852282132 ) ) ;
#189073 = CARTESIAN_POINT ( 'NONE',  ( 1.364683531249988535, 4.467708333674754506, -0.7879004041258300672 ) ) ;
#189074 = AXIS2_PLACEMENT_3D ( 'NONE', #173065, #24645, #28936 ) ;
#189075 = CARTESIAN_POINT ( 'NONE',  ( 3.151204110225252819, -1.610897424746060791, -1.136263970179009819 ) ) ;
#189076 = CARTESIAN_POINT ( 'NONE',  ( 0.7977241263109683400, -0.6962278615636787737, 1.796346399320443821 ) ) ;
#189077 = CARTESIAN_POINT ( 'NONE',  ( 3.608139902456270143, -0.7572706533398064765, -1.710698989992056607 ) ) ;
#189078 = CARTESIAN_POINT ( 'NONE',  ( 2.192384427926857615, -0.9847255960707482769, 2.087179981119008598 ) ) ;
#189079 = CARTESIAN_POINT ( 'NONE',  ( 4.035495103658576888, 1.752908062920730092, -0.6255878229263853729 ) ) ;
#189080 = CARTESIAN_POINT ( 'NONE',  ( 1.364683531249990311, 4.134375000341417028, 1.214306433183764966E-14 ) ) ;
#189081 = CARTESIAN_POINT ( 'NONE',  ( -5.623934791570306402, 5.455678766453782913, 0.7998128361456341429 ) ) ;
#189082 = CARTESIAN_POINT ( 'NONE',  ( 7.149227073107712549, 7.235186428247455837, -0.7998128361456281477 ) ) ;
#189083 = CARTESIAN_POINT ( 'NONE',  ( 6.455298931196946199, -8.176227052203557832, 7.002681350352347067 ) ) ;
#189084 = CARTESIAN_POINT ( 'NONE',  ( 0.6277293814327978838, -1.999128025905463568, 0.6627883249872651428 ) ) ;
#189085 = CARTESIAN_POINT ( 'NONE',  ( 3.023105065722948126, 6.470780310077995701, 0.7216878364870338292 ) ) ;
#189087 = CARTESIAN_POINT ( 'NONE',  ( 3.834746474454188013E-15, 8.812500000000000000, 1.500000000000001554 ) ) ;
#189086 = CARTESIAN_POINT ( 'NONE',  ( 0.6823417656249899377, 4.988541667008086655, -1.181850606188754593 ) ) ;
#189088 = CARTESIAN_POINT ( 'NONE',  ( 1.264911064067347324, 3.965635264483307054, 0.5000000000000092149 ) ) ;
#189089 = CARTESIAN_POINT ( 'NONE',  ( 1.652743449602233072, 2.098267697663995790, 0.3060111223712052020 ) ) ;
#189090 = CARTESIAN_POINT ( 'NONE',  ( 0.3694064801790334918, -1.708597689296184274, -1.076810303892479226 ) ) ;
#189091 = CARTESIAN_POINT ( 'NONE',  ( -1.364683531250000748, 0.5093750003414208027, 0.000000000000000000 ) ) ;
#189092 =( GEOMETRIC_REPRESENTATION_CONTEXT ( 3 ) GLOBAL_UNCERTAINTY_ASSIGNED_CONTEXT ( ( #24913 ) ) GLOBAL_UNIT_ASSIGNED_CONTEXT ( ( #170060, #39010, #184174 ) ) REPRESENTATION_CONTEXT ( 'NONE', 'WORKASPACE' ) );
#189093 = CARTESIAN_POINT ( 'NONE',  ( -5.287316719649550301, 5.270883715786984780, 0.7216878364870317197 ) ) ;
#189094 = CARTESIAN_POINT ( 'NONE',  ( 4.690231075323689325, 7.559354456931247412, 1.199719254218462483 ) ) ;
#189095 = CARTESIAN_POINT ( 'NONE',  ( 1.106953007505812492, 1.637591863572019690, -1.411084338363017832 ) ) ;
#189098 = CARTESIAN_POINT ( 'NONE',  ( 3.877268743828276243, 4.586196958296845594, 1.082531754730560403 ) ) ;
#189097 = CARTESIAN_POINT ( 'NONE',  ( 6.825078400183556937, 1.282741234726336943, 1.971047034039685952 ) ) ;
#189096 = CARTESIAN_POINT ( 'NONE',  ( 4.980641328173811999, 6.904110530993182948, 1.599625672291269396 ) ) ;
#189099 = CARTESIAN_POINT ( 'NONE',  ( -5.503684012504701961, 5.385662534202396934, 0.000000000000000000 ) ) ;
#189100 = CARTESIAN_POINT ( 'NONE',  ( 5.999232488047272049, -0.2420365156972601739, 2.001857322483958423 ) ) ;
#189101 = CARTESIAN_POINT ( 'NONE',  ( -7.483737605063437215, 10.71448239167390604, 1.082531754730549967 ) ) ;
#189102 = CARTESIAN_POINT ( 'NONE',  ( -0.09381621004311831158, -0.9424329983100244723, -1.976553698157037076 ) ) ;
#189103 = CARTESIAN_POINT ( 'NONE',  ( 1.854049621773927514, 5.499999999999998224, -0.7500000000000006661 ) ) ;
#189105 = CARTESIAN_POINT ( 'NONE',  ( 1.364683531250000748, 11.00520833367473550, -0.7879004041258355073 ) ) ;
#189104 = CARTESIAN_POINT ( 'NONE',  ( 6.666866396406604167, -1.974176978123330040, -0.8811043787171415342 ) ) ;
#189106 = CARTESIAN_POINT ( 'NONE',  ( -10.13202086811422475, 10.71511252242175161, -0.7998128361456291469 ) ) ;
#189108 = CARTESIAN_POINT ( 'NONE',  ( 0.7025736824820059123, 1.770395976773591284, 0.7320947492839694482 ) ) ;
#189107 = CARTESIAN_POINT ( 'NONE',  ( -5.870317324592821073, 6.911420302522161663, -1.082531754730543083 ) ) ;
#189109 = CARTESIAN_POINT ( 'NONE',  ( -0.6823417656250003738, 1.280208333674752508, -1.181850606188749264 ) ) ;
#189110 = DIRECTION ( 'NONE',  ( 0.000000000000000000, -1.000000000000000000, 0.000000000000000000 ) ) ;
#189111 = CARTESIAN_POINT ( 'NONE',  ( -1.500000000000001110, 9.020833333333330373, 0.8660254037844419273 ) ) ;
#189112 = CARTESIAN_POINT ( 'NONE',  ( 3.299128894759464359, 1.360359547890070964, 1.060362228049552158 ) ) ;
#189113 = CARTESIAN_POINT ( 'NONE',  ( 5.578253857379852576, 5.472660686556754861, -0.7998128361456481317 ) ) ;
#189114 = CARTESIAN_POINT ( 'NONE',  ( 0.8777613430710672349, -0.9896981104785051997, 1.466914328529956180 ) ) ;
#189115 = CARTESIAN_POINT ( 'NONE',  ( 1.611978021082097978, -0.6760664726842831040, 1.896312242100234524 ) ) ;
#189116 = CARTESIAN_POINT ( 'NONE',  ( 8.867053104062428304, 4.021557182957047338, 7.983930475901377832 ) ) ;
#189117 = EDGE_CURVE ( 'NONE', #190459, #138847, #197945, .T. ) ;
#189118 = CARTESIAN_POINT ( 'NONE',  ( 4.278500955059440614, -1.273273528111932063, 1.802203266693293671 ) ) ;
#189119 = ORIENTED_EDGE ( 'NONE', *, *, #115265, .T. ) ;
#189120 = CARTESIAN_POINT ( 'NONE',  ( 7.687109908824030668, 10.95175007939464606, -1.082531754730543083 ) ) ;
#189121 = CARTESIAN_POINT ( 'NONE',  ( -5.901542003698421190, 10.10715911428198055, 0.000000000000000000 ) ) ;
#189123 = CARTESIAN_POINT ( 'NONE',  ( 4.148064665909578785, 0.9530284220014314522, 1.777003606838889915 ) ) ;
#189122 = CARTESIAN_POINT ( 'NONE',  ( 4.248766647586673884, 2.079802475202694900, 0.4125236972643344102 ) ) ;
#189125 = ORIENTED_EDGE ( 'NONE', *, *, #67738, .F. ) ;
#189124 = CARTESIAN_POINT ( 'NONE',  ( 3.023486134662889402, -0.3489238238089559241, 1.777470660238470224 ) ) ;
#189126 = CARTESIAN_POINT ( 'NONE',  ( 5.411639590510088027, 6.342609606130419131, -1.199719254218452047 ) ) ;
#189127 = VERTEX_POINT ( 'NONE', #85534 ) ;
#189128 = CARTESIAN_POINT ( 'NONE',  ( 1.445950363956361340, 1.868363765441739099, 0.09516058986362013750 ) ) ;
#189129 = CARTESIAN_POINT ( 'NONE',  ( 6.182242880246401562, -0.9723386526096773341, 1.545037271442825100 ) ) ;
#189130 = DIRECTION ( 'NONE',  ( -5.578564026256490882E-16, -1.000000000000000000, -9.066213480720158442E-32 ) ) ;
#189131 = CARTESIAN_POINT ( 'NONE',  ( 6.609000000000036401, 7.629137130509070275, 2.600000000000000977 ) ) ;
#189132 = CARTESIAN_POINT ( 'NONE',  ( -0.4019237886466871523, 8.729914550367427140, -1.499999999999998668 ) ) ;
#189133 = CARTESIAN_POINT ( 'NONE',  ( -1.364683531250012516, 3.301041667008084879, -0.7879004041258289570 ) ) ;
#189134 =( NAMED_UNIT ( * ) SI_UNIT ( $, .STERADIAN. ) SOLID_ANGLE_UNIT ( ) );
#189135 = CARTESIAN_POINT ( 'NONE',  ( 5.221298555038576872, 9.105615724271411082, 0.000000000000000000 ) ) ;
#189136 = CARTESIAN_POINT ( 'NONE',  ( -4.556949027968976829, 5.449433633119473264, 1.082531754730549078 ) ) ;
#189137 = CARTESIAN_POINT ( 'NONE',  ( -6.947627372360122955, 7.070263120700404968, 0.000000000000000000 ) ) ;
#189138 = CARTESIAN_POINT ( 'NONE',  ( 4.640951271726033056, 2.030106984047326701, 0.6129599860185754867 ) ) ;
#189139 = ADVANCED_FACE ( 'NONE', ( #101792 ), #38924, .T. ) ;
#189141 = CARTESIAN_POINT ( 'NONE',  ( -11.15867860892636365, 6.757705308438493041, -5.812542620506402358 ) ) ;
#189140 = CARTESIAN_POINT ( 'NONE',  ( -0.02948999725177046949, 0.7228889410342426158, -2.008564694272568563 ) ) ;
#189142 = CARTESIAN_POINT ( 'NONE',  ( 5.501234710350423107, 1.610096860432849830, 1.137200068526170060 ) ) ;
#189143 = CARTESIAN_POINT ( 'NONE',  ( -1.364683531250014514, 0.4885416670080875434, -0.7879004041258289570 ) ) ;
#189144 = CARTESIAN_POINT ( 'NONE',  ( 0.3518148739534024960, -1.426620726115679361, -1.420723246562720421 ) ) ;
#189145 = ORIENTED_EDGE ( 'NONE', *, *, #151210, .F. ) ;
#189146 = TOROIDAL_SURFACE ( 'NONE', #88822, 11.92000000000000171, 0.08000000000000000167 ) ;
#189147 = CARTESIAN_POINT ( 'NONE',  ( 0.3338148283143215767, 0.6594671527525318711, -2.011992694175788188 ) ) ;
#189148 = DIRECTION ( 'NONE',  ( 1.000000000000000000, 0.000000000000000000, 0.000000000000000000 ) ) ;
#189149 = CARTESIAN_POINT ( 'NONE',  ( 1.275928261265106833, -2.020323679977220621, 0.4517519998969782291 ) ) ;
#189150 = CARTESIAN_POINT ( 'NONE',  ( 5.499767588998890844, 6.445425604367387429, 1.199719254218451159 ) ) ;
#189151 = CARTESIAN_POINT ( 'NONE',  ( 4.199993725183334803, 8.122019456014369254, -0.7998128361456362523 ) ) ;
#189153 = CARTESIAN_POINT ( 'NONE',  ( 4.157546660884947620, 8.002221537674429896, 1.040834085586084257E-14 ) ) ;
#189152 = CARTESIAN_POINT ( 'NONE',  ( 4.119144422497845959, -2.000575632760223765, 0.6069725389450402186 ) ) ;
#189154 = CARTESIAN_POINT ( 'NONE',  ( 6.230854113932139171, 9.427024345299638952, 1.199719254218452047 ) ) ;
#189157 = ORIENTED_EDGE ( 'NONE', *, *, #58497, .F. ) ;
#189156 = CARTESIAN_POINT ( 'NONE',  ( 1.312835156398382885, 1.481033882128342194, -1.042734985588577468 ) ) ;
#189155 = CARTESIAN_POINT ( 'NONE',  ( 2.344514592193002400, 0.3973361102717865023, 1.781653928021959432 ) ) ;
#189158 = CARTESIAN_POINT ( 'NONE',  ( 5.250674450588199704, 0.6379336648693231249, 2.112661011922472021 ) ) ;
#189159 = CARTESIAN_POINT ( 'NONE',  ( -1.992711204631002198E-15, 2.999999999999989342, 1.224999999999989875 ) ) ;
#189160 = CARTESIAN_POINT ( 'NONE',  ( 4.489439581592091777, 1.972811803287272348, -0.9889974963176446643 ) ) ;
#189161 = CARTESIAN_POINT ( 'NONE',  ( 7.283754839039659146, 9.520799950344851936, -1.599625672291262513 ) ) ;
#189162 = CARTESIAN_POINT ( 'NONE',  ( 3.833604091385769408, 6.010284403505129269, -1.249999994511383772 ) ) ;
#189163 = CARTESIAN_POINT ( 'NONE',  ( 2.930216680654484041, -0.9444820207657660394, -1.662695861641521278 ) ) ;
#189164 = CARTESIAN_POINT ( 'NONE',  ( 10.24726517383036928, 10.84956421242393887, 0.000000000000000000 ) ) ;
#189165 = CARTESIAN_POINT ( 'NONE',  ( 5.266107318980479235, -2.060723932065291031, 0.1993833602659672022 ) ) ;
#189166 = DIRECTION ( 'NONE',  ( 1.908195823574487804E-17, 1.000000000000000000, -3.097714438736600596E-15 ) ) ;
#189167 = CARTESIAN_POINT ( 'NONE',  ( 6.286699343557897279, 1.907799665397521105, -1.078441415684105120 ) ) ;
#189168 = ORIENTED_EDGE ( 'NONE', *, *, #181087, .F. ) ;
#189169 = ADVANCED_FACE ( 'NONE', ( #20523 ), #100723, .T. ) ;
#189170 = CARTESIAN_POINT ( 'NONE',  ( -0.3866937364864243554, 3.956598013261175772, 11.53692321988874170 ) ) ;
#189171 = CARTESIAN_POINT ( 'NONE',  ( 5.408776937209000657, 5.274937613024121674, 0.7998128361456352531 ) ) ;
#189172 = CARTESIAN_POINT ( 'NONE',  ( -0.02319159430947624612, 7.629137130509076492, -2.410989586153564623 ) ) ;
#189173 = CIRCLE ( 'NONE', #40461, 0.07999999999999940492 ) ;
#189174 = SURFACE_STYLE_USAGE ( .BOTH. , #155615 ) ;
#189175 = ADVANCED_FACE ( 'NONE', ( #70326 ), #183037, .T. ) ;
#189176 = CARTESIAN_POINT ( 'NONE',  ( -7.375272376154081932, 10.58793962461302485, -1.082531754730543971 ) ) ;
#189178 = CARTESIAN_POINT ( 'NONE',  ( 5.896870467300973750, 5.844380064798101237, 0.7998128361456352531 ) ) ;
#189177 = AXIS2_PLACEMENT_3D ( 'NONE', #166829, #203553, #151651 ) ;
#189179 = CARTESIAN_POINT ( 'NONE',  ( 6.297728486381423352, -1.495382609916453998, -1.431936454106122358 ) ) ;
#189180 = CARTESIAN_POINT ( 'NONE',  ( 4.424389683245252947, 1.183944675904605504, -1.519688292035234367 ) ) ;
#189181 = CARTESIAN_POINT ( 'NONE',  ( 0.5093889453341126083, -1.913797760093600919, 0.6352206787166372326 ) ) ;
#189182 = CARTESIAN_POINT ( 'NONE',  ( -9.969323024750229578, 10.52529837183042716, -0.7998128361456291469 ) ) ;
#189183 = CARTESIAN_POINT ( 'NONE',  ( 5.083381250481017410, 4.895309311841474553, 0.7998128361456352531 ) ) ;
#189184 = CARTESIAN_POINT ( 'NONE',  ( 5.459211493810820492, 6.084350935433496588, -0.8767179110168581424 ) ) ;
#189185 = CARTESIAN_POINT ( 'NONE',  ( 0.6038064816080711550, -2.180521553291506986, 0.2185767975278959385 ) ) ;
#189186 = CARTESIAN_POINT ( 'NONE',  ( 5.391160240453525709, 1.608232483172780558, -0.8641324296934371763 ) ) ;
#189187 = CARTESIAN_POINT ( 'NONE',  ( 6.590672070018850803, 7.822110515511036866, -1.082531754730548412 ) ) ;
#189188 = CARTESIAN_POINT ( 'NONE',  ( 8.048736748007069508, 12.54194330598362406, -0.7998128361456352531 ) ) ;
#189189 = EDGE_CURVE ( 'NONE', #32739, #157452, #58014, .T. ) ;
#189190 = CARTESIAN_POINT ( 'NONE',  ( -5.712781623311813384, 7.758274208654143855, -1.599625672291271394 ) ) ;
#189191 = CARTESIAN_POINT ( 'NONE',  ( 5.192936529234042808, 6.017179691316550283, -1.199719254218452047 ) ) ;
#189192 = CARTESIAN_POINT ( 'NONE',  ( 6.066347387471824781, 6.042103138330730872, -0.7998128361456481317 ) ) ;
#189193 = EDGE_LOOP ( 'NONE', ( #1843, #173458, #35862, #27876 ) ) ;
#189195 = CARTESIAN_POINT ( 'NONE',  ( 6.451439527836500432, -1.796305863176387518, 0.9092463195026576628 ) ) ;
#189194 = CARTESIAN_POINT ( 'NONE',  ( 3.122423488780329492, 0.04808623196613136253, 1.840796284283818585 ) ) ;
#189196 = CARTESIAN_POINT ( 'NONE',  ( 2.021309514094786763, 2.292189817666248075, -0.1691314976695507954 ) ) ;
#189197 = CARTESIAN_POINT ( 'NONE',  ( 6.948121807170864805, -0.8414398651286276731, 1.770450887113049099 ) ) ;
#189198 = CARTESIAN_POINT ( 'NONE',  ( -4.717347382551060342, 7.590990148696470818, 1.199719254218464037 ) ) ;
#189199 = CARTESIAN_POINT ( 'NONE',  ( -6.825879202496262899, -6.900108348305959538, 6.758184431511289780 ) ) ;
#189200 = CARTESIAN_POINT ( 'NONE',  ( -3.379006598303881059, 4.965260336153046516, -1.599625672291256295 ) ) ;
#189201 = CARTESIAN_POINT ( 'NONE',  ( 0.3618904354094238385, -0.5536326762660361833, 1.994880328902041589 ) ) ;
#189202 = CARTESIAN_POINT ( 'NONE',  ( -6.400857919427531684, 9.521399101757175742, 1.082531754730549967 ) ) ;
#189204 = CARTESIAN_POINT ( 'NONE',  ( 0.6548940681232479077, -1.578012236938080015, -1.004313744925364071 ) ) ;
#189203 = CARTESIAN_POINT ( 'NONE',  ( 2.630511997247253486, 0.2585083551314356631, 2.074647729848762889 ) ) ;
#189205 = CARTESIAN_POINT ( 'NONE',  ( 1.686874821769188237, -1.117660090026689979, -1.677749154088927552 ) ) ;
#189206 = CARTESIAN_POINT ( 'NONE',  ( 7.117667457494414762, 11.24776976714476184, 1.040834085586084257E-14 ) ) ;
#189207 = CARTESIAN_POINT ( 'NONE',  ( -1.364683531250012516, 4.551041667008083103, -0.7879004041258300672 ) ) ;
#189208 = CARTESIAN_POINT ( 'NONE',  ( 1.926944929849357280, -1.137335869680399902, -1.317475996949101669 ) ) ;
#189209 = CARTESIAN_POINT ( 'NONE',  ( 6.484877546038077867, 6.460111979999551224, 1.040834085586084257E-14 ) ) ;
#189210 = CYLINDRICAL_SURFACE ( 'NONE', #148346, 0.3999999999999997446 ) ;
#189211 = CARTESIAN_POINT ( 'NONE',  ( 2.683889919492283394, -0.8868522494023568514, 1.479262710868123110 ) ) ;
#189212 = CARTESIAN_POINT ( 'NONE',  ( 2.560326853991791829, -1.509077608345666066, 1.589458984681046516 ) ) ;
#189213 = CARTESIAN_POINT ( 'NONE',  ( 0.01762850287782054270, -1.587011929513387098, 0.6995264333442567928 ) ) ;
#189214 = CARTESIAN_POINT ( 'NONE',  ( 5.531908139154323223, -1.397534428995873546, -1.707979418440738195 ) ) ;
#189215 = CARTESIAN_POINT ( 'NONE',  ( -9.399770542442999144, 4.999985930147239799, -6.933469103752857521 ) ) ;
#189216 = CIRCLE ( 'NONE', #75118, 0.04999999999999991257 ) ;
#189217 = CARTESIAN_POINT ( 'NONE',  ( 2.975608675790370583, -0.2172404834940108442, 2.160205341352925856 ) ) ;
#189218 = CARTESIAN_POINT ( 'NONE',  ( 1.119449510670032177, -1.781678707675336870, 0.3977030049751931196 ) ) ;
#189219 = CARTESIAN_POINT ( 'NONE',  ( 1.445103857046235563, 8.688264192038509748, -2.625611233228769770 ) ) ;
#189220 = CARTESIAN_POINT ( 'NONE',  ( 4.487589638097394307, -0.5612149057237262317, 2.041579019078069379 ) ) ;
#189221 = DIRECTION ( 'NONE',  ( 0.000000000000000000, 1.000000000000000000, 0.000000000000000000 ) ) ;
#189222 = ORIENTED_EDGE ( 'NONE', *, *, #183120, .T. ) ;
#189224 = CARTESIAN_POINT ( 'NONE',  ( 1.364683531249986537, 1.467708333674748289, -0.7879004041258239610 ) ) ;
#189223 = CARTESIAN_POINT ( 'NONE',  ( 4.775077868145559457, 2.139425163340304525, -0.8237163094031977328 ) ) ;
#189225 = CARTESIAN_POINT ( 'NONE',  ( -2.216394925932018367, 5.529618480321886409, 1.040834085586084257E-14 ) ) ;
#189226 = CARTESIAN_POINT ( 'NONE',  ( 3.181359600701000989, 6.863336634126477875, 0.000000000000000000 ) ) ;
#189227 = COLOUR_RGB ( '', 0.31764706, 0.68627451, 0.89019608) ;
#189228 = CARTESIAN_POINT ( 'NONE',  ( 6.586594613159782341, -1.369803613283290700, 1.749543456560544552 ) ) ;
#189229 = CARTESIAN_POINT ( 'NONE',  ( -4.921246572080546500, 8.685278734161874681, 1.214306433183764966E-14 ) ) ;
#189230 = CARTESIAN_POINT ( 'NONE',  ( 3.633221978782282147, 5.261844946711204507, -1.443375672974057666 ) ) ;
#189231 = CARTESIAN_POINT ( 'NONE',  ( -6.358410854684793279, 7.480862754296137673, -1.082531754730543083 ) ) ;
#189232 = CARTESIAN_POINT ( 'NONE',  ( 4.638297949650961982, 5.544340708415133712, -1.082531754730548412 ) ) ;
#189233 = VERTEX_POINT ( 'NONE', #53033 ) ;
#189234 = CARTESIAN_POINT ( 'NONE',  ( 4.834611377684539413, 0.6298767044488963185, -1.915599524792414465 ) ) ;
#189236 = CARTESIAN_POINT ( 'NONE',  ( 2.852447711054075796, -2.056726475855717773, -0.1563953359742433491 ) ) ;
#189235 = CARTESIAN_POINT ( 'NONE',  ( 4.527533231959700366, 7.369540306339926516, 1.199719254218462483 ) ) ;
#189238 = CARTESIAN_POINT ( 'NONE',  ( -0.2408018239684097672, 5.720833683022617855, -2.694520676430669059 ) ) ;
#189237 = CARTESIAN_POINT ( 'NONE',  ( 7.075376061485196821, 9.347967719856493218, 1.599625672291268286 ) ) ;
#189239 = CARTESIAN_POINT ( 'NONE',  ( 5.194182247366881278, 5.232503174782402233, 0.7216878364870328300 ) ) ;
#189240 = CARTESIAN_POINT ( 'NONE',  ( 3.285556943750000070, -3.434374999522042060, 0.000000000000000000 ) ) ;
#189241 = CARTESIAN_POINT ( 'NONE',  ( 5.683573789218531402, -0.9880169931659465998, 1.956149625775935430 ) ) ;
#189242 = CARTESIAN_POINT ( 'NONE',  ( 3.111954093273407107, 0.05229746705895028935, 2.015912966248374349 ) ) ;
#189243 = CARTESIAN_POINT ( 'NONE',  ( 2.753256032281672372, 1.832158412346639453, -0.1828795585285883096 ) ) ;
#189244 = AXIS2_PLACEMENT_3D ( 'NONE', #8627, #42226, #172217 ) ;
#189245 = EDGE_CURVE ( 'NONE', #51499, #179285, #88228, .T. ) ;
#189246 = CARTESIAN_POINT ( 'NONE',  ( 5.960781091502512119, 10.10599504006161986, 0.7998128361456462443 ) ) ;
#189247 = CARTESIAN_POINT ( 'NONE',  ( 6.370122744524995717, 0.9412729668686821149, 1.564051812004362940 ) ) ;
#189248 = CARTESIAN_POINT ( 'NONE',  ( -5.689618019229208734, 9.789638122409414223, 0.7998128361456481317 ) ) ;
#189249 = CARTESIAN_POINT ( 'NONE',  ( 6.315309700038255869, -0.2845791475536703086, 2.244501093609466924 ) ) ;
#189250 = CARTESIAN_POINT ( 'NONE',  ( 2.104260374134783174, -2.105582044810641484, 0.05271062337313356383 ) ) ;
#189251 = CARTESIAN_POINT ( 'NONE',  ( -7.096767062110449942, 7.244259425409119046, -0.7998128361456362523 ) ) ;
#189252 = CARTESIAN_POINT ( 'NONE',  ( 8.101160479365381306, 9.410107633136481908, -1.199719254218446718 ) ) ;
#189253 = CARTESIAN_POINT ( 'NONE',  ( 6.983858524370772258, 9.241197259889668558, 1.443375672974063439 ) ) ;
#189254 = SURFACE_SIDE_STYLE ('',( #139458 ) ) ;
#189255 = CARTESIAN_POINT ( 'NONE',  ( -5.364222332501225488, 9.410009821226765325, 0.7998128361456481317 ) ) ;
#189256 = CARTESIAN_POINT ( 'NONE',  ( 6.263503779389103521, 10.25124547602188763, 1.040834085586084257E-14 ) ) ;
#189257 = CARTESIAN_POINT ( 'NONE',  ( 4.021084497595363239, 7.798870403269500429, 0.3307836955792880507 ) ) ;
#189258 = CARTESIAN_POINT ( 'NONE',  ( -5.436983294280064882, 6.301900917203534291, 1.199719254218450271 ) ) ;
#189259 = CARTESIAN_POINT ( 'NONE',  ( 4.113701061080524468, 1.785520537663972451, 1.321432767922005924 ) ) ;
#189260 = CARTESIAN_POINT ( 'NONE',  ( 2.009981539508858273, -1.034714594384738229, -1.931790675223004738 ) ) ;
#189261 = CARTESIAN_POINT ( 'NONE',  ( 0.6630615684519860498, -1.595754342771567025, 1.524677653706180802 ) ) ;
#189262 = CARTESIAN_POINT ( 'NONE',  ( -4.472210567661380587, 6.310941310395290493, 1.599625672291270506 ) ) ;
#189263 = CARTESIAN_POINT ( 'NONE',  ( 4.316819842036943911, -1.455217238560998272, 1.315978175897666080 ) ) ;
#189264 = CARTESIAN_POINT ( 'NONE',  ( 9.901532256681887745, 10.44620914241737530, 0.000000000000000000 ) ) ;
#189265 = CARTESIAN_POINT ( 'NONE',  ( -3.904598122329041576, 2.800000000000024691, -0.7749999999999944711 ) ) ;
#189266 = CARTESIAN_POINT ( 'NONE',  ( -1.364683531250000748, 0.009375000341420303140, 0.000000000000000000 ) ) ;
#189267 = CARTESIAN_POINT ( 'NONE',  ( -3.350273356352693188, 6.922752992471175482, 0.000000000000000000 ) ) ;
#189269 = EDGE_LOOP ( 'NONE', ( #29439, #106425, #37049, #45521 ) ) ;
#189268 = CARTESIAN_POINT ( 'NONE',  ( -7.226132686403777150, 7.532835677000276675, 1.040834085586084257E-14 ) ) ;
#189270 = CARTESIAN_POINT ( 'NONE',  ( 3.885109016898561585, -1.979880364965879380, -0.7601140796509860964 ) ) ;
#189271 = CARTESIAN_POINT ( 'NONE',  ( -7.485510208520816278, 8.866088343763324886, 1.082531754730549078 ) ) ;
#189272 = CARTESIAN_POINT ( 'NONE',  ( 5.260679775997886054, -1.568431141927080219, 1.487858469166832176 ) ) ;
#189273 = CARTESIAN_POINT ( 'NONE',  ( 4.054132754448328768, -1.361571661076573792, 1.239656203754434971 ) ) ;
#189274 = CARTESIAN_POINT ( 'NONE',  ( -5.779651213448679492, 6.079991247305356339, 0.5991391260298760679 ) ) ;
#189275 = CARTESIAN_POINT ( 'NONE',  ( -1.364683531250000748, 2.071875000341422357, 1.214306433183764966E-14 ) ) ;
#189276 = CARTESIAN_POINT ( 'NONE',  ( 6.386628771994263154, 1.510377909004370522, -0.8644441249686038997 ) ) ;
#189277 = CARTESIAN_POINT ( 'NONE',  ( 6.827182134110225675, 7.053278108740402175, 2.409100297097351184 ) ) ;
#189278 = CARTESIAN_POINT ( 'NONE',  ( 3.389175213736297820, 4.977123720824209840, 1.443375672974062551 ) ) ;
#189279 = CARTESIAN_POINT ( 'NONE',  ( 11.96786122759180770, 6.617496858734535969, 1.004052467025347006 ) ) ;
#189280 = CARTESIAN_POINT ( 'NONE',  ( 4.135729569369491543, -1.488772398488470872, -1.567562023322838671 ) ) ;
#189281 = CARTESIAN_POINT ( 'NONE',  ( -5.759516327706961647, 5.613857225279885732, -0.7998128361456221525 ) ) ;
#189282 = CARTESIAN_POINT ( 'NONE',  ( 5.501327308730313170, 1.985796898448642933, 0.3474119236192701465 ) ) ;
#189283 = CARTESIAN_POINT ( 'NONE',  ( -8.202319746143382773, 9.632089794331152532, 1.082531754730558626 ) ) ;
#189284 = CARTESIAN_POINT ( 'NONE',  ( 3.625982885822197410, -1.285997354380935098, -1.737435825693343094 ) ) ;
#189285 = CARTESIAN_POINT ( 'NONE',  ( 4.235589135538409877, -1.357111243005538759, -1.430095230664797379 ) ) ;
#189286 = CARTESIAN_POINT ( 'NONE',  ( 0.2049558871960316941, 1.909868400323280424, 1.074723926240577221 ) ) ;
#189287 = CARTESIAN_POINT ( 'NONE',  ( 1.167484012262551607, -2.087313454887162578, -0.9842159052040798661 ) ) ;
#189288 = CARTESIAN_POINT ( 'NONE',  ( 3.268875894143012939, -1.902732241629549348, -0.7919657925325486181 ) ) ;
#189289 = CARTESIAN_POINT ( 'NONE',  ( 5.618683182394583753, -0.04358239772479224894, 1.941727988928889204 ) ) ;
#189291 = EDGE_CURVE ( 'NONE', #24541, #12413, #131445, .T. ) ;
#189290 = CARTESIAN_POINT ( 'NONE',  ( -8.202319746143382773, 9.632089794331152532, 1.082531754730558626 ) ) ;
#189292 = CARTESIAN_POINT ( 'NONE',  ( -7.605197822622922210, 7.837428646007010613, -0.7998128361456362523 ) ) ;
#189293 = CARTESIAN_POINT ( 'NONE',  ( -11.86686399458719343, 13.60928729775336699, -1.056461745586973811 ) ) ;
#189295 = ORIENTED_EDGE ( 'NONE', *, *, #25609, .F. ) ;
#189294 = CARTESIAN_POINT ( 'NONE',  ( -5.178288325776719603, 5.006034233019745372, 0.000000000000000000 ) ) ;
#189296 = CARTESIAN_POINT ( 'NONE',  ( -7.741342523278709642, 10.05465224862374285, 1.443375672974090751 ) ) ;
#189297 = CARTESIAN_POINT ( 'NONE',  ( 2.819571115601596123, -0.2173934082839618642, 2.196046946737562511 ) ) ;
#189298 = CARTESIAN_POINT ( 'NONE',  ( 1.642778471875001811, -3.230208332855373676, 2.845375778867859751 ) ) ;
#189299 = EDGE_LOOP ( 'NONE', ( #132398, #30184, #61990, #70024 ) ) ;
#189300 = CARTESIAN_POINT ( 'NONE',  ( 0.3032578436052570936, -1.433215674808469009, -1.186817810889209124 ) ) ;
#189301 = CARTESIAN_POINT ( 'NONE',  ( -0.1290005225502675879, 5.719648796287211567, -2.768066027128403217 ) ) ;
#189302 = CARTESIAN_POINT ( 'NONE',  ( 0.7499999999999920064, 5.264583334016151639, 1.299038105676669330 ) ) ;
#189303 = CARTESIAN_POINT ( 'NONE',  ( 4.333225684176827741, 7.421547172477886534, -1.117180756173659084 ) ) ;
#189306 = AXIS2_PLACEMENT_3D ( 'NONE', #200946, #203085, #167421 ) ;
#189305 = CARTESIAN_POINT ( 'NONE',  ( -10.99663476780025206, -7.859187537802515777, 0.2753234695294815570 ) ) ;
#189304 = CARTESIAN_POINT ( 'NONE',  ( -6.489832820117282353, 6.840411167308092288, -0.6218019135817691723 ) ) ;
#189307 = CARTESIAN_POINT ( 'NONE',  ( 6.158133876658566486, -1.298579738958350660, 1.305440813956220136 ) ) ;
#189308 = ORIENTED_EDGE ( 'NONE', *, *, #117712, .F. ) ;
#189309 = CARTESIAN_POINT ( 'NONE',  ( 2.536071046656536598, 0.9725223524452746293, -1.817000187329747884 ) ) ;
#189310 = CARTESIAN_POINT ( 'NONE',  ( -3.755786496842897795E-14, 1.078125000341431106, -1.570758158831814466 ) ) ;
#189311 = ADVANCED_FACE ( 'NONE', ( #50914 ), #98599, .F. ) ;
#189312 = CARTESIAN_POINT ( 'NONE',  ( -5.682838942422375084, 9.781729199468104596, 0.000000000000000000 ) ) ;
#189313 = CARTESIAN_POINT ( 'NONE',  ( -2.911621704963911927, 6.548642422433190724, 0.3158334299713649318 ) ) ;
#189314 = CARTESIAN_POINT ( 'NONE',  ( 11.86685672517501899, 11.10918917859810584, 1.056525322636017172 ) ) ;
#189315 = CARTESIAN_POINT ( 'NONE',  ( 4.798696304233017074, 7.685897223992134819, -1.199719254218452047 ) ) ;
#189316 = CARTESIAN_POINT ( 'NONE',  ( 1.252885565054340011, -1.625093837591420787, 1.267311679704327121 ) ) ;
#189318 = CARTESIAN_POINT ( 'NONE',  ( 4.616662711240536510, -0.08544939198026380023, 1.839383977539174264 ) ) ;
#189317 = CARTESIAN_POINT ( 'NONE',  ( -3.129460678718345878, 6.444905630999884671, -0.7687999843507524744 ) ) ;
#189319 = CARTESIAN_POINT ( 'NONE',  ( 7.308008492965924141, 8.484763649003774333, -1.199719254218451159 ) ) ;
#189320 = CARTESIAN_POINT ( 'NONE',  ( -5.468734858265826837, 7.473552982767158070, 1.599625672291263179 ) ) ;
#189321 = ORIENTED_EDGE ( 'NONE', *, *, #1852, .F. ) ;
#189322 = CARTESIAN_POINT ( 'NONE',  ( 3.985166894971280183, -0.2153072539897090687, -2.196357064762343825 ) ) ;
#189323 = CARTESIAN_POINT ( 'NONE',  ( 0.6851285477917113953, -0.2638797801631336259, -2.145333599305146333 ) ) ;
#189324 = CARTESIAN_POINT ( 'NONE',  ( -4.717874267875590277, 7.487641831621378863, 1.082531754730560403 ) ) ;
#189325 = CARTESIAN_POINT ( 'NONE',  ( 0.1934256698341470238, 1.783621342183003389, -0.6902995980747894667 ) ) ;
#189326 = CARTESIAN_POINT ( 'NONE',  ( 1.182827746461931229, 1.645757370610765102, -1.164989914844760444 ) ) ;
#189327 = CARTESIAN_POINT ( 'NONE',  ( 7.810905894804431426, 8.285347430126213553, 0.000000000000000000 ) ) ;
#189328 = CARTESIAN_POINT ( 'NONE',  ( 0.07536363704233049743, 0.2309889609098912111, -2.177957698420322163 ) ) ;
#189329 = CARTESIAN_POINT ( 'NONE',  ( 0.7500000000000006661, 12.11458333401613174, 1.299038105676657340 ) ) ;
#189330 = DIRECTION ( 'NONE',  ( 1.000000000000000000, 0.000000000000000000, -0.000000000000000000 ) ) ;
#189331 = EDGE_CURVE ( 'NONE', #209328, #17507, #5170, .T. ) ;
#189332 = CARTESIAN_POINT ( 'NONE',  ( 0.3209005354254980680, -0.09642172165634513292, 1.868300368337752815 ) ) ;
#189333 = MECHANICAL_DESIGN_GEOMETRIC_PRESENTATION_REPRESENTATION (  '', ( #89015 ), #85428 ) ;
#189334 = CARTESIAN_POINT ( 'NONE',  ( 2.501185699981960830, -0.1928336239410358699, 2.007256303757164240 ) ) ;
#189336 = CARTESIAN_POINT ( 'NONE',  ( -4.616310724566642598, 7.428787828840222041, 1.089621741958981094 ) ) ;
#189335 = CARTESIAN_POINT ( 'NONE',  ( 1.364683531249986537, 0.8635416670080893198, 0.7879004041258500513 ) ) ;
#189338 = CARTESIAN_POINT ( 'NONE',  ( 3.633512520595981066, -1.945918672469678867, 0.8060524589711003385 ) ) ;
#189337 = CARTESIAN_POINT ( 'NONE',  ( -7.167456763118792651, 11.51378332361394818, 0.000000000000000000 ) ) ;
#189339 = CARTESIAN_POINT ( 'NONE',  ( 7.283754839039659146, 9.520799950344851936, -1.599625672291262513 ) ) ;
#189341 = CARTESIAN_POINT ( 'NONE',  ( -9.013473194986783454, 9.410140237106395134, -0.7998128361456291469 ) ) ;
#189340 = CARTESIAN_POINT ( 'NONE',  ( 4.064412189046650248, 7.963840997188264659, 0.7998128361456271485 ) ) ;
#189342 = CARTESIAN_POINT ( 'NONE',  ( 3.744402900219420793, 1.076886947916893211, -1.708549110318995368 ) ) ;
#189343 = CARTESIAN_POINT ( 'NONE',  ( 0.6823417656249917140, 5.092708333674749177, 1.181850606188765695 ) ) ;
#189344 = CARTESIAN_POINT ( 'NONE',  ( 9.910647101909615841, 10.66476916175714607, 0.000000000000000000 ) ) ;
#189345 = CARTESIAN_POINT ( 'NONE',  ( 4.376362478467909156, -1.248523626585487989, 1.764366501186130698 ) ) ;
#189346 = CARTESIAN_POINT ( 'NONE',  ( 5.525830126021535449, 8.604496359403894346, -1.199719254218452047 ) ) ;
#189347 = CARTESIAN_POINT ( 'NONE',  ( -0.6823417656250246877, -0.1364583329919108468, 1.181850606188755259 ) ) ;
#189349 = SURFACE_STYLE_FILL_AREA ( #57224 ) ;
#189348 = CARTESIAN_POINT ( 'NONE',  ( 5.234329823327693809, 8.264412672927770487, 1.199719254218451159 ) ) ;
#189350 = CARTESIAN_POINT ( 'NONE',  ( 7.239690839573049708, 11.39013037956983965, 1.040834085586084257E-14 ) ) ;
#189352 = FACE_OUTER_BOUND ( 'NONE', #40446, .T. ) ;
#189351 = CARTESIAN_POINT ( 'NONE',  ( 2.524086392267041568, 2.129678358216775536, -0.4216712753718852014 ) ) ;
#189354 = CARTESIAN_POINT ( 'NONE',  ( 1.171164436615620863, 1.096940724416964885, 1.478650282607060662 ) ) ;
#189353 = CARTESIAN_POINT ( 'NONE',  ( -5.585596099150191840, 7.539614753807099667, -1.443375672974052559 ) ) ;
#189355 = CARTESIAN_POINT ( 'NONE',  ( 0.6823417656249882723, 1.676041667008083769, -1.181850606188749264 ) ) ;
#189356 = CARTESIAN_POINT ( 'NONE',  ( 3.632539538618652752, 0.3231117836275976818, 2.167502126216628522 ) ) ;
#189357 = CARTESIAN_POINT ( 'NONE',  ( -0.1305260785387524214, -7.912329794880667677, 10.96023284214815163 ) ) ;
#189358 = CARTESIAN_POINT ( 'NONE',  ( 3.731548843211284439, -2.091483890824384684, 0.8634027215336376182 ) ) ;
#189359 = CARTESIAN_POINT ( 'NONE',  ( -6.184490626128011925, 10.36698949712469364, -0.7998128361456291469 ) ) ;
#189360 = CARTESIAN_POINT ( 'NONE',  ( -1.201851678989727383E-14, 5.259375000341421469, -1.575800808251660134 ) ) ;
#189361 = CARTESIAN_POINT ( 'NONE',  ( 6.335378924966214242, 6.849830188997488634, 0.6565068261209184852 ) ) ;
#189362 = CARTESIAN_POINT ( 'NONE',  ( 0.7500000000000006661, 14.16666666666666785, -1.299038105676657340 ) ) ;
#189363 = CARTESIAN_POINT ( 'NONE',  ( 5.397554552016216256, 7.390509292142662723, 1.443375672974065660 ) ) ;
#189364 = CARTESIAN_POINT ( 'NONE',  ( 4.991328707773068807, 1.311207439723049317, 1.188721964340031301 ) ) ;
#189365 = CARTESIAN_POINT ( 'NONE',  ( 8.097244055859613709, 10.46987070330147063, -1.599625672291262513 ) ) ;
#189366 = CARTESIAN_POINT ( 'NONE',  ( 1.184755817749640894, -2.054561091436296838, -0.4616562467647678525 ) ) ;
#189368 = CARTESIAN_POINT ( 'NONE',  ( -1.402160292154681736E-14, 1.587500000000018785, -1.732050807568863648 ) ) ;
#189367 = CARTESIAN_POINT ( 'NONE',  ( 0.6823417656249934904, 10.19270833367473550, 1.181850606188764807 ) ) ;
#189369 = CARTESIAN_POINT ( 'NONE',  ( 1.099984078287146394, 0.8012805854674235340, -1.799388124431312797 ) ) ;
#189370 = CARTESIAN_POINT ( 'NONE',  ( -4.767627293860968507, 5.591261926706423857, -1.199719254218453823 ) ) ;
#189371 = CARTESIAN_POINT ( 'NONE',  ( 3.671470136052636946, 7.354626245547865260, -0.09674656412868055944 ) ) ;
#189373 = ORIENTED_EDGE ( 'NONE', *, *, #137043, .T. ) ;
#189372 = CARTESIAN_POINT ( 'NONE',  ( 6.258062559271784231, 0.6844122130202813237, -1.677549884021255933 ) ) ;
#189374 = CARTESIAN_POINT ( 'NONE',  ( 6.127922243696800386, 10.09306701771420656, -0.7216878364870267237 ) ) ;
#189375 = MECHANICAL_DESIGN_GEOMETRIC_PRESENTATION_REPRESENTATION (  '', ( #144441 ), #47625 ) ;
#189376 = CARTESIAN_POINT ( 'NONE',  ( 10.55910270694468345, 11.21337466772398095, 0.7998128361456462443 ) ) ;
#189377 = CARTESIAN_POINT ( 'NONE',  ( 4.996879044411707937, 1.554903924810165705, -1.039696167511289238 ) ) ;
#189378 = CARTESIAN_POINT ( 'NONE',  ( 2.920892028740289081, 5.495125569250587816, 1.199719254218452047 ) ) ;
#189379 = CARTESIAN_POINT ( 'NONE',  ( 4.153231765667256603, 1.751622898902647663, -1.103220242290925190 ) ) ;
#189380 = CARTESIAN_POINT ( 'NONE',  ( 0.6125000000000019318, 1.833333333333346582, 1.060881119635934455 ) ) ;
#189381 = CARTESIAN_POINT ( 'NONE',  ( -5.790741006368224753, 5.928488393617260321, 0.7216878364870257245 ) ) ;
#189382 = LINE ( 'NONE', #59382, #53476 ) ;
#189383 = CARTESIAN_POINT ( 'NONE',  ( 7.995557903757111617, 10.35123685918189729, 1.599625672291281386 ) ) ;
#189384 = CARTESIAN_POINT ( 'NONE',  ( -9.022061154889962964, 12.61315621642528129, -1.199719254218446718 ) ) ;
#189385 = CARTESIAN_POINT ( 'NONE',  ( 5.508355548902068577, 9.648441583686274470, 0.7998128361456331437 ) ) ;
#189386 = CARTESIAN_POINT ( 'NONE',  ( 5.078858209280799230, 4.912784287789808246, -0.2022913385141849041 ) ) ;
#189387 = CARTESIAN_POINT ( 'NONE',  ( 0.6823417656249882723, 0.1760416670080894308, -1.181850606188749264 ) ) ;
#189388 = CARTESIAN_POINT ( 'NONE',  ( 0.7499999999999885647, 1.816666666666688634, -1.299038105676652899 ) ) ;
#189389 = CARTESIAN_POINT ( 'NONE',  ( 4.404711838702720428, 0.5211615849865286476, 1.891323523724611766 ) ) ;
#189390 = CARTESIAN_POINT ( 'NONE',  ( 2.600935288962639369, 0.9528664403582010056, -1.776738882381201812 ) ) ;
#189391 = CARTESIAN_POINT ( 'NONE',  ( -0.1108833634136768137, 2.883350581177961391, -2.385667623150728112 ) ) ;
#189392 = CARTESIAN_POINT ( 'NONE',  ( -4.874313559192080092, 4.961021341527962036, 0.5169845646830675268 ) ) ;
#189393 = FACE_OUTER_BOUND ( 'NONE', #145234, .T. ) ;
#189394 = CARTESIAN_POINT ( 'NONE',  ( 1.704156511045151978, -0.6684128243485131238, -1.747238085743174185 ) ) ;
#189395 = CARTESIAN_POINT ( 'NONE',  ( -1.500000000000015099, -1.297916665983847029, 0.8660254037844403729 ) ) ;
#189396 = CARTESIAN_POINT ( 'NONE',  ( 4.254156334807709605, 0.8570458487419434501, -1.821774543695050319 ) ) ;
#189397 = CARTESIAN_POINT ( 'NONE',  ( -6.808165692356648258, 11.09461040772476714, 0.7998128361456481317 ) ) ;
#189399 = CARTESIAN_POINT ( 'NONE',  ( 3.726253221435165575, 2.107214626963071602, 0.2054869192316331195 ) ) ;
#189398 = CARTESIAN_POINT ( 'NONE',  ( -5.368665641331555882, 8.246898433986675769, 1.082531754730548412 ) ) ;
#189400 = CARTESIAN_POINT ( 'NONE',  ( 6.825078400183546279, 2.419143596098617621, 2.525240329153962904 ) ) ;
#189401 = CARTESIAN_POINT ( 'NONE',  ( 5.213363469605923228, -1.747142239327776903, -1.110534646669825376 ) ) ;
#189402 = CARTESIAN_POINT ( 'NONE',  ( 5.318541398310776103, 9.426991741329731056, -0.7998128361456481317 ) ) ;
#189404 = CARTESIAN_POINT ( 'NONE',  ( 6.720655732516654268, 4.688933928088002467, 2.736284108207136079 ) ) ;
#189403 = CARTESIAN_POINT ( 'NONE',  ( 6.714806893291140888, -0.1599574331335733013, 2.055667697375664016 ) ) ;
#189406 = ORIENTED_EDGE ( 'NONE', *, *, #184823, .F. ) ;
#189405 = CARTESIAN_POINT ( 'NONE',  ( 6.000976577881286467, 1.490888274384492895, -1.053294804101669868 ) ) ;
#189407 = CARTESIAN_POINT ( 'NONE',  ( 8.052653171512838881, 11.48218023581863001, -1.199719254218446718 ) ) ;
#189408 = CARTESIAN_POINT ( 'NONE',  ( 7.827294160508029286, -6.717993526550377403, -7.547439985188189482 ) ) ;
#189409 = CARTESIAN_POINT ( 'NONE',  ( -11.94651559118242368, 13.65130655878970956, 1.135242698369626435 ) ) ;
#189410 = CARTESIAN_POINT ( 'NONE',  ( -11.23957921816311512, 4.929848952671569862, 5.866464787178605533 ) ) ;
#189411 = CARTESIAN_POINT ( 'NONE',  ( 7.090551149822735155, 9.295395646258437949, 1.443375672974076540 ) ) ;
#189412 = CARTESIAN_POINT ( 'NONE',  ( -1.364683531250014514, 11.90104166700806587, -0.7879004041258335089 ) ) ;
#189413 = CARTESIAN_POINT ( 'NONE',  ( 6.393217174440144035, -0.09883813596619006603, -1.909861267343159863 ) ) ;
#189414 = CARTESIAN_POINT ( 'NONE',  ( -8.350932551013499960, 11.83017284523606172, -1.199719254218446718 ) ) ;
#189415 = CARTESIAN_POINT ( 'NONE',  ( 6.817052309572890323, 6.847649204123507083, 0.7998128361456341429 ) ) ;
#189416 = CARTESIAN_POINT ( 'NONE',  ( -0.6801582343750351978, 2.630208333674721732, -1.178068619123886718 ) ) ;
#189417 = CARTESIAN_POINT ( 'NONE',  ( 2.535011535630975477, 5.901337858304024131, 0.7216878364870438212 ) ) ;
#189418 = CARTESIAN_POINT ( 'NONE',  ( -1.500000000000008216, 12.28125000068279427, 3.469446951953614189E-15 ) ) ;
#189419 = CARTESIAN_POINT ( 'NONE',  ( 4.681643115420508039, 4.356338477612361260, 0.7998128361456341429 ) ) ;
#189420 = VERTEX_POINT ( 'NONE', #26920 ) ;
#189421 = EDGE_CURVE ( 'NONE', #108640, #115330, #42144, .T. ) ;
#189422 = PRODUCT_DEFINITION ( 'UNKNOWN', '', #90350, #82879 ) ;
#189423 = CARTESIAN_POINT ( 'NONE',  ( -7.096767062110449942, 7.244259425409119046, -0.7998128361456362523 ) ) ;
#189424 = CARTESIAN_POINT ( 'NONE',  ( 5.536732523015378327, -1.587826920732600122, 1.242742243127918700 ) ) ;
#189425 = DIRECTION ( 'NONE',  ( 1.000000000000000000, -0.000000000000000000, -0.000000000000000000 ) ) ;
#189426 = CARTESIAN_POINT ( 'NONE',  ( -6.855650617048436146, -7.357813805523307771, 6.855650617048461015 ) ) ;
#189427 = CARTESIAN_POINT ( 'NONE',  ( -0.1405533004718676759, 6.947778977978678050, -2.315285900534403307 ) ) ;
#189428 = CARTESIAN_POINT ( 'NONE',  ( -5.639828713604883248, 6.642516923036197340, 1.082531754730548412 ) ) ;
#189429 = CARTESIAN_POINT ( 'NONE',  ( 4.532503425670185493, 4.182342172903648070, 1.214306433183764966E-14 ) ) ;
#189430 = CARTESIAN_POINT ( 'NONE',  ( 2.694150338025066205, 0.9325801345280826382, -1.734679099899273824 ) ) ;
#189431 = CARTESIAN_POINT ( 'NONE',  ( 4.833611329963474645, 0.6298591494234163646, -1.915606498650752831 ) ) ;
#189432 = CARTESIAN_POINT ( 'NONE',  ( -6.449928391799210736, 8.548002428564306143, -1.599625672291263179 ) ) ;
#189433 = CARTESIAN_POINT ( 'NONE',  ( 6.827182134110230116, 2.398703475977175703, 2.668604416072619223 ) ) ;
#189434 = CARTESIAN_POINT ( 'NONE',  ( 4.277398745584213735, 1.430588233724191083, 1.660156109410643177 ) ) ;
#189435 = FACE_OUTER_BOUND ( 'NONE', #183346, .T. ) ;
#189436 = CARTESIAN_POINT ( 'NONE',  ( 3.698194863803183630, -1.924136204678703832, -0.09579085892482024078 ) ) ;
#189437 = CARTESIAN_POINT ( 'NONE',  ( -7.635213062790267458, 12.05949900656400686, 0.000000000000000000 ) ) ;
#189438 =( LENGTH_UNIT ( ) NAMED_UNIT ( * ) SI_UNIT ( .MILLI., .METRE. ) );
#189439 = CARTESIAN_POINT ( 'NONE',  ( 0.3994152196779980346, 1.832435997337564348, -1.229551327501000157 ) ) ;
#189440 =( NAMED_UNIT ( * ) PLANE_ANGLE_UNIT ( ) SI_UNIT ( $, .RADIAN. ) );
#189441 = CARTESIAN_POINT ( 'NONE',  ( -0.6823417656250003738, 13.15104166700806232, 1.181850606188754593 ) ) ;
#189442 = CARTESIAN_POINT ( 'NONE',  ( 6.484877546038077867, 6.460111979999551224, 1.040834085586084257E-14 ) ) ;
#189443 = CARTESIAN_POINT ( 'NONE',  ( 0.000000000000000000, 2.499999999999998668, 0.000000000000000000 ) ) ;
#189444 = CARTESIAN_POINT ( 'NONE',  ( 3.919715808126649659, 7.587102519540811940, 0.000000000000000000 ) ) ;
#189445 = EDGE_LOOP ( 'NONE', ( #199474, #23842, #168102, #156413 ) ) ;
#189447 = CARTESIAN_POINT ( 'NONE',  ( 2.455728839946738518, -1.493258543598206201, -1.350275873876593868 ) ) ;
#189446 = CARTESIAN_POINT ( 'NONE',  ( 6.163598723784101452, 0.9525508894225950263, 1.575581956637741587 ) ) ;
#189448 = CARTESIAN_POINT ( 'NONE',  ( 5.097139630348237027, 1.187786601409031695, -1.967583100176452549 ) ) ;
#189450 = CARTESIAN_POINT ( 'NONE',  ( 2.852234624111050110, -1.855622028292166714, -0.1419291048156411938 ) ) ;
#189449 = CARTESIAN_POINT ( 'NONE',  ( -5.921879234118920365, 10.13088588310589699, 0.000000000000000000 ) ) ;
#189451 = CARTESIAN_POINT ( 'NONE',  ( 1.001543065824772753E-15, -0.7218749995220414828, 3.793834371823811669 ) ) ;
#189452 = CARTESIAN_POINT ( 'NONE',  ( -4.723994514485429619, 8.288620342878445513, -0.7462711413273189764 ) ) ;
#189453 = PRESENTATION_STYLE_ASSIGNMENT (( #58391 ) ) ;
#189454 = CARTESIAN_POINT ( 'NONE',  ( -5.831978632172702071, 9.955725504176825780, 0.7998128361456481317 ) ) ;
#189455 = CARTESIAN_POINT ( 'NONE',  ( -4.719646871332968452, 5.639247783710797712, 1.082531754730549078 ) ) ;
#189456 = CARTESIAN_POINT ( 'NONE',  ( 6.427293192253748622, -1.366186911818557226, -1.582700853868714397 ) ) ;
#189457 = CARTESIAN_POINT ( 'NONE',  ( 4.663641653420880218, 8.384739662392275861, -0.7216878364870207285 ) ) ;
#189458 = ORIENTED_EDGE ( 'NONE', *, *, #108709, .T. ) ;
#189459 = CARTESIAN_POINT ( 'NONE',  ( -1.499999999999997780, 5.790625000341422357, 1.214306433183764966E-14 ) ) ;
#189461 = CARTESIAN_POINT ( 'NONE',  ( 3.194917754314666514, 6.879154480009089134, 0.7998128361456321445 ) ) ;
#189460 = CARTESIAN_POINT ( 'NONE',  ( 4.796824973295459316, 8.251456047330133714, 0.8599625132450954279 ) ) ;
#189462 = CARTESIAN_POINT ( 'NONE',  ( 6.059189007909253633, -1.483166448586000774, -0.8803546789384365523 ) ) ;
#189463 = CARTESIAN_POINT ( 'NONE',  ( -4.415151579544611238, 8.302760609444034046, -0.7998128361456281477 ) ) ;
#189464 = CARTESIAN_POINT ( 'NONE',  ( 0.9845302160453218709, -1.734343004718540637, -0.001328871039332768294 ) ) ;
#189465 = CARTESIAN_POINT ( 'NONE',  ( 0.1236583036082015280, 1.000000000000000888, -11.99936284241577233 ) ) ;
#189466 = FACE_BOUND ( 'NONE', #11163, .T. ) ;
#189467 = AXIS2_PLACEMENT_3D ( 'NONE', #56530, #6684, #190774 ) ;
#189468 = LINE ( 'NONE', #91996, #184897 ) ;
#189469 = CARTESIAN_POINT ( 'NONE',  ( 5.401315523140023167, -1.865749354952720207, 1.109950958716971803 ) ) ;
#189470 = CARTESIAN_POINT ( 'NONE',  ( 5.232948167349782409, 0.1380416123818763163, 1.820529236867339584 ) ) ;
#189471 = CARTESIAN_POINT ( 'NONE',  ( 2.571086506140254357, 1.750134206675527437, 0.8865088104979682582 ) ) ;
#189472 = CARTESIAN_POINT ( 'NONE',  ( 1.500000000000007105, 10.64264068711930733, 1.214306433183764966E-14 ) ) ;
#189473 = CARTESIAN_POINT ( 'NONE',  ( -10.65400978224035811, 11.32409958890225710, 1.040834085586084257E-14 ) ) ;
#189474 = CARTESIAN_POINT ( 'NONE',  ( 8.288111976655649471, 8.563885482386732306, -0.7998128361456291469 ) ) ;
#189475 = CARTESIAN_POINT ( 'NONE',  ( 4.143311163141574660, 0.1052805922370502884, 2.118007119816091688 ) ) ;
#189476 = FACE_OUTER_BOUND ( 'NONE', #101084, .T. ) ;
#189477 = CARTESIAN_POINT ( 'NONE',  ( -4.434757016570429755, 7.116138787269118637, -1.097766128466563851 ) ) ;
#189478 = CIRCLE ( 'NONE', #30408, 2.250000000000000444 ) ;
#189479 = CARTESIAN_POINT ( 'NONE',  ( 1.797802452481820135, -1.496673605676283714, -1.430578824989765518 ) ) ;
#189480 = CARTESIAN_POINT ( 'NONE',  ( 1.499999999999997113, 14.92708333401612997, -0.8660254037844378194 ) ) ;
#189482 = ORIENTED_EDGE ( 'NONE', *, *, #40036, .T. ) ;
#189481 = CARTESIAN_POINT ( 'NONE',  ( 3.703960633009816483, 1.609604546992912999, 1.531039788047829253 ) ) ;
#189483 = CARTESIAN_POINT ( 'NONE',  ( 1.407308937662318460, -1.282028150163934122, -1.907831638372993410 ) ) ;
#189485 = CARTESIAN_POINT ( 'NONE',  ( 0.4089400952669055567, -1.579117232646386704, 1.163831224039679979 ) ) ;
#189484 = CARTESIAN_POINT ( 'NONE',  ( 9.897088948295943212, 11.60932053017587506, 1.082531754730548412 ) ) ;
#189487 = CARTESIAN_POINT ( 'NONE',  ( 1.737499999999999378, -0.1166666666666676955, -3.009438278150925683 ) ) ;
#189486 = CARTESIAN_POINT ( 'NONE',  ( 4.203910148689107729, 7.062256385849379647, -1.199719254218448494 ) ) ;
#189488 = B_SPLINE_CURVE_WITH_KNOTS ( 'NONE', 3,
 ( #160553, #12161, #78232, #144355, #210356, #84627, #104091, #198361, #35874, #17471, #202621, #165886 ),
 .UNSPECIFIED., .F., .F.,
 ( 4, 2, 2, 2, 2, 4 ),
 ( 0.001597310297180445406, 0.001963012261066415971, 0.002328714224952386971, 0.003060118152724327668, 0.003791522080496267932, 0.004522926008268208196 ),
 .UNSPECIFIED. ) ;
#189489 = DIRECTION ( 'NONE',  ( 0.000000000000000000, 0.000000000000000000, -1.000000000000000000 ) ) ;
#189490 = CARTESIAN_POINT ( 'NONE',  ( -11.07790593930098311, 11.29999999999999893, 0.6999999999999992895 ) ) ;
#189491 = CARTESIAN_POINT ( 'NONE',  ( -3.337985173046072340, 6.383183490859034137, 0.8077998227833966816 ) ) ;
#189492 = CARTESIAN_POINT ( 'NONE',  ( -0.2102771530458276972, -0.008943344768331040057, -2.203482896658352175 ) ) ;
#189493 = CARTESIAN_POINT ( 'NONE',  ( 2.713528120726243831, -1.706327644498882634, 0.2505720552260106149 ) ) ;
#189494 = CARTESIAN_POINT ( 'NONE',  ( 2.835173002801576914, -1.651343842416474139, -1.157098616274463865 ) ) ;
#189495 = CARTESIAN_POINT ( 'NONE',  ( 2.549810578889585067, -1.582449011024213981, 1.667500336659861748 ) ) ;
#189496 = CARTESIAN_POINT ( 'NONE',  ( 3.374574379025939486, -1.350666858538966064, 1.814832908163630742 ) ) ;
#189497 = CARTESIAN_POINT ( 'NONE',  ( 5.760410450299061402, 0.8521563956989952615, 1.926159629354136316 ) ) ;
#189498 = CARTESIAN_POINT ( 'NONE',  ( -6.780486220610184134, 9.003929572168926754, -1.443375672974066548 ) ) ;
#189499 = CARTESIAN_POINT ( 'NONE',  ( 3.497073372749549769, 1.393195626148287403, 1.091155617269304878 ) ) ;
#189501 = CARTESIAN_POINT ( 'NONE',  ( 5.899983332490822185, -0.8214817842997054198, -2.140285636048167017 ) ) ;
#189500 = CARTESIAN_POINT ( 'NONE',  ( 7.309781096423290769, 8.557108029695882578, 1.199719254218452935 ) ) ;
#189502 = CARTESIAN_POINT ( 'NONE',  ( 5.314338895140062746, 1.702579029208791450, 0.7012131971957940024 ) ) ;
#189503 = CARTESIAN_POINT ( 'NONE',  ( -2.950870989268691957, 6.594433254122103349, -0.7998128361456281477 ) ) ;
#189504 = CARTESIAN_POINT ( 'NONE',  ( 5.578137875217415775, -2.137416510240647494, -0.4829537091169676666 ) ) ;
#189505 = CARTESIAN_POINT ( 'NONE',  ( -3.273404022695637572, 5.906389562198459231, 1.199719254218462483 ) ) ;
#189506 = CYLINDRICAL_SURFACE ( 'NONE', #87634, 0.07999999999999998779 ) ;
#189507 = CARTESIAN_POINT ( 'NONE',  ( 5.705552448923417508, -1.629793913574303588, -1.276656259598766940 ) ) ;
#189508 = CARTESIAN_POINT ( 'NONE',  ( -0.1355283706049141557, -1.957205112593700003, -0.4852584411360050254 ) ) ;
#189509 = AXIS2_PLACEMENT_3D ( 'NONE', #46522, #16110, #13983 ) ;
#189510 = CARTESIAN_POINT ( 'NONE',  ( 0.7499999999999885647, -0.9854166659838472508, 1.299038105676657340 ) ) ;
#189511 = CARTESIAN_POINT ( 'NONE',  ( 3.879452639046445661, 1.813680402594812557, -0.6499425845708036720 ) ) ;
#189512 = CARTESIAN_POINT ( 'NONE',  ( -1.364683531250014514, 9.838541667008064096, -0.7879004041258335089 ) ) ;
#189513 = CARTESIAN_POINT ( 'NONE',  ( -0.1399463097118925359, -1.722747986054250058, -1.402038615606171046 ) ) ;
#189515 = ORIENTED_EDGE ( 'NONE', *, *, #213374, .T. ) ;
#189514 = DIRECTION ( 'NONE',  ( 0.7592566023653004592, 0.6507913734559639396, 0.000000000000000000 ) ) ;
#189516 = CARTESIAN_POINT ( 'NONE',  ( -3.350273356352693188, 6.922752992471175482, 0.000000000000000000 ) ) ;
#189517 = CARTESIAN_POINT ( 'NONE',  ( 3.216308754939877446, 4.775446185561722956, -1.599625672291262513 ) ) ;
#189518 = CARTESIAN_POINT ( 'NONE',  ( -4.894130264408873110, 5.772535398974209642, -1.082531754730543971 ) ) ;
#189519 = CARTESIAN_POINT ( 'NONE',  ( -1.926045559592023171, 3.520657594588521455, -0.4000000000000374922 ) ) ;
#189520 = CARTESIAN_POINT ( 'NONE',  ( 10.65587894154546511, 9.861925906080523774, -5.419733535610468778 ) ) ;
#189521 = CARTESIAN_POINT ( 'NONE',  ( 10.20892648096591770, 11.01276177065614981, -0.7216878364870257245 ) ) ;
#189523 = CARTESIAN_POINT ( 'NONE',  ( 1.240593047436115759, -1.913272810121857237, -0.4332019784048374289 ) ) ;
#189522 = AXIS2_PLACEMENT_3D ( 'NONE', #8788, #26100, #10905 ) ;
#189524 = CARTESIAN_POINT ( 'NONE',  ( -1.402160292154681736E-14, 1.009375000341417916, -1.575800808251659024 ) ) ;
#189525 = DIRECTION ( 'NONE',  ( 0.000000000000000000, 0.000000000000000000, 1.000000000000000000 ) ) ;
#189526 = CARTESIAN_POINT ( 'NONE',  ( 5.951606347324345236, 1.484592722905058393, 1.282605414028796353 ) ) ;
#189527 = CARTESIAN_POINT ( 'NONE',  ( -7.784352752540590004, 12.23349531127272094, 0.7998128361456481317 ) ) ;
#189528 = CARTESIAN_POINT ( 'NONE',  ( -6.358410854684796831, 6.520493539994793863, -0.7216878364870267237 ) ) ;
#189529 = CARTESIAN_POINT ( 'NONE',  ( 6.684453901184132185, -2.118919246787358102, -0.4271090584619871566 ) ) ;
#189531 = ORIENTED_EDGE ( 'NONE', *, *, #46711, .T. ) ;
#189530 = CARTESIAN_POINT ( 'NONE',  ( -6.501298352952815662, 7.543601818988450169, -1.199719254218446718 ) ) ;
#189532 = CARTESIAN_POINT ( 'NONE',  ( -1.201851678989727383E-14, 5.446875000341422357, -1.575800808251660134 ) ) ;
#189533 = CARTESIAN_POINT ( 'NONE',  ( 1.932664581101939838, 0.1784410483233467293, 1.861995071071875785 ) ) ;
#189534 = CARTESIAN_POINT ( 'NONE',  ( 0.1758332513315676859, 1.282751065617006248, 1.167194905859494591 ) ) ;
#189536 = CARTESIAN_POINT ( 'NONE',  ( 4.581673536070863584, -1.032772929490553215, 1.932928240684625099 ) ) ;
#189535 = CARTESIAN_POINT ( 'NONE',  ( -1.360316468750056851, 2.119791667008092517, -0.7853790794159082322 ) ) ;
#189537 = CARTESIAN_POINT ( 'NONE',  ( 4.841030633121579996, 0.3891503725830172677, 2.274395804800657839 ) ) ;
#189538 = CARTESIAN_POINT ( 'NONE',  ( 0.2157906144764632494, -2.021207876486079691, 0.4015242071495705445 ) ) ;
#189539 = CARTESIAN_POINT ( 'NONE',  ( 2.870961461768199108, 1.843879596475753502, -0.6095136124301904212 ) ) ;
#189540 = CARTESIAN_POINT ( 'NONE',  ( -4.731432421044877934, 6.543090462684225450, -1.443375672974051449 ) ) ;
#189541 = DIRECTION ( 'NONE',  ( 1.000000000000000000, 0.000000000000000000, 0.000000000000000000 ) ) ;
#189542 = CARTESIAN_POINT ( 'NONE',  ( 5.168275554957600271, 2.118074532352266282, -0.1063875075708180934 ) ) ;
#189543 = CARTESIAN_POINT ( 'NONE',  ( -1.162044386198238738E-15, 2.937500000000009326, -1.225000000000010303 ) ) ;
#189544 = CARTESIAN_POINT ( 'NONE',  ( 3.182267690267494231, 1.591318367894577701, 1.238320962759748234 ) ) ;
#189545 = CARTESIAN_POINT ( 'NONE',  ( -4.812781342726871969, 6.637997537979888563, 1.443375672974064550 ) ) ;
#189546 = CARTESIAN_POINT ( 'NONE',  ( -7.119966945832006289, 8.335658187339330283, 1.199719254218452047 ) ) ;
#189547 = CARTESIAN_POINT ( 'NONE',  ( 9.073431116043567002, 11.60875560684942265, -1.599625672291262513 ) ) ;
#189548 = CARTESIAN_POINT ( 'NONE',  ( 1.558932953716257730, -1.564965500463588732, -0.9399777662534372080 ) ) ;
#189550 = B_SPLINE_CURVE_WITH_KNOTS ( 'NONE', 3,
 ( #47421, #165404, #48481, #64703 ),
 .UNSPECIFIED., .F., .F.,
 ( 4, 4 ),
 ( 0.001203384219977627961, 0.001801384605269243855 ),
 .UNSPECIFIED. ) ;
#189549 = CARTESIAN_POINT ( 'NONE',  ( -6.231907884136888676, 7.299589282028351001, -1.199719254218453823 ) ) ;
#189551 = CARTESIAN_POINT ( 'NONE',  ( -0.03257979115088098510, 15.47115322108842328, 11.98509113246685409 ) ) ;
#189552 = CARTESIAN_POINT ( 'NONE',  ( -10.14895191633106819, 5.000000000000002665, 7.601392964450658596 ) ) ;
#189553 = ORIENTED_EDGE ( 'NONE', *, *, #203402, .F. ) ;
#189554 = CARTESIAN_POINT ( 'NONE',  ( 6.016494556629995216, 1.386029456380773572, -1.525348796181945854 ) ) ;
#189555 = CARTESIAN_POINT ( 'NONE',  ( -7.255021596644144921, 7.636815748939187465, 0.7216878364870317197 ) ) ;
#189556 = EDGE_CURVE ( 'NONE', #6739, #211508, #24531, .T. ) ;
#189557 = DIRECTION ( 'NONE',  ( -0.8002608041566144914, -0.5996521035822427459, -8.676445024215948894E-15 ) ) ;
#189558 = CARTESIAN_POINT ( 'NONE',  ( -3.066115294984855133, 6.728884944124295053, 0.7998128361456341429 ) ) ;
#189559 = CARTESIAN_POINT ( 'NONE',  ( -4.864214080903581205, 4.879786425613829692, -0.6392378712632117432 ) ) ;
#189560 = CARTESIAN_POINT ( 'NONE',  ( 4.002606914492294443, -1.998013091498285654, -0.2940530905436929410 ) ) ;
#189561 = CARTESIAN_POINT ( 'NONE',  ( 5.285853969472154468, 2.141190784740894415, -0.5908706489107099502 ) ) ;
#189562 = AXIS2_PLACEMENT_3D ( 'NONE', #74665, #208902, #155921 ) ;
#189564 = CARTESIAN_POINT ( 'NONE',  ( 7.402388683381404988, 10.61957531637824204, -1.082531754730537976 ) ) ;
#189563 = CARTESIAN_POINT ( 'NONE',  ( -5.752402313948099533, 9.933162809573264695, -0.7998128361456362523 ) ) ;
#189565 = CARTESIAN_POINT ( 'NONE',  ( 4.971035877704902184, 8.951292290631053916, 1.040834085586084257E-14 ) ) ;
#189566 = CARTESIAN_POINT ( 'NONE',  ( 3.748945967280458369, -1.685778541264292274, 1.185220002557571206 ) ) ;
#189567 = CARTESIAN_POINT ( 'NONE',  ( 3.709611425391425854, 1.915599900965975433, 0.6298755557959597740 ) ) ;
#189568 = EDGE_LOOP ( 'NONE', ( #6531, #71709 ) ) ;
#189569 = DIRECTION ( 'NONE',  ( -5.578564026256490882E-16, -1.000000000000000000, -9.066213480720158442E-32 ) ) ;
#189570 = CARTESIAN_POINT ( 'NONE',  ( 3.344057444064992168, 7.053150784717805877, 1.040834085586084257E-14 ) ) ;
#189571 = CARTESIAN_POINT ( 'NONE',  ( -6.957269102468015554, 8.145844036748005834, 1.199719254218452047 ) ) ;
#189572 = CARTESIAN_POINT ( 'NONE',  ( 4.745935331938881951, 8.308991367555595531, -0.7587592799198628057 ) ) ;
#189573 = CARTESIAN_POINT ( 'NONE',  ( 3.673203737196802710, -0.8145011343782401214, -1.844427810980188820 ) ) ;
#189574 = CARTESIAN_POINT ( 'NONE',  ( 2.607153984523866264, -1.821078476238715327, 0.2702138248509636242 ) ) ;
#189575 = CARTESIAN_POINT ( 'NONE',  ( 4.450244736158118108, 7.987476157872649196, 2.500000000000000444 ) ) ;
#189576 = CARTESIAN_POINT ( 'NONE',  ( 0.6105616303546910206, -2.295997848557976617, 0.2320981213338509652 ) ) ;
#189577 = CARTESIAN_POINT ( 'NONE',  ( 5.969332771766739931, 10.18624834369502885, -0.7998128361456481317 ) ) ;
#189578 = CARTESIAN_POINT ( 'NONE',  ( 3.761131992884462871, -1.904433681825665969, -1.022602951024270679 ) ) ;
#189579 = AXIS2_PLACEMENT_3D ( 'NONE', #26033, #204767, #124702 ) ;
#189580 = CARTESIAN_POINT ( 'NONE',  ( -6.735703387890906946, 6.752742128827836865, -0.7998128361456291469 ) ) ;
#189581 = CARTESIAN_POINT ( 'NONE',  ( 3.269240723250285363, -2.295843464198448203, 0.1100516299901241751 ) ) ;
#189582 = CARTESIAN_POINT ( 'NONE',  ( 3.241898903847886913E-13, -7.217880409008443188, -9.581975256308904676 ) ) ;
#189583 = CARTESIAN_POINT ( 'NONE',  ( 2.465516990510143280, 1.834972510290140191, -0.3627323784974947340 ) ) ;
#189585 = EDGE_CURVE ( 'NONE', #31095, #111709, #184493, .T. ) ;
#189584 = SHAPE_REPRESENTATION ( 'rubber for base', ( #200407 ), #138598 ) ;
#189586 = CARTESIAN_POINT ( 'NONE',  ( 5.682488568729203493, -1.923295458312636264, -0.4324549907560610307 ) ) ;
#189588 = CARTESIAN_POINT ( 'NONE',  ( -7.208094944320834863, 8.438474185576302133, -1.199719254218452047 ) ) ;
#189587 = CARTESIAN_POINT ( 'NONE',  ( -1.001543065824772872E-14, 4.821875000341419693, 1.575800808251672791 ) ) ;
#189590 = CARTESIAN_POINT ( 'NONE',  ( 0.6982365061397632910, -0.7907169553198112322, 2.060542492664858560 ) ) ;
#189589 = CARTESIAN_POINT ( 'NONE',  ( -6.898401231254901234, 6.942556279419168419, -0.7998128361456291469 ) ) ;
#189591 = CARTESIAN_POINT ( 'NONE',  ( -1.474199074347627425, 7.377996015708403910, -4.279257749350879436 ) ) ;
#189592 = CARTESIAN_POINT ( 'NONE',  ( 5.412729640353754590, 7.337937218544611895, 1.599625672291267398 ) ) ;
#189593 = CARTESIAN_POINT ( 'NONE',  ( -6.196239896645333367, 7.187700286629718605, -1.199719254218446718 ) ) ;
#189594 = CARTESIAN_POINT ( 'NONE',  ( -0.1523027874135017556, -6.731960136058439126, -9.611344009005488687 ) ) ;
#189595 = CARTESIAN_POINT ( 'NONE',  ( 5.735224789204648843, -1.782488891340678894, 0.8425237689327728097 ) ) ;
#189596 = CARTESIAN_POINT ( 'NONE',  ( 5.725286558339668375, -0.06233732282829743815, 2.307013574275817547 ) ) ;
#189597 = CARTESIAN_POINT ( 'NONE',  ( 0.2737812321212430566, -1.924752420120953822, 0.3788971555385572954 ) ) ;
#189598 = CARTESIAN_POINT ( 'NONE',  ( 2.993094585481168579, 0.2480512885563341541, 2.047511573040517341 ) ) ;
#189599 = CARTESIAN_POINT ( 'NONE',  ( 5.314433026876846711, 9.143996264757578984, -0.7216878364870267237 ) ) ;
#189600 = CARTESIAN_POINT ( 'NONE',  ( 7.679767667498067496, 7.924426798361372093, 0.000000000000000000 ) ) ;
#189601 = CARTESIAN_POINT ( 'NONE',  ( 7.470179451005385829, 8.777926116670192513, -1.082531754730537976 ) ) ;
#189602 = CARTESIAN_POINT ( 'NONE',  ( -1.364683531250012516, 2.842708333674754506, 0.7879004041258379498 ) ) ;
#189603 = CARTESIAN_POINT ( 'NONE',  ( -9.569358774130440892, 3.553060279300377822, -7.167287524826073231 ) ) ;
#189604 = CARTESIAN_POINT ( 'NONE',  ( 6.141480396866128899, 6.267408005873028820, -0.7216878364870257245 ) ) ;
#189605 = CARTESIAN_POINT ( 'NONE',  ( 5.389208567375425751, 0.1545246996936377182, 2.165725388718000133 ) ) ;
#189607 = CARTESIAN_POINT ( 'NONE',  ( 5.636236351835953506, 0.3653394402399374741, 1.804471444190151930 ) ) ;
#189606 = CARTESIAN_POINT ( 'NONE',  ( -2.155383234892699562, 5.458438174109348395, 1.040834085586084257E-14 ) ) ;
#189609 = CARTESIAN_POINT ( 'NONE',  ( 6.620655732516651071, 7.053049904137934867, 2.524417197114035005 ) ) ;
#189608 = CARTESIAN_POINT ( 'NONE',  ( -11.86239285000045740, 11.29999999999998295, 1.812080536912751061 ) ) ;
#189610 = CARTESIAN_POINT ( 'NONE',  ( 6.462441986028243157, -2.002789442531027309, -0.8901952361822995652 ) ) ;
#189611 = CARTESIAN_POINT ( 'NONE',  ( 0.2099203756031532975, -0.7936979409460078738, -1.692237190125941648 ) ) ;
#189612 = CARTESIAN_POINT ( 'NONE',  ( 0.2810632938833834693, -2.195003449849114663, -0.5476492663787374537 ) ) ;
#189613 = CARTESIAN_POINT ( 'NONE',  ( -4.277728075731661583, 7.474117497184462167, -1.086723757153153835 ) ) ;
#189614 = CARTESIAN_POINT ( 'NONE',  ( 11.41381675112460847, 11.03016735491475941, -3.704697986577268232 ) ) ;
#189615 = CARTESIAN_POINT ( 'NONE',  ( 6.459053645710411296, 6.863086831863287607, 0.6637952124323226455 ) ) ;
#189616 = CARTESIAN_POINT ( 'NONE',  ( -5.926322542504884439, 6.086666852443364029, -0.7216878364870338292 ) ) ;
#189617 = CARTESIAN_POINT ( 'NONE',  ( 0.2406774923011632261, 1.829974501424940891, 0.5550298453492612527 ) ) ;
#189618 = CARTESIAN_POINT ( 'NONE',  ( 2.359889027365429826, 0.7540158325645224258, 1.601324458166239806 ) ) ;
#189620 = CARTESIAN_POINT ( 'NONE',  ( -0.1049974700286886165, -0.1398519552151776535, -1.881156918050665094 ) ) ;
#189619 = CIRCLE ( 'NONE', #148193, 12.00000000000000178 ) ;
#189622 = CARTESIAN_POINT ( 'NONE',  ( 3.269047429782430125, 1.730524700466531396, -0.8218109994902050852 ) ) ;
#189621 = CARTESIAN_POINT ( 'NONE',  ( -3.212919216314315207, 5.731860938133201522, 1.082531754730560403 ) ) ;
#189623 = CARTESIAN_POINT ( 'NONE',  ( 5.858512798400357546, 6.179092012920288646, 0.8810539604525641222 ) ) ;
#189624 = CARTESIAN_POINT ( 'NONE',  ( 4.527769023902194157, 1.910916496070225179, -0.4765158004534468805 ) ) ;
#189625 = CARTESIAN_POINT ( 'NONE',  ( 6.205333298273250975, 1.755376394247827987, -0.9990029765977179732 ) ) ;
#189626 = CARTESIAN_POINT ( 'NONE',  ( -2.286521462199063492, 5.819358805874190743, 1.040834085586084257E-14 ) ) ;
#189627 = CARTESIAN_POINT ( 'NONE',  ( 2.553401164250346245, 0.5009360343536627402, -1.802255699741683870 ) ) ;
#189629 = ORIENTED_EDGE ( 'NONE', *, *, #170125, .F. ) ;
#189628 = CARTESIAN_POINT ( 'NONE',  ( 5.602095939246814815, -1.725068444894608310, 0.006287883723511687381 ) ) ;
#189631 = CARTESIAN_POINT ( 'NONE',  ( 5.504247177468190699, 5.523969249908757817, 0.7216878364870317197 ) ) ;
#189630 = CARTESIAN_POINT ( 'NONE',  ( 2.508667999599442755, -0.8457060194008919618, -2.038605049697986615 ) ) ;
#189632 = CARTESIAN_POINT ( 'NONE',  ( 1.364683531249988535, 2.967708333674755394, -0.7879004041258239610 ) ) ;
#189633 = CARTESIAN_POINT ( 'NONE',  ( 6.092239754786219486, 0.9682357284593717806, -1.706234036142616928 ) ) ;
#189634 = CARTESIAN_POINT ( 'NONE',  ( 6.903072767652295383, 11.20533532890304684, 1.040834085586084257E-14 ) ) ;
#189635 = CARTESIAN_POINT ( 'NONE',  ( 9.926723642588102692, -7.126685749119995528, 1.734723475976807094E-15 ) ) ;
#189636 = CARTESIAN_POINT ( 'NONE',  ( -4.066556009095094737, 6.831733546331167695, 1.199719254218464037 ) ) ;
#189637 = DIRECTION ( 'NONE',  ( 0.000000000000000000, 0.000000000000000000, 1.000000000000000000 ) ) ;
#189638 = CIRCLE ( 'NONE', #172339, 0.08000000000000020983 ) ;
#189639 = CARTESIAN_POINT ( 'NONE',  ( 1.645070734656968625, -0.3017366986639741788, -2.048123538821471801 ) ) ;
#189640 = CARTESIAN_POINT ( 'NONE',  ( 1.499999999999989120, 3.025000000000020783, 1.214306433183764966E-14 ) ) ;
#189641 = CARTESIAN_POINT ( 'NONE',  ( 4.660252114795294887, 6.460046772059735432, -1.599625672291256295 ) ) ;
#189642 = CARTESIAN_POINT ( 'NONE',  ( 5.727393547130178675, 5.646656991265468939, 0.000000000000000000 ) ) ;
#189643 = CARTESIAN_POINT ( 'NONE',  ( 0.1705770660650838266, 0.7750864355984161680, 1.865232097879976125 ) ) ;
#189644 = CARTESIAN_POINT ( 'NONE',  ( -3.197497122698730099, 6.431928158754201874, 0.6077543439236172684 ) ) ;
#189645 = CARTESIAN_POINT ( 'NONE',  ( -0.6823417656250212460, 4.551041667008086655, 1.181850606188767472 ) ) ;
#189646 = ORIENTED_EDGE ( 'NONE', *, *, #5202, .T. ) ;
#189648 = CARTESIAN_POINT ( 'NONE',  ( 8.758204044747994743, 12.20135990463928266, 1.082531754730546636 ) ) ;
#189647 = DIRECTION ( 'NONE',  ( 0.000000000000000000, 0.000000000000000000, 1.000000000000000000 ) ) ;
#189649 = CARTESIAN_POINT ( 'NONE',  ( 5.167342215279057349, -0.6766115767681827320, -1.899327316215810635 ) ) ;
#189650 = CARTESIAN_POINT ( 'NONE',  ( 5.243340954880816973, 0.3670949043641066889, -1.880036887305686966 ) ) ;
#189651 = CARTESIAN_POINT ( 'NONE',  ( 6.539320575229258914, 2.958022083381315337, 2.556018433155104574 ) ) ;
#189652 = CARTESIAN_POINT ( 'NONE',  ( 2.841561854484982774, 0.7863008361240211297, -2.045831095052422555 ) ) ;
#189653 = CARTESIAN_POINT ( 'NONE',  ( -0.7500000000000006661, 2.639583334016156080, -1.299038105676652011 ) ) ;
#189654 = CARTESIAN_POINT ( 'NONE',  ( 2.320441991784210067, -0.7354482596747035084, -1.765520077574176172 ) ) ;
#189655 = CARTESIAN_POINT ( 'NONE',  ( -6.392833124043511894, 7.417059051927569868, 1.199719254218450271 ) ) ;
#189657 = CARTESIAN_POINT ( 'NONE',  ( -0.0003749349099593791675, -1.976945657698804704, 0.3961262320883383592 ) ) ;
#189656 = DIRECTION ( 'NONE',  ( 0.000000000000000000, 0.000000000000000000, -1.000000000000000000 ) ) ;
#189658 = CARTESIAN_POINT ( 'NONE',  ( -0.6823417656250039265, 10.13020833367472839, -1.181850606188755259 ) ) ;
#189660 = CARTESIAN_POINT ( 'NONE',  ( -6.577640801285370209, 7.702944352034914566, -1.199719254218452047 ) ) ;
#189659 = CARTESIAN_POINT ( 'NONE',  ( 6.251546423958431298, 2.185849743821382862, -0.1592787069685035195 ) ) ;
#189662 = ORIENTED_EDGE ( 'NONE', *, *, #32479, .F. ) ;
#189661 = CARTESIAN_POINT ( 'NONE',  ( 2.889346415704593607, 1.218289440699829473, 1.221169829160633435 ) ) ;
#189663 = CARTESIAN_POINT ( 'NONE',  ( 5.941668366282723213, -1.996146358238064522, 0.7160658055916299114 ) ) ;
#189664 = CARTESIAN_POINT ( 'NONE',  ( 4.473300617505036492, 7.306268922809479704, -1.199719254218452047 ) ) ;
#189665 = CARTESIAN_POINT ( 'NONE',  ( 8.500000000000000000, 6.200000000000038369, -2.900000000000000799 ) ) ;
#189666 = CARTESIAN_POINT ( 'NONE',  ( 0.4847190467827041105, 1.876267867961832980, 0.5731238010058882226 ) ) ;
#189667 = CARTESIAN_POINT ( 'NONE',  ( 11.41381678389391574, 10.07120581758926647, -3.704697885617874942 ) ) ;
#189668 = CARTESIAN_POINT ( 'NONE',  ( 6.006425746053997372, 6.966250444273174303, -1.199719254218445830 ) ) ;
#189669 = CARTESIAN_POINT ( 'NONE',  ( 2.075332711124678653, 1.720726420432414860, -11.62496126974820143 ) ) ;
#189670 = ORIENTED_EDGE ( 'NONE', *, *, #3623, .F. ) ;
#189671 =( BOUNDED_CURVE ( )  B_SPLINE_CURVE ( 3, ( #89870, #173251, #138610, #60534 ),
 .UNSPECIFIED., .F., .T. ) 
 B_SPLINE_CURVE_WITH_KNOTS ( ( 4, 4 ),
 ( 0.6625062783163327973, 1.570796326794872799 ),
 .UNSPECIFIED. ) 
 CURVE ( )  GEOMETRIC_REPRESENTATION_ITEM ( )  RATIONAL_B_SPLINE_CURVE ( ( 1.000000000000000000, 0.9324242863012305316, 0.9324242863012305316, 1.000000000000000000 ) ) 
 REPRESENTATION_ITEM ( '' )  );
#189672 = ORIENTED_EDGE ( 'NONE', *, *, #44751, .F. ) ;
#189673 = CARTESIAN_POINT ( 'NONE',  ( 3.070771698229213698, -1.370002115350689165, 1.185199408711124835 ) ) ;
#189674 = ORIENTED_EDGE ( 'NONE', *, *, #116730, .F. ) ;
#189675 = CARTESIAN_POINT ( 'NONE',  ( 9.402743226277308963, 10.92862083786708816, -1.199719254218446718 ) ) ;
#189676 = CARTESIAN_POINT ( 'NONE',  ( 3.711900195091365262, 7.552577004240394132, -0.7998128361456362523 ) ) ;
#189677 = CARTESIAN_POINT ( 'NONE',  ( 3.387185712204858312, 0.04143215291275677975, -1.811162278692766581 ) ) ;
#189678 = CARTESIAN_POINT ( 'NONE',  ( 7.363486825553451354, 8.723727730301414240, -1.082531754730548412 ) ) ;
#189679 = FACE_OUTER_BOUND ( 'NONE', #8924, .T. ) ;
#189680 = CARTESIAN_POINT ( 'NONE',  ( 5.890592889100787488, 5.978139607520936316, 0.07745371066007235294 ) ) ;
#189681 = ADVANCED_FACE ( 'NONE', ( #110390, #93029 ), #6397, .T. ) ;
#189683 = CARTESIAN_POINT ( 'NONE',  ( 1.364683531250000303, 14.25520833367473372, -0.7879004041258355073 ) ) ;
#189682 = CARTESIAN_POINT ( 'NONE',  ( 4.773795620589037725, -1.825254877749547866, 0.3623055857514579370 ) ) ;
#189684 = CARTESIAN_POINT ( 'NONE',  ( 3.128438982650301625, 0.4684375082077455454, 1.857299403769121060 ) ) ;
#189685 = CARTESIAN_POINT ( 'NONE',  ( 1.430379662499326354, 1.758314708518812663, 0.4907259477668829972 ) ) ;
#189686 = SURFACE_SIDE_STYLE ('',( #155067 ) ) ;
#189687 = CARTESIAN_POINT ( 'NONE',  ( -10.48267169704037727, 5.268073273308885973, 5.153989745587932880 ) ) ;
#189688 = CARTESIAN_POINT ( 'NONE',  ( 6.137634773950260580, 6.983624353001562923, 0.9378011681944794509 ) ) ;
#189689 = CARTESIAN_POINT ( 'NONE',  ( -11.41381678389398502, 10.07120581758917233, 3.704697885617667996 ) ) ;
#189690 = CARTESIAN_POINT ( 'NONE',  ( 0.000000000000000000, 4.000000000000003553, 0.000000000000000000 ) ) ;
#189691 = CARTESIAN_POINT ( 'NONE',  ( 6.925078400183577010, 2.950057911518181974, 2.596529392604688180 ) ) ;
#189692 = CARTESIAN_POINT ( 'NONE',  ( 7.456621297836078632, 8.762108271306003004, 1.082531754730558626 ) ) ;
#189693 = CARTESIAN_POINT ( 'NONE',  ( 5.946149452469858154, -0.8887192358506822432, 1.757629817417952767 ) ) ;
#189694 = CARTESIAN_POINT ( 'NONE',  ( -3.846762897975357198, 5.510976019103107859, -1.599625672291256295 ) ) ;
#189695 = CARTESIAN_POINT ( 'NONE',  ( 1.060620546929908148, -1.890798925694850974, -0.8922787324358200101 ) ) ;
#189696 = CARTESIAN_POINT ( 'NONE',  ( 6.704134009050578769, -1.925936059460537697, 0.04828832120675958378 ) ) ;
#189697 = CARTESIAN_POINT ( 'NONE',  ( -6.878064000834399394, 6.918829510595249310, -0.7998128361456291469 ) ) ;
#189698 = CARTESIAN_POINT ( 'NONE',  ( 1.957752326685862077, 1.820926393389955988, -0.1310869387763091420 ) ) ;
#189699 = CARTESIAN_POINT ( 'NONE',  ( 2.983271218942393332, -0.1628219013674602478, -2.200934326520533446 ) ) ;
#189700 = DIRECTION ( 'NONE',  ( -0.000000000000000000, 1.000000000000000000, -0.000000000000000000 ) ) ;
#189701 = CARTESIAN_POINT ( 'NONE',  ( 0.4922593472763935329, -1.060406550076501642, 1.591262010887870115 ) ) ;
#189702 = CARTESIAN_POINT ( 'NONE',  ( 1.381238074367253876, -0.05158952566820934615, 1.969057209924016227 ) ) ;
#189703 = CARTESIAN_POINT ( 'NONE',  ( 2.208448867685277150, 1.735655609654564113, 0.8713670519163093653 ) ) ;
#189704 = VERTEX_POINT ( 'NONE', #88755 ) ;
#189705 = CARTESIAN_POINT ( 'NONE',  ( 3.189213936345665523, 2.817530495244580102, 2.450448857954567572 ) ) ;
#189707 = CARTESIAN_POINT ( 'NONE',  ( 6.332830178222744522, -1.766687566082520533, -0.5848361604409312298 ) ) ;
#189706 = CARTESIAN_POINT ( 'NONE',  ( -4.842197138736131556, 5.678260079060780008, 1.199719254218452935 ) ) ;
#189708 = CARTESIAN_POINT ( 'NONE',  ( 4.573896719763862251, 6.429575154514868274, -1.599625672291273171 ) ) ;
#189709 = CARTESIAN_POINT ( 'NONE',  ( 0.000000000000000000, 3.599999999999999201, 0.000000000000000000 ) ) ;
#189710 = CARTESIAN_POINT ( 'NONE',  ( 8.886479618753304166, 12.45497775759917758, -1.199719254218446718 ) ) ;
#189711 = CARTESIAN_POINT ( 'NONE',  ( -6.784929528996132220, 6.880448970109080520, 0.000000000000000000 ) ) ;
#189712 = CARTESIAN_POINT ( 'NONE',  ( 2.331793494658142230, 1.030094174309360344, -1.934364310732391345 ) ) ;
#189713 = CARTESIAN_POINT ( 'NONE',  ( -10.95308175811721085, 9.799999999999998934, -1.800000000000001155 ) ) ;
#189714 = VECTOR ( 'NONE', #162740, 1000.000000000000114 ) ;
#189715 = CARTESIAN_POINT ( 'NONE',  ( 6.013923656113508542, 9.173938811177871244, -1.199719254218452047 ) ) ;
#189716 = CARTESIAN_POINT ( 'NONE',  ( -15.75000000000000000, 13.40000000000000036, -1.100000000000002087 ) ) ;
#189718 = CARTESIAN_POINT ( 'NONE',  ( 5.981657729715996297, -0.6748525008196132324, 1.900413905137773529 ) ) ;
#189717 = CARTESIAN_POINT ( 'NONE',  ( 2.490611698265518648, -0.3118145247060916114, -1.798701865878708839 ) ) ;
#189719 = SURFACE_STYLE_USAGE ( .BOTH. , #75978 ) ;
#189720 = CARTESIAN_POINT ( 'NONE',  ( -8.676855123066012254, 12.10645282934361866, -1.082531754730543971 ) ) ;
#189721 = CARTESIAN_POINT ( 'NONE',  ( -5.114454317065560751, 7.920171510810852133, -1.228010840421199568 ) ) ;
#189722 = CARTESIAN_POINT ( 'NONE',  ( 8.860417081730671995, 10.29590700256267155, 1.199719254218453823 ) ) ;
#189724 = EDGE_CURVE ( 'NONE', #199128, #47264, #40000, .T. ) ;
#189723 = CARTESIAN_POINT ( 'NONE',  ( 2.156748612084181005, -1.489394325481137260, 1.221923121036755600 ) ) ;
#189725 = CARTESIAN_POINT ( 'NONE',  ( 6.157081138237819218, 1.605775322519078729, -1.126676614267435150 ) ) ;
#189726 = CARTESIAN_POINT ( 'NONE',  ( -0.7500000000000006661, 14.95833333333333748, -1.299038105676657340 ) ) ;
#189727 = CARTESIAN_POINT ( 'NONE',  ( -7.039708073993679704, 9.236078724457858158, 1.599625672291283607 ) ) ;
#189728 = CARTESIAN_POINT ( 'NONE',  ( 5.657830175604453338, 5.495223381160312393, 0.7998128361456341429 ) ) ;
#189729 = CARTESIAN_POINT ( 'NONE',  ( -5.329763783503577379, 6.351050847909847086, 1.082531754730549078 ) ) ;
#189730 = CARTESIAN_POINT ( 'NONE',  ( -3.090895833791289071, 6.549869539491048442, 1.040834085586084257E-14 ) ) ;
#189732 = EDGE_CURVE ( 'NONE', #144836, #74967, #5306, .T. ) ;
#189731 = CARTESIAN_POINT ( 'NONE',  ( 1.464175926609780964E-14, -2.187499999999999112, -3.475000000000000533 ) ) ;
#189733 = CARTESIAN_POINT ( 'NONE',  ( 5.225469540725330653, 0.2083811790645866135, -2.059773418507819365 ) ) ;
#189734 = CARTESIAN_POINT ( 'NONE',  ( 1.364683531249988535, 3.217708333674748289, -0.7879004041258239610 ) ) ;
#189735 = CARTESIAN_POINT ( 'NONE',  ( 5.221416903470996296, 2.264307454851313572, 0.3953409806420198347 ) ) ;
#189736 = CARTESIAN_POINT ( 'NONE',  ( 7.131225611108096274, 8.382479970123348778, 1.082531754730558626 ) ) ;
#189738 = CARTESIAN_POINT ( 'NONE',  ( -5.458264003855187951, 7.602368174425947700, -1.382272695577278387 ) ) ;
#189737 = CARTESIAN_POINT ( 'NONE',  ( 5.722950238744211937, 5.849399164722627553, 0.7216878364870328300 ) ) ;
#189739 = CARTESIAN_POINT ( 'NONE',  ( 6.532792773074245218, -2.049936377808206700, 1.026291560346163534 ) ) ;
#189740 = CARTESIAN_POINT ( 'NONE',  ( 1.224999999999965006, 0.3541666666667217522, 0.7072540797572456350 ) ) ;
#189741 = CARTESIAN_POINT ( 'NONE',  ( -7.910256278930404505, 8.193330178365746619, -0.7998128361456362523 ) ) ;
#189742 = CARTESIAN_POINT ( 'NONE',  ( 5.402268692527759875, 1.469326413266746956, -1.269838510729433212 ) ) ;
#189743 = ORIENTED_EDGE ( 'NONE', *, *, #101693, .T. ) ;
#189744 = CARTESIAN_POINT ( 'NONE',  ( 9.097157884645296733, 10.67606762258344055, -1.082531754730543083 ) ) ;
#189745 = EDGE_LOOP ( 'NONE', ( #26638, #206790, #141848, #30543 ) ) ;
#189746 = CARTESIAN_POINT ( 'NONE',  ( 6.451426615364327155, -1.705040744490589066, 0.8662930942644477827 ) ) ;
#189747 = CARTESIAN_POINT ( 'NONE',  ( 0.9083514600924915694, 1.308824770132447135, -1.123559637378883203 ) ) ;
#189748 = CARTESIAN_POINT ( 'NONE',  ( 5.893767612163585135, -2.000732204962274441, 0.2516274335107801519 ) ) ;
#189750 = CARTESIAN_POINT ( 'NONE',  ( -4.095971805104331231, 5.871996087412059140, 1.443375672974065660 ) ) ;
#189749 = CARTESIAN_POINT ( 'NONE',  ( -7.316596452869116973, 11.68777962832266049, 0.7998128361456481317 ) ) ;
#189751 = CARTESIAN_POINT ( 'NONE',  ( -1.642778471875000035, -2.005208332855376696, -2.845375778867859751 ) ) ;
#189753 = CARTESIAN_POINT ( 'NONE',  ( 1.322737547172361472, -0.04825712817433693014, 1.769365563168373345 ) ) ;
#189752 = CARTESIAN_POINT ( 'NONE',  ( 1.130938551725582109, -1.889365942417848832, 0.8953178049561462126 ) ) ;
#189754 = CARTESIAN_POINT ( 'NONE',  ( 4.167806878822868377, 7.207497389070224081, 1.120509907031017605 ) ) ;
#189756 = CARTESIAN_POINT ( 'NONE',  ( 4.365347222306335873, 2.224029864950861857, -0.5546456485611241938 ) ) ;
#189755 = CARTESIAN_POINT ( 'NONE',  ( 3.410758162289653672, 6.136912401716668519, -1.199719254218453823 ) ) ;
#189757 = CARTESIAN_POINT ( 'NONE',  ( 2.343362483081043557, 1.739954169810492557, 0.04345107811378270263 ) ) ;
#189758 = CARTESIAN_POINT ( 'NONE',  ( 3.571683402196252910, 6.254382171615883834, 1.199719254218462483 ) ) ;
#189759 = CARTESIAN_POINT ( 'NONE',  ( 3.199588043238619228, 1.915454767000431602, -0.9102714984489732597 ) ) ;
#189761 = CARTESIAN_POINT ( 'NONE',  ( 0.6124999999999828360, 0.6458333340161465097, 1.060881119635891157 ) ) ;
#189760 = PRODUCT_RELATED_PRODUCT_CATEGORY ( 'part', '', ( #60975 ) ) ;
#189762 = CARTESIAN_POINT ( 'NONE',  ( 2.706025971585944490, -1.282006620817040643, -1.167505586895122072 ) ) ;
#189763 = CARTESIAN_POINT ( 'NONE',  ( -0.6801582343750351978, 2.630208333674721732, -1.178068619123886718 ) ) ;
#189764 = CARTESIAN_POINT ( 'NONE',  ( 1.381066672459789979, -0.05041352683890670816, 1.860554536023711458 ) ) ;
#189765 = CARTESIAN_POINT ( 'NONE',  ( 2.172564162468085147, -1.022266837292043595, -1.915435327925461229 ) ) ;
#189766 = CARTESIAN_POINT ( 'NONE',  ( 6.335737856287750880, 6.286115675290828264, -0.7998128361456281477 ) ) ;
#189767 = CARTESIAN_POINT ( 'NONE',  ( 3.749232653202066778, 0.2420323627391370025, -2.001857840249580800 ) ) ;
#189768 = CARTESIAN_POINT ( 'NONE',  ( 3.000000000000002665, -1.776620610948833047E-13, -2.052068128417948945 ) ) ;
#189769 = PRESENTATION_LAYER_ASSIGNMENT (  '', '', ( #30698 ) ) ;
#189770 = CARTESIAN_POINT ( 'NONE',  ( 0.7499999999999902300, 2.514583334016148974, 1.299038105676669330 ) ) ;
#189771 = CARTESIAN_POINT ( 'NONE',  ( 1.307504913943892122, -0.4706295199745584301, 1.867897339068110618 ) ) ;
#189772 = CARTESIAN_POINT ( 'NONE',  ( -1.402160292154681736E-14, 13.67187500034139447, 1.575800808251682339 ) ) ;
#189773 = CARTESIAN_POINT ( 'NONE',  ( 5.097972104635399404, 1.492264293747805226, 1.645667271412653898 ) ) ;
#189774 = VERTEX_POINT ( 'NONE', #108259 ) ;
#189775 = CARTESIAN_POINT ( 'NONE',  ( -1.499999999999960476, 7.000000000000000000, -10.99818166789402163 ) ) ;
#189776 = CARTESIAN_POINT ( 'NONE',  ( 1.499999999999987121, 1.004166666666687968, 0.8660254037844524744 ) ) ;
#189777 = CARTESIAN_POINT ( 'NONE',  ( 8.098297826064319693, 8.342435640030188893, 0.7998128361456481317 ) ) ;
#189778 = CARTESIAN_POINT ( 'NONE',  ( 1.364683531249986537, -0.5947916663252456049, -0.7879004041258309554 ) ) ;
#189779 = CARTESIAN_POINT ( 'NONE',  ( 5.730790430626864662, 1.492114905813126446, -1.645873056973495618 ) ) ;
#189780 = CARTESIAN_POINT ( 'NONE',  ( 5.160583804383015227, -0.6592509027269661814, -1.847929681152965520 ) ) ;
#189781 = CARTESIAN_POINT ( 'NONE',  ( 9.246297574839980271, 10.85006392781057905, 1.082531754730549967 ) ) ;
#189782 = DIRECTION ( 'NONE',  ( 0.7592566023652995710, -0.6507913734559650498, 0.000000000000000000 ) ) ;
#189783 = CARTESIAN_POINT ( 'NONE',  ( 5.694667785318580755, -0.5416461603767928068, -2.196524604246933521 ) ) ;
#189784 = CIRCLE ( 'NONE', #20312, 0.07999999999999971023 ) ;
#189785 = CARTESIAN_POINT ( 'NONE',  ( -6.644904684473536882, 6.925012684740138980, 0.7216878364870317197 ) ) ;
#189786 = CARTESIAN_POINT ( 'NONE',  ( 2.770046845359328103, -2.040585247751625086, 0.3002346618998888439 ) ) ;
#189787 = CARTESIAN_POINT ( 'NONE',  ( -6.230135280679522936, 7.227244901336242755, 1.199719254218450271 ) ) ;
#189788 = ORIENTED_EDGE ( 'NONE', *, *, #35599, .T. ) ;
#189789 = CARTESIAN_POINT ( 'NONE',  ( 0.7499999999999902300, 3.014583334016149418, 1.299038105676669330 ) ) ;
#189790 = CARTESIAN_POINT ( 'NONE',  ( -1.201851678989727383E-14, 4.509375000341417916, -1.575800808251660134 ) ) ;
#189791 = CARTESIAN_POINT ( 'NONE',  ( 4.288257209584379837, -1.849852534125648207, -0.2767368629695772797 ) ) ;
#189792 = CARTESIAN_POINT ( 'NONE',  ( 3.410549273128512304, -1.036309148604511288, -1.390238610006881981 ) ) ;
#189793 = CARTESIAN_POINT ( 'NONE',  ( 1.715945410011958217, 1.623988859063689949, 0.6264298892959454523 ) ) ;
#189794 = CARTESIAN_POINT ( 'NONE',  ( 1.101600182630409819, -0.5506920761103645257, 2.225148091679912454 ) ) ;
#189795 = CARTESIAN_POINT ( 'NONE',  ( 1.343116161061377545, 0.4315099961175078436, 2.164003993775004187 ) ) ;
#189796 = CARTESIAN_POINT ( 'NONE',  ( 4.317973780707057507, 1.284968578774790426, -1.649195526182813509 ) ) ;
#189797 = CARTESIAN_POINT ( 'NONE',  ( 5.419850138435895914, 1.155063568626579995, -1.560950513000541662 ) ) ;
#189798 = CARTESIAN_POINT ( 'NONE',  ( 7.988145303641245754, 15.26989286654994693, 8.896987721899689561 ) ) ;
#189799 =( NAMED_UNIT ( * ) PLANE_ANGLE_UNIT ( ) SI_UNIT ( $, .RADIAN. ) );
#189800 = CARTESIAN_POINT ( 'NONE',  ( 0.7213275451133926985, 1.987047012402185731, 0.3419330716275259530 ) ) ;
#189801 = CARTESIAN_POINT ( 'NONE',  ( -1.499999999999964029, 6.999999999999999112, 9.886859966642596476 ) ) ;
#189802 = DIRECTION ( 'NONE',  ( 7.387867266669436732E-31, -1.000000000000000000, -8.546850786086424434E-32 ) ) ;
#189803 = CARTESIAN_POINT ( 'NONE',  ( -9.341731535015849630, 10.85744053139533349, 1.199719254218462483 ) ) ;
#189804 = CARTESIAN_POINT ( 'NONE',  ( 7.494959990256193194, 7.638541498254023843, -0.7998128361456281477 ) ) ;
#189805 = CARTESIAN_POINT ( 'NONE',  ( 4.301258635363705451, 1.467727663998198429, 1.085573330547324744 ) ) ;
#189806 = CARTESIAN_POINT ( 'NONE',  ( 1.870444250305805856, 1.134645063044220858, 1.892580404734986121 ) ) ;
#189807 = ORIENTED_EDGE ( 'NONE', *, *, #2092, .F. ) ;
#189808 = CARTESIAN_POINT ( 'NONE',  ( -3.296040741453672318, 6.859481608422314025, 0.7216878364870338292 ) ) ;
#189809 = ADVANCED_FACE ( 'NONE', ( #189435 ), #190486, .T. ) ;
#189810 = UNCERTAINTY_MEASURE_WITH_UNIT (LENGTH_MEASURE( 1.000000000000000082E-05 ), #31192, 'distance_accuracy_value', 'NONE');
#189811 = CARTESIAN_POINT ( 'NONE',  ( 2.032879073410320814E-16, -7.473374494045017968, -9.579665964948882007 ) ) ;
#189812 = CARTESIAN_POINT ( 'NONE',  ( -1.642778471875000035, -2.005208332855376696, -2.845375778867859751 ) ) ;
#189813 = CARTESIAN_POINT ( 'NONE',  ( -6.507023659554960204, 9.678945805201045971, 1.199719254218452047 ) ) ;
#189814 = CARTESIAN_POINT ( 'NONE',  ( 0.7385429019767172365, 1.199765550694283478, -1.624703887242204825 ) ) ;
#189815 = CARTESIAN_POINT ( 'NONE',  ( -2.081668171172168513E-14, 5.868705557303649734, 4.125226524755077229 ) ) ;
#189816 = CARTESIAN_POINT ( 'NONE',  ( -5.822300622425855110, 5.757381912443740646, 0.7998128361456281477 ) ) ;
#189817 = CARTESIAN_POINT ( 'NONE',  ( 3.291705155655884951, -1.246473628130102762, -1.382024748694546501 ) ) ;
#189818 = CARTESIAN_POINT ( 'NONE',  ( 10.56588178375152864, 11.22128359066528169, -0.7998128361456281477 ) ) ;
#189819 = CIRCLE ( 'NONE', #34115, 0.2999999999999999334 ) ;
#189820 = FACE_OUTER_BOUND ( 'NONE', #150282, .T. ) ;
#189821 = ORIENTED_EDGE ( 'NONE', *, *, #102547, .T. ) ;
#189822 = CARTESIAN_POINT ( 'NONE',  ( -5.901876940650454095, 5.779944607047298177, -0.7998128361456291469 ) ) ;
#189823 = CARTESIAN_POINT ( 'NONE',  ( -7.160677686311960777, 11.50587440067263678, -0.7998128361456291469 ) ) ;
#189824 = CARTESIAN_POINT ( 'NONE',  ( 4.758326833623739205, 0.7015320795021735556, 1.685726030614169924 ) ) ;
#189826 = CARTESIAN_POINT ( 'NONE',  ( -3.976511113072466408, 7.848157239995420476, -0.08586869108932922157 ) ) ;
#189825 = CARTESIAN_POINT ( 'NONE',  ( -4.004454267989906668, 5.765225627445230927, 1.599625672291270506 ) ) ;
#189827 = CARTESIAN_POINT ( 'NONE',  ( 5.494857653270467601, 7.581134149042087600, -1.337725346733337872 ) ) ;
#189828 = CARTESIAN_POINT ( 'NONE',  ( 0.1922019376490837483, -1.058930769078871403, -1.372993611190379104 ) ) ;
#189829 = CARTESIAN_POINT ( 'NONE',  ( 0.5854151811709865649, -1.726609166672494311, -0.2174223460936832719 ) ) ;
#189830 = CARTESIAN_POINT ( 'NONE',  ( 3.897355454345535097, 1.950357463199345442, -1.233256315927799607 ) ) ;
#189831 = CARTESIAN_POINT ( 'NONE',  ( 4.903208829997618423, 5.749440385532527564, -1.199719254218450271 ) ) ;
#189832 = CARTESIAN_POINT ( 'NONE',  ( 6.608665842073913943, 1.606649649811153990, -1.446306907624186344 ) ) ;
#189833 = CARTESIAN_POINT ( 'NONE',  ( 6.928380191783277908, 8.041863964290678624, 1.199719254218462483 ) ) ;
#189834 = EDGE_CURVE ( 'NONE', #180747, #21587, #185145, .T. ) ;
#189835 = AXIS2_PLACEMENT_3D ( 'NONE', #204227, #89470, #170691 ) ;
#189836 = CARTESIAN_POINT ( 'NONE',  ( 6.169324051992485458, -0.8183585724929974825, -2.147936757437307165 ) ) ;
#189837 = CARTESIAN_POINT ( 'NONE',  ( -0.2949299779344195516, -3.232243495192088201, 3.285556943750023606 ) ) ;
#189838 = CARTESIAN_POINT ( 'NONE',  ( -7.449279056065764237, 7.655523418356991350, 0.7998128361456341429 ) ) ;
#189839 = CARTESIAN_POINT ( 'NONE',  ( 5.541831131927607679, 0.7570117910807551143, -1.710825945835430462 ) ) ;
#189840 = ORIENTED_EDGE ( 'NONE', *, *, #26426, .T. ) ;
#189842 = CARTESIAN_POINT ( 'NONE',  ( -4.930325137224961907, 5.781076077297750970, -1.199719254218453823 ) ) ;
#189841 = CARTESIAN_POINT ( 'NONE',  ( 2.759904966095374501, 0.6844231338998980618, -1.785916880244736715 ) ) ;
#189843 = CARTESIAN_POINT ( 'NONE',  ( 5.461621781982892720, 0.4335984126433762853, -2.163701019753036192 ) ) ;
#189844 = CARTESIAN_POINT ( 'NONE',  ( 4.856716432673345629, -1.994826133969303195, -0.7102248925668596113 ) ) ;
#189845 = CARTESIAN_POINT ( 'NONE',  ( -1.225000000000044276, 0.7916666673494796580, -0.7072540797572998139 ) ) ;
#189846 = CARTESIAN_POINT ( 'NONE',  ( 0.4294425147611385940, -9.006862915010128035, -9.490288674561771387 ) ) ;
#189847 = CARTESIAN_POINT ( 'NONE',  ( 4.380693030546905398, 8.124909279031149012, 0.7216878364870247253 ) ) ;
#189848 = CARTESIAN_POINT ( 'NONE',  ( -4.624739795592936353, 7.449261290616792763, -1.082531754730549967 ) ) ;
#189849 = ADVANCED_FACE ( 'NONE', ( #204591 ), #154101, .F. ) ;
#189850 = CARTESIAN_POINT ( 'NONE',  ( 2.749405113950495583, -1.918974089273906003, 1.281321877411125909 ) ) ;
#189851 = CARTESIAN_POINT ( 'NONE',  ( 3.789464544343919883, -1.813617537123424661, 0.7486148740368094856 ) ) ;
#189852 = CARTESIAN_POINT ( 'NONE',  ( -5.581116510680924847, 6.540332679663050541, -1.199719254218453823 ) ) ;
#189853 = CARTESIAN_POINT ( 'NONE',  ( 6.772339297775464395, -0.9671665324481359960, -1.821725317472399963 ) ) ;
#189854 = CARTESIAN_POINT ( 'NONE',  ( 2.562127843302666186, 5.932973550587659517, 0.000000000000000000 ) ) ;
#189855 = CARTESIAN_POINT ( 'NONE',  ( 5.239300017038202917, 5.077214539491492928, 0.000000000000000000 ) ) ;
#189856 = VERTEX_POINT ( 'NONE', #155879 ) ;
#189857 = CARTESIAN_POINT ( 'NONE',  ( 5.243375144629232487, 0.3886363430659239837, -1.978554426619572926 ) ) ;
#189858 =( BOUNDED_CURVE ( )  B_SPLINE_CURVE ( 1, ( #73831, #6674 ),
 .UNSPECIFIED., .F., .T. ) 
 B_SPLINE_CURVE_WITH_KNOTS ( ( 2, 2 ),
 ( 0.000000000000000000, 6.249999999999832079E-05 ),
 .UNSPECIFIED. ) 
 CURVE ( )  GEOMETRIC_REPRESENTATION_ITEM ( )  RATIONAL_B_SPLINE_CURVE ( ( 0.9345202395942817652, 0.9345202395942817652 ) ) 
 REPRESENTATION_ITEM ( '' )  );
#189859 = CARTESIAN_POINT ( 'NONE',  ( -8.676328237741483207, 12.20980114641871062, -1.199719254218446718 ) ) ;
#189860 = CARTESIAN_POINT ( 'NONE',  ( 11.84668730067608600, 13.39999999999998259, 1.399999999999998579 ) ) ;
#189861 = CARTESIAN_POINT ( 'NONE',  ( 1.419999999999990603, 6.280000000000042881, 2.580000000000000515 ) ) ;
#189862 = CARTESIAN_POINT ( 'NONE',  ( 8.829384350997564468, 11.32403438096243775, 1.599625672291281386 ) ) ;
#189863 = CARTESIAN_POINT ( 'NONE',  ( 1.815514387157551646, -1.860550965366158715, -1.118705476460989168 ) ) ;
#189864 = B_SPLINE_CURVE_WITH_KNOTS ( 'NONE', 3,
 ( #196161, #178856, #47802, #15249 ),
 .UNSPECIFIED., .F., .F.,
 ( 4, 4 ),
 ( 6.505213034913028530E-19, 0.0003197243294388478550 ),
 .UNSPECIFIED. ) ;
#189865 = PLANE ( 'NONE',  #117365 ) ;
#189866 = CARTESIAN_POINT ( 'NONE',  ( 11.68720892159067937, 1.016282880930320598, -3.797404372613902179 ) ) ;
#189867 = LINE ( 'NONE', #156319, #77251 ) ;
#189868 = CARTESIAN_POINT ( 'NONE',  ( 5.275877007301786215, 7.772378248882220397, 1.293907329011657614 ) ) ;
#189869 = AXIS2_PLACEMENT_3D ( 'NONE', #53233, #36973, #197343 ) ;
#189870 = CARTESIAN_POINT ( 'NONE',  ( 1.440775599906311433, 0.3991536164789717955, 2.021572055866586837 ) ) ;
#189872 = CARTESIAN_POINT ( 'NONE',  ( 6.727182134110170075, 7.629137130509032971, 2.510944104600740356 ) ) ;
#189871 = CARTESIAN_POINT ( 'NONE',  ( -0.02224634325202321655, 2.854569189074110280, -2.777010687634806629 ) ) ;
#189873 = CARTESIAN_POINT ( 'NONE',  ( 1.364683531249986537, 0.1135416670080857532, 0.7879004041258500513 ) ) ;
#189874 = SURFACE_SIDE_STYLE ('',( #124965 ) ) ;
#189875 = ORIENTED_EDGE ( 'NONE', *, *, #100966, .F. ) ;
#189876 = CARTESIAN_POINT ( 'NONE',  ( 3.387273370026026686, 0.04433669930821101945, -1.911926451916061476 ) ) ;
#189877 = CARTESIAN_POINT ( 'NONE',  ( 5.682415782506053503, -1.727394229680437876, -0.3844701117694647174 ) ) ;
#189878 = CARTESIAN_POINT ( 'NONE',  ( 6.658989722967328717, 7.797851427330578566, 1.199719254218452935 ) ) ;
#189879 = CARTESIAN_POINT ( 'NONE',  ( -5.603597561149804562, 5.431951997629870910, 0.7998128361456341429 ) ) ;
#189881 = CARTESIAN_POINT ( 'NONE',  ( 6.538697978567284963, -1.477089011224671955, 1.219511253712385335 ) ) ;
#189880 = CARTESIAN_POINT ( 'NONE',  ( 7.460470246983015308, -6.805008568744152164, 7.900729602272511976 ) ) ;
#189882 = AXIS2_PLACEMENT_3D ( 'NONE', #109549, #208023, #13017 ) ;
#189883 = CARTESIAN_POINT ( 'NONE',  ( 0.7499999999999867883, -0.6833333333333135862, -1.299038105676652899 ) ) ;
#189884 = CARTESIAN_POINT ( 'NONE',  ( 0.7485892145711986467, -2.054541080789675789, -0.2550698046258002005 ) ) ;
#189885 = CARTESIAN_POINT ( 'NONE',  ( -1.402160292154681736E-14, -0.7406249996585823059, -1.575800808251665908 ) ) ;
#189886 = CARTESIAN_POINT ( 'NONE',  ( 5.629731426258720361, -1.187751674602673058, -1.445209747047627946 ) ) ;
#189887 = CARTESIAN_POINT ( 'NONE',  ( 2.490611698265518648, -0.3118145247060916114, -1.798701865878708839 ) ) ;
#189888 = EDGE_CURVE ( 'NONE', #181635, #109578, #32215, .T. ) ;
#189890 = CARTESIAN_POINT ( 'NONE',  ( 6.017777097630443883, 7.067734144800174256, 1.048426327298467742 ) ) ;
#189889 = CARTESIAN_POINT ( 'NONE',  ( 5.707716145626243964, -0.5396369327701348029, 2.139774205771049154 ) ) ;
#189891 = CARTESIAN_POINT ( 'NONE',  ( -0.6823417656250003738, 0.4677083336747517306, -1.181850606188749264 ) ) ;
#189892 = CARTESIAN_POINT ( 'NONE',  ( 3.086439574430835275, 1.148074821921121647, -1.713452782031915200 ) ) ;
#189893 = CARTESIAN_POINT ( 'NONE',  ( -6.690058733339450114, 9.892486724616283311, 1.199719254218452047 ) ) ;
#189894 = CARTESIAN_POINT ( 'NONE',  ( 8.239604668803105270, 10.63595808506888396, -1.599625672291268286 ) ) ;
#189895 = CARTESIAN_POINT ( 'NONE',  ( 5.529027716274630855, 5.344953845275508542, 1.040834085586084257E-14 ) ) ;
#189896 = CARTESIAN_POINT ( 'NONE',  ( 0.4038910500440278106, -0.5768866637368921246, 2.083095904058133385 ) ) ;
#189897 = CARTESIAN_POINT ( 'NONE',  ( 5.993586425693011144, 9.150212042353954800, -1.199719254218452047 ) ) ;
#189898 = CARTESIAN_POINT ( 'NONE',  ( 5.143061708805018561, -0.2499388813127951525, -2.055141626981969338 ) ) ;
#189899 = CARTESIAN_POINT ( 'NONE',  ( -1.364683531250000748, 0.3218750003414205807, 0.000000000000000000 ) ) ;
#189900 = CARTESIAN_POINT ( 'NONE',  ( 3.497504216883956296, 1.701635573755799324, 1.332874705691905248 ) ) ;
#189901 = CARTESIAN_POINT ( 'NONE',  ( -4.768476522361002168, 8.183970109320437558, 0.7579922544750415936 ) ) ;
#189903 = CARTESIAN_POINT ( 'NONE',  ( 2.488659587246494276, 1.902222718079676689, 0.4795239450603656084 ) ) ;
#189902 = CARTESIAN_POINT ( 'NONE',  ( 2.930336769707508893, -0.9972767022783147750, -1.756213584645490267 ) ) ;
#189904 = CARTESIAN_POINT ( 'NONE',  ( 6.720655732516642722, 6.033109933379183332, 2.868628414513713309 ) ) ;
#189906 = CARTESIAN_POINT ( 'NONE',  ( 5.490689023854504747, 9.349628261231513804, 1.040834085586084257E-14 ) ) ;
#189905 = CARTESIAN_POINT ( 'NONE',  ( -1.642778471874998480, -3.901041666188709289, 2.845375778867863303 ) ) ;
#189907 = CARTESIAN_POINT ( 'NONE',  ( -7.391130018105325661, 8.652015104991543026, -1.199719254218452047 ) ) ;
#189908 = CARTESIAN_POINT ( 'NONE',  ( 2.589077643123653072, 1.706113014995232380, 1.074661422923957055 ) ) ;
#189910 = CARTESIAN_POINT ( 'NONE',  ( -1.123270288250315163, 2.985197346350006331, -0.7749999999993613109 ) ) ;
#189909 = CARTESIAN_POINT ( 'NONE',  ( -4.391951695823077984, 7.211361847513815704, 1.199719254218464037 ) ) ;
#189911 = CARTESIAN_POINT ( 'NONE',  ( 4.731432421044862835, 6.543090462684225450, -1.443375672974051449 ) ) ;
#189912 = CARTESIAN_POINT ( 'NONE',  ( 5.695548698317931091, 1.764485844685494742, -0.7379451211212140205 ) ) ;
#189913 = CARTESIAN_POINT ( 'NONE',  ( -11.86685672517501899, 12.49081082140188670, 1.056525322636010289 ) ) ;
#189914 = CARTESIAN_POINT ( 'NONE',  ( 5.843201017365476702, 6.879784610756938257, -1.082531754730543083 ) ) ;
#189916 = CARTESIAN_POINT ( 'NONE',  ( 2.794546173781168541, 1.458544728081469177, -1.392559875802508396 ) ) ;
#189915 = CARTESIAN_POINT ( 'NONE',  ( -7.470179451005382276, 11.65903375957422128, 0.7216878364870458196 ) ) ;
#189917 = CARTESIAN_POINT ( 'NONE',  ( -0.7499999999999972244, 4.358333333333352932, -1.299038105676652011 ) ) ;
#189918 = CARTESIAN_POINT ( 'NONE',  ( -1.364683531250000748, 13.17187500034139980, 0.000000000000000000 ) ) ;
#189919 = CARTESIAN_POINT ( 'NONE',  ( 0.06452196833307657919, -1.538014849765593439, -0.7809378474108348289 ) ) ;
#189920 = CARTESIAN_POINT ( 'NONE',  ( 7.309781096423290769, 8.557108029695882578, 1.199719254218452935 ) ) ;
#189921 = CARTESIAN_POINT ( 'NONE',  ( 9.273413882067330860, 9.921330405274451536, -0.7216878364870257245 ) ) ;
#189922 = FACE_OUTER_BOUND ( 'NONE', #157743, .T. ) ;
#189923 = CARTESIAN_POINT ( 'NONE',  ( 4.428871017648271291, 0.08965458760558722706, 1.868499062828571367 ) ) ;
#189924 = DIRECTION ( 'NONE',  ( -5.578564026256490882E-16, -1.000000000000000000, -9.066213480720158442E-32 ) ) ;
#189925 = CARTESIAN_POINT ( 'NONE',  ( 1.727480438796034745, 0.1563249218069600044, -2.064440809470533544 ) ) ;
#189926 = CARTESIAN_POINT ( 'NONE',  ( -6.061904078641520144, 10.08632216847484031, 0.7216878364870267237 ) ) ;
#189927 = ORIENTED_EDGE ( 'NONE', *, *, #121060, .T. ) ;
#189928 = CARTESIAN_POINT ( 'NONE',  ( 5.415556014015861841, 5.282846535965431300, -0.7998128361456481317 ) ) ;
#189929 = CARTESIAN_POINT ( 'NONE',  ( 0.6854714705560975840, 1.745592605935637920, -0.4840870370880663853 ) ) ;
#189930 = EDGE_CURVE ( 'NONE', #88893, #133104, #88391, .T. ) ;
#189931 = CARTESIAN_POINT ( 'NONE',  ( 3.879041346841291649, 7.539648981374564407, 1.040834085586084257E-14 ) ) ;
#189932 = CARTESIAN_POINT ( 'NONE',  ( -1.394453263437886604E-15, 2.375000000682794266, 1.224999999999975220 ) ) ;
#189933 = ORIENTED_EDGE ( 'NONE', *, *, #87853, .F. ) ;
#189934 = CARTESIAN_POINT ( 'NONE',  ( 8.568389893712330618, 9.098802418860289620, 1.040834085586084257E-14 ) ) ;
#189935 = EDGE_CURVE ( 'NONE', #140937, #85328, #89020, .T. ) ;
#189936 = CARTESIAN_POINT ( 'NONE',  ( 7.832860060393120882, 10.16142270859057462, 1.599625672291281386 ) ) ;
#189937 = CARTESIAN_POINT ( 'NONE',  ( 5.519116348382159032, -1.729776616345682028, 0.8233883490022309015 ) ) ;
#189938 = CARTESIAN_POINT ( 'NONE',  ( 6.827182134110198142, 0.003888933837258023996, 1.810856214465889069 ) ) ;
#189939 = DIRECTION ( 'NONE',  ( 0.000000000000000000, 0.000000000000000000, 1.000000000000000000 ) ) ;
#189941 = ORIENTED_EDGE ( 'NONE', *, *, #184591, .F. ) ;
#189940 = CARTESIAN_POINT ( 'NONE',  ( 5.355107487717867265, 5.349972945200037522, 1.040834085586084257E-14 ) ) ;
#189942 = CARTESIAN_POINT ( 'NONE',  ( -7.646435448427427062, 10.90429654226522693, 1.082531754730549967 ) ) ;
#189943 = CARTESIAN_POINT ( 'NONE',  ( 3.239309987758617115, -1.907233169736745060, 1.017530501952010447 ) ) ;
#189944 = CARTESIAN_POINT ( 'NONE',  ( -6.455090533882193782, 9.584670485287619002, -1.082531754730549967 ) ) ;
#189945 = EDGE_CURVE ( 'NONE', #49812, #13166, #105737, .T. ) ;
#189946 = CARTESIAN_POINT ( 'NONE',  ( 6.211043768836170820, 9.299949259400630552, 1.082531754730549967 ) ) ;
#189947 = CARTESIAN_POINT ( 'NONE',  ( -0.08743476694611679312, -2.120266877281291595, -0.04547849331201780226 ) ) ;
#189948 = CARTESIAN_POINT ( 'NONE',  ( 6.282242891264209206, -0.9739734823789309992, 1.543877162560061134 ) ) ;
#189949 = CARTESIAN_POINT ( 'NONE',  ( 10.90597896324554306, 8.126158609150163414, 4.424724984770519676 ) ) ;
#189950 = CARTESIAN_POINT ( 'NONE',  ( 0.6847650648834556764, -0.2371060910116972453, -1.956967405937762639 ) ) ;
#189951 = ORIENTED_EDGE ( 'NONE', *, *, #104977, .F. ) ;
#189952 = CARTESIAN_POINT ( 'NONE',  ( -11.44779964734733113, 10.10189529870398850, -3.599999963171534478 ) ) ;
#189953 = CARTESIAN_POINT ( 'NONE',  ( 4.861744415569490663, -0.5273948137594737240, 1.897533870164061831 ) ) ;
#189954 = EDGE_LOOP ( 'NONE', ( #207057, #48919, #56750, #66907 ) ) ;
#189955 = CARTESIAN_POINT ( 'NONE',  ( 6.005412763054238212, -1.926851508234005195, 0.2422190414417753623 ) ) ;
#189956 = ORIENTED_EDGE ( 'NONE', *, *, #117909, .T. ) ;
#189957 = CARTESIAN_POINT ( 'NONE',  ( -5.123001941117347080, 7.070197912760590064, 1.599625672291263179 ) ) ;
#189959 = CARTESIAN_POINT ( 'NONE',  ( 6.170199167347634628, 2.114832956739281400, -0.1575216572810705096 ) ) ;
#189958 = CARTESIAN_POINT ( 'NONE',  ( -4.610654757099099221, 7.536791762327691657, 1.199719254218452935 ) ) ;
#189960 = CARTESIAN_POINT ( 'NONE',  ( 7.065207446052794715, 9.336104335185329006, -1.443375672974064550 ) ) ;
#189962 = ORIENTED_EDGE ( 'NONE', *, *, #190238, .F. ) ;
#189961 = CARTESIAN_POINT ( 'NONE',  ( 3.861887077619485797, 0.6414691495152945455, -1.801623935260010079 ) ) ;
#189963 = CARTESIAN_POINT ( 'NONE',  ( 1.167327668269029228, -1.995579438226593894, -0.9423882379527288577 ) ) ;
#189964 = PRESENTATION_LAYER_ASSIGNMENT (  '', '', ( #68881 ) ) ;
#189965 = CARTESIAN_POINT ( 'NONE',  ( 9.405838923370980709, 3.553052382341641113, -7.381490207074687504 ) ) ;
#189966 = CARTESIAN_POINT ( 'NONE',  ( 6.164703283132928924, 0.6335332109005767931, 1.910856914995302303 ) ) ;
#189967 = DIRECTION ( 'NONE',  ( 0.7592566023653005702, 0.6507913734559639396, 0.000000000000000000 ) ) ;
#189968 = CARTESIAN_POINT ( 'NONE',  ( 6.586557105272873969, -1.791547847876047594, -0.3505316570680468979 ) ) ;
#189969 = CARTESIAN_POINT ( 'NONE',  ( 2.295452831283749440, -1.850383948470477602, 0.9288054807428182125 ) ) ;
#189970 = CARTESIAN_POINT ( 'NONE',  ( -7.386494761346872551, 7.511998731193139989, -0.7998128361456291469 ) ) ;
#189971 = CARTESIAN_POINT ( 'NONE',  ( -5.638797120722775169, 7.366710520292286901, -1.234282198493292793 ) ) ;
#189972 = CARTESIAN_POINT ( 'NONE',  ( -6.471393748265538370, 5.229711127717889596, -2.419999999999995044 ) ) ;
#189973 = CARTESIAN_POINT ( 'NONE',  ( 6.335737856287750880, 6.286115675290828264, -0.7998128361456281477 ) ) ;
#189974 = CARTESIAN_POINT ( 'NONE',  ( 4.665414256878284149, 6.536345614481700927, -1.443375672974068769 ) ) ;
#189975 = CARTESIAN_POINT ( 'NONE',  ( -0.07538891330675720481, -7.154544010627095219, 9.499700864329915007 ) ) ;
#189976 = DIRECTION ( 'NONE',  ( 0.000000000000000000, -1.000000000000000000, -0.000000000000000000 ) ) ;
#189977 = CARTESIAN_POINT ( 'NONE',  ( 1.364683531250000303, 11.06770833367473550, -0.7879004041258355073 ) ) ;
#189979 = CARTESIAN_POINT ( 'NONE',  ( -4.945692173934974178, 8.992000979557944973, 0.000000000000000000 ) ) ;
#189978 = CARTESIAN_POINT ( 'NONE',  ( 6.925078400183531713, 2.446544591822760850, 2.338552149501707422 ) ) ;
#189980 = CARTESIAN_POINT ( 'NONE',  ( 5.133366751340045830, 0.5111148723837605212, 1.657103328152222055 ) ) ;
#189981 = CARTESIAN_POINT ( 'NONE',  ( -4.928552533767591726, 5.708731696605642725, 1.199719254218462483 ) ) ;
#189982 = CARTESIAN_POINT ( 'NONE',  ( 2.606376076552410659, 2.069701014239883730, 0.05521581806712527740 ) ) ;
#189983 = CARTESIAN_POINT ( 'NONE',  ( 3.937202496034042376, -1.761399977300786901, -1.174509457245224597 ) ) ;
#189984 = CARTESIAN_POINT ( 'NONE',  ( 5.587931867126699537, 9.671004278289832001, -0.7998128361456291469 ) ) ;
#189986 = EDGE_CURVE ( 'NONE', #186977, #86388, #94097, .T. ) ;
#189985 = DIRECTION ( 'NONE',  ( -0.7592566023652990159, -0.6507913734559659380, 0.000000000000000000 ) ) ;
#189987 = CARTESIAN_POINT ( 'NONE',  ( 1.551539110526085619, 1.487754399324931365, 1.290523904849065095 ) ) ;
#189988 = CARTESIAN_POINT ( 'NONE',  ( 6.078105975125470017, 6.038708432876411791, -0.3507111650211444109 ) ) ;
#189990 = CARTESIAN_POINT ( 'NONE',  ( 0.2813230411330031044, 0.1852680230450229892, -1.903361379684164412 ) ) ;
#189989 = CARTESIAN_POINT ( 'NONE',  ( 1.001543065824772753E-15, -1.662500000000000533, 4.012584370867899430 ) ) ;
#189991 = CARTESIAN_POINT ( 'NONE',  ( 3.293229231460121031, 1.807080150709074129, 1.410200864199236293 ) ) ;
#189992 = CARTESIAN_POINT ( 'NONE',  ( 1.523764310407934808, -1.012771255265769943, -1.518815351243132161 ) ) ;
#189993 = EDGE_CURVE ( 'NONE', #161612, #136572, #160136, .T. ) ;
#189994 = CARTESIAN_POINT ( 'NONE',  ( 5.174371902270911150, 6.065797303184739420, 1.199719254218452047 ) ) ;
#189995 = CARTESIAN_POINT ( 'NONE',  ( 5.124618875841165710, 8.922546421882614709, 1.040834085586084257E-14 ) ) ;
#189996 = CARTESIAN_POINT ( 'NONE',  ( -7.670162217029145246, 9.971608557999250166, 1.599625672291295375 ) ) ;
#189997 = CARTESIAN_POINT ( 'NONE',  ( 3.427992945418765203, -1.982693224445150060, 0.3483943456095982549 ) ) ;
#189998 = CARTESIAN_POINT ( 'NONE',  ( 2.957805016080543581, -0.6199431972748243869, 1.861265166911831859 ) ) ;
#189999 = CARTESIAN_POINT ( 'NONE',  ( -8.833300774503376473, 10.26427131079744193, 1.199719254218462483 ) ) ;
#190000 = CARTESIAN_POINT ( 'NONE',  ( -6.093499974338126179, 9.196501505781426999, -1.199719254218440723 ) ) ;
#190001 = CYLINDRICAL_SURFACE ( 'NONE', #57462, 0.08000000000000041800 ) ;
#190003 = CARTESIAN_POINT ( 'NONE',  ( 4.592510532270950740, -0.3890688374885014067, -1.726373200486588377 ) ) ;
#190002 = CARTESIAN_POINT ( 'NONE',  ( 5.648407305961395508, -1.648567506571393615, 1.285558710341473621 ) ) ;
#190004 = CARTESIAN_POINT ( 'NONE',  ( -0.3282377607281330989, 2.301335450315363129, 1.224999999999980771 ) ) ;
#190005 = CARTESIAN_POINT ( 'NONE',  ( 0.7443833103580773658, 0.6396484562771963533, 2.096019810003430184 ) ) ;
#190006 = CARTESIAN_POINT ( 'NONE',  ( 5.824081541776103599, 1.678935111502709354, 0.4578980800337121848 ) ) ;
#190007 = VECTOR ( 'NONE', #152513, 1000.000000000000227 ) ;
#190008 = CARTESIAN_POINT ( 'NONE',  ( 9.237182729612253951, 9.671134694169463586, 0.7998128361456462443 ) ) ;
#190009 = CARTESIAN_POINT ( 'NONE',  ( 0.1331715793776860612, 5.723291439345874920, -2.547624684121822636 ) ) ;
#190010 = CARTESIAN_POINT ( 'NONE',  ( 6.240923344934847350, 2.292853006454723452, -0.1649963611656188323 ) ) ;
#190011 = CARTESIAN_POINT ( 'NONE',  ( 0.000000000000000000, 13.49999999999999822, -1.500000000000000222 ) ) ;
#190012 = CARTESIAN_POINT ( 'NONE',  ( 5.624279254961046526, 0.3357223255188810374, -1.700804604882939053 ) ) ;
#190013 = CARTESIAN_POINT ( 'NONE',  ( 5.547405112160277874, 1.917339678720403118, -1.018715297254897401 ) ) ;
#190014 = CARTESIAN_POINT ( 'NONE',  ( -2.788906526875773208E-15, 11.18749999999999822, -1.499999999999998446 ) ) ;
#190015 = CARTESIAN_POINT ( 'NONE',  ( -0.1001773172763717329, -2.075113514603315945, 0.4199855073994100407 ) ) ;
#190016 = CARTESIAN_POINT ( 'NONE',  ( 3.781250000000002665, 0.7852924748301846058, 1.895863743164001081 ) ) ;
#190017 = CARTESIAN_POINT ( 'NONE',  ( 6.827182134110199030, -0.004087946457608306570, 2.088967824442849341 ) ) ;
#190018 = CARTESIAN_POINT ( 'NONE',  ( 3.944294614955777600, 1.917013643722576433, 0.1899554498810165082 ) ) ;
#190019 = CARTESIAN_POINT ( 'NONE',  ( 0.7500000000000006661, 10.69791666734946212, -1.299038105676657340 ) ) ;
#190020 = CARTESIAN_POINT ( 'NONE',  ( 1.067367041543025197, -1.747990651676500029, 1.370551686305313321 ) ) ;
#190021 = VERTEX_POINT ( 'NONE', #180643 ) ;
#190022 = CARTESIAN_POINT ( 'NONE',  ( 1.499999999999990896, 4.775000000000022560, 1.214306433183764966E-14 ) ) ;
#190023 = CARTESIAN_POINT ( 'NONE',  ( 4.741601036477289810, 6.554953847355395880, 1.599625672291267398 ) ) ;
#190024 = CARTESIAN_POINT ( 'NONE',  ( 7.467843683028853263, 7.606905806488803101, 0.7998128361456341429 ) ) ;
#190025 = CARTESIAN_POINT ( 'NONE',  ( 2.860263265526213683, 0.7972832613293324711, -2.073463298260522780 ) ) ;
#190026 = CARTESIAN_POINT ( 'NONE',  ( -9.517460647113315630, 10.20605163116143821, 0.7216878364870438212 ) ) ;
#190027 = CYLINDRICAL_SURFACE ( 'NONE', #39168, 0.3999999999999997446 ) ;
#190028 = CARTESIAN_POINT ( 'NONE',  ( 6.100805936469477331, 9.101062111647635788, -1.082531754730537088 ) ) ;
#190029 = CARTESIAN_POINT ( 'NONE',  ( -8.419250203962027612, 11.80591375705560608, 1.082531754730549967 ) ) ;
#190030 = CARTESIAN_POINT ( 'NONE',  ( 5.533136088152891929, 9.469426179571447832, -0.7216878364870458196 ) ) ;
#190031 = CARTESIAN_POINT ( 'NONE',  ( 0.7916389524552720491, 1.525042296397002284, -1.319230309296010928 ) ) ;
#190033 = CARTESIAN_POINT ( 'NONE',  ( 6.865701141133224716, -0.4594653659172152071, 2.018469443450424894 ) ) ;
#190032 = CARTESIAN_POINT ( 'NONE',  ( 9.264299036839600987, 9.702770385934682551, -0.7998128361456281477 ) ) ;
#190034 = CARTESIAN_POINT ( 'NONE',  ( -10.87712779691732834, -6.655928102866995211, 0.1480828224388648917 ) ) ;
#190035 = CARTESIAN_POINT ( 'NONE',  ( 7.634649897826745857, 8.079715433652276957, 0.7216878364870267237 ) ) ;
#190036 = CARTESIAN_POINT ( 'NONE',  ( -2.425588855773942676, 2.974000657016653282, 11.41149836408661322 ) ) ;
#190037 = CARTESIAN_POINT ( 'NONE',  ( -0.6823417656250003738, 1.717708333674752730, -1.181850606188749264 ) ) ;
#190038 = CARTESIAN_POINT ( 'NONE',  ( 1.317257508235271102, -1.728110672573167639, 0.3808341387830004865 ) ) ;
#190039 = CARTESIAN_POINT ( 'NONE',  ( 6.469374514269041754, -1.702674068921444572, -0.3278888851577909658 ) ) ;
#190040 = CARTESIAN_POINT ( 'NONE',  ( 0.01093749962182561514, -1.805946196879631094, 0.3578947576599255664 ) ) ;
#190041 = CARTESIAN_POINT ( 'NONE',  ( 4.423529165095542837, -1.409716928370784661, -1.807567988613969723 ) ) ;
#190042 = CARTESIAN_POINT ( 'NONE',  ( -1.402160292154681736E-14, -0.9281249996585830830, 1.575800808251672791 ) ) ;
#190043 = CARTESIAN_POINT ( 'NONE',  ( 2.484105014303281234, -0.3146448974087300288, -1.813890345909507928 ) ) ;
#190044 = CARTESIAN_POINT ( 'NONE',  ( 9.748476143425788720, 11.33197590787365172, -1.199719254218440723 ) ) ;
#190045 = CARTESIAN_POINT ( 'NONE',  ( 6.928203230275525648, 15.00000000000000000, -9.797958971132702644 ) ) ;
#190046 = CARTESIAN_POINT ( 'NONE',  ( 2.959763373685083909, 1.816946311034864703, -0.1772020141349931188 ) ) ;
#190047 = CARTESIAN_POINT ( 'NONE',  ( 3.639296212489909532, 0.7283784247123014088, 1.880435045658496618 ) ) ;
#190048 = CARTESIAN_POINT ( 'NONE',  ( -10.10098813738111545, 11.74323990082152491, -1.199719254218441611 ) ) ;
#190050 = CARTESIAN_POINT ( 'NONE',  ( 8.964365016547233722, 14.59103508737832300, -8.971863053630826812 ) ) ;
#190049 = CARTESIAN_POINT ( 'NONE',  ( 3.977597974223236132, 2.131470459685447238, -0.7591987100158004154 ) ) ;
#190051 = CARTESIAN_POINT ( 'NONE',  ( 4.999102919943527290, 1.752478773177888582, -1.167534824283325667 ) ) ;
#190052 = CARTESIAN_POINT ( 'NONE',  ( 10.07786606378326688, 13.99524484309983130, 7.406424912067739896 ) ) ;
#190053 = CARTESIAN_POINT ( 'NONE',  ( 2.822784111170244525, -1.429543836668966561, 1.497820115680066344 ) ) ;
#190054 = CARTESIAN_POINT ( 'NONE',  ( 3.194917754314666514, 6.879154480009089134, 0.7998128361456321445 ) ) ;
#190055 = CARTESIAN_POINT ( 'NONE',  ( 1.360316468749957597, 0.7760416670081098367, 0.7853790794158520550 ) ) ;
#190056 = CARTESIAN_POINT ( 'NONE',  ( 4.776102292387626846, 2.097323840013893381, -0.3118266106481304423 ) ) ;
#190057 = CONTEXT_DEPENDENT_SHAPE_REPRESENTATION ( #43736, #43683 ) ;
#190059 = CARTESIAN_POINT ( 'NONE',  ( 0.6098321186917586845, -1.917330571200571265, 0.1878080533235688687 ) ) ;
#190058 = CARTESIAN_POINT ( 'NONE',  ( -2.941756144040970522, 5.415504020480993219, -1.082531754730543083 ) ) ;
#190060 = CARTESIAN_POINT ( 'NONE',  ( -4.167152111353897403, 5.955039778036558040, 1.599625672291270506 ) ) ;
#190061 = CARTESIAN_POINT ( 'NONE',  ( 9.420217803396747414, 9.884675613584706255, 0.7998128361456462443 ) ) ;
#190062 = CARTESIAN_POINT ( 'NONE',  ( 6.061904078641523697, 7.205214525570814210, -1.082531754730548412 ) ) ;
#190063 = CARTESIAN_POINT ( 'NONE',  ( 4.871297188390688149, 6.684807392805372395, 1.249964738027457889 ) ) ;
#190064 = CARTESIAN_POINT ( 'NONE',  ( 1.001543065824772753E-15, -0.9187499990440851638, 4.012584370867899430 ) ) ;
#190065 = CARTESIAN_POINT ( 'NONE',  ( -3.903858165731105778, 6.641919395739846799, 1.199719254218464037 ) ) ;
#190066 = CARTESIAN_POINT ( 'NONE',  ( 0.9673671849170182302, -1.746833394359051495, 1.372194155552537431 ) ) ;
#190067 = CARTESIAN_POINT ( 'NONE',  ( 1.923017885777689839, 1.964713842245609410, 0.7587240108328905386 ) ) ;
#190068 = CARTESIAN_POINT ( 'NONE',  ( -4.573896719763875574, 6.429575154514868274, -1.599625672291271394 ) ) ;
#190069 = CARTESIAN_POINT ( 'NONE',  ( 8.450809820019639318, 8.753699632978056755, -0.7998128361456291469 ) ) ;
#190070 = CARTESIAN_POINT ( 'NONE',  ( 6.825069993440997074, -1.701324435194497831, -0.7545304760708021474 ) ) ;
#190071 = CARTESIAN_POINT ( 'NONE',  ( 6.751070424600909448, 9.963667031088037973, -1.199719254218441611 ) ) ;
#190072 = SURFACE_SIDE_STYLE ('',( #172778 ) ) ;
#190073 = CARTESIAN_POINT ( 'NONE',  ( -7.132998214565509087, 7.494455136514109661, 0.7216878364870317197 ) ) ;
#190074 = CARTESIAN_POINT ( 'NONE',  ( -7.537970219518066450, 11.73812298950569044, -0.7216878364870267237 ) ) ;
#190075 = CARTESIAN_POINT ( 'NONE',  ( -0.01710467543277957581, -1.380256469788909035, 1.610041658517608054 ) ) ;
#190076 = CARTESIAN_POINT ( 'NONE',  ( -5.576146316970437944, 9.727530813099326323, 0.000000000000000000 ) ) ;
#190078 = CARTESIAN_POINT ( 'NONE',  ( 3.051168888765115828, 1.684027830550902882, -1.006202029777767848 ) ) ;
#190077 = CARTESIAN_POINT ( 'NONE',  ( 1.224999999999957012, -0.8958333333332680892, 0.7072540797572596238 ) ) ;
#190079 = CARTESIAN_POINT ( 'NONE',  ( 2.624079441566569582, -1.243859440641072123, -1.767801033134681843 ) ) ;
#190081 = CARTESIAN_POINT ( 'NONE',  ( -5.312752313518235958, 6.384578190230367767, -1.125208257168613502 ) ) ;
#190080 = CARTESIAN_POINT ( 'NONE',  ( -3.797165540279144214, 6.587721009371067638, 1.199719254218452935 ) ) ;
#190082 = CARTESIAN_POINT ( 'NONE',  ( 1.364683531249988757, 1.884375000341421913, 0.000000000000000000 ) ) ;
#190083 = CARTESIAN_POINT ( 'NONE',  ( 3.960698422707895627, 0.2102999545306425688, -1.727497421908174458 ) ) ;
#190084 = CARTESIAN_POINT ( 'NONE',  ( 5.314433026876846711, 9.143996264757578984, -0.7216878364870267237 ) ) ;
#190085 = CARTESIAN_POINT ( 'NONE',  ( -12.45759369916135029, 8.320971494343229580, 2.471636155840711169 ) ) ;
#190086 = ORIENTED_EDGE ( 'NONE', *, *, #97862, .T. ) ;
#190087 = CARTESIAN_POINT ( 'NONE',  ( 2.056017322730230301, 1.755501262438976751, -0.9912458455646618871 ) ) ;
#190088 = CARTESIAN_POINT ( 'NONE',  ( 6.825078400183544503, 6.034152930826206962, 2.739236550662868197 ) ) ;
#190089 = CARTESIAN_POINT ( 'NONE',  ( -4.981695098378565945, 4.776675467721892332, -0.7998128361456362523 ) ) ;
#190090 = CARTESIAN_POINT ( 'NONE',  ( 1.938291742056476030, 1.949724373066508143, 0.2912656003557292927 ) ) ;
#190092 = ORIENTED_EDGE ( 'NONE', *, *, #135275, .T. ) ;
#190091 = CARTESIAN_POINT ( 'NONE',  ( -4.312902262922974295, 8.045820050136510915, 0.7216878364870338292 ) ) ;
#190093 = CARTESIAN_POINT ( 'NONE',  ( -6.305950843687521790, 7.489935751457798219, 1.082531754730548412 ) ) ;
#190094 = CARTESIAN_POINT ( 'NONE',  ( 5.525830126021535449, 8.604496359403894346, -1.199719254218452047 ) ) ;
#190095 = CARTESIAN_POINT ( 'NONE',  ( -6.479871072688648148, 6.524547437750345402, 0.000000000000000000 ) ) ;
#190096 = CARTESIAN_POINT ( 'NONE',  ( 2.016276777042900203, -2.019190368190917795, 0.05175015523710930349 ) ) ;
#190097 = CARTESIAN_POINT ( 'NONE',  ( 1.347111479062087616E-15, -9.999999999999994671, -10.99999999999999112 ) ) ;
#190098 = EDGE_CURVE ( 'NONE', #108269, #207703, #176860, .T. ) ;
#190099 = CARTESIAN_POINT ( 'NONE',  ( 6.036188935239226616, 1.144513723677667461, -2.003705632283636184 ) ) ;
#190100 = FACE_OUTER_BOUND ( 'NONE', #203841, .T. ) ;
#190101 = CARTESIAN_POINT ( 'NONE',  ( 3.239059677355364375, -0.1396402669299641186, -1.956817938210092089 ) ) ;
#190102 = CARTESIAN_POINT ( 'NONE',  ( 7.886038904643079661, 12.35212915539230139, -0.7998128361456352531 ) ) ;
#190103 = CARTESIAN_POINT ( 'NONE',  ( 1.020157974382044364, -1.821741137083273010, 0.8647263380179845971 ) ) ;
#190104 = ORIENTED_EDGE ( 'NONE', *, *, #154690, .T. ) ;
#190105 = CARTESIAN_POINT ( 'NONE',  ( 1.903655596893740087, -2.052436370740511773, 0.5197080100793128876 ) ) ;
#190107 = CARTESIAN_POINT ( 'NONE',  ( -6.826694039680798021, 7.923230120171105284, -1.199719254218446718 ) ) ;
#190106 = CARTESIAN_POINT ( 'NONE',  ( 3.469446951953614189E-15, 6.400000000000023448, 1.214306433183764966E-14 ) ) ;
#190108 = CARTESIAN_POINT ( 'NONE',  ( 2.448939195788137013, 0.4911642875529352303, -1.774347143093172097 ) ) ;
#190109 = ORIENTED_EDGE ( 'NONE', *, *, #170070, .T. ) ;
#190110 = CARTESIAN_POINT ( 'NONE',  ( -10.62011439820619429, 11.28455497419572318, -0.7998128361456221525 ) ) ;
#190111 = CARTESIAN_POINT ( 'NONE',  ( 3.146849984228027974, 2.069795010335002239, 0.4607391970517027979 ) ) ;
#190112 = CARTESIAN_POINT ( 'NONE',  ( 0.02305342982030639601, -1.130023889514218505, -1.454075609423427728 ) ) ;
#190113 = CARTESIAN_POINT ( 'NONE',  ( 0.7499999999999902300, 4.847916667349482012, -1.299038105676658228 ) ) ;
#190114 = CARTESIAN_POINT ( 'NONE',  ( 6.805303039055573322, 10.02693841461847057, 1.199719254218460707 ) ) ;
#190115 = CARTESIAN_POINT ( 'NONE',  ( 5.677832469072920496, 9.846164657218904992, 0.000000000000000000 ) ) ;
#190116 = CARTESIAN_POINT ( 'NONE',  ( 4.675106833541732954, 0.004019643978107888781, -2.060967561157340810 ) ) ;
#190117 = AXIS2_PLACEMENT_3D ( 'NONE', #185592, #416, #51349 ) ;
#190119 = CARTESIAN_POINT ( 'NONE',  ( 1.329379181053941483, 0.9071106928158387817, -1.602193565413398968 ) ) ;
#190118 = CARTESIAN_POINT ( 'NONE',  ( -6.201965203247477909, 9.323044272842313518, 1.199719254218452047 ) ) ;
#190120 = CARTESIAN_POINT ( 'NONE',  ( 1.364683531249990311, 4.613541667008083103, 0.7879004041258500513 ) ) ;
#190121 = CARTESIAN_POINT ( 'NONE',  ( -0.02244404828157658613, 0.6916080914694566761, -2.270927585766496559 ) ) ;
#190122 = CARTESIAN_POINT ( 'NONE',  ( -1.569538198872308055, 8.730447571940807450, 2.495330465740724701 ) ) ;
#190123 = CARTESIAN_POINT ( 'NONE',  ( 0.000000000000000000, -0.5000000000000004441, 0.000000000000000000 ) ) ;
#190124 = CARTESIAN_POINT ( 'NONE',  ( 1.067327838873022516, -1.996528553209110379, -0.9406146916221403975 ) ) ;
#190125 = CARTESIAN_POINT ( 'NONE',  ( 3.233911077135812384, -1.516719621523674677, -1.678889276187053081 ) ) ;
#190126 = CARTESIAN_POINT ( 'NONE',  ( -8.405692050792730186, 9.869357483088723626, 1.082531754730558626 ) ) ;
#190127 = CARTESIAN_POINT ( 'NONE',  ( 3.709066938097814514, 1.527391393591450486, -0.9738182928965555263 ) ) ;
#190128 = CARTESIAN_POINT ( 'NONE',  ( 3.256958599878871485, 0.04175330623504669436, -1.915424027289241993 ) ) ;
#190129 = CARTESIAN_POINT ( 'NONE',  ( 4.773920332862017446, -2.031068740936771366, 0.4005940302675218834 ) ) ;
#190130 = CARTESIAN_POINT ( 'NONE',  ( -0.6823417656250003738, 2.530208333674753618, -1.181850606188749264 ) ) ;
#190131 = CARTESIAN_POINT ( 'NONE',  ( 3.186357099593698283, -1.942036093696447363, -0.3385421596419062595 ) ) ;
#190132 = CARTESIAN_POINT ( 'NONE',  ( 1.377817859240665577, 1.145177193861897758, 1.548917676831958801 ) ) ;
#190133 = CARTESIAN_POINT ( 'NONE',  ( 3.502682687546424312, 1.475339254275360279, -1.149998991230333223 ) ) ;
#190135 = EDGE_CURVE ( 'NONE', #108645, #824, #125133, .T. ) ;
#190134 = CIRCLE ( 'NONE', #48392, 8.049999999999993605 ) ;
#190136 = CARTESIAN_POINT ( 'NONE',  ( 2.473609491499198398, 0.1116694970143172483, -2.305109432965181337 ) ) ;
#190137 = CARTESIAN_POINT ( 'NONE',  ( 4.246440214068532448, -1.840602306905499086, -0.2743259802632999622 ) ) ;
#190138 = CARTESIAN_POINT ( 'NONE',  ( 0.6823417656249899377, 4.426041667008086655, -1.181850606188754593 ) ) ;
#190139 = CARTESIAN_POINT ( 'NONE',  ( -4.924636110261798372, 6.768494766770632332, 1.599625672291267398 ) ) ;
#190140 = CARTESIAN_POINT ( 'NONE',  ( 7.124973419181436007, 8.271222729588529887, -1.199719254218446718 ) ) ;
#190141 = CARTESIAN_POINT ( 'NONE',  ( 6.764898216727350366, -7.628386336122866318, 6.764898216730284020 ) ) ;
#190142 = CARTESIAN_POINT ( 'NONE',  ( 0.1179828827667589730, -2.064941173381201978, 0.4132506003948192563 ) ) ;
#190143 = CARTESIAN_POINT ( 'NONE',  ( 4.975479186090860928, 4.907073259968533385, 0.7216878364870317197 ) ) ;
#190145 = DIRECTION ( 'NONE',  ( 8.881784197001252323E-16, 0.000000000000000000, -1.000000000000000000 ) ) ;
#190144 = CARTESIAN_POINT ( 'NONE',  ( 1.364683531249990311, 3.446875000341416584, 1.214306433183764966E-14 ) ) ;
#190146 = CARTESIAN_POINT ( 'NONE',  ( 6.714160596891073141, -1.012370167489636819, -1.909856561116265672 ) ) ;
#190147 = CARTESIAN_POINT ( 'NONE',  ( 1.564851893998190135, 0.6701894319398638000, 2.011955567234039677 ) ) ;
#190148 = CARTESIAN_POINT ( 'NONE',  ( 0.7912781446984231692, -0.05379174966265751895, -2.019256707098691095 ) ) ;
#190149 = CARTESIAN_POINT ( 'NONE',  ( 0.6823417656249882723, 1.426041667008083547, -1.181850606188749264 ) ) ;
#190150 = CARTESIAN_POINT ( 'NONE',  ( -3.578989364327652467, 6.158942777482099729, 1.082531754730560403 ) ) ;
#190151 = CARTESIAN_POINT ( 'NONE',  ( 6.484877546038077867, 6.460111979999551224, 1.040834085586084257E-14 ) ) ;
#190152 = CARTESIAN_POINT ( 'NONE',  ( 0.9839146201040609441, 1.450980403326153301, 1.602422216231303320 ) ) ;
#190155 = CARTESIAN_POINT ( 'NONE',  ( 3.226477370372293763, 6.708047998835573900, 0.7216878364870317197 ) ) ;
#190154 = CARTESIAN_POINT ( 'NONE',  ( 6.925078400183531713, 7.629137130509038300, 2.555651831298339616 ) ) ;
#190153 = CARTESIAN_POINT ( 'NONE',  ( 3.874598038455354665, 7.742391154831717692, -0.7998128361456362523 ) ) ;
#190156 = CARTESIAN_POINT ( 'NONE',  ( -3.142457743317409680, 6.888227477170756785, 0.7998128361456352531 ) ) ;
#190157 = CARTESIAN_POINT ( 'NONE',  ( 5.735564631760892595, 0.5807582108038509272, -1.931123567068816493 ) ) ;
#190159 = CARTESIAN_POINT ( 'NONE',  ( -6.414416072596849538, 7.616478518518682073, -1.082531754730549967 ) ) ;
#190158 = CARTESIAN_POINT ( 'NONE',  ( -8.459924665247381625, 11.85336729522185806, 1.082531754730560403 ) ) ;
#190160 =( REPRESENTATION_RELATIONSHIP ('NONE','NONE', #84563, #203468 ) REPRESENTATION_RELATIONSHIP_WITH_TRANSFORMATION ( #205222 )SHAPE_REPRESENTATION_RELATIONSHIP( ) );
#190161 = CARTESIAN_POINT ( 'NONE',  ( 0.000000000000000000, -3.600000000000005862, -4.500000000000000000 ) ) ;
#190163 = CARTESIAN_POINT ( 'NONE',  ( -8.012344526598182026E-15, 10.29687500034139447, -1.575800808251669460 ) ) ;
#190162 = CARTESIAN_POINT ( 'NONE',  ( 0.1634265777989383772, -2.022787333623011108, -1.013812598571243617 ) ) ;
#190164 = CARTESIAN_POINT ( 'NONE',  ( -9.053093885623068715, 11.58502883802551153, -1.599625672291263179 ) ) ;
#190166 = CARTESIAN_POINT ( 'NONE',  ( 0.2806859451011362583, 1.592165405827509650, -1.064819009530016958 ) ) ;
#190165 = CARTESIAN_POINT ( 'NONE',  ( -6.697364695026446491, 6.915939687060050467, 1.040834085586084257E-14 ) ) ;
#190167 = CARTESIAN_POINT ( 'NONE',  ( 1.364683531249986537, 0.6760416670080884316, 0.7879004041258500513 ) ) ;
#190168 = CARTESIAN_POINT ( 'NONE',  ( -6.661184041420952440, -7.215597533173327527, 6.773376349083140013 ) ) ;
#190169 = CARTESIAN_POINT ( 'NONE',  ( -1.500000000000015099, 8.979166666666666075, -0.8660254037844309360 ) ) ;
#190170 = CARTESIAN_POINT ( 'NONE',  ( 3.316762602600237475, 1.559927958434914608, 0.7363868292221543710 ) ) ;
#190171 = CARTESIAN_POINT ( 'NONE',  ( 6.668631453075247073, 8.873432343378178544, -1.599625672291281386 ) ) ;
#190172 = CARTESIAN_POINT ( 'NONE',  ( 5.017399365509065845, 8.011327138806002779, -1.199719254218450271 ) ) ;
#190173 = CARTESIAN_POINT ( 'NONE',  ( 1.159032429170350653, 0.3524738178620877571, -1.734097463706934183 ) ) ;
#190174 = CARTESIAN_POINT ( 'NONE',  ( 1.717441043944417878, 1.674910534618522906, 1.116504076032026616 ) ) ;
#190175 = CARTESIAN_POINT ( 'NONE',  ( 6.825078400183575589, -0.005632053428735600553, 2.144262460745151255 ) ) ;
#190176 = CARTESIAN_POINT ( 'NONE',  ( 4.700333112842928429, -2.206180118464650786, -0.05804534286662357823 ) ) ;
#190177 = VERTEX_POINT ( 'NONE', #47475 ) ;
#190178 = CARTESIAN_POINT ( 'NONE',  ( 7.904040366642684390, 11.20483561351640844, 1.082531754730558626 ) ) ;
#190180 = CARTESIAN_POINT ( 'NONE',  ( 3.075796161730546707, -0.8146103074460913085, 1.844718345957757188 ) ) ;
#190179 = CARTESIAN_POINT ( 'NONE',  ( 4.530007735025624704, -2.079396993832134388, 0.4145621898983055109 ) ) ;
#190182 = VERTEX_POINT ( 'NONE', #15984 ) ;
#190181 = CARTESIAN_POINT ( 'NONE',  ( 3.955163173390123799, -1.573275279051716158, 0.8980309717551668847 ) ) ;
#190183 = CARTESIAN_POINT ( 'NONE',  ( 4.899292406491845497, 6.809203455697518947, -1.599625672291273171 ) ) ;
#190184 = CARTESIAN_POINT ( 'NONE',  ( 1.674454752297813265, -1.775319108138155633, -0.5897529795871117031 ) ) ;
#190185 = CARTESIAN_POINT ( 'NONE',  ( 6.199803715563785289, -0.6102442156579389598, 1.720816905678754782 ) ) ;
#190187 = CARTESIAN_POINT ( 'NONE',  ( 2.606530347446478046, 1.805417332896454230, 0.6411187296449465389 ) ) ;
#190186 = CARTESIAN_POINT ( 'NONE',  ( -2.981903720001798597, 5.566305875722335372, -1.199719254218446718 ) ) ;
#190188 = FACE_OUTER_BOUND ( 'NONE', #73267, .T. ) ;
#190189 = SURFACE_STYLE_USAGE ( .BOTH. , #124230 ) ;
#190190 = CARTESIAN_POINT ( 'NONE',  ( -1.402160292154681736E-14, 1.259375000341419248, -1.575800808251659024 ) ) ;
#190191 = CARTESIAN_POINT ( 'NONE',  ( 6.780486220610169035, 9.003929572168926754, -1.443375672974078761 ) ) ;
#190192 = CARTESIAN_POINT ( 'NONE',  ( -4.340018570150322219, 5.196348098997705556, -1.082531754730551743 ) ) ;
#190193 = EDGE_CURVE ( 'NONE', #116046, #92739, #57159, .T. ) ;
#190194 = CARTESIAN_POINT ( 'NONE',  ( -5.250750630242457362, 9.347902511916677426, 0.000000000000000000 ) ) ;
#190195 = CARTESIAN_POINT ( 'NONE',  ( 3.445663904809421307, -1.957918079443463855, 0.8150281543025170716 ) ) ;
#190197 = CARTESIAN_POINT ( 'NONE',  ( -11.15881748666195072, 6.758040191959135079, 5.811769976250384495 ) ) ;
#190196 = CARTESIAN_POINT ( 'NONE',  ( 2.505492374191277349, 3.019799309332890314, -11.78741486268894434 ) ) ;
#190198 = CARTESIAN_POINT ( 'NONE',  ( 4.411372364376418886, -0.3401156029278085136, 1.941656249039567905 ) ) ;
#190199 = CARTESIAN_POINT ( 'NONE',  ( -0.07006079923273231258, -1.973546630392996493, 0.3967976802892440036 ) ) ;
#190200 = ORIENTED_EDGE ( 'NONE', *, *, #75043, .F. ) ;
#190201 = CARTESIAN_POINT ( 'NONE',  ( 0.5271635063940235399, -1.813475876746664772, 1.092501443452270404 ) ) ;
#190202 = CARTESIAN_POINT ( 'NONE',  ( 1.750525128138082254, -2.060206210462053988, -0.2049951091474821463 ) ) ;
#190203 = CARTESIAN_POINT ( 'NONE',  ( 5.494797395288433250, 9.632623737803665875, 0.000000000000000000 ) ) ;
#190204 = CARTESIAN_POINT ( 'NONE',  ( 4.692003678781083487, 7.631698837623355658, -1.199719254218450271 ) ) ;
#190205 = CARTESIAN_POINT ( 'NONE',  ( 5.176180785367283654, 9.260904359562321275, -0.7998128361456481317 ) ) ;
#190207 = CARTESIAN_POINT ( 'NONE',  ( 4.385172619016207918, 7.203452924572514959, 1.199719254218462483 ) ) ;
#190206 = CARTESIAN_POINT ( 'NONE',  ( 4.048837805470763662, -1.738144455908509078, -1.161405209330027555 ) ) ;
#190208 = CARTESIAN_POINT ( 'NONE',  ( 6.282224075085741433, 8.422623735723785643, 1.599625672291268286 ) ) ;
#190210 = ORIENTED_EDGE ( 'NONE', *, *, #24898, .T. ) ;
#190209 = CARTESIAN_POINT ( 'NONE',  ( 0.3108108888784698598, 1.507076236086818399, -1.004716094995859121 ) ) ;
#190211 = CARTESIAN_POINT ( 'NONE',  ( 5.988949835885216011, -0.3198878037087344306, -2.183464699167809275 ) ) ;
#190212 = CARTESIAN_POINT ( 'NONE',  ( 1.836970198721030181E-16, 13.49999999999999822, 1.500000000000000222 ) ) ;
#190213 = CARTESIAN_POINT ( 'NONE',  ( 4.436686946050734548, 2.163524548302516060, 0.4339203326570104102 ) ) ;
#190214 = CARTESIAN_POINT ( 'NONE',  ( 6.988338112840064120, 10.24047933403371502, 1.199719254218460707 ) ) ;
#190215 = CARTESIAN_POINT ( 'NONE',  ( -11.01135777277262129, 10.19999999999998153, 1.399999999999998579 ) ) ;
#190216 = ADVANCED_FACE ( 'NONE', ( #79939 ), #28000, .F. ) ;
#190217 = CARTESIAN_POINT ( 'NONE',  ( 3.070860992347378637, -1.446505282863861375, 1.250851760459831041 ) ) ;
#190218 = CARTESIAN_POINT ( 'NONE',  ( 7.397945374551106568, 11.78268670361832093, -0.7998128361456291469 ) ) ;
#190219 = CARTESIAN_POINT ( 'NONE',  ( 5.055165704564410944, 1.723227314588217318, -1.147259442322377865 ) ) ;
#190221 = CARTESIAN_POINT ( 'NONE',  ( 2.465889518630470789, 2.120156730345585938, -0.4209195040108040797 ) ) ;
#190220 = CARTESIAN_POINT ( 'NONE',  ( 1.501703635994434238, 8.650726486491324252, -2.563578082221926735 ) ) ;
#190222 = CARTESIAN_POINT ( 'NONE',  ( 6.058177568126345669, -1.550975213528119623, 1.548612826651605712 ) ) ;
#190223 = VERTEX_POINT ( 'NONE', #83132 ) ;
#190224 = VERTEX_POINT ( 'NONE', #70069 ) ;
#190225 = CARTESIAN_POINT ( 'NONE',  ( -9.537847510268184337, -7.985988503423656404, 0.1421055763938848249 ) ) ;
#190226 = CARTESIAN_POINT ( 'NONE',  ( -0.02500845152586464101, 3.700502905159948508, 11.79962023279682271 ) ) ;
#190227 = CARTESIAN_POINT ( 'NONE',  ( 3.725458348705031231, 7.568394850123006279, -1.734723475976807094E-15 ) ) ;
#190228 = CARTESIAN_POINT ( 'NONE',  ( -1.364683531250000748, 15.17187500034139447, 0.000000000000000000 ) ) ;
#190229 = FILL_AREA_STYLE ('',( #89565 ) ) ;
#190230 = CARTESIAN_POINT ( 'NONE',  ( -7.456621297836087514, 9.722477485607340597, 1.443375672974090751 ) ) ;
#190231 = CARTESIAN_POINT ( 'NONE',  ( 4.389807875774629942, 8.343469298370917997, 0.7998128361456271485 ) ) ;
#190232 = CARTESIAN_POINT ( 'NONE',  ( 5.682505902380680318, 1.237739610710282046, -1.659335868388504220 ) ) ;
#190233 = CARTESIAN_POINT ( 'NONE',  ( 4.107974109700462506, -1.921244671385572422, 0.1431019773510885384 ) ) ;
#190234 = CARTESIAN_POINT ( 'NONE',  ( 0.5797041155359906606, -0.7231210598357665775, 1.882482590253447663 ) ) ;
#190235 = CARTESIAN_POINT ( 'NONE',  ( -10.63367255181986160, 11.30037282007833532, 1.040834085586084257E-14 ) ) ;
#190236 = CARTESIAN_POINT ( 'NONE',  ( 6.373214726875630731, 9.593111727067046957, 1.199719254218452047 ) ) ;
#190238 = EDGE_CURVE ( 'NONE', #111140, #136413, #166476, .T. ) ;
#190237 = CARTESIAN_POINT ( 'NONE',  ( -4.510196435976065565, 7.040407170307378060, -1.149263043085164915 ) ) ;
#190239 = CARTESIAN_POINT ( 'NONE',  ( 0.8322822162843239724, 2.159637434087835928, 0.3711470721824081109 ) ) ;
#190240 = CARTESIAN_POINT ( 'NONE',  ( 4.811078068098579408, 1.589968679568127596, 0.8971634079883784585 ) ) ;
#190241 = ADVANCED_FACE ( 'NONE', ( #197457 ), #192105, .T. ) ;
#190242 = CARTESIAN_POINT ( 'NONE',  ( 6.387299765813869712, 6.624473612970537495, 0.000000000000000000 ) ) ;
#190243 = CARTESIAN_POINT ( 'NONE',  ( 3.592547517496925913, 5.214391408544949869, -1.443375672974058777 ) ) ;
#190244 = CARTESIAN_POINT ( 'NONE',  ( -4.793689830883590020, 7.750332681742931662, 1.199719254218452935 ) ) ;
#190245 = CARTESIAN_POINT ( 'NONE',  ( 3.718679271898170491, 7.560485927181699317, 0.7998128361456271485 ) ) ;
#190246 = VERTEX_POINT ( 'NONE', #83705 ) ;
#190248 = CARTESIAN_POINT ( 'NONE',  ( 5.748296788003684377, 0.9886478197097836595, -1.753632158501418514 ) ) ;
#190247 = CARTESIAN_POINT ( 'NONE',  ( 3.210337823311388394, 1.665856106666419034, 0.7845605768846477535 ) ) ;
#190249 = CARTESIAN_POINT ( 'NONE',  ( 1.247910673863032116, -2.242740372501272006, -0.5020730165456227523 ) ) ;
#190250 = CARTESIAN_POINT ( 'NONE',  ( 6.508651776674191147, 0.6122461511635870490, 1.863871573545019533 ) ) ;
#190251 = CARTESIAN_POINT ( 'NONE',  ( -5.636439174979254396, 7.598931675607687453, -1.599625672291256295 ) ) ;
#190252 = CARTESIAN_POINT ( 'NONE',  ( 9.765991159990626613, -7.287292132425312374, 9.269928574751062911E-15 ) ) ;
#190253 = CARTESIAN_POINT ( 'NONE',  ( -3.704402285031864306, 5.344888637335695414, -1.599625672291256295 ) ) ;
#190254 = CARTESIAN_POINT ( 'NONE',  ( 0.3091450132529197647, -1.663722454078466306, 1.232067777400827069 ) ) ;
#190255 = CARTESIAN_POINT ( 'NONE',  ( -7.268579750702160780, 8.613002809641560731, -1.082531754730549967 ) ) ;
#190257 = CARTESIAN_POINT ( 'NONE',  ( 1.041631754505952134, 0.7616270086890539748, -1.708776438048253077 ) ) ;
#190256 = CARTESIAN_POINT ( 'NONE',  ( 2.735971011012145127, 2.075282486531265569, 0.2531079119270570610 ) ) ;
#190258 = CARTESIAN_POINT ( 'NONE',  ( 1.475935241056694602, 1.776738309990203213, 0.9528675108748105860 ) ) ;
#190259 = CARTESIAN_POINT ( 'NONE',  ( 8.514157279702022407, 10.95626946445095307, -1.443375672974063439 ) ) ;
#190260 = ORIENTED_EDGE ( 'NONE', *, *, #191685, .T. ) ;
#190261 = CARTESIAN_POINT ( 'NONE',  ( 0.6823417656249917140, 4.405208333674755394, 1.181850606188765695 ) ) ;
#190262 = CARTESIAN_POINT ( 'NONE',  ( 2.559766225087984903, -1.198919528351283681, 1.261881593406234403 ) ) ;
#190263 = CARTESIAN_POINT ( 'NONE',  ( 4.527533231959700366, 7.369540306339926516, 1.199719254218462483 ) ) ;
#190265 = CARTESIAN_POINT ( 'NONE',  ( -2.791122189554258290E-19, 3.467171072964057910, 11.99762841690770365 ) ) ;
#190264 = SURFACE_SIDE_STYLE ('',( #141576 ) ) ;
#190266 = CARTESIAN_POINT ( 'NONE',  ( 2.877275982374318364, 1.637783285604855088, -0.5413683153251740432 ) ) ;
#190267 =( BOUNDED_CURVE ( )  B_SPLINE_CURVE ( 3, ( #172092, #71353, #5276, #206705 ),
 .UNSPECIFIED., .F., .T. ) 
 B_SPLINE_CURVE_WITH_KNOTS ( ( 4, 4 ),
 ( 0.000000000000000000, 0.4999999999999992784 ),
 .UNSPECIFIED. ) 
 CURVE ( )  GEOMETRIC_REPRESENTATION_ITEM ( )  RATIONAL_B_SPLINE_CURVE ( ( 1.000000000000000000, 0.3333333333333343140, 0.3333333333333333703, 0.9999999999999990008 ) ) 
 REPRESENTATION_ITEM ( '' )  );
#190268 = CARTESIAN_POINT ( 'NONE',  ( 3.157961424266928052, 0.9873743524775533409, 1.956624655947765357 ) ) ;
#190269 = CARTESIAN_POINT ( 'NONE',  ( 5.233140740401229785, 0.1595256157847015632, 2.201181388321731269 ) ) ;
#190270 = CARTESIAN_POINT ( 'NONE',  ( -10.14895191580505163, 4.000029896383376027, -7.601392964056682189 ) ) ;
#190271 = CARTESIAN_POINT ( 'NONE',  ( 2.501036472447940362, 0.4719354416190780777, 2.119019701963683833 ) ) ;
#190272 = CARTESIAN_POINT ( 'NONE',  ( 1.471042373949003501, 0.1361147407585860392, -1.820667060309004937 ) ) ;
#190273 = CARTESIAN_POINT ( 'NONE',  ( 3.907494643824228397, -2.025022917198250560, 0.6182885518764801303 ) ) ;
#190274 = CARTESIAN_POINT ( 'NONE',  ( 6.539320575229236709, 2.970193638644866851, 2.450124720169952752 ) ) ;
#190275 = ORIENTED_EDGE ( 'NONE', *, *, #58624, .F. ) ;
#190277 = CARTESIAN_POINT ( 'NONE',  ( 1.364683531249986537, 1.717708333674749399, -0.7879004041258239610 ) ) ;
#190276 = CARTESIAN_POINT ( 'NONE',  ( 3.790815982946276641, 1.936215313137353178, -1.226956277148362862 ) ) ;
#190278 = CARTESIAN_POINT ( 'NONE',  ( -1.326716514427061987E-15, 2.999999999999988454, -1.225000000000003864 ) ) ;
#190279 = CARTESIAN_POINT ( 'NONE',  ( 3.192055101013606233, 5.811482486902795230, -1.199719254218446718 ) ) ;
#190280 = CARTESIAN_POINT ( 'NONE',  ( 0.04773460823432121303, -1.936894771697717621, 0.8635138731061947626 ) ) ;
#190281 = CARTESIAN_POINT ( 'NONE',  ( -6.561783159334145132, 6.757761228752363181, -0.7216878364870278340 ) ) ;
#190282 = VECTOR ( 'NONE', #113965, 1000.000000000000114 ) ;
#190283 = CARTESIAN_POINT ( 'NONE',  ( 4.392478581147586603, 4.226905887534702977, -0.7216878364870188411 ) ) ;
#190284 = CARTESIAN_POINT ( 'NONE',  ( -6.860062538390436337, 7.105753837651378468, 1.040834085586084257E-14 ) ) ;
#190285 = CARTESIAN_POINT ( 'NONE',  ( 0.03750003396568112046, -9.978860739388867529, 10.91964959838802507 ) ) ;
#190286 = ORIENTED_EDGE ( 'NONE', *, *, #110968, .T. ) ;
#190287 = CARTESIAN_POINT ( 'NONE',  ( 4.553361389630797618, -1.314998166741452090, 1.528740011303417745 ) ) ;
#190289 = CARTESIAN_POINT ( 'NONE',  ( 3.309489505334945569, -1.683523595015530505, -1.191345380358753925 ) ) ;
#190288 = CARTESIAN_POINT ( 'NONE',  ( 5.961834861707224320, 7.978559976790334574, -1.599625672291262513 ) ) ;
#190290 = CARTESIAN_POINT ( 'NONE',  ( 6.912678218121202534, 9.158153569265168770, 1.599625672291268286 ) ) ;
#190291 = CARTESIAN_POINT ( 'NONE',  ( 4.706088717274906408, 5.623429937309770921, 1.082531754730549078 ) ) ;
#190292 = CARTESIAN_POINT ( 'NONE',  ( 1.001543065824772753E-15, -2.471874999522041705, 3.793834371823811669 ) ) ;
#190293 = CARTESIAN_POINT ( 'NONE',  ( 6.404242042726283834, 1.626525233829802408, -1.468802942141099299 ) ) ;
#190294 = CARTESIAN_POINT ( 'NONE',  ( 3.656875104409584853, 1.122498086849915921, 1.674887873639265390 ) ) ;
#190295 = CARTESIAN_POINT ( 'NONE',  ( 3.016969003575611818, -1.773741936391802332, 0.4936923545346691977 ) ) ;
#190296 = CARTESIAN_POINT ( 'NONE',  ( 7.253775878511261155, 8.421492265473332850, 1.199719254218462483 ) ) ;
#190297 = CARTESIAN_POINT ( 'NONE',  ( 6.264658373536385660, -1.288822541704701452, 1.293195164663100583 ) ) ;
#190298 = CARTESIAN_POINT ( 'NONE',  ( 0.2472849680876147149, 2.272430822888141133, -0.3459996173978163725 ) ) ;
#190299 = CARTESIAN_POINT ( 'NONE',  ( -5.713871673155502151, 8.753601821068331290, 1.199719254218452047 ) ) ;
#190300 = CARTESIAN_POINT ( 'NONE',  ( 6.280173827431851485, -1.216757814587710929, 1.907326054681435235 ) ) ;
#190301 = CARTESIAN_POINT ( 'NONE',  ( 2.174573150871310201, -1.294977634586411908, 1.660803824364719405 ) ) ;
#190302 = CARTESIAN_POINT ( 'NONE',  ( -6.608673532018475960, 6.674816973635147477, -0.7998128361456362523 ) ) ;
#190303 = CARTESIAN_POINT ( 'NONE',  ( 8.535021395002688749, 9.916278701380017324, 1.199719254218462483 ) ) ;
#190304 = CARTESIAN_POINT ( 'NONE',  ( 7.648208051440442468, 8.095533279534887328, 0.000000000000000000 ) ) ;
#190305 = CARTESIAN_POINT ( 'NONE',  ( -5.526920175865215334, 9.599823971818089774, 0.7998128361456481317 ) ) ;
#190306 = FACE_OUTER_BOUND ( 'NONE', #175612, .T. ) ;
#190307 = CARTESIAN_POINT ( 'NONE',  ( 5.951666246274784910, 9.887435020721849099, 0.7216878364870438212 ) ) ;
#190308 = CARTESIAN_POINT ( 'NONE',  ( 4.414360472080629094, 7.100309700288360837, -1.094782333960819809 ) ) ;
#190309 = CARTESIAN_POINT ( 'NONE',  ( -4.225337428953291230, 8.081310767087481750, 0.7998128361456341429 ) ) ;
#190311 = CARTESIAN_POINT ( 'NONE',  ( 3.691809873939347675, 2.090716244852005357, -0.7509968985505171002 ) ) ;
#190310 = CARTESIAN_POINT ( 'NONE',  ( 2.250376613284802207, 0.9954810856505689198, -1.872389709364124188 ) ) ;
#190312 = CARTESIAN_POINT ( 'NONE',  ( 0.7268461993804631316, 0.1648446022758827123, 2.185306563462440899 ) ) ;
#190313 = CARTESIAN_POINT ( 'NONE',  ( 0.2939702064862387276, 1.638257335637434364, 1.478849500172851217 ) ) ;
#190314 = CARTESIAN_POINT ( 'NONE',  ( -5.635349125135588721, 6.603604063193491136, 1.199719254218452935 ) ) ;
#190315 = CARTESIAN_POINT ( 'NONE',  ( 4.685966490639408732, -1.205361723144786845, -1.547842780461285761 ) ) ;
#190316 = CARTESIAN_POINT ( 'NONE',  ( 8.215351014876830504, 11.67199438640995801, -1.199719254218446718 ) ) ;
#190317 = CARTESIAN_POINT ( 'NONE',  ( -5.526177461252244960, 6.240421959547291841, 0.9601993850730760061 ) ) ;
#190318 = DIRECTION ( 'NONE',  ( 0.000000000000000000, 0.2129637811552522741, -0.9770600943217657708 ) ) ;
#190319 = CARTESIAN_POINT ( 'NONE',  ( -1.364683531250014514, 1.238541667008091096, -0.7879004041258289570 ) ) ;
#190320 = CARTESIAN_POINT ( 'NONE',  ( -4.095971805104331231, 5.871996087412059140, 1.443375672974065660 ) ) ;
#190322 = EDGE_LOOP ( 'NONE', ( #182034, #54098, #108342, #210878, #16389, #192070 ) ) ;
#190321 = CARTESIAN_POINT ( 'NONE',  ( -5.965224400332865606, 7.022145224218852455, 1.082531754730549967 ) ) ;
#190323 =( BOUNDED_CURVE ( )  B_SPLINE_CURVE ( 2, ( #165447, #31201, #35440, #82059, #167588, #19189, #99394, #130888, #49564 ),
 .UNSPECIFIED., .F., .T. ) 
 B_SPLINE_CURVE_WITH_KNOTS ( ( 3, 2, 2, 2, 3 ),
 ( 0.6517857142857143016, 0.6547619047619047672, 0.6607142857142856984, 0.6666666666666666297, 0.6696428571428570953 ),
 .UNSPECIFIED. ) 
 CURVE ( )  GEOMETRIC_REPRESENTATION_ITEM ( )  RATIONAL_B_SPLINE_CURVE ( ( 0.9330127018922194093, 0.9330127018922194093, 1.000000000000000000, 0.8660254037844387076, 1.000000000000000000, 0.8660254037844387076, 1.000000000000000000, 0.9330127018922206306, 0.9330127018922194093 ) ) 
 REPRESENTATION_ITEM ( '' )  );
#190324 = CARTESIAN_POINT ( 'NONE',  ( 3.709332143218791789, 1.789599998243587731, -1.137392358348317201 ) ) ;
#190325 = CARTESIAN_POINT ( 'NONE',  ( -6.102578539926875933, 10.13377570664109051, 0.7216878364870267237 ) ) ;
#190326 = CARTESIAN_POINT ( 'NONE',  ( 5.981359018292748075, 1.999130597612966742, -0.8229454869796914984 ) ) ;
#190327 = CARTESIAN_POINT ( 'NONE',  ( 3.772867777003403589, 1.732451475078290448, -0.6238847238279123797 ) ) ;
#190328 = CARTESIAN_POINT ( 'NONE',  ( -5.602744053211161201, 6.190815373437144942, 0.8771416995774529157 ) ) ;
#190329 = CARTESIAN_POINT ( 'NONE',  ( 0.6823417656249882723, 1.988541667008083991, -1.181850606188749264 ) ) ;
#190330 = CARTESIAN_POINT ( 'NONE',  ( -0.1123202547218312558, -0.3730905450354308206, -1.705658634530213602 ) ) ;
#190331 = CARTESIAN_POINT ( 'NONE',  ( 6.827182134110203471, 2.976138737189625516, 2.364467684523130497 ) ) ;
#190332 = CARTESIAN_POINT ( 'NONE',  ( 2.846849069189655967, 5.304779099821139710, -1.082531754730543083 ) ) ;
#190333 = LINE ( 'NONE', #91812, #73702 ) ;
#190334 = VECTOR ( 'NONE', #62369, 1000.000000000000000 ) ;
#190335 = CARTESIAN_POINT ( 'NONE',  ( 4.575171270262055501, 0.003154952768896768234, -2.161883445794945846 ) ) ;
#190336 = CARTESIAN_POINT ( 'NONE',  ( 5.747422657745248742, -1.966344092054626680, -0.4444320411668146731 ) ) ;
#190337 = CARTESIAN_POINT ( 'NONE',  ( -7.144783764277399030, 11.27940545839156528, 0.7216878364870458196 ) ) ;
#190338 = CARTESIAN_POINT ( 'NONE',  ( 3.959979445722985325, 2.145676688911036578, -0.2621329562078680842 ) ) ;
#190339 = CARTESIAN_POINT ( 'NONE',  ( 3.550034410471062163, 1.971530340838826278, 0.003394978380427334484 ) ) ;
#190340 = CARTESIAN_POINT ( 'NONE',  ( -0.03969736035582727834, -7.921780080556630743, 11.00000000000013145 ) ) ;
#190341 = CARTESIAN_POINT ( 'NONE',  ( 1.554236647822554218, 0.6679093176565461532, -2.208796357520240949 ) ) ;
#190342 = CARTESIAN_POINT ( 'NONE',  ( 3.356764223755447141, -1.562743594079138321, 1.343508228479517230 ) ) ;
#190343 = CARTESIAN_POINT ( 'NONE',  ( 5.196799823744689739, 1.589972550305688070, 1.114921412299192172 ) ) ;
#190345 = EDGE_LOOP ( 'NONE', ( #77548, #75065, #204600, #200600 ) ) ;
#190344 = CARTESIAN_POINT ( 'NONE',  ( -7.009202228140744673, 10.16085778526412042, -1.082531754730537088 ) ) ;
#190346 = CARTESIAN_POINT ( 'NONE',  ( -5.875479466675803231, 7.948088359245467416, -1.599625672291271394 ) ) ;
#190347 = CARTESIAN_POINT ( 'NONE',  ( -4.858757509019059562, 5.629766575900002401, 2.420000000000000373 ) ) ;
#190349 = ORIENTED_EDGE ( 'NONE', *, *, #139587, .F. ) ;
#190348 = CARTESIAN_POINT ( 'NONE',  ( -1.980939963429228401, 3.482546949474376596, -0.4617747962884479751 ) ) ;
#190350 = CARTESIAN_POINT ( 'NONE',  ( -6.683806541412756985, 10.74159869838281622, -0.7216878364870267237 ) ) ;
#190351 = CARTESIAN_POINT ( 'NONE',  ( 1.940722911589174204, 2.182806717142399489, 0.3235914145361811767 ) ) ;
#190352 = CARTESIAN_POINT ( 'NONE',  ( 3.285556943750000070, -3.871874999522042504, 0.000000000000000000 ) ) ;
#190353 = CARTESIAN_POINT ( 'NONE',  ( 6.315287901512626867, -1.680818388338392699, -1.011408691396285420 ) ) ;
#190354 = CARTESIAN_POINT ( 'NONE',  ( -0.1291982275798807533, 2.865258409039960430, -2.562285117308207294 ) ) ;
#190355 = CARTESIAN_POINT ( 'NONE',  ( 1.499999999999989120, 5.035416667349487341, 0.8660254037844524744 ) ) ;
#190356 = CARTESIAN_POINT ( 'NONE',  ( 4.193801852926431373, 7.579907728022624802, -0.9040490846396221913 ) ) ;
#190358 = CARTESIAN_POINT ( 'NONE',  ( -10.98676690055265581, -7.666862915010298707, 0.5459353850038998202 ) ) ;
#190357 = FACE_OUTER_BOUND ( 'NONE', #77505, .T. ) ;
#190359 = CARTESIAN_POINT ( 'NONE',  ( 4.980324010294663317, -0.2286266671043569454, -1.826820671449409295 ) ) ;
#190360 = ORIENTED_EDGE ( 'NONE', *, *, #133034, .T. ) ;
#190361 = CARTESIAN_POINT ( 'NONE',  ( 2.483339057139447803, 1.884786786457379737, -0.8339860623947179530 ) ) ;
#190362 = CARTESIAN_POINT ( 'NONE',  ( 1.360316468749953600, 0.4947916670081083934, 0.7853790794158861388 ) ) ;
#190363 = CARTESIAN_POINT ( 'NONE',  ( -6.880926654135487652, 7.986501503701545879, 1.199719254218450271 ) ) ;
#190364 = CARTESIAN_POINT ( 'NONE',  ( 0.07680821025393774759, 7.629137130509076492, -2.410791881123967251 ) ) ;
#190365 = CARTESIAN_POINT ( 'NONE',  ( -10.10176665042269839, 1.000000000000000888, -6.279211784079198999 ) ) ;
#190366 = CARTESIAN_POINT ( 'NONE',  ( 3.825371897350130723, 7.614684313550482031, 0.7998128361456321445 ) ) ;
#190367 = EDGE_CURVE ( 'NONE', #118273, #55414, #50251, .T. ) ;
#190368 = CARTESIAN_POINT ( 'NONE',  ( 1.358354339613274675, 0.8343398477911911915, 1.884629720726511692 ) ) ;
#190370 = CARTESIAN_POINT ( 'NONE',  ( 4.827609030688454261, 0.9420861819694618111, -1.581835861328761528 ) ) ;
#190369 = CARTESIAN_POINT ( 'NONE',  ( -10.62729803237054149, 4.099240035649311942, -5.576248508406539628 ) ) ;
#190371 = CARTESIAN_POINT ( 'NONE',  ( 7.202405917357655341, 9.425892875049191488, 1.599625672291281386 ) ) ;
#190372 = CARTESIAN_POINT ( 'NONE',  ( -9.417400627377789490, 14.63813357754229294, -7.338645108920092142 ) ) ;
#190373 = COLOUR_RGB ( '', 0.72549020, 0.75294118, 0.79215686) ;
#190374 = CARTESIAN_POINT ( 'NONE',  ( -4.847922445338252118, 7.813604065273374921, -1.199719254218453823 ) ) ;
#190376 = VERTEX_POINT ( 'NONE', #294 ) ;
#190375 = CARTESIAN_POINT ( 'NONE',  ( 6.610000000000010090, 0.5825982378308904863, 2.053072689460200273 ) ) ;
#190377 = CARTESIAN_POINT ( 'NONE',  ( 4.934293700819583073, 1.136511309699510308, -1.891595316245115788 ) ) ;
#190378 = CARTESIAN_POINT ( 'NONE',  ( 0.3159878724818787066, -2.119942686789745068, 0.4214050671751194410 ) ) ;
#190379 = CARTESIAN_POINT ( 'NONE',  ( -6.073689629242165822, 7.148687991279732756, -1.082531754730544860 ) ) ;
#190380 = CARTESIAN_POINT ( 'NONE',  ( 0.1231139863388103495, 1.664874722635242277, 0.9407772870168448209 ) ) ;
#190381 = CARTESIAN_POINT ( 'NONE',  ( -0.06521966986864842497, -1.616690375843790051, 1.205047459138554045 ) ) ;
#190382 = EDGE_CURVE ( 'NONE', #102987, #177962, #15695, .T. ) ;
#190383 = CARTESIAN_POINT ( 'NONE',  ( 7.200788982189461507, 8.533913579710086239, -1.082531754730548412 ) ) ;
#190384 = CARTESIAN_POINT ( 'NONE',  ( 1.734723475976807094E-15, 1.000000000000000888, 0.000000000000000000 ) ) ;
#190385 = EDGE_CURVE ( 'NONE', #180365, #116455, #68246, .T. ) ;
#190386 = CARTESIAN_POINT ( 'NONE',  ( 6.111958284735683478, -0.6397702040911549259, 1.802229686255519603 ) ) ;
#190387 = PRESENTATION_STYLE_ASSIGNMENT (( #57205 ) ) ;
#190388 = CARTESIAN_POINT ( 'NONE',  ( 0.6900581440293825919, -1.856003987442723657, -0.2331820809091043056 ) ) ;
#190389 = CARTESIAN_POINT ( 'NONE',  ( 2.887907956677421506, -2.014008092954455265, 0.1037802451031161477 ) ) ;
#190391 = CARTESIAN_POINT ( 'NONE',  ( 4.020224483524700076, -1.082363273655801095, -1.806513482918799429 ) ) ;
#190390 = CARTESIAN_POINT ( 'NONE',  ( -9.528683032306089373, 10.01121838064558744, 0.7998128361456462443 ) ) ;
#190392 = CARTESIAN_POINT ( 'NONE',  ( 6.774270308322468459, 11.05506579301824743, 0.7998128361456462443 ) ) ;
#190394 = CARTESIAN_POINT ( 'NONE',  ( -8.202846631467911820, 9.528741477256060577, 1.199719254218462483 ) ) ;
#190393 = CARTESIAN_POINT ( 'NONE',  ( 0.7499999999999885647, -0.01666666666664401442, 1.299038105676657340 ) ) ;
#190395 = DIRECTION ( 'NONE',  ( 0.000000000000000000, 1.000000000000000000, 0.000000000000000000 ) ) ;
#190396 = CARTESIAN_POINT ( 'NONE',  ( 3.638929714444568919, 1.919204589499112323, 0.6297368113697666692 ) ) ;
#190397 = CARTESIAN_POINT ( 'NONE',  ( -0.6823417656250212460, 4.801041667008086655, 1.181850606188767472 ) ) ;
#190398 = CARTESIAN_POINT ( 'NONE',  ( 9.571693261567965294, 10.26932301469188857, 0.7216878364870438212 ) ) ;
#190399 = CARTESIAN_POINT ( 'NONE',  ( 4.499409293453607184, 1.733128992574247684, 1.291583502853070886 ) ) ;
#190400 = CARTESIAN_POINT ( 'NONE',  ( 5.189738938980948291, 9.276722205444929870, 0.000000000000000000 ) ) ;
#190401 = CARTESIAN_POINT ( 'NONE',  ( -1.499999999999997780, 5.400000000000022560, 1.214306433183764966E-14 ) ) ;
#190403 = CARTESIAN_POINT ( 'NONE',  ( 0.000000000000000000, -13.99999999999999822, 0.000000000000000000 ) ) ;
#190402 = CARTESIAN_POINT ( 'NONE',  ( 6.150558962454855561, 7.204682206732687000, 1.199719254218452047 ) ) ;
#190404 = B_SPLINE_CURVE_WITH_KNOTS ( 'NONE', 3,
 ( #22833, #88947, #155001, #56434 ),
 .UNSPECIFIED., .F., .F.,
 ( 4, 4 ),
 ( 0.001357288427014568134, 0.001636127605392573552 ),
 .UNSPECIFIED. ) ;
#190405 = CARTESIAN_POINT ( 'NONE',  ( 7.402388682937041331, 11.57994453016116587, 1.040834085586084257E-14 ) ) ;
#190407 = CARTESIAN_POINT ( 'NONE',  ( -0.1826339422288273118, -7.841768514962170755, 10.96557956857094673 ) ) ;
#190406 = CARTESIAN_POINT ( 'NONE',  ( 1.451894146256039519, 1.643730891105445346, 1.418569794807096107 ) ) ;
#190409 = CARTESIAN_POINT ( 'NONE',  ( 0.3449248370967008537, 0.5783895242766275979, -1.748133987124582012 ) ) ;
#190408 = CARTESIAN_POINT ( 'NONE',  ( -5.748293942514180799, 7.729428904398431222, -1.443375672974052559 ) ) ;
#190410 = CARTESIAN_POINT ( 'NONE',  ( -1.201851678989727383E-14, 1.571875000341420581, 1.575800808251672791 ) ) ;
#190411 = CARTESIAN_POINT ( 'NONE',  ( 3.140350738262797314, 0.5347024899306859202, 2.125194831261326911 ) ) ;
#190412 = CARTESIAN_POINT ( 'NONE',  ( 6.883263157960349155, 7.052567563008111051, 2.551962282169925711 ) ) ;
#190413 = CARTESIAN_POINT ( 'NONE',  ( 4.065478255348141445, 0.2803405965145295275, -2.245028738816820635 ) ) ;
#190414 = CARTESIAN_POINT ( 'NONE',  ( -6.344325816190970357, 9.489131654609717970, 1.199719254218452047 ) ) ;
#190415 = CARTESIAN_POINT ( 'NONE',  ( -1.001543065824772872E-14, 4.884375000341420581, 1.575800808251672791 ) ) ;
#190416 = CARTESIAN_POINT ( 'NONE',  ( 6.353009478083933459, 6.838182937092724956, 0.6209923359970755952 ) ) ;
#190417 = CARTESIAN_POINT ( 'NONE',  ( -0.7500000000000006661, 12.70833333333333570, -1.299038105676657340 ) ) ;
#190418 = CARTESIAN_POINT ( 'NONE',  ( 5.885648082108199119, 6.999582529615296700, 1.082531754730549967 ) ) ;
#190419 = CARTESIAN_POINT ( 'NONE',  ( 4.710057611840397840, -0.7560107150014344635, -1.600242281814190148 ) ) ;
#190420 = B_SPLINE_CURVE_WITH_KNOTS ( 'NONE', 3,
 ( #25097, #9918, #59739, #111761, #191856, #95477, #75992, #208110, #128040, #211308, #177767, #161525, #125897, #10972 ),
 .UNSPECIFIED., .F., .F.,
 ( 4, 2, 2, 2, 2, 2, 4 ),
 ( -5.999999999644659878E-08, 0.0007540416219186539450, 0.001508143243837304498, 0.001885194054796629666, 0.002262244865755954834, 0.002639295676715280002, 0.003016346487674605170 ),
 .UNSPECIFIED. ) ;
#190421 = CARTESIAN_POINT ( 'NONE',  ( 7.313733799568044702, 10.62010763521636214, 1.199719254218460707 ) ) ;
#190422 = CARTESIAN_POINT ( 'NONE',  ( 0.2531349071235571846, -1.691105571228457505, 1.254881668439677966 ) ) ;
#190424 = CARTESIAN_POINT ( 'NONE',  ( 1.499999999999987121, 1.504166666666690411, 0.8660254037844524744 ) ) ;
#190423 = CARTESIAN_POINT ( 'NONE',  ( 0.6823417656249969321, 11.02604166700806765, -1.181850606188757036 ) ) ;
#190425 = CARTESIAN_POINT ( 'NONE',  ( 0.9945129418027212065, 1.939812372797902862, 0.3400383455644633290 ) ) ;
#190426 = CARTESIAN_POINT ( 'NONE',  ( -9.569358774130488854, 4.446955548196734220, -7.167287524826102540 ) ) ;
#190427 = CARTESIAN_POINT ( 'NONE',  ( 6.028922772295511656, -1.701938481575874684, 1.081082441910637071 ) ) ;
#190428 = ORIENTED_EDGE ( 'NONE', *, *, #107850, .T. ) ;
#190429 = CARTESIAN_POINT ( 'NONE',  ( 8.297226821883377568, 8.782445501726501291, -0.7216878364870267237 ) ) ;
#190430 = CARTESIAN_POINT ( 'NONE',  ( 4.856247981345184428, 0.7163626499266175784, 1.728251504774950709 ) ) ;
#190431 = VERTEX_POINT ( 'NONE', #213684 ) ;
#190432 = CARTESIAN_POINT ( 'NONE',  ( 3.995033623311712301, 0.2988084191791628985, 2.048438004591215389 ) ) ;
#190433 = CARTESIAN_POINT ( 'NONE',  ( 1.224999999999955014, 2.145833333333346360, -0.7072540797573136917 ) ) ;
#190434 = CARTESIAN_POINT ( 'NONE',  ( -5.926322542504864899, 8.967774495347393682, -1.082531754730549967 ) ) ;
#190435 = CARTESIAN_POINT ( 'NONE',  ( 8.565000355531088516, 11.01558638625153286, -1.599625672291257406 ) ) ;
#190436 = CARTESIAN_POINT ( 'NONE',  ( -10.15522075183580419, 11.80651128435196462, 1.199719254218462483 ) ) ;
#190437 = CARTESIAN_POINT ( 'NONE',  ( 5.494797395288433250, 9.632623737803665875, 0.000000000000000000 ) ) ;
#190438 = B_SPLINE_CURVE_WITH_KNOTS ( 'NONE', 3,
 ( #54695, #204109, #120847, #121917, #6982, #73063, #139162, #56833 ),
 .UNSPECIFIED., .F., .F.,
 ( 4, 2, 2, 4 ),
 ( 2.544396950753999607E-07, 0.0002984430161315527606, 0.0005966315925680303707, 0.001193008745440985808 ),
 .UNSPECIFIED. ) ;
#190439 = DIRECTION ( 'NONE',  ( -5.551115123125765446E-17, 0.000000000000000000, 1.000000000000000000 ) ) ;
#190440 = CARTESIAN_POINT ( 'NONE',  ( -1.364683531250014514, -0.9697916663252473812, 0.7879004041258379498 ) ) ;
#190441 = CARTESIAN_POINT ( 'NONE',  ( 0.7499999999999885647, 0.4833333333333564297, 1.299038105676657340 ) ) ;
#190442 = CARTESIAN_POINT ( 'NONE',  ( 4.211346380768822506, -1.629847038978438079, -1.091715234301626314 ) ) ;
#190443 = CARTESIAN_POINT ( 'NONE',  ( 2.495470048217228065, 1.954872899240958972, 0.4925676099705801891 ) ) ;
#190444 = EDGE_CURVE ( 'NONE', #16927, #181635, #1769, .T. ) ;
#190445 = CARTESIAN_POINT ( 'NONE',  ( -3.135678666510573365, 6.880318554229450712, 0.000000000000000000 ) ) ;
#190446 = CARTESIAN_POINT ( 'NONE',  ( 0.4809368265653416463, 3.139971263792683764, 0.3999999999999678257 ) ) ;
#190447 = SURFACE_SIDE_STYLE ('',( #56201 ) ) ;
#190448 = CARTESIAN_POINT ( 'NONE',  ( 1.159204581426832803, 0.3705859133612994794, -1.833297903905316772 ) ) ;
#190449 = CARTESIAN_POINT ( 'NONE',  ( 0.6823417656249899377, 4.926041667008086655, -1.181850606188754593 ) ) ;
#190450 = CARTESIAN_POINT ( 'NONE',  ( 2.496342308839387680, -1.031403195114518390, 1.728778584395810114 ) ) ;
#190452 = CARTESIAN_POINT ( 'NONE',  ( 3.515340291283968632, -1.955329406025432482, 0.8124583124677657864 ) ) ;
#190451 = CARTESIAN_POINT ( 'NONE',  ( -4.758548728716557541, 8.495464583570553785, 1.040834085586084257E-14 ) ) ;
#190453 = CYLINDRICAL_SURFACE ( 'NONE', #101038, 6.249999999999995559 ) ;
#190454 = CARTESIAN_POINT ( 'NONE',  ( 4.703616579153604427, -1.598285800263723910, -1.315984976451072930 ) ) ;
#190455 = CARTESIAN_POINT ( 'NONE',  ( 6.749980374757213575, 8.968339418673846097, 1.599625672291268286 ) ) ;
#190457 = CARTESIAN_POINT ( 'NONE',  ( 6.620655732516615544, 0.0004550665019913135447, 2.073887158236031425 ) ) ;
#190456 = CARTESIAN_POINT ( 'NONE',  ( 0.5739142741672832448, -1.158190483201524179, 1.740425096305434183 ) ) ;
#190459 = VERTEX_POINT ( 'NONE', #15496 ) ;
#190458 = CARTESIAN_POINT ( 'NONE',  ( 5.737271026523679041, -1.649412122839075234, 0.7826820710771440481 ) ) ;
#190460 = CARTESIAN_POINT ( 'NONE',  ( 9.088043039861931405, 9.497138389460751284, 1.040834085586084257E-14 ) ) ;
#190461 = CARTESIAN_POINT ( 'NONE',  ( 7.966449380362733201, -6.654700410849428316, -7.586197045692575358 ) ) ;
#190462 = TOROIDAL_SURFACE ( 'NONE', #93563, 3.971937515251341644, 0.08000000000000000167 ) ;
#190463 = CARTESIAN_POINT ( 'NONE',  ( -9.978677811866239367, 3.146997876264563843, 6.103086072356673775 ) ) ;
#190464 = CARTESIAN_POINT ( 'NONE',  ( -1.364683531250010740, 12.19270833367473195, 0.7879004041258445001 ) ) ;
#190465 = CARTESIAN_POINT ( 'NONE',  ( 6.287759715630294011, 1.828497742151834027, -0.5598019499635784602 ) ) ;
#190466 = CARTESIAN_POINT ( 'NONE',  ( -8.320953590485107298, 10.73086516036454618, 1.599625672291269396 ) ) ;
#190467 = CARTESIAN_POINT ( 'NONE',  ( 6.551614543901692400, 8.666636272683888365, 1.599625672291281386 ) ) ;
#190468 = CARTESIAN_POINT ( 'NONE',  ( 0.6801582343749987825, 2.338541667008108060, -1.178068619123883165 ) ) ;
#190469 = CARTESIAN_POINT ( 'NONE',  ( 0.000000000000000000, 9.200000000000020606, 0.4000000000000166755 ) ) ;
#190470 = CARTESIAN_POINT ( 'NONE',  ( 5.820528018968444961, 5.685037531751635953, 0.7998128361456341429 ) ) ;
#190471 = ORIENTED_EDGE ( 'NONE', *, *, #196844, .T. ) ;
#190472 = STYLED_ITEM ( 'NONE', ( #65612 ), #163756 ) ;
#190473 = CARTESIAN_POINT ( 'NONE',  ( -4.911796789900812144, 8.952456364851418158, 0.7998128361456291469 ) ) ;
#190474 = CARTESIAN_POINT ( 'NONE',  ( 5.202749988929913805, 1.864175517894875789, 0.7691070904374335271 ) ) ;
#190475 = CARTESIAN_POINT ( 'NONE',  ( -3.999533323540116037, 7.701302116590127866, 0.08613759814882990251 ) ) ;
#190476 = CARTESIAN_POINT ( 'NONE',  ( -0.4000000000000109024, 3.251480759208445814, -0.4649507210925222789 ) ) ;
#190477 = CARTESIAN_POINT ( 'NONE',  ( -6.478676351974181458, 6.772485410396933858, 0.2589597434300341394 ) ) ;
#190478 = CARTESIAN_POINT ( 'NONE',  ( -4.094199201646926412, 7.720390135322642067, 0.7216878364870317197 ) ) ;
#190479 = CARTESIAN_POINT ( 'NONE',  ( 8.758204044747994743, 12.20135990463928266, 1.082531754730546636 ) ) ;
#190480 = CARTESIAN_POINT ( 'NONE',  ( 1.955843269872016066, -0.6684750375501640196, 1.852638994923772930 ) ) ;
#190481 = CARTESIAN_POINT ( 'NONE',  ( 2.864861414439429321, -0.1511590275467006306, -2.010826137130202529 ) ) ;
#190482 = CARTESIAN_POINT ( 'NONE',  ( -6.333630315878337136, 10.54098580183340772, 0.000000000000000000 ) ) ;
#190484 = EDGE_CURVE ( 'NONE', #4353, #168515, #103570, .T. ) ;
#190483 = CARTESIAN_POINT ( 'NONE',  ( 6.827182134110198142, 6.033542260787205791, 2.783941933017803905 ) ) ;
#190485 = CARTESIAN_POINT ( 'NONE',  ( 3.328257738700185264, 2.138080787187321086, 0.4799892483983853042 ) ) ;
#190486 = CYLINDRICAL_SURFACE ( 'NONE', #199047, 1.500000000000000222 ) ;
#190487 = CARTESIAN_POINT ( 'NONE',  ( 2.379798427543390105, 1.183398162072072823, 1.519983715915488531 ) ) ;
#190488 = CARTESIAN_POINT ( 'NONE',  ( -9.345647958521597687, 9.797677461230342999, 0.7998128361456462443 ) ) ;
#190489 = CARTESIAN_POINT ( 'NONE',  ( -0.1296875068448125057, 7.629137130509072939, -2.426516348560475933 ) ) ;
#190490 = CARTESIAN_POINT ( 'NONE',  ( -0.05513001983272274725, -8.135652870098727618, -11.00000000000013145 ) ) ;
#190491 = LINE ( 'NONE', #205676, #96688 ) ;
#190492 = CARTESIAN_POINT ( 'NONE',  ( 8.471147050440139381, 8.777426401801974976, -0.7998128361456281477 ) ) ;
#190493 = CARTESIAN_POINT ( 'NONE',  ( 4.364835388595708743, 7.179726155748598515, 1.199719254218462483 ) ) ;
#190494 = CARTESIAN_POINT ( 'NONE',  ( -1.225000000000060263, 1.270833333333357906, 0.7072540797572717253 ) ) ;
#190495 = CARTESIAN_POINT ( 'NONE',  ( 5.614485009834906393, 6.683225611963085733, -1.082531754730548412 ) ) ;
#190496 = ORIENTED_EDGE ( 'NONE', *, *, #45609, .F. ) ;
#190498 = CARTESIAN_POINT ( 'NONE',  ( 3.193996758133522018, 1.278685386795814560, 1.554813472153792286 ) ) ;
#190497 = CARTESIAN_POINT ( 'NONE',  ( 5.601068772352080671, -0.4412860211496574814, 1.787476196608045464 ) ) ;
#190499 = CARTESIAN_POINT ( 'NONE',  ( 4.271116411733427043, -2.292556078035115075, 0.1642532200917065921 ) ) ;
#190501 = CARTESIAN_POINT ( 'NONE',  ( 3.098338563049109151, 1.846317948315750357, 0.2325098740301386746 ) ) ;
#190500 = CARTESIAN_POINT ( 'NONE',  ( -0.02919842301642854021, 4.085261895051949921, -2.628472738367752637 ) ) ;
#190502 = CARTESIAN_POINT ( 'NONE',  ( -3.285556943749998737, -1.130208332855377140, 1.896917185911908499 ) ) ;
#190504 = EDGE_CURVE ( 'NONE', #119302, #55041, #21826, .T. ) ;
#190503 = DIRECTION ( 'NONE',  ( -0.5038915848335266956, -0.5182601445871922730, 0.6910135261095975423 ) ) ;
#190505 = CARTESIAN_POINT ( 'NONE',  ( 6.504189997394580480, -0.8109953713257547214, 1.730197269205424160 ) ) ;
#190506 = CARTESIAN_POINT ( 'NONE',  ( -7.507464373665155399, 9.781794407407920389, 1.599625672291295375 ) ) ;
#190507 = CARTESIAN_POINT ( 'NONE',  ( -3.851925040058337579, 6.547644075826416277, -1.082531754730546636 ) ) ;
#190508 = CARTESIAN_POINT ( 'NONE',  ( 5.706606250695148042, 1.844387978369428582, 0.9845570724962575682 ) ) ;
#190509 = CARTESIAN_POINT ( 'NONE',  ( 5.910991785878156435, 7.919243054989755670, -1.443375672974057666 ) ) ;
#190510 = EDGE_LOOP ( 'NONE', ( #78341, #92504, #45723, #139673 ) ) ;
#190511 = CARTESIAN_POINT ( 'NONE',  ( -1.500000000000079936, 7.361486028693807526, 4.203520246199945021 ) ) ;
#190513 = CARTESIAN_POINT ( 'NONE',  ( 3.330499290451326200, 7.037332938835193730, -0.7998128361456291469 ) ) ;
#190512 = CARTESIAN_POINT ( 'NONE',  ( 5.431895982697334091, 6.433277491268158954, -1.247050338538328029 ) ) ;
#190514 = CARTESIAN_POINT ( 'NONE',  ( 6.322847717702526182, 1.612277268089978621, 0.6135241758537502976 ) ) ;
#190515 = CARTESIAN_POINT ( 'NONE',  ( -4.062639585589296942, 7.891496616496157301, 0.7998128361456341429 ) ) ;
#190516 = CARTESIAN_POINT ( 'NONE',  ( 1.125167334363995852, 0.3372632679971860337, 1.700812921812058454 ) ) ;
#190517 = FACE_OUTER_BOUND ( 'NONE', #161613, .T. ) ;
#190518 = CARTESIAN_POINT ( 'NONE',  ( -0.7500000000000215383, 5.472916667349482900, 1.299038105676671107 ) ) ;
#190519 = CARTESIAN_POINT ( 'NONE',  ( 0.05470795666945791474, -5.634700952767746962, -11.00000000000002487 ) ) ;
#190520 = CARTESIAN_POINT ( 'NONE',  ( 6.104372708633159839, 2.168188666507598228, 0.1146961476086311021 ) ) ;
#190521 = CARTESIAN_POINT ( 'NONE',  ( 4.512205841073367196, -0.7830535718562798841, -1.649371741558727678 ) ) ;
#190522 = CARTESIAN_POINT ( 'NONE',  ( 2.553501467334079678, 1.513274546892771966, 1.248348448719404535 ) ) ;
#190523 =( GEOMETRIC_REPRESENTATION_CONTEXT ( 3 ) GLOBAL_UNCERTAINTY_ASSIGNED_CONTEXT ( ( #145373 ) ) GLOBAL_UNIT_ASSIGNED_CONTEXT ( ( #180815, #160577, #26297 ) ) REPRESENTATION_CONTEXT ( 'NONE', 'WORKASPACE' ) );
#190524 = CARTESIAN_POINT ( 'NONE',  ( -3.929058411375426108, -1.000000000000000888, 0.7499999999999988898 ) ) ;
#190525 = CARTESIAN_POINT ( 'NONE',  ( -8.292783513053063160, 12.82666453187061073, 0.7998128361456481317 ) ) ;
#190526 = CARTESIAN_POINT ( 'NONE',  ( 7.079328764629950754, 11.41096732537697633, 0.7998128361456462443 ) ) ;
#190527 = CARTESIAN_POINT ( 'NONE',  ( 3.141385665567609564, 0.05408136815227351790, 2.119969838212852675 ) ) ;
#190528 = CARTESIAN_POINT ( 'NONE',  ( -2.819732761962335577, 5.273143408055916304, -1.082531754730543971 ) ) ;
#190529 = DIRECTION ( 'NONE',  ( 7.387867266669436732E-31, -1.000000000000000000, -8.546850786086424434E-32 ) ) ;
#190530 = EDGE_CURVE ( 'NONE', #191870, #29472, #37090, .T. ) ;
#190531 = CARTESIAN_POINT ( 'NONE',  ( -4.397708481796120950, 7.154691356138512148, -1.067048916732843411 ) ) ;
#190532 = CARTESIAN_POINT ( 'NONE',  ( 1.622023338512183832, 2.040292009219225378, -0.3499636251925800079 ) ) ;
#190534 = CARTESIAN_POINT ( 'NONE',  ( -1.402160292154681736E-14, 15.09375000068279604, 1.732050807568881190 ) ) ;
#190533 = CARTESIAN_POINT ( 'NONE',  ( 3.147653791585693028, 8.920000000000001705, 2.499999999999999556 ) ) ;
#190536 = ORIENTED_EDGE ( 'NONE', *, *, #38452, .F. ) ;
#190535 = CARTESIAN_POINT ( 'NONE',  ( 3.897323497890590627, -0.2185073706607517652, -2.210542651646169698 ) ) ;
#190537 = CARTESIAN_POINT ( 'NONE',  ( 2.321245813631057864, 1.080353426350823209, -2.028982405110477227 ) ) ;
#190539 = CARTESIAN_POINT ( 'NONE',  ( 6.139522945012108934, 1.907909241145373525, -0.7841019685283256990 ) ) ;
#190538 = CARTESIAN_POINT ( 'NONE',  ( 9.924205255523292024, 10.68058700763975466, -0.7216878364870257245 ) ) ;
#190541 = CARTESIAN_POINT ( 'NONE',  ( -1.737500000000000266, -0.05833333333333384774, -3.009438278150923907 ) ) ;
#190540 = CARTESIAN_POINT ( 'NONE',  ( 4.740510986633625024, 5.559626234941203116, -1.199719254218450271 ) ) ;
#190542 = CARTESIAN_POINT ( 'NONE',  ( 1.477171894776290046E-15, 15.32408086029860428, 11.75104470124082034 ) ) ;
#190543 = CARTESIAN_POINT ( 'NONE',  ( 6.233933901472759942, 1.822226914158030286, 0.2631550708301691466 ) ) ;
#190544 = CARTESIAN_POINT ( 'NONE',  ( -0.2106725631050281045, 2.870437361830021405, -2.492085498774513574 ) ) ;
#190545 = CARTESIAN_POINT ( 'NONE',  ( 3.135487559415173653, -1.157359333423061409, -1.278988843622446137 ) ) ;
#190546 = CARTESIAN_POINT ( 'NONE',  ( 2.413296319342159713, -1.879803466158457059, 0.7303082167480907660 ) ) ;
#190547 = CARTESIAN_POINT ( 'NONE',  ( 2.690384307321362467, 1.943607183752774636, 1.227106530010623864 ) ) ;
#190548 = CARTESIAN_POINT ( 'NONE',  ( 3.937032273161138463, 0.3271595461276222139, 2.238503835787652996 ) ) ;
#190549 = CARTESIAN_POINT ( 'NONE',  ( 5.813134535821789406, 1.856751089961257373, 0.9939634876292826604 ) ) ;
#190550 = CARTESIAN_POINT ( 'NONE',  ( -5.451787166470911217, 9.374519104275787384, 0.7216878364870267237 ) ) ;
#190551 = CARTESIAN_POINT ( 'NONE',  ( 3.760817854529928894, -1.559684770762577388, -0.8363013385033011282 ) ) ;
#190553 = CARTESIAN_POINT ( 'NONE',  ( 5.917577160708873407, -1.270305590232129633, -1.908037719346373784 ) ) ;
#190552 = CARTESIAN_POINT ( 'NONE',  ( 3.390947816749319443, 6.970206529600588397, -1.734723475976807094E-15 ) ) ;
#190554 = CARTESIAN_POINT ( 'NONE',  ( 5.947170714876299336, 0.5300644225827764178, -1.763184533696081857 ) ) ;
#190555 = CARTESIAN_POINT ( 'NONE',  ( -2.435661151949389147, 5.993355110582911038, 0.7998128361456341429 ) ) ;
#190556 = UNCERTAINTY_MEASURE_WITH_UNIT (LENGTH_MEASURE( 1.000000000000000082E-05 ), #180847, 'distance_accuracy_value', 'NONE');
#190557 = CARTESIAN_POINT ( 'NONE',  ( 6.005898860729467437, 7.069598761348265370, -1.082531754730543083 ) ) ;
#190558 = CARTESIAN_POINT ( 'NONE',  ( -1.201851678989727383E-14, 3.587500000000020339, -1.732050807568863648 ) ) ;
#190559 = CARTESIAN_POINT ( 'NONE',  ( 5.121103774788174690, -2.081602751171758747, 0.6852947426586111224 ) ) ;
#190560 = CARTESIAN_POINT ( 'NONE',  ( -4.295235737431041478, 3.905529869957963029, -0.7998128361456221525 ) ) ;
#190561 = CARTESIAN_POINT ( 'NONE',  ( -7.079625160978284093, 15.44809611314506803, 9.644241769956890309 ) ) ;
#190562 = CARTESIAN_POINT ( 'NONE',  ( 5.811005889236001032, -1.634438611397070806, 1.270752202701043609 ) ) ;
#190563 = CARTESIAN_POINT ( 'NONE',  ( 0.3390778084843976137, -1.706115258973059490, -1.074657883261991076 ) ) ;
#190564 = CARTESIAN_POINT ( 'NONE',  ( -1.001543065824772872E-14, 5.071875000341421469, 1.575800808251672791 ) ) ;
#190565 = CARTESIAN_POINT ( 'NONE',  ( 3.281779325460960628, 1.222525406819600757, 1.488901545882119759 ) ) ;
#190566 = CARTESIAN_POINT ( 'NONE',  ( -0.6823417656250003738, 10.40104166700806587, 1.181850606188754593 ) ) ;
#190567 = FACE_OUTER_BOUND ( 'NONE', #161600, .T. ) ;
#190568 = CARTESIAN_POINT ( 'NONE',  ( 0.2818602545999105424, 0.2096452599892709712, -2.211486639639495433 ) ) ;
#190570 = ORIENTED_EDGE ( 'NONE', *, *, #77841, .T. ) ;
#190569 = CARTESIAN_POINT ( 'NONE',  ( 3.902768115887398803, 5.646591783325653147, -1.599625672291269396 ) ) ;
#190572 = DIRECTION ( 'NONE',  ( -0.000000000000000000, -1.000000000000000000, -0.000000000000000000 ) ) ;
#190571 = CARTESIAN_POINT ( 'NONE',  ( -4.502716413514313842, 5.386162249589033557, -1.082531754730549967 ) ) ;
#190573 = CARTESIAN_POINT ( 'NONE',  ( 3.018661757337009810, 6.673522483535157868, 0.000000000000000000 ) ) ;
#190574 = FACE_OUTER_BOUND ( 'NONE', #121523, .T. ) ;
#190575 = CARTESIAN_POINT ( 'NONE',  ( -3.719872605471121751, 6.605953636083950364, 2.420000000000000373 ) ) ;
#190576 = CARTESIAN_POINT ( 'NONE',  ( 9.585251414737269826, 11.24551007435741568, -1.082531754730537088 ) ) ;
#190577 = CARTESIAN_POINT ( 'NONE',  ( 1.838261372102001800, -1.052240823716396267, 1.655630454418555830 ) ) ;
#190578 = CARTESIAN_POINT ( 'NONE',  ( -1.364683531250012516, 1.842708333674749843, 0.7879004041258379498 ) ) ;
#190579 = CARTESIAN_POINT ( 'NONE',  ( 0.000000000000000000, 9.799999999999998934, 0.000000000000000000 ) ) ;
#190580 = CARTESIAN_POINT ( 'NONE',  ( 5.810985101215744741, -1.547553103248515027, 1.205733875218002238 ) ) ;
#190581 = CARTESIAN_POINT ( 'NONE',  ( -7.971304249830880373, 11.38727316052296601, 1.199719254218453823 ) ) ;
#190582 = CIRCLE ( 'NONE', #211305, 0.04999999999999969746 ) ;
#190583 = CARTESIAN_POINT ( 'NONE',  ( -6.046573321570485327, 6.156683084694754449, 0.000000000000000000 ) ) ;
#190584 = CARTESIAN_POINT ( 'NONE',  ( 6.438358464623771482, 2.137424745569570295, 0.3223339197731683869 ) ) ;
#190586 = VERTEX_POINT ( 'NONE', #170290 ) ;
#190585 = CARTESIAN_POINT ( 'NONE',  ( -0.3663205537283738544, -5.223179855898254509, -10.97093617010719946 ) ) ;
#190587 = CARTESIAN_POINT ( 'NONE',  ( -0.7500000000000249800, -0.7770833326505161009, 1.299038105676659116 ) ) ;
#190588 = CARTESIAN_POINT ( 'NONE',  ( 0.7197278698120103124, -0.9953326032119573785, -1.583558375183778288 ) ) ;
#190589 = CARTESIAN_POINT ( 'NONE',  ( 5.694640849732851784, -1.102317705797692726, -1.338331167630167684 ) ) ;
#190591 = CARTESIAN_POINT ( 'NONE',  ( 3.210657068901449307, 1.982179491636561819, 0.9350799695589939731 ) ) ;
#190590 = CARTESIAN_POINT ( 'NONE',  ( -1.953008978358306879E-14, 0.7031250003414774019, 1.570758158831782270 ) ) ;
#190592 = CARTESIAN_POINT ( 'NONE',  ( 3.909432592967517550, 1.977442543354444249, 1.189201670975383429 ) ) ;
#190593 = CARTESIAN_POINT ( 'NONE',  ( 0.1279053400650804195, -1.267571945882491447, -1.625495855733450457 ) ) ;
#190594 = CARTESIAN_POINT ( 'NONE',  ( 2.326030237553232016, 1.883725225384206281, 0.4715086074991140519 ) ) ;
#190595 = CARTESIAN_POINT ( 'NONE',  ( -5.273758565591545988, 6.215435083687305351, 1.082531754730546636 ) ) ;
#190596 = PRODUCT_DEFINITION_SHAPE ( 'NONE', 'NONE',  #214432 ) ;
#190597 = CARTESIAN_POINT ( 'NONE',  ( 5.590118541908202232, 1.264772504208915072, 1.701965355810124203 ) ) ;
#190598 = CARTESIAN_POINT ( 'NONE',  ( -1.752700365193352683E-14, 0.07812500034142640104, -1.570758158831804474 ) ) ;
#190599 = CARTESIAN_POINT ( 'NONE',  ( 3.287732575140737801, 1.587837554856496691, -1.242726844152845178 ) ) ;
#190600 = CARTESIAN_POINT ( 'NONE',  ( -5.395781948114519722, 5.397426482329451325, 0.000000000000000000 ) ) ;
#190601 = CARTESIAN_POINT ( 'NONE',  ( -7.944151662964566540, 8.232874793072271657, 0.000000000000000000 ) ) ;
#190602 = CARTESIAN_POINT ( 'NONE',  ( 8.536830278099042602, 13.11138575775759563, -0.7998128361456352531 ) ) ;
#190603 = CARTESIAN_POINT ( 'NONE',  ( 1.365546509989667534, 1.798985258052044900, -0.3101867277976525505 ) ) ;
#190604 = CARTESIAN_POINT ( 'NONE',  ( -4.990283058281743678, 7.979691447040783814, -1.199719254218453823 ) ) ;
#190605 = CARTESIAN_POINT ( 'NONE',  ( -4.793689830883590020, 7.750332681742931662, 1.199719254218452935 ) ) ;
#190606 = CARTESIAN_POINT ( 'NONE',  ( 2.580963302752299349, 0.4788041664877049075, 0.000000000000000000 ) ) ;
#190607 = EDGE_LOOP ( 'NONE', ( #52353, #169085, #201454, #213549 ) ) ;
#190608 = CARTESIAN_POINT ( 'NONE',  ( 5.436423068491611055, 2.030003055342466389, 0.3545201283375771228 ) ) ;
#190609 = CARTESIAN_POINT ( 'NONE',  ( -5.750066545527201534, 9.722511713174800008, 0.000000000000000000 ) ) ;
#190610 = CARTESIAN_POINT ( 'NONE',  ( -5.427341564172148303, 5.226320001155936090, 0.000000000000000000 ) ) ;
#190611 = CARTESIAN_POINT ( 'NONE',  ( -3.142457743317409680, 6.888227477170756785, 0.7998128361456352531 ) ) ;
#190612 = CARTESIAN_POINT ( 'NONE',  ( 4.213539248340679499, 1.623360089863118860, 1.201376956910469307 ) ) ;
#190614 = ORIENTED_EDGE ( 'NONE', *, *, #41407, .F. ) ;
#190613 = CARTESIAN_POINT ( 'NONE',  ( 5.549557930969759134, -2.008940618436024117, 0.9481178722350207533 ) ) ;
#190616 = CARTESIAN_POINT ( 'NONE',  ( 8.093854517678360949, 12.38665467069271386, 1.040834085586084257E-14 ) ) ;
#190615 = CARTESIAN_POINT ( 'NONE',  ( -5.738844160334429567, 9.917344963690652548, 0.000000000000000000 ) ) ;
#190617 = CARTESIAN_POINT ( 'NONE',  ( 6.307567778855705853, 8.381915046796901692, -1.599625672291262513 ) ) ;
#190618 = CARTESIAN_POINT ( 'NONE',  ( 3.643480044026959241, -1.559369103033839465, -1.347540176210021423 ) ) ;
#190619 = CARTESIAN_POINT ( 'NONE',  ( 3.973279856364997809, -1.994869694282218386, -0.2930714778977619450 ) ) ;
#190620 = ORIENTED_EDGE ( 'NONE', *, *, #85341, .F. ) ;
#190621 = SURFACE_SIDE_STYLE ('',( #174417 ) ) ;
#190622 = CARTESIAN_POINT ( 'NONE',  ( 4.867540842506059562, 5.637551390133895168, -1.199719254218452047 ) ) ;
#190624 = EDGE_LOOP ( 'NONE', ( #28101, #2172, #163212, #36855 ) ) ;
#190623 = CARTESIAN_POINT ( 'NONE',  ( -7.306918443122272677, 7.489436036589583345, 0.7998128361456341429 ) ) ;
#190625 = CARTESIAN_POINT ( 'NONE',  ( 5.303225773876714122, 7.631601692149430072, -1.229104931163179426 ) ) ;
#190626 = CARTESIAN_POINT ( 'NONE',  ( 3.444685325028495004, 1.276847194542466646, 1.560261755768836744 ) ) ;
#190627 = CARTESIAN_POINT ( 'NONE',  ( 2.835703941817575569, 1.827261480098177682, 0.2250241719141123087 ) ) ;
#190628 = CARTESIAN_POINT ( 'NONE',  ( 0.5577797733781300060, -1.952719008213155139, -1.229525757098411942 ) ) ;
#190629 = CARTESIAN_POINT ( 'NONE',  ( 3.573456005653643519, 6.326726552307992080, -1.199719254218453823 ) ) ;
#190630 = CARTESIAN_POINT ( 'NONE',  ( 3.778741785029844369, -2.082091666206013159, -0.5805316298483630399 ) ) ;
#190631 = CARTESIAN_POINT ( 'NONE',  ( -6.358937740009323214, 7.377514437221045718, -1.199719254218446718 ) ) ;
#190633 = EDGE_CURVE ( 'NONE', #57699, #131570, #70925, .T. ) ;
#190632 = PRESENTATION_LAYER_ASSIGNMENT (  '', '', ( #111090 ) ) ;
#190634 = ORIENTED_EDGE ( 'NONE', *, *, #166214, .T. ) ;
#190635 = DIRECTION ( 'NONE',  ( 0.000000000000000000, -1.000000000000000000, 0.000000000000000000 ) ) ;
#190636 = CARTESIAN_POINT ( 'NONE',  ( 1.832664747978371533, 0.1804508633567840359, 1.861920966532565336 ) ) ;
#190637 = CARTESIAN_POINT ( 'NONE',  ( 5.348493512783888626, 0.5714336785274246600, 1.886844506308351210 ) ) ;
#190639 = CARTESIAN_POINT ( 'NONE',  ( 7.388830529323379359, 11.56412668427855195, -0.7216878364870267237 ) ) ;
#190638 = CARTESIAN_POINT ( 'NONE',  ( -0.6823417656250212460, 4.801041667008086655, 1.181850606188767472 ) ) ;
#190641 = CARTESIAN_POINT ( 'NONE',  ( 0.01274299142895937362, -0.9473294304004549193, -1.991142614049784099 ) ) ;
#190640 = CARTESIAN_POINT ( 'NONE',  ( -4.903245109636583443, 8.872203061218007392, -0.7998128361456281477 ) ) ;
#190642 = CARTESIAN_POINT ( 'NONE',  ( 10.39025099420807052, 3.467171072964058354, -5.998814208453958408 ) ) ;
#190643 = CARTESIAN_POINT ( 'NONE',  ( 4.843287188579786573, 6.673587691474970107, -1.599625672291256295 ) ) ;
#190644 = CARTESIAN_POINT ( 'NONE',  ( -6.573005544526917099, 6.562927978236513304, -0.7998128361456291469 ) ) ;
#190645 = CARTESIAN_POINT ( 'NONE',  ( 6.539320575229278454, 3.689604457162498630, 2.617406275049142916 ) ) ;
#190646 = CARTESIAN_POINT ( 'NONE',  ( 5.787953125587765868, -0.8870788200928159117, 1.760698262704742723 ) ) ;
#190647 = CARTESIAN_POINT ( 'NONE',  ( 5.198025161738785371, -0.8347013672818380803, 2.151627338387426036 ) ) ;
#190648 = CARTESIAN_POINT ( 'NONE',  ( 5.986726177563552298, 1.793701560725208699, 0.4957798874403050449 ) ) ;
#190649 = CARTESIAN_POINT ( 'NONE',  ( 2.694246160070143503, 0.9763755106866910394, -1.816870488346455037 ) ) ;
#190650 = CARTESIAN_POINT ( 'NONE',  ( 6.968527767744109980, 7.232296605230681408, 0.7216878364870317197 ) ) ;
#190651 = CARTESIAN_POINT ( 'NONE',  ( 4.947799714344386146, 4.737130853015369958, -0.7998128361456481317 ) ) ;
#190652 = CARTESIAN_POINT ( 'NONE',  ( 7.009202228140744673, 9.200488570962775725, -1.443375672974058777 ) ) ;
#190653 = CARTESIAN_POINT ( 'NONE',  ( 0.6823417656249882723, 2.738541667008084879, -1.181850606188749264 ) ) ;
#190654 = DIRECTION ( 'NONE',  ( 0.000000000000000000, 0.000000000000000000, -1.000000000000000000 ) ) ;
#190655 = CARTESIAN_POINT ( 'NONE',  ( 4.812781342726855982, 7.598366752281232372, 1.082531754730558626 ) ) ;
#190656 = CARTESIAN_POINT ( 'NONE',  ( 4.967309339809048652, 1.886637975807739176, 1.074439269227177363 ) ) ;
#190657 = CARTESIAN_POINT ( 'NONE',  ( -5.249999999999987566, 0.9165151389911689872, 1.199999999999999734 ) ) ;
#190659 = CARTESIAN_POINT ( 'NONE',  ( 4.493604616018744835, -1.840970053361364656, -0.04044509776383875543 ) ) ;
#190658 = CARTESIAN_POINT ( 'NONE',  ( -11.33772463945036968, 10.09088423488573838, -3.600000000000000977 ) ) ;
#190661 = CARTESIAN_POINT ( 'NONE',  ( 9.555169238417182243, -7.776896528353608673, -0.04234008746931129663 ) ) ;
#190660 = CARTESIAN_POINT ( 'NONE',  ( 0.6823417656249917140, 5.592708333674749177, 1.181850606188765695 ) ) ;
#190662 = CARTESIAN_POINT ( 'NONE',  ( 6.374583145400191775, -0.1054333438532777389, -2.189162923280890904 ) ) ;
#190663 = CARTESIAN_POINT ( 'NONE',  ( 0.4639452589547733985, 2.947031273455551492, 1.945529950462648205 ) ) ;
#190664 = CARTESIAN_POINT ( 'NONE',  ( 0.9314073880264511773, 0.1673361042086803641, 2.256242939573564144 ) ) ;
#190665 = CARTESIAN_POINT ( 'NONE',  ( -4.002915605954192380, 7.811702849818844108, -0.3674259761444337302 ) ) ;
#190666 = DIRECTION ( 'NONE',  ( -0.000000000000000000, -0.000000000000000000, -1.000000000000000000 ) ) ;
#190667 = CARTESIAN_POINT ( 'NONE',  ( 5.869365784521903606, 7.282179437329668659, 1.264975801879052453 ) ) ;
#190668 = CARTESIAN_POINT ( 'NONE',  ( -5.492461626867567226, 6.540864998501174199, 1.082531754730549078 ) ) ;
#190669 = CARTESIAN_POINT ( 'NONE',  ( 11.86686399458719521, 13.60928729775337054, 1.056461745586970258 ) ) ;
#190670 = CARTESIAN_POINT ( 'NONE',  ( 0.3382653665467276749, 0.2958422019357190291, 1.744775138515190616 ) ) ;
#190671 = AXIS2_PLACEMENT_3D ( 'NONE', #203662, #87812, #157091 ) ;
#190672 = CARTESIAN_POINT ( 'NONE',  ( 5.215494488825547670, 1.647103507230001096, 1.157162265453457239 ) ) ;
#190673 = CARTESIAN_POINT ( 'NONE',  ( 4.143988507271280319, 7.986403691791820414, -0.7998128361456221525 ) ) ;
#190674 = CARTESIAN_POINT ( 'NONE',  ( 4.278421442896533478, -1.214510211351152336, 1.720268157014235078 ) ) ;
#190676 = CARTESIAN_POINT ( 'NONE',  ( 2.952642602588346321, -1.771063984568725935, -0.7304820402930515266 ) ) ;
#190675 = CARTESIAN_POINT ( 'NONE',  ( -4.744990574658554117, 4.638169879964154418, 1.214306433183764966E-14 ) ) ;
#190677 = PRESENTATION_LAYER_ASSIGNMENT (  '', '', ( #118249 ) ) ;
#190678 = CARTESIAN_POINT ( 'NONE',  ( -0.02244404828160087226, 1.995160441984781041, -2.602654351998904492 ) ) ;
#190679 = CARTESIAN_POINT ( 'NONE',  ( 4.158625497742932886, -0.6157697831138170264, -1.870904811771924470 ) ) ;
#190680 = CARTESIAN_POINT ( 'NONE',  ( 5.941667304196568189, -1.900381328601069342, 0.6844855596733252501 ) ) ;
#190681 = CARTESIAN_POINT ( 'NONE',  ( 2.272138710904994863, -1.152746988206950096, 1.473173409640892162 ) ) ;
#190684 = ORIENTED_EDGE ( 'NONE', *, *, #115527, .T. ) ;
#190683 = CARTESIAN_POINT ( 'NONE',  ( 1.353610510645312237, -1.387278792934818705, -1.316581319992945920 ) ) ;
#190682 = CARTESIAN_POINT ( 'NONE',  ( 5.021954727502539129, -0.9268850835505036967, -1.454474922752227339 ) ) ;
#190686 = CARTESIAN_POINT ( 'NONE',  ( 5.016153647376217606, 4.954526798134778254, 0.7216878364870317197 ) ) ;
#190685 = CARTESIAN_POINT ( 'NONE',  ( 1.911028901235469313, 1.633884665098099598, -1.483674895440662667 ) ) ;
#190687 = CARTESIAN_POINT ( 'NONE',  ( -1.364683531250014514, 1.551041667008084435, -0.7879004041258289570 ) ) ;
#190688 = CARTESIAN_POINT ( 'NONE',  ( 6.478960399985357554, 1.830089090633261417, 0.7073212282268787066 ) ) ;
#190689 = CARTESIAN_POINT ( 'NONE',  ( 8.589254009457354400, 9.979550084910457031, -1.199719254218446718 ) ) ;
#190690 = LINE ( 'NONE', #123672, #171295 ) ;
#190691 = PLANE ( 'NONE',  #102438 ) ;
#190692 = CARTESIAN_POINT ( 'NONE',  ( -5.253948220495577637, 6.088359997788290734, 1.199719254218450271 ) ) ;
#190693 = CARTESIAN_POINT ( 'NONE',  ( -1.499999999999966693, 7.750000000000000000, 9.886859966642596476 ) ) ;
#190694 = EDGE_LOOP ( 'NONE', ( #176856, #4997, #26895, #121484 ) ) ;
#190695 = CARTESIAN_POINT ( 'NONE',  ( 1.996617168637443429, 2.047528291220417351, 0.3059219562495316125 ) ) ;
#190696 = CARTESIAN_POINT ( 'NONE',  ( 1.499999999999989120, 3.004166666666689522, 0.8660254037844524744 ) ) ;
#190697 = CARTESIAN_POINT ( 'NONE',  ( 4.961394147597008697, 7.875711374583454827, -1.199719254218452047 ) ) ;
#190698 = CARTESIAN_POINT ( 'NONE',  ( 3.217027588192558074, 6.975225629525113824, -1.734723475976807094E-15 ) ) ;
#190699 = CARTESIAN_POINT ( 'NONE',  ( 6.393239817247728496, -0.1034752114322245314, -2.118097640427937911 ) ) ;
#190700 = CARTESIAN_POINT ( 'NONE',  ( -9.498256814137544524, -6.950186805636726639, -0.04218801535505443956 ) ) ;
#190701 = CARTESIAN_POINT ( 'NONE',  ( -1.201851678989727383E-14, 3.321875000341421025, 1.575800808251672791 ) ) ;
#190703 = CARTESIAN_POINT ( 'NONE',  ( 9.585251415181632595, 10.28514086057449184, 0.000000000000000000 ) ) ;
#190702 = CARTESIAN_POINT ( 'NONE',  ( -11.55950211276791428, 11.37999999999999901, -3.221476510067114329 ) ) ;
#190704 = CARTESIAN_POINT ( 'NONE',  ( 5.395861176733054876, 0.1455124041884261754, 2.010896217931843921 ) ) ;
#190705 = EDGE_CURVE ( 'NONE', #187130, #80718, #19144, .T. ) ;
#190706 = CARTESIAN_POINT ( 'NONE',  ( 5.331221607142452967, -1.514317160175217447, -1.173313937468897672 ) ) ;
#190707 = CARTESIAN_POINT ( 'NONE',  ( 6.639320575229283428, 0.5834889568891787892, 2.056715522164854981 ) ) ;
#190708 = CARTESIAN_POINT ( 'NONE',  ( 3.175498511859841333, 1.392037702009111033, 1.692654053968026151 ) ) ;
#190709 = CARTESIAN_POINT ( 'NONE',  ( 8.154303043976348420, 8.478051404252736845, 0.7998128361456281477 ) ) ;
#190710 = CARTESIAN_POINT ( 'NONE',  ( -1.499999999999997780, 2.681250000682818158, 1.214306433183764966E-14 ) ) ;
#190711 = CARTESIAN_POINT ( 'NONE',  ( 5.783453021694040963, 0.1439598661895292731, -2.008088619348106896 ) ) ;
#190712 = CARTESIAN_POINT ( 'NONE',  ( 1.388764059443419407, -1.816923020173771830, -0.5969786173363604842 ) ) ;
#190713 = CARTESIAN_POINT ( 'NONE',  ( -5.368138756007025947, 8.350246751061767725, 1.199719254218452047 ) ) ;
#190715 = CARTESIAN_POINT ( 'NONE',  ( 6.503513627744350600, -2.053693679520858684, 0.5143327402655095693 ) ) ;
#190714 = CARTESIAN_POINT ( 'NONE',  ( -2.806174608348664723, 6.217694776474651519, 1.040834085586084257E-14 ) ) ;
#190716 = CARTESIAN_POINT ( 'NONE',  ( -8.012344526598182026E-15, 9.359375000341399797, -1.575800808251669460 ) ) ;
#190718 = CARTESIAN_POINT ( 'NONE',  ( -5.336015975430226099, 8.383046517047350932, -1.199719254218453823 ) ) ;
#190717 = CARTESIAN_POINT ( 'NONE',  ( 3.403930425450612418, -0.8493818440679711257, -1.910634358282743417 ) ) ;
#190720 = EDGE_LOOP ( 'NONE', ( #46916, #119594, #87515, #89911 ) ) ;
#190719 = CARTESIAN_POINT ( 'NONE',  ( 1.957592155046536941, 1.720466030779904454, -0.1226356519287794405 ) ) ;
#190721 = CARTESIAN_POINT ( 'NONE',  ( 5.311043488251262268, 7.219303374425030562, -1.599625672291256295 ) ) ;
#190722 = FACE_BOUND ( 'NONE', #124316, .T. ) ;
#190723 = DIRECTION ( 'NONE',  ( 1.000000000000000000, 0.000000000000000000, 0.000000000000000000 ) ) ;
#190724 = CARTESIAN_POINT ( 'NONE',  ( -11.84668730067608600, 10.19999999999999929, -1.400000000000001910 ) ) ;
#190725 = CARTESIAN_POINT ( 'NONE',  ( 5.144429221381498607, 8.089252293998699272, -1.199719254218452047 ) ) ;
#190726 = ORIENTED_EDGE ( 'NONE', *, *, #175281, .F. ) ;
#190727 = CARTESIAN_POINT ( 'NONE',  ( -11.92619526913699879, 13.40000000000000036, -1.328859060402686199 ) ) ;
#190728 = ORIENTED_EDGE ( 'NONE', *, *, #135027, .F. ) ;
#190729 = CARTESIAN_POINT ( 'NONE',  ( 3.316878987808123735, 1.426168316962544091, -1.116757653536442740 ) ) ;
#190730 = ORIENTED_EDGE ( 'NONE', *, *, #187759, .F. ) ;
#190731 = CARTESIAN_POINT ( 'NONE',  ( 4.162516854595432747, 4.815023404238158555, 1.199719254218464037 ) ) ;
#190732 = CARTESIAN_POINT ( 'NONE',  ( 4.061549535745618833, 6.896169004081968090, -1.199719254218452047 ) ) ;
#190733 = CARTESIAN_POINT ( 'NONE',  ( 3.475094438140493125, -1.599078698050887981, -0.8510578468755282122 ) ) ;
#190734 = CARTESIAN_POINT ( 'NONE',  ( 6.539320575229215393, 2.445213257098968640, 2.379920919941742152 ) ) ;
#190735 = SURFACE_STYLE_USAGE ( .BOTH. , #176643 ) ;
#190736 = CARTESIAN_POINT ( 'NONE',  ( 5.335014106237911946, 6.336523053015567619, 1.100733037772538170 ) ) ;
#190738 = CARTESIAN_POINT ( 'NONE',  ( 1.364683531250000303, 14.75520833367472839, -0.7879004041258355073 ) ) ;
#190737 = CARTESIAN_POINT ( 'NONE',  ( 3.806960202730264253, -1.522499362102507359, 1.069998817686746984 ) ) ;
#190739 = CARTESIAN_POINT ( 'NONE',  ( 1.810024464468898309, 1.101340386757416967, -1.567151550741460397 ) ) ;
#190740 = CARTESIAN_POINT ( 'NONE',  ( 1.289775909805501719, -0.8246113042270180049, 1.628811597173693393 ) ) ;
#190741 = CARTESIAN_POINT ( 'NONE',  ( 4.822014627293360611, 8.104635198319419587, 0.8657228342519827091 ) ) ;
#190742 = CARTESIAN_POINT ( 'NONE',  ( -1.718115394875207258, -1.500000000000000888, 2.017567716309124126 ) ) ;
#190743 = TOROIDAL_SURFACE ( 'NONE', #3937, 10.92000000000000171, 0.08000000000000000167 ) ;
#190744 = CARTESIAN_POINT ( 'NONE',  ( 4.943016831304842817, 7.975319854387232787, 1.017975537214605319 ) ) ;
#190745 = CARTESIAN_POINT ( 'NONE',  ( 5.020734711527275351, 8.014512191897464888, 1.145736749330818149 ) ) ;
#190746 = LINE ( 'NONE', #42410, #129606 ) ;
#190747 = CARTESIAN_POINT ( 'NONE',  ( -5.914749137557818059, 6.074338953224275528, -0.6118981238392419142 ) ) ;
#190748 = CARTESIAN_POINT ( 'NONE',  ( 7.619319141200070256, 8.951922421897323900, 1.082531754730558626 ) ) ;
#190749 = CARTESIAN_POINT ( 'NONE',  ( 5.366046204681790499, -1.960318410495393238, 0.1889891646899461708 ) ) ;
#190750 = CARTESIAN_POINT ( 'NONE',  ( -4.120788623549732854, 6.895004929861607401, -1.199719254218452047 ) ) ;
#190751 = CARTESIAN_POINT ( 'NONE',  ( -11.94980361490462428, 10.09667875264143255, -1.099999952232860290 ) ) ;
#190752 = EDGE_CURVE ( 'NONE', #119510, #171296, #120565, .T. ) ;
#190753 = CARTESIAN_POINT ( 'NONE',  ( 6.597619724345276104, -2.191060131252516641, 0.04951108399064289151 ) ) ;
#190754 = CARTESIAN_POINT ( 'NONE',  ( 6.141620278036529434, -1.395723430145169752, -1.327979989909616521 ) ) ;
#190755 = CARTESIAN_POINT ( 'NONE',  ( -6.663996196316808174, 7.733415969579778171, -1.199719254218446718 ) ) ;
#190756 = CARTESIAN_POINT ( 'NONE',  ( 1.254616015376356586, -1.441780481750528420, 1.119729341354458452 ) ) ;
#190757 = CARTESIAN_POINT ( 'NONE',  ( 2.455956380646412196, 0.5873987694336445520, -2.127207350628975924 ) ) ;
#190758 = CARTESIAN_POINT ( 'NONE',  ( -1.115562610750309283E-14, 10.06250000000000000, 1.500000000000001554 ) ) ;
#190759 = CARTESIAN_POINT ( 'NONE',  ( 1.371198541116287917, -1.641758494746584418, -0.9804709962101465504 ) ) ;
#190760 = CARTESIAN_POINT ( 'NONE',  ( 0.2562226757886588713, -1.969045882358761101, -0.05199970915584737480 ) ) ;
#190761 = CARTESIAN_POINT ( 'NONE',  ( 2.261185778363482779, 1.904153404235246594, -0.3810316102009890238 ) ) ;
#190762 = EDGE_LOOP ( 'NONE', ( #137824, #86879, #62565, #115638 ) ) ;
#190763 = LINE ( 'NONE', #42427, #88612 ) ;
#190765 = CARTESIAN_POINT ( 'NONE',  ( 6.789920448004552078, -1.215336557376142101, -1.409407482083424590 ) ) ;
#190764 = CARTESIAN_POINT ( 'NONE',  ( -5.655686355556086120, 6.627330832017406692, 1.199719254218452935 ) ) ;
#190766 = CARTESIAN_POINT ( 'NONE',  ( 5.571474780572990504, 5.464751763615448787, 0.7998128361456352531 ) ) ;
#190768 = ADVANCED_FACE ( 'NONE', ( #87984 ), #67621, .T. ) ;
#190767 = CARTESIAN_POINT ( 'NONE',  ( -11.49966000274973155, 13.74232845564745276, -3.429881629453017222 ) ) ;
#190769 = CARTESIAN_POINT ( 'NONE',  ( 8.211434591371064684, 12.73175745657494851, -0.7998128361456352531 ) ) ;
#190770 = CARTESIAN_POINT ( 'NONE',  ( -5.098748287191073203, 8.106234214101666780, 1.199719254218452935 ) ) ;
#190771 = CARTESIAN_POINT ( 'NONE',  ( 2.841561854484982774, 0.7863008361240211297, -2.045831095052422555 ) ) ;
#190772 = AXIS2_PLACEMENT_3D ( 'NONE', #40944, #206613, #58243 ) ;
#190773 = CARTESIAN_POINT ( 'NONE',  ( 6.393551957296131683, 9.616838495890963401, 1.199719254218452047 ) ) ;
#190774 = DIRECTION ( 'NONE',  ( 1.000000000000000000, -9.486769009248179575E-16, 0.000000000000000000 ) ) ;
#190775 = CARTESIAN_POINT ( 'NONE',  ( 2.842213963582499670, 1.811911227886909614, 0.2232855069103783507 ) ) ;
#190776 = DIRECTION ( 'NONE',  ( 0.000000000000000000, 0.000000000000000000, -1.000000000000000000 ) ) ;
#190777 = CARTESIAN_POINT ( 'NONE',  ( -3.358669367883384105, 4.941533567329135401, -1.599625672291262513 ) ) ;
#190778 = CARTESIAN_POINT ( 'NONE',  ( -4.818718062179155659, 8.223694781438435797, -0.9201054579500017594 ) ) ;
#190779 = CARTESIAN_POINT ( 'NONE',  ( 6.925078400183548588, 0.0006614011395407459748, 1.855452278108092656 ) ) ;
#190780 = CARTESIAN_POINT ( 'NONE',  ( 7.553864141108259211, 11.96459193126834464, 1.040834085586084257E-14 ) ) ;
#190781 = CARTESIAN_POINT ( 'NONE',  ( 0.5746741651161955122, -1.813631458699631160, -0.6500969746191431753 ) ) ;
#190782 = CARTESIAN_POINT ( 'NONE',  ( 5.383633123045536983, -1.864019207510819953, 0.6117972396969258986 ) ) ;
#190783 = CIRCLE ( 'NONE', #55975, 2.000000000000000000 ) ;
#190784 = CARTESIAN_POINT ( 'NONE',  ( 0.7500000000000006661, 15.33333333333333037, 1.299038105676657340 ) ) ;
#190785 = CARTESIAN_POINT ( 'NONE',  ( -7.985916173649233230, 9.275655943134292869, -1.199719254218446718 ) ) ;
#190786 = CARTESIAN_POINT ( 'NONE',  ( 6.159481859310094620, 6.080483678816896109, 1.040834085586084257E-14 ) ) ;
#190787 = CARTESIAN_POINT ( 'NONE',  ( 5.126606437771586755, 0.1607948393855564151, 2.185736094377451089 ) ) ;
#190788 = EDGE_CURVE ( 'NONE', #153847, #173630, #102053, .T. ) ;
#190789 = DIRECTION ( 'NONE',  ( 0.000000000000000000, -1.000000000000000000, 0.000000000000000000 ) ) ;
#190790 = CARTESIAN_POINT ( 'NONE',  ( -3.307826292054316664, 4.882216645528547616, -1.443375672974059665 ) ) ;
#190791 = CARTESIAN_POINT ( 'NONE',  ( 5.594608825991118195, 2.038665915018455177, 0.3594684214384344378 ) ) ;
#190792 = CARTESIAN_POINT ( 'NONE',  ( 0.6823417656249899377, 2.905208333674754062, 1.181850606188765695 ) ) ;
#190793 = ORIENTED_EDGE ( 'NONE', *, *, #149015, .T. ) ;
#190794 = ORIENTED_EDGE ( 'NONE', *, *, #85069, .F. ) ;
#190795 = CARTESIAN_POINT ( 'NONE',  ( 4.729243902325204196, 2.292384926013335988, 0.1706581203582517303 ) ) ;
#190796 = CARTESIAN_POINT ( 'NONE',  ( 7.144783764721768904, 7.437928601704619780, 1.040834085586084257E-14 ) ) ;
#190798 = CARTESIAN_POINT ( 'NONE',  ( -1.499999999999997780, 4.681250000682819490, 1.214306433183765124E-14 ) ) ;
#190797 = CARTESIAN_POINT ( 'NONE',  ( 5.234856708652233515, 6.240325927249993576, 1.082531754730549078 ) ) ;
#190799 = CARTESIAN_POINT ( 'NONE',  ( 0.3051332635122120385, 1.997493689478089252, 1.124391992203729540 ) ) ;
#190800 = CARTESIAN_POINT ( 'NONE',  ( -5.427006627220116286, 9.553534508390610469, -0.7998128361456362523 ) ) ;
#190801 = CARTESIAN_POINT ( 'NONE',  ( 4.857337426984369877, 1.920559571908975194, -0.2866867867914507650 ) ) ;
#190802 = ORIENTED_EDGE ( 'NONE', *, *, #181980, .F. ) ;
#190803 = CARTESIAN_POINT ( 'NONE',  ( 8.175203438916005538, 11.52119253116861586, -1.082531754730543083 ) ) ;
#190804 = ORIENTED_EDGE ( 'NONE', *, *, #55359, .T. ) ;
#190805 = CARTESIAN_POINT ( 'NONE',  ( 5.097880177178074845, 1.288836597028759634, 1.412999258680311510 ) ) ;
#190806 = CARTESIAN_POINT ( 'NONE',  ( 6.440463960111763697, 1.706863596762456581, 0.2470990609701722573 ) ) ;
#190807 = CARTESIAN_POINT ( 'NONE',  ( 6.016814611094169152, 0.2024578496369993375, 2.006372135924570088 ) ) ;
#190809 = DIRECTION ( 'NONE',  ( 1.000000000000000000, 0.000000000000000000, 0.000000000000000000 ) ) ;
#190808 = CARTESIAN_POINT ( 'NONE',  ( -9.840520565420403543, 10.37502883594562597, 1.040834085586084257E-14 ) ) ;
#190810 = CARTESIAN_POINT ( 'NONE',  ( 0.000000000000000000, -1.684374999522041172, -3.793834371823813001 ) ) ;
#190812 = CARTESIAN_POINT ( 'NONE',  ( 0.6371259318241145886, -1.247223858821765230, -1.255979444004810430 ) ) ;
#190811 = CARTESIAN_POINT ( 'NONE',  ( 1.798888674052185888, 1.738860765912113138, 1.160333176109765274 ) ) ;
#190813 = CARTESIAN_POINT ( 'NONE',  ( 6.311172677262812059, 1.158691452862798954, -1.650079838712660063 ) ) ;
#190815 = CARTESIAN_POINT ( 'NONE',  ( 2.765910322896072859, 1.227222833649963540, 1.935908780871216761 ) ) ;
#190814 = CARTESIAN_POINT ( 'NONE',  ( 3.953084306836263995, 6.769626237021087789, 1.199719254218452047 ) ) ;
#190816 = CARTESIAN_POINT ( 'NONE',  ( 2.396107360292961008, 1.398095582919863133, -1.036136137726038520 ) ) ;
#190817 = CARTESIAN_POINT ( 'NONE',  ( 3.146849984228027974, 2.069795010335002239, 0.4607391970517027979 ) ) ;
#190818 = CARTESIAN_POINT ( 'NONE',  ( 0.3282377607281143916, 0.7388354509981899243, -1.225000000000014300 ) ) ;
#190819 = CARTESIAN_POINT ( 'NONE',  ( 1.844673738135360175, -0.9321790797625574276, 1.461707330738234667 ) ) ;
#190820 = CARTESIAN_POINT ( 'NONE',  ( 0.6801582343749883464, 1.505208333674713739, 1.178068619123805227 ) ) ;
#190821 = CARTESIAN_POINT ( 'NONE',  ( 1.539268068193447858, 1.721329529071988107, -0.7080023387807417024 ) ) ;
#190822 = CARTESIAN_POINT ( 'NONE',  ( 2.524086392267041568, 2.129678358216775536, -0.4216712753718852014 ) ) ;
#190823 = CARTESIAN_POINT ( 'NONE',  ( 3.608611488583326032, 1.916353073142588403, 0.6279913346786819561 ) ) ;
#190824 = CARTESIAN_POINT ( 'NONE',  ( 4.093750000000002665, -1.895863743164171611, -0.7852924748297696045 ) ) ;
#190825 = AXIS2_PLACEMENT_3D ( 'NONE', #141912, #12915, #78995 ) ;
#190826 = B_SPLINE_CURVE_WITH_KNOTS ( 'NONE', 3,
 ( #189170, #172942, #24520, #140466, #58109, #190226, #41885, #107996 ),
 .UNSPECIFIED., .F., .F.,
 ( 4, 2, 2, 4 ),
 ( 7.413913665834773066E-18, 0.0002034531274099240334, 0.0004069062548198406400, 0.0008138125096396705465 ),
 .UNSPECIFIED. ) ;
#190827 = CARTESIAN_POINT ( 'NONE',  ( 1.499999999999987121, 1.077083334016148308, -0.8660254037844253849 ) ) ;
#190828 = CARTESIAN_POINT ( 'NONE',  ( 1.412975430660408538, 1.697568229685364249, 0.9106500277177332903 ) ) ;
#190829 = CARTESIAN_POINT ( 'NONE',  ( -0.6823417656250003738, 14.65104166700806410, 1.181850606188754593 ) ) ;
#190830 = CARTESIAN_POINT ( 'NONE',  ( 3.533611464748823927, -0.1604399991079318022, 2.215644447872004985 ) ) ;
#190831 = ORIENTED_EDGE ( 'NONE', *, *, #213257, .F. ) ;
#190832 = TOROIDAL_SURFACE ( 'NONE', #163190, 9.559451093910102060, 0.08000000000000000167 ) ;
#190833 = CARTESIAN_POINT ( 'NONE',  ( -1.201851678989727383E-14, 0.9625000000000237810, 1.732050807568877637 ) ) ;
#190834 = CARTESIAN_POINT ( 'NONE',  ( 6.252281394196331554, 10.44607872653774372, 1.040834085586084257E-14 ) ) ;
#190835 = CARTESIAN_POINT ( 'NONE',  ( -1.402160292154681736E-14, -0.5531249996585814177, -1.575800808251665908 ) ) ;
#190836 = CARTESIAN_POINT ( 'NONE',  ( 5.695613681701293451, 2.052597959444299125, -0.8498680618601384129 ) ) ;
#190837 = CARTESIAN_POINT ( 'NONE',  ( 4.527759979645433752, 1.903474890065796732, -0.4746247275292309609 ) ) ;
#190839 = CARTESIAN_POINT ( 'NONE',  ( -5.829642864196175722, 7.824335979694092558, 1.443375672974064550 ) ) ;
#190838 = CARTESIAN_POINT ( 'NONE',  ( 8.432808358020015049, 11.82173160345663376, 1.082531754730546636 ) ) ;
#190840 = CARTESIAN_POINT ( 'NONE',  ( -11.40816717570230310, 3.487142912321092414, 3.706738213303463425 ) ) ;
#190841 = CARTESIAN_POINT ( 'NONE',  ( 6.151720675889260193, 0.6653518678880927517, -2.162357237652327679 ) ) ;
#190842 = CARTESIAN_POINT ( 'NONE',  ( -4.475600106286965918, 8.235634200727838916, 0.7216878364870338292 ) ) ;
#190843 = CARTESIAN_POINT ( 'NONE',  ( 1.820832581213110313, -1.460207654653251419, 1.457104742506893036 ) ) ;
#190844 = CARTESIAN_POINT ( 'NONE',  ( -7.217017841176048165, 7.314275657660511243, 1.040834085586084257E-14 ) ) ;
#190845 =( BOUNDED_SURFACE ( )  B_SPLINE_SURFACE ( 1, 2, ( 
 ( #71594, #118301, #4449, #105208, #188564, #121525, #136634, #103061, #122601, #172329, #153945, #38060, #185356, #54310, #70519, #23918, #184287, #170177, #151819, #40195, #85734, #35913, #168057, #5513, #155009, #152871, #119368, #101988, #171245, #21765, #36978, #137703, #169115, #20711, #86805, #120448, #19659, #201591, #87873, #73751, #203723, #7666, #55371, #187495, #39125, #72674, #106307, #3392, #22841, #88955, #90023, #69462, #138771, #156080, #200529, #56442, #6594, #135567, #208006, #9810, #78014, #95367, #93231, #59631, #159263, #175535, #75885, #124725, #161417, #206942, #76937, #190686, #42345, #26056, #108460, #41279, #140928, #141992, #13001, #174480, #139846, #10864, #92169, #27125, #11942, #127941, #205875, #143063, #58571, #45541, #57509, #144138, #61773, #177667, #210131, #158221, #125789, #191751, #43406, #193893, #123668, #209058, #109529, #60694, #126858, #192816, #44474, #189631, #110590, #176592, #91095, #28204, #94298, #111655, #160338, #8747, #29275, #107388, #173411, #24992, #157155, #74828, #80144, #147296, #64948, #14055, #180839, #98535, #15128, #100657, #81216, #165663, #32465, #30347, #83327, #62827, #133196, #198145, #82266, #194966, #213326, #164596, #131100, #197089, #96432, #16182, #149414, #148359, #146247, #145195, #50846, #48727, #214358, #128987, #97486, #212263, #46602, #17250, #166735, #179792, #163543, #116973, #113790, #114841, #112720, #33525, #65988, #132138, #211201, #49777, #115904, #67060, #181889, #99597, #196045, #996, #182970, #199198, #34585, #63897, #79077, #178732, #162483, #130052, #47679, #31412, #154753, #118045, #84409, #200270, #186163, #187236, #185089, #151559, #2056, #203463, #4194, #69196, #152608, #103871, #150497, #36713, #137446, #6337, #153686, #168857, #135317, #72409, #204532, #37796, #70264, #3127, #20460, #102799, #56182, #68129, #202397, #184031, #138509, #35647, #134264, #51922, #169920, #38865, #86543, #201331, #101726, #55117, #136378, #52969, #21506, #119107, #54049, #120186, #87615, #167797, #19392, #5254, #106048, #71331, #39940, #121263, #104948, #170988, #22587, #122343, #85471, #88693, #188300, #18326, #23665, #113271, #96976, #212810, #30899, #74570, #25800, #91909, #42086, #179276, #130592, #125533, #157966, #191492, #207749, #108201, #156895, #196581, #24730, #90833, #123410, #75635, #58315, #80704, #174225, #41017, #63382, #48223, #8483, #163024, #140669, #146794, #173149, #9558, #141743, #107126, #59376, #43160, #109272, #172071, #175280, #47155, #26867, #189374, #14607, #155821, #64447, #79624, #92971, #73486, #161962, #13552, #145743, #211744, #206683, #129537, #89775, #195518, #124470, #7405, #139586, #205613, #57250, #190429, #132677, #115394, #81759, #200807, #135850, #466, #198683, #86023, #148893, #34067, #164091, #68678, #147841, #201872, #52458, #114336, #83879, #51400, #183513, #67601, #181387, #131629, #197628, #15672, #82817, #149970, #213859, #152096, #33010, #199755, #50328, #49273, #84951, #99089, #117520, #184571, #66536, #116446, #101194, #65479, #167282, #165141, #16732, #182440, #100138, #166201, #2609, #36191, #133747, #17791, #1539, #35122, #18867, #134801, #102267, #151040, #118584, #168342, #19937, #3667, #180331, #69744, #31954, #98038, #55654, #204005, #87087, #40491, #185639, #157445, #9039, #189921, #57792, #120738, #171535, #72957, #7956, #91385, #75113, #71878, #41566, #106596, #107679, #172623, #173708, #141225, #39409, #187778, #37271, #53520, #119654, #23128, #169404, #25284, #24199, #155296, #74048, #121810, #105503, #103341, #20990, #202947, #156372, #153157, #137988, #4732, #70807, #22050, #90302, #136920, #89245, #6879, #140138, #139059, #206164, #54591, #186711, #5801, #38340, #123952, #104416, #205087, #122896, #170465, #88161, #56728, #154229, #188855, #13305, #161713, #145497, #59921, #42638, #162778, #126076, #207234, #192037, #96729, #190971, #58858, #76172, #95662, #80446, #43700, #211492, #109817, #113018, #208288, #60995, #193121, #142277, #94586, #12229, #143352, #14356, #209347, #79378, #160628, #158499, #63129, #108746, #46904, #111954, #210429, #174772, #127148, #78302 ),
 ( #26347, #129293, #125014, #93517, #77234, #179027, #27419, #44769, #92460, #195269, #110877, #144427, #10098, #11156, #177956, #30645, #128226, #176882, #175827, #159559, #28494, #62071, #194188, #45833, #29570, #164890, #184323, #64204, #116203, #97783, #68431, #31708, #212565, #114094, #99897, #100944, #98840, #65236, #130345, #117268, #132435, #197382, #83631, #131386, #49023, #32758, #115142, #47978, #147591, #148651, #19695, #181138, #168096, #165958, #16484, #33818, #18626, #134561, #196334, #182190, #82565, #52211, #180085, #84705, #200564, #35948, #2355, #217, #66288, #198436, #50082, #150792, #102027, #17542, #149714, #1294, #67352, #133497, #199500, #146547, #213609, #51144, #163843, #183266, #34870, #118338, #167031, #15422, #81512, #202699, #201625, #86841, #87909, #173448, #136674, #107423, #105245, #38097, #187531, #172366, #73785, #151854, #121560, #4484, #205911, #3430, #23956, #7702, #123703, #156120, #54349, #153981, #5548, #170216, #90060, #41316, #39162, #71630, #171285, #22877, #21801, #70555, #85773, #152906, #120488, #37012, #203763, #186460, #57546, #137743, #169153, #188602, #69497, #104168, #139881, #55406, #189664, #88993, #155046, #6632, #20746, #72711, #138806, #204825, #135604, #56477, #53274, #122639, #103094, #119405, #185394, #40233, #106344, #28239, #140967, #27163, #44510, #175572, #143102, #190721, #110627, #95403, #94332, #26094, #91127, #211235, #93268, #160374, #8781, #43444, #92208, #206977, #111691, #46635, #125826, #109568, #62860, #59667, #159301, #74864, #193928, #10900, #176628, #157186, #76975, #144174, #13035, #11976, #209095, #142026, #161455, #129025, #192851, #60730, #9848, #126893, #78050, #195001, #58608, #210166, #42384, #79112, #124762, #108494, #174518, #61807, #45575, #191788, #158259, #75923, #127976, #177698, #208040, #29309, #145230, #112758, #25027, #213359, #199235, #133231, #117005, #31445, #14089, #134298, #97524, #178770, #163580, #68166, #162517, #30382, #212298, #200305, #183004, #51957, #148395, #115940, #33560, #132174, #15163, #196080, #47712, #80180, #147331, #214396, #146285, #150531, #81251, #49814, #197124, #113827, #149448, #64980, #181929, #34622, #131135, #48763, #165698, #130085, #17287, #179826, #114875, #180877, #32498, #98572, #67095, #100691, #198180, #164634, #66025, #16218, #82302, #50882, #166769, #63930, #99632, #18364, #84442, #83363, #96468, #2093, #1030, #106082, #120221, #54085, #151594, #104983, #35684, #7439, #73520, #39975, #122378, #185123, #21540, #137482, #72441, #155852, #139622, #136414, #172105, #171023, #23698, #22620, #89808, #205645, #103906, #37828, #101762, #118079, #184066, #87650, #19428, #167829, #88729, #5288, #138542, #186195, #169952, #85508, #3161, #53006, #6372, #69233, #202430, #135351, #201365, #86579, #154787, #119141, #153720, #71366, #204567, #203496, #56214, #36748, #102834, #70298, #168890, #188335, #20493, #55149, #187271, #152643, #4228, #121296, #38897, #78838, #209898, #144959, #26896, #208836, #126623, #10637, #124501, #74599, #140703, #107158, #25828, #93000, #24763, #29046, #190460, #142829, #75663, #206717, #27973, #42119, #60466, #127702, #91938, #157998, #44241, #8518, #110362, #58345, #108231, #174256, #9587, #191522, #160107, #193662, #76713, #141770, #159044, #207778, #43187, #77784, #45305, #156929, #192586, #61536, #111424, #59405, #57283, #177428, #125561, #95129, #109300, #175309, #90865, #176366, #189407, #161178, #12764, #123445, #41049, #94067, #11710, #143905, #173183, #34358, #100431, #14890, #132968, #49545, #198971, #197917, #50615, #18093, #196863, #130867, #194728, #166502, #84181, #180611, #112487, #116740, #115671, #98307, #165428, #147074, #48501, #46367, #182739, #146016, #99376, #178496, #80985, #210965, #62592, #179561, #33292, #128755, #213095, #64725, #181665, #32236, #17025, #30106, #96196, #163309, #162246, #83102, #149182, #114620, #65762, #13833, #759, #164372, #66825, #31182, #79908, #212027, #63670, #129824, #195806, #47443, #113558, #97255, #15956, #82039, #148133, #214134, #131909, #105817, #2901, #68974, #101501, #53828, #36494, #55961, #20234 ) ),
 .UNSPECIFIED., .F., .F., .T. ) 
 B_SPLINE_SURFACE_WITH_KNOTS ( ( 2, 2 ),
 ( 3, 2, 2, 2, 2, 2, 2, 2, 2, 2, 2, 2, 2, 2, 2, 2, 2, 2, 2, 2, 2, 2, 2, 2, 2, 2, 2, 2, 2, 2, 2, 2, 2, 2, 2, 2, 2, 2, 2, 2, 2, 2, 2, 2, 2, 2, 2, 2, 2, 2, 2, 2, 2, 2, 2, 2, 2, 2, 2, 2, 2, 2, 2, 2, 2, 2, 2, 2, 2, 2, 2, 2, 2, 2, 2, 2, 2, 2, 2, 2, 2, 2, 2, 2, 2, 2, 2, 2, 2, 2, 2, 2, 2, 2, 2, 2, 2, 2, 2, 2, 2, 2, 2, 2, 2, 2, 2, 2, 2, 2, 2, 2, 2, 2, 2, 2, 2, 2, 2, 2, 2, 2, 2, 2, 2, 2, 2, 2, 2, 2, 2, 2, 2, 2, 2, 2, 2, 2, 2, 2, 2, 2, 2, 2, 2, 2, 2, 2, 2, 2, 2, 2, 2, 2, 2, 2, 2, 2, 2, 2, 2, 2, 2, 2, 2, 2, 2, 2, 2, 2, 2, 2, 2, 2, 2, 2, 2, 2, 2, 2, 2, 2, 2, 2, 2, 2, 2, 2, 2, 2, 2, 2, 2, 2, 2, 2, 2, 2, 2, 2, 2, 2, 2, 2, 2, 2, 2, 2, 2, 2, 2, 2, 2, 2, 2, 2, 2, 2, 2, 2, 2, 2, 2, 2, 2, 2, 2, 2, 2, 2, 2, 2, 2, 2, 2, 2, 2, 2, 2, 2, 3 ),
 ( 0.000000000000000000, 1.000000000000000000 ),
 ( 0.000000000000000000, 0.004166666666666666609, 0.008333333333333333218, 0.01250000000000000069, 0.01666666666666666644, 0.02083333333333333218, 0.02500000000000000139, 0.02916666666666666713, 0.03333333333333333287, 0.03749999999999999861, 0.04166666666666666435, 0.04583333333333333010, 0.05000000000000000278, 0.05416666666666666852, 0.05833333333333333426, 0.06250000000000000000, 0.06666666666666666574, 0.07083333333333333148, 0.07499999999999999722, 0.07916666666666666297, 0.08333333333333332871, 0.08749999999999999445, 0.09166666666666666019, 0.09583333333333333981, 0.1000000000000000056, 0.1041666666666666713, 0.1083333333333333370, 0.1125000000000000028, 0.1166666666666666685, 0.1208333333333333343, 0.1250000000000000000, 0.1291666666666666796, 0.1333333333333333315, 0.1375000000000000111, 0.1416666666666666630, 0.1458333333333333426, 0.1499999999999999944, 0.1541666666666666741, 0.1583333333333333259, 0.1625000000000000056, 0.1666666666666666574, 0.1708333333333333370, 0.1749999999999999889, 0.1791666666666666685, 0.1833333333333333204, 0.1875000000000000000, 0.1916666666666666796, 0.1958333333333333315, 0.2000000000000000111, 0.2041666666666666630, 0.2083333333333333426, 0.2124999999999999944, 0.2166666666666666741, 0.2208333333333333259, 0.2250000000000000056, 0.2291666666666666574, 0.2333333333333333370, 0.2374999999999999889, 0.2416666666666666685, 0.2458333333333333204, 0.2500000000000000000, 0.2541666666666666519, 0.2583333333333333592, 0.2625000000000000111, 0.2666666666666666630, 0.2708333333333333148, 0.2750000000000000222, 0.2791666666666666741, 0.2833333333333333259, 0.2874999999999999778, 0.2916666666666666852, 0.2958333333333333370, 0.2999999999999999889, 0.3041666666666666408, 0.3083333333333333481, 0.3125000000000000000, 0.3166666666666666519, 0.3208333333333333592, 0.3250000000000000111, 0.3291666666666666630, 0.3333333333333333148, 0.3375000000000000222, 0.3416666666666666741, 0.3458333333333333259, 0.3499999999999999778, 0.3541666666666666852, 0.3583333333333333370, 0.3624999999999999889, 0.3666666666666666408, 0.3708333333333333481, 0.3750000000000000000, 0.3791666666666666519, 0.3833333333333333592, 0.3875000000000000111, 0.3916666666666666630, 0.3958333333333333148, 0.4000000000000000222, 0.4041666666666666741, 0.4083333333333333259, 0.4124999999999999778, 0.4166666666666666852, 0.4208333333333333370, 0.4249999999999999889, 0.4291666666666666408, 0.4333333333333333481, 0.4375000000000000000, 0.4416666666666666519, 0.4458333333333333592, 0.4500000000000000111, 0.4541666666666666630, 0.4583333333333333148, 0.4625000000000000222, 0.4666666666666666741, 0.4708333333333333259, 0.4749999999999999778, 0.4791666666666666852, 0.4833333333333333370, 0.4874999999999999889, 0.4916666666666666408, 0.4958333333333333481, 0.5000000000000000000, 0.5041666666666666519, 0.5083333333333333037, 0.5124999999999999556, 0.5166666666666667185, 0.5208333333333333703, 0.5250000000000000222, 0.5291666666666666741, 0.5333333333333333259, 0.5374999999999999778, 0.5416666666666666297, 0.5458333333333332815, 0.5500000000000000444, 0.5541666666666666963, 0.5583333333333333481, 0.5625000000000000000, 0.5666666666666666519, 0.5708333333333333037, 0.5749999999999999556, 0.5791666666666667185, 0.5833333333333333703, 0.5875000000000000222, 0.5916666666666666741, 0.5958333333333333259, 0.5999999999999999778, 0.6041666666666666297, 0.6083333333333332815, 0.6125000000000000444, 0.6166666666666666963, 0.6208333333333333481, 0.6250000000000000000, 0.6291666666666666519, 0.6333333333333333037, 0.6374999999999999556, 0.6416666666666667185, 0.6458333333333333703, 0.6500000000000000222, 0.6541666666666666741, 0.6583333333333333259, 0.6624999999999999778, 0.6666666666666666297, 0.6708333333333332815, 0.6750000000000000444, 0.6791666666666666963, 0.6833333333333333481, 0.6875000000000000000, 0.6916666666666666519, 0.6958333333333333037, 0.6999999999999999556, 0.7041666666666667185, 0.7083333333333333703, 0.7125000000000000222, 0.7166666666666666741, 0.7208333333333333259, 0.7249999999999999778, 0.7291666666666666297, 0.7333333333333332815, 0.7375000000000000444, 0.7416666666666666963, 0.7458333333333333481, 0.7500000000000000000, 0.7541666666666666519, 0.7583333333333333037, 0.7624999999999999556, 0.7666666666666667185, 0.7708333333333333703, 0.7750000000000000222, 0.7791666666666666741, 0.7833333333333333259, 0.7874999999999999778, 0.7916666666666666297, 0.7958333333333332815, 0.8000000000000000444, 0.8041666666666666963, 0.8083333333333333481, 0.8125000000000000000, 0.8166666666666666519, 0.8208333333333333037, 0.8249999999999999556, 0.8291666666666667185, 0.8333333333333333703, 0.8375000000000000222, 0.8416666666666666741, 0.8458333333333333259, 0.8499999999999999778, 0.8541666666666666297, 0.8583333333333332815, 0.8625000000000000444, 0.8666666666666666963, 0.8708333333333333481, 0.8750000000000000000, 0.8791666666666666519, 0.8833333333333333037, 0.8874999999999999556, 0.8916666666666667185, 0.8958333333333333703, 0.9000000000000000222, 0.9041666666666666741, 0.9083333333333333259, 0.9124999999999999778, 0.9166666666666666297, 0.9208333333333332815, 0.9250000000000000444, 0.9291666666666666963, 0.9333333333333333481, 0.9375000000000000000, 0.9416666666666666519, 0.9458333333333333037, 0.9499999999999999556, 0.9541666666666667185, 0.9583333333333333703, 0.9625000000000000222, 0.9666666666666666741, 0.9708333333333333259, 0.9749999999999999778, 0.9791666666666666297, 0.9833333333333332815, 0.9875000000000000444, 0.9916666666666666963, 0.9958333333333333481, 1.000000000000000000 ),
 .UNSPECIFIED. ) 
 GEOMETRIC_REPRESENTATION_ITEM ( )  RATIONAL_B_SPLINE_SURFACE ( (
 ( 1.000000000000000000, 0.8660254037844387076, 1.000000000000000000, 0.8660254037844387076, 1.000000000000000000, 0.8660254037844387076, 1.000000000000000000, 0.8660254037844387076, 1.000000000000000000, 0.8660254037844387076, 1.000000000000000000, 0.8660254037844387076, 1.000000000000000000, 0.8660254037844387076, 1.000000000000000000, 0.8660254037844387076, 1.000000000000000000, 0.8660254037844387076, 1.000000000000000000, 0.8660254037844387076, 1.000000000000000000, 0.8660254037844387076, 1.000000000000000000, 0.8660254037844387076, 1.000000000000000000, 0.8660254037844387076, 1.000000000000000000, 0.8660254037844387076, 1.000000000000000000, 0.8660254037844387076, 1.000000000000000000, 0.8660254037844387076, 1.000000000000000000, 0.8660254037844387076, 1.000000000000000000, 0.8660254037844387076, 1.000000000000000000, 0.8660254037844387076, 1.000000000000000000, 0.8660254037844387076, 1.000000000000000000, 0.8660254037844387076, 1.000000000000000000, 0.8660254037844387076, 1.000000000000000000, 0.8660254037844387076, 1.000000000000000000, 0.8660254037844387076, 1.000000000000000000, 0.8660254037844387076, 1.000000000000000000, 0.8660254037844387076, 1.000000000000000000, 0.8660254037844387076, 1.000000000000000000, 0.8660254037844387076, 1.000000000000000000, 0.8660254037844387076, 1.000000000000000000, 0.8660254037844387076, 1.000000000000000000, 0.8660254037844387076, 1.000000000000000000, 0.8660254037844387076, 1.000000000000000000, 0.8660254037844387076, 1.000000000000000000, 0.8660254037844387076, 1.000000000000000000, 0.8660254037844387076, 1.000000000000000000, 0.8660254037844387076, 1.000000000000000000, 0.8660254037844387076, 1.000000000000000000, 0.8660254037844387076, 1.000000000000000000, 0.8660254037844387076, 1.000000000000000000, 0.8660254037844387076, 1.000000000000000000, 0.8660254037844387076, 1.000000000000000000, 0.8660254037844387076, 1.000000000000000000, 0.8660254037844387076, 1.000000000000000000, 0.8660254037844387076, 1.000000000000000000, 0.8660254037844387076, 1.000000000000000000, 0.8660254037844387076, 1.000000000000000000, 0.8660254037844387076, 1.000000000000000000, 0.8660254037844387076, 1.000000000000000000, 0.8660254037844387076, 1.000000000000000000, 0.8660254037844387076, 1.000000000000000000, 0.8660254037844387076, 1.000000000000000000, 0.8660254037844387076, 1.000000000000000000, 0.8660254037844387076, 1.000000000000000000, 0.8660254037844387076, 1.000000000000000000, 0.8660254037844387076, 1.000000000000000000, 0.8660254037844387076, 1.000000000000000000, 0.8660254037844387076, 1.000000000000000000, 0.8660254037844387076, 1.000000000000000000, 0.8660254037844387076, 1.000000000000000000, 0.8660254037844387076, 1.000000000000000000, 0.8660254037844387076, 1.000000000000000000, 0.8660254037844387076, 1.000000000000000000, 0.8660254037844387076, 1.000000000000000000, 0.8660254037844387076, 1.000000000000000000, 0.8660254037844387076, 1.000000000000000000, 0.8660254037844387076, 1.000000000000000000, 0.8660254037844387076, 1.000000000000000000, 0.8660254037844387076, 1.000000000000000000, 0.8660254037844387076, 1.000000000000000000, 0.8660254037844387076, 1.000000000000000000, 0.8660254037844387076, 1.000000000000000000, 0.8660254037844387076, 1.000000000000000000, 0.8660254037844387076, 1.000000000000000000, 0.8660254037844387076, 1.000000000000000000, 0.8660254037844387076, 1.000000000000000000, 0.8660254037844387076, 1.000000000000000000, 0.8660254037844387076, 1.000000000000000000, 0.8660254037844387076, 1.000000000000000000, 0.8660254037844387076, 1.000000000000000000, 0.8660254037844387076, 1.000000000000000000, 0.8660254037844387076, 1.000000000000000000, 0.8660254037844387076, 1.000000000000000000, 0.8660254037844387076, 1.000000000000000000, 0.8660254037844387076, 1.000000000000000000, 0.8660254037844387076, 1.000000000000000000, 0.8660254037844387076, 1.000000000000000000, 0.8660254037844387076, 1.000000000000000000, 0.8660254037844387076, 1.000000000000000000, 0.8660254037844387076, 1.000000000000000000, 0.8660254037844387076, 1.000000000000000000, 0.8660254037844387076, 1.000000000000000000, 0.8660254037844387076, 1.000000000000000000, 0.8660254037844387076, 1.000000000000000000, 0.8660254037844387076, 1.000000000000000000, 0.8660254037844387076, 1.000000000000000000, 0.8660254037844387076, 1.000000000000000000, 0.8660254037844387076, 1.000000000000000000, 0.8660254037844387076, 1.000000000000000000, 0.8660254037844387076, 1.000000000000000000, 0.8660254037844387076, 1.000000000000000000, 0.8660254037844387076, 1.000000000000000000, 0.8660254037844387076, 1.000000000000000000, 0.8660254037844387076, 1.000000000000000000, 0.8660254037844387076, 1.000000000000000000, 0.8660254037844387076, 1.000000000000000000, 0.8660254037844387076, 1.000000000000000000, 0.8660254037844387076, 1.000000000000000000, 0.8660254037844387076, 1.000000000000000000, 0.8660254037844387076, 1.000000000000000000, 0.8660254037844387076, 1.000000000000000000, 0.8660254037844387076, 1.000000000000000000, 0.8660254037844387076, 1.000000000000000000, 0.8660254037844387076, 1.000000000000000000, 0.8660254037844387076, 1.000000000000000000, 0.8660254037844387076, 1.000000000000000000, 0.8660254037844387076, 1.000000000000000000, 0.8660254037844387076, 1.000000000000000000, 0.8660254037844387076, 1.000000000000000000, 0.8660254037844387076, 1.000000000000000000, 0.8660254037844387076, 1.000000000000000000, 0.8660254037844387076, 1.000000000000000000, 0.8660254037844387076, 1.000000000000000000, 0.8660254037844387076, 1.000000000000000000, 0.8660254037844387076, 1.000000000000000000, 0.8660254037844387076, 1.000000000000000000, 0.8660254037844387076, 1.000000000000000000, 0.8660254037844387076, 1.000000000000000000, 0.8660254037844387076, 1.000000000000000000, 0.8660254037844387076, 1.000000000000000000, 0.8660254037844387076, 1.000000000000000000, 0.8660254037844387076, 1.000000000000000000, 0.8660254037844387076, 1.000000000000000000, 0.8660254037844387076, 1.000000000000000000, 0.8660254037844387076, 1.000000000000000000, 0.8660254037844387076, 1.000000000000000000, 0.8660254037844387076, 1.000000000000000000, 0.8660254037844387076, 1.000000000000000000, 0.8660254037844387076, 1.000000000000000000, 0.8660254037844387076, 1.000000000000000000, 0.8660254037844387076, 1.000000000000000000, 0.8660254037844387076, 1.000000000000000000, 0.8660254037844387076, 1.000000000000000000, 0.8660254037844387076, 1.000000000000000000, 0.8660254037844387076, 1.000000000000000000, 0.8660254037844387076, 1.000000000000000000, 0.8660254037844387076, 1.000000000000000000, 0.8660254037844387076, 1.000000000000000000, 0.8660254037844387076, 1.000000000000000000, 0.8660254037844387076, 1.000000000000000000, 0.8660254037844387076, 1.000000000000000000, 0.8660254037844387076, 1.000000000000000000, 0.8660254037844387076, 1.000000000000000000, 0.8660254037844387076, 1.000000000000000000, 0.8660254037844387076, 1.000000000000000000, 0.8660254037844387076, 1.000000000000000000, 0.8660254037844387076, 1.000000000000000000, 0.8660254037844387076, 1.000000000000000000, 0.8660254037844387076, 1.000000000000000000, 0.8660254037844387076, 1.000000000000000000, 0.8660254037844387076, 1.000000000000000000, 0.8660254037844387076, 1.000000000000000000, 0.8660254037844387076, 1.000000000000000000, 0.8660254037844387076, 1.000000000000000000, 0.8660254037844387076, 1.000000000000000000, 0.8660254037844387076, 1.000000000000000000, 0.8660254037844387076, 1.000000000000000000, 0.8660254037844387076, 1.000000000000000000, 0.8660254037844387076, 1.000000000000000000, 0.8660254037844387076, 1.000000000000000000, 0.8660254037844387076, 1.000000000000000000, 0.8660254037844387076, 1.000000000000000000, 0.8660254037844387076, 1.000000000000000000, 0.8660254037844387076, 1.000000000000000000, 0.8660254037844387076, 1.000000000000000000, 0.8660254037844387076, 1.000000000000000000, 0.8660254037844387076, 1.000000000000000000, 0.8660254037844387076, 1.000000000000000000, 0.8660254037844387076, 1.000000000000000000, 0.8660254037844387076, 1.000000000000000000, 0.8660254037844387076, 1.000000000000000000, 0.8660254037844387076, 1.000000000000000000, 0.8660254037844387076, 1.000000000000000000, 0.8660254037844387076, 1.000000000000000000, 0.8660254037844387076, 1.000000000000000000, 0.8660254037844387076, 1.000000000000000000, 0.8660254037844387076, 1.000000000000000000, 0.8660254037844387076, 1.000000000000000000, 0.8660254037844387076, 1.000000000000000000, 0.8660254037844387076, 1.000000000000000000, 0.8660254037844387076, 1.000000000000000000, 0.8660254037844387076, 1.000000000000000000, 0.8660254037844387076, 1.000000000000000000, 0.8660254037844387076, 1.000000000000000000, 0.8660254037844387076, 1.000000000000000000, 0.8660254037844387076, 1.000000000000000000, 0.8660254037844387076, 1.000000000000000000, 0.8660254037844387076, 1.000000000000000000, 0.8660254037844387076, 1.000000000000000000, 0.8660254037844387076, 1.000000000000000000, 0.8660254037844387076, 1.000000000000000000, 0.8660254037844387076, 1.000000000000000000, 0.8660254037844387076, 1.000000000000000000, 0.8660254037844387076, 1.000000000000000000, 0.8660254037844387076, 1.000000000000000000, 0.8660254037844387076, 1.000000000000000000, 0.8660254037844387076, 1.000000000000000000, 0.8660254037844387076, 1.000000000000000000, 0.8660254037844387076, 1.000000000000000000, 0.8660254037844387076, 1.000000000000000000, 0.8660254037844387076, 1.000000000000000000, 0.8660254037844387076, 1.000000000000000000, 0.8660254037844387076, 1.000000000000000000, 0.8660254037844387076, 1.000000000000000000, 0.8660254037844387076, 1.000000000000000000, 0.8660254037844387076, 1.000000000000000000, 0.8660254037844387076, 1.000000000000000000, 0.8660254037844387076, 1.000000000000000000, 0.8660254037844387076, 1.000000000000000000, 0.8660254037844387076, 1.000000000000000000, 0.8660254037844387076, 1.000000000000000000, 0.8660254037844387076, 1.000000000000000000, 0.8660254037844387076, 1.000000000000000000, 0.8660254037844387076, 1.000000000000000000, 0.8660254037844387076, 1.000000000000000000, 0.8660254037844387076, 1.000000000000000000, 0.8660254037844387076, 1.000000000000000000, 0.8660254037844387076, 1.000000000000000000, 0.8660254037844387076, 1.000000000000000000, 0.8660254037844387076, 1.000000000000000000, 0.8660254037844387076, 1.000000000000000000, 0.8660254037844387076, 1.000000000000000000, 0.8660254037844387076, 1.000000000000000000, 0.8660254037844387076, 1.000000000000000000, 0.8660254037844387076, 1.000000000000000000, 0.8660254037844387076, 1.000000000000000000, 0.8660254037844387076, 1.000000000000000000, 0.8660254037844387076, 1.000000000000000000, 0.8660254037844387076, 1.000000000000000000, 0.8660254037844387076, 1.000000000000000000, 0.8660254037844387076, 1.000000000000000000),
 ( 1.000000000000000000, 0.8660254037844387076, 1.000000000000000000, 0.8660254037844387076, 1.000000000000000000, 0.8660254037844387076, 1.000000000000000000, 0.8660254037844387076, 1.000000000000000000, 0.8660254037844387076, 1.000000000000000000, 0.8660254037844387076, 1.000000000000000000, 0.8660254037844387076, 1.000000000000000000, 0.8660254037844387076, 1.000000000000000000, 0.8660254037844387076, 1.000000000000000000, 0.8660254037844387076, 1.000000000000000000, 0.8660254037844387076, 1.000000000000000000, 0.8660254037844387076, 1.000000000000000000, 0.8660254037844387076, 1.000000000000000000, 0.8660254037844387076, 1.000000000000000000, 0.8660254037844387076, 1.000000000000000000, 0.8660254037844387076, 1.000000000000000000, 0.8660254037844387076, 1.000000000000000000, 0.8660254037844387076, 1.000000000000000000, 0.8660254037844387076, 1.000000000000000000, 0.8660254037844387076, 1.000000000000000000, 0.8660254037844387076, 1.000000000000000000, 0.8660254037844387076, 1.000000000000000000, 0.8660254037844387076, 1.000000000000000000, 0.8660254037844387076, 1.000000000000000000, 0.8660254037844387076, 1.000000000000000000, 0.8660254037844387076, 1.000000000000000000, 0.8660254037844387076, 1.000000000000000000, 0.8660254037844387076, 1.000000000000000000, 0.8660254037844387076, 1.000000000000000000, 0.8660254037844387076, 1.000000000000000000, 0.8660254037844387076, 1.000000000000000000, 0.8660254037844387076, 1.000000000000000000, 0.8660254037844387076, 1.000000000000000000, 0.8660254037844387076, 1.000000000000000000, 0.8660254037844387076, 1.000000000000000000, 0.8660254037844387076, 1.000000000000000000, 0.8660254037844387076, 1.000000000000000000, 0.8660254037844387076, 1.000000000000000000, 0.8660254037844387076, 1.000000000000000000, 0.8660254037844387076, 1.000000000000000000, 0.8660254037844387076, 1.000000000000000000, 0.8660254037844387076, 1.000000000000000000, 0.8660254037844387076, 1.000000000000000000, 0.8660254037844387076, 1.000000000000000000, 0.8660254037844387076, 1.000000000000000000, 0.8660254037844387076, 1.000000000000000000, 0.8660254037844387076, 1.000000000000000000, 0.8660254037844387076, 1.000000000000000000, 0.8660254037844387076, 1.000000000000000000, 0.8660254037844387076, 1.000000000000000000, 0.8660254037844387076, 1.000000000000000000, 0.8660254037844387076, 1.000000000000000000, 0.8660254037844387076, 1.000000000000000000, 0.8660254037844387076, 1.000000000000000000, 0.8660254037844387076, 1.000000000000000000, 0.8660254037844387076, 1.000000000000000000, 0.8660254037844387076, 1.000000000000000000, 0.8660254037844387076, 1.000000000000000000, 0.8660254037844387076, 1.000000000000000000, 0.8660254037844387076, 1.000000000000000000, 0.8660254037844387076, 1.000000000000000000, 0.8660254037844387076, 1.000000000000000000, 0.8660254037844387076, 1.000000000000000000, 0.8660254037844387076, 1.000000000000000000, 0.8660254037844387076, 1.000000000000000000, 0.8660254037844387076, 1.000000000000000000, 0.8660254037844387076, 1.000000000000000000, 0.8660254037844387076, 1.000000000000000000, 0.8660254037844387076, 1.000000000000000000, 0.8660254037844387076, 1.000000000000000000, 0.8660254037844387076, 1.000000000000000000, 0.8660254037844387076, 1.000000000000000000, 0.8660254037844387076, 1.000000000000000000, 0.8660254037844387076, 1.000000000000000000, 0.8660254037844387076, 1.000000000000000000, 0.8660254037844387076, 1.000000000000000000, 0.8660254037844387076, 1.000000000000000000, 0.8660254037844387076, 1.000000000000000000, 0.8660254037844387076, 1.000000000000000000, 0.8660254037844387076, 1.000000000000000000, 0.8660254037844387076, 1.000000000000000000, 0.8660254037844387076, 1.000000000000000000, 0.8660254037844387076, 1.000000000000000000, 0.8660254037844387076, 1.000000000000000000, 0.8660254037844387076, 1.000000000000000000, 0.8660254037844387076, 1.000000000000000000, 0.8660254037844387076, 1.000000000000000000, 0.8660254037844387076, 1.000000000000000000, 0.8660254037844387076, 1.000000000000000000, 0.8660254037844387076, 1.000000000000000000, 0.8660254037844387076, 1.000000000000000000, 0.8660254037844387076, 1.000000000000000000, 0.8660254037844387076, 1.000000000000000000, 0.8660254037844387076, 1.000000000000000000, 0.8660254037844387076, 1.000000000000000000, 0.8660254037844387076, 1.000000000000000000, 0.8660254037844387076, 1.000000000000000000, 0.8660254037844387076, 1.000000000000000000, 0.8660254037844387076, 1.000000000000000000, 0.8660254037844387076, 1.000000000000000000, 0.8660254037844387076, 1.000000000000000000, 0.8660254037844387076, 1.000000000000000000, 0.8660254037844387076, 1.000000000000000000, 0.8660254037844387076, 1.000000000000000000, 0.8660254037844387076, 1.000000000000000000, 0.8660254037844387076, 1.000000000000000000, 0.8660254037844387076, 1.000000000000000000, 0.8660254037844387076, 1.000000000000000000, 0.8660254037844387076, 1.000000000000000000, 0.8660254037844387076, 1.000000000000000000, 0.8660254037844387076, 1.000000000000000000, 0.8660254037844387076, 1.000000000000000000, 0.8660254037844387076, 1.000000000000000000, 0.8660254037844387076, 1.000000000000000000, 0.8660254037844387076, 1.000000000000000000, 0.8660254037844387076, 1.000000000000000000, 0.8660254037844387076, 1.000000000000000000, 0.8660254037844387076, 1.000000000000000000, 0.8660254037844387076, 1.000000000000000000, 0.8660254037844387076, 1.000000000000000000, 0.8660254037844387076, 1.000000000000000000, 0.8660254037844387076, 1.000000000000000000, 0.8660254037844387076, 1.000000000000000000, 0.8660254037844387076, 1.000000000000000000, 0.8660254037844387076, 1.000000000000000000, 0.8660254037844387076, 1.000000000000000000, 0.8660254037844387076, 1.000000000000000000, 0.8660254037844387076, 1.000000000000000000, 0.8660254037844387076, 1.000000000000000000, 0.8660254037844387076, 1.000000000000000000, 0.8660254037844387076, 1.000000000000000000, 0.8660254037844387076, 1.000000000000000000, 0.8660254037844387076, 1.000000000000000000, 0.8660254037844387076, 1.000000000000000000, 0.8660254037844387076, 1.000000000000000000, 0.8660254037844387076, 1.000000000000000000, 0.8660254037844387076, 1.000000000000000000, 0.8660254037844387076, 1.000000000000000000, 0.8660254037844387076, 1.000000000000000000, 0.8660254037844387076, 1.000000000000000000, 0.8660254037844387076, 1.000000000000000000, 0.8660254037844387076, 1.000000000000000000, 0.8660254037844387076, 1.000000000000000000, 0.8660254037844387076, 1.000000000000000000, 0.8660254037844387076, 1.000000000000000000, 0.8660254037844387076, 1.000000000000000000, 0.8660254037844387076, 1.000000000000000000, 0.8660254037844387076, 1.000000000000000000, 0.8660254037844387076, 1.000000000000000000, 0.8660254037844387076, 1.000000000000000000, 0.8660254037844387076, 1.000000000000000000, 0.8660254037844387076, 1.000000000000000000, 0.8660254037844387076, 1.000000000000000000, 0.8660254037844387076, 1.000000000000000000, 0.8660254037844387076, 1.000000000000000000, 0.8660254037844387076, 1.000000000000000000, 0.8660254037844387076, 1.000000000000000000, 0.8660254037844387076, 1.000000000000000000, 0.8660254037844387076, 1.000000000000000000, 0.8660254037844387076, 1.000000000000000000, 0.8660254037844387076, 1.000000000000000000, 0.8660254037844387076, 1.000000000000000000, 0.8660254037844387076, 1.000000000000000000, 0.8660254037844387076, 1.000000000000000000, 0.8660254037844387076, 1.000000000000000000, 0.8660254037844387076, 1.000000000000000000, 0.8660254037844387076, 1.000000000000000000, 0.8660254037844387076, 1.000000000000000000, 0.8660254037844387076, 1.000000000000000000, 0.8660254037844387076, 1.000000000000000000, 0.8660254037844387076, 1.000000000000000000, 0.8660254037844387076, 1.000000000000000000, 0.8660254037844387076, 1.000000000000000000, 0.8660254037844387076, 1.000000000000000000, 0.8660254037844387076, 1.000000000000000000, 0.8660254037844387076, 1.000000000000000000, 0.8660254037844387076, 1.000000000000000000, 0.8660254037844387076, 1.000000000000000000, 0.8660254037844387076, 1.000000000000000000, 0.8660254037844387076, 1.000000000000000000, 0.8660254037844387076, 1.000000000000000000, 0.8660254037844387076, 1.000000000000000000, 0.8660254037844387076, 1.000000000000000000, 0.8660254037844387076, 1.000000000000000000, 0.8660254037844387076, 1.000000000000000000, 0.8660254037844387076, 1.000000000000000000, 0.8660254037844387076, 1.000000000000000000, 0.8660254037844387076, 1.000000000000000000, 0.8660254037844387076, 1.000000000000000000, 0.8660254037844387076, 1.000000000000000000, 0.8660254037844387076, 1.000000000000000000, 0.8660254037844387076, 1.000000000000000000, 0.8660254037844387076, 1.000000000000000000, 0.8660254037844387076, 1.000000000000000000, 0.8660254037844387076, 1.000000000000000000, 0.8660254037844387076, 1.000000000000000000, 0.8660254037844387076, 1.000000000000000000, 0.8660254037844387076, 1.000000000000000000, 0.8660254037844387076, 1.000000000000000000, 0.8660254037844387076, 1.000000000000000000, 0.8660254037844387076, 1.000000000000000000, 0.8660254037844387076, 1.000000000000000000, 0.8660254037844387076, 1.000000000000000000, 0.8660254037844387076, 1.000000000000000000, 0.8660254037844387076, 1.000000000000000000, 0.8660254037844387076, 1.000000000000000000, 0.8660254037844387076, 1.000000000000000000, 0.8660254037844387076, 1.000000000000000000, 0.8660254037844387076, 1.000000000000000000, 0.8660254037844387076, 1.000000000000000000, 0.8660254037844387076, 1.000000000000000000, 0.8660254037844387076, 1.000000000000000000, 0.8660254037844387076, 1.000000000000000000, 0.8660254037844387076, 1.000000000000000000, 0.8660254037844387076, 1.000000000000000000, 0.8660254037844387076, 1.000000000000000000, 0.8660254037844387076, 1.000000000000000000, 0.8660254037844387076, 1.000000000000000000, 0.8660254037844387076, 1.000000000000000000, 0.8660254037844387076, 1.000000000000000000, 0.8660254037844387076, 1.000000000000000000, 0.8660254037844387076, 1.000000000000000000, 0.8660254037844387076, 1.000000000000000000, 0.8660254037844387076, 1.000000000000000000, 0.8660254037844387076, 1.000000000000000000, 0.8660254037844387076, 1.000000000000000000, 0.8660254037844387076, 1.000000000000000000, 0.8660254037844387076, 1.000000000000000000, 0.8660254037844387076, 1.000000000000000000, 0.8660254037844387076, 1.000000000000000000, 0.8660254037844387076, 1.000000000000000000, 0.8660254037844387076, 1.000000000000000000, 0.8660254037844387076, 1.000000000000000000, 0.8660254037844387076, 1.000000000000000000, 0.8660254037844387076, 1.000000000000000000, 0.8660254037844387076, 1.000000000000000000, 0.8660254037844387076, 1.000000000000000000, 0.8660254037844387076, 1.000000000000000000, 0.8660254037844387076, 1.000000000000000000, 0.8660254037844387076, 1.000000000000000000) ) ) 
 REPRESENTATION_ITEM ( '' )  SURFACE ( )  );
#190846 = ORIENTED_EDGE ( 'NONE', *, *, #207247, .T. ) ;
#190847 = CARTESIAN_POINT ( 'NONE',  ( 1.499999999999989120, 2.785416667349484676, 0.8660254037844524744 ) ) ;
#190848 = CARTESIAN_POINT ( 'NONE',  ( 1.364683531249988535, 3.717708333674750953, -0.7879004041258239610 ) ) ;
#190849 = CARTESIAN_POINT ( 'NONE',  ( 3.549935554046261821, 1.870726058081632504, 0.003126486288931861444 ) ) ;
#190850 = CARTESIAN_POINT ( 'NONE',  ( 2.865509578329272777, -0.1299577181766899403, -1.729349861900606022 ) ) ;
#190851 = CARTESIAN_POINT ( 'NONE',  ( 6.409741707328596938, -1.031184584194230647, -1.933826218581576439 ) ) ;
#190852 = CARTESIAN_POINT ( 'NONE',  ( 0.5697015142280477118, 0.2141057807664332180, -2.196374807094509496 ) ) ;
#190853 = CARTESIAN_POINT ( 'NONE',  ( 4.704676425016507402, 1.819892833079386651, 1.028999879293402531 ) ) ;
#190854 = CARTESIAN_POINT ( 'NONE',  ( 5.630791504788829727, -1.754662785997921359, 0.8323459256341717571 ) ) ;
#190856 = ORIENTED_EDGE ( 'NONE', *, *, #75342, .F. ) ;
#190855 = CARTESIAN_POINT ( 'NONE',  ( 9.255591775348552375, 14.20198051862420385, 7.641521890740467171 ) ) ;
#190857 = CARTESIAN_POINT ( 'NONE',  ( 0.0006249722829775038483, -1.976948959267275541, 0.3961041280396286890 ) ) ;
#190858 = FILL_AREA_STYLE_COLOUR ( '', #138211 ) ;
#190859 = FACE_OUTER_BOUND ( 'NONE', #156018, .T. ) ;
#190860 = SURFACE_SIDE_STYLE ('',( #124897 ) ) ;
#190861 = CARTESIAN_POINT ( 'NONE',  ( -9.501566725078754772, 9.979582688880366703, -0.7998128361456291469 ) ) ;
#190862 = CARTESIAN_POINT ( 'NONE',  ( 6.551614543901692400, 8.666636272683888365, 1.599625672291281386 ) ) ;
#190863 = DIRECTION ( 'NONE',  ( -0.000000000000000000, 1.000000000000000000, -0.000000000000000000 ) ) ;
#190864 = CARTESIAN_POINT ( 'NONE',  ( 4.002439121739418404, -0.5745171773131328985, -1.733004836422600725 ) ) ;
#190865 = CARTESIAN_POINT ( 'NONE',  ( 2.643839551151895506, -1.634601560588926361, -1.482707865360691990 ) ) ;
#190866 = ORIENTED_EDGE ( 'NONE', *, *, #164153, .F. ) ;
#190867 = CARTESIAN_POINT ( 'NONE',  ( -5.772739544368596043, 9.956889578397179363, -0.7998128361456362523 ) ) ;
#190868 = CARTESIAN_POINT ( 'NONE',  ( 0.000000000000000000, -2.734374999522040550, -3.793834371823813001 ) ) ;
#190869 = CARTESIAN_POINT ( 'NONE',  ( -7.965578943228732278, 9.251929174310385307, -1.199719254218446718 ) ) ;
#190870 = CARTESIAN_POINT ( 'NONE',  ( 1.353777543752776591, -1.465856132443652760, -1.389804628120022478 ) ) ;
#190871 = CARTESIAN_POINT ( 'NONE',  ( 11.89835103415199313, 9.771069141675322811, 1.561208891256346876 ) ) ;
#190872 = CARTESIAN_POINT ( 'NONE',  ( -4.146814880933400005, 5.931313009212638931, 1.599625672291270506 ) ) ;
#190873 = CARTESIAN_POINT ( 'NONE',  ( 2.887382943596613849, -1.738241981009930992, 0.6650857031204291392 ) ) ;
#190874 = CARTESIAN_POINT ( 'NONE',  ( 4.227444969362701421, 3.826440640544909400, 1.214306433183764966E-14 ) ) ;
#190875 = DIRECTION ( 'NONE',  ( -1.000000000000000000, 0.000000000000000000, 0.000000000000000000 ) ) ;
#190876 = ORIENTED_EDGE ( 'NONE', *, *, #208132, .T. ) ;
#190877 = EDGE_LOOP ( 'NONE', ( #159056, #75964 ) ) ;
#190878 = CARTESIAN_POINT ( 'NONE',  ( -3.554208825076827782, 7.298327395898266623, 0.7998128361456341429 ) ) ;
#190879 = CARTESIAN_POINT ( 'NONE',  ( -7.133561379084627063, 11.47423870890741782, 0.7998128361456481317 ) ) ;
#190880 = CARTESIAN_POINT ( 'NONE',  ( 4.336427269025699971, 1.790907886515300085, 0.3537760332646966432 ) ) ;
#190882 = FACE_BOUND ( 'NONE', #17579, .T. ) ;
#190881 = CARTESIAN_POINT ( 'NONE',  ( -2.830620210203090181, 6.524417021870718258, 0.000000000000000000 ) ) ;
#190883 = CARTESIAN_POINT ( 'NONE',  ( 6.142241479726070708, 7.081583759122534794, -1.089790755372788800 ) ) ;
#190884 = CARTESIAN_POINT ( 'NONE',  ( 0.7722569432341424012, -1.726285329646786382, 0.1615719764154876226 ) ) ;
#190885 = CARTESIAN_POINT ( 'NONE',  ( 6.158133876658566486, -1.298579738958350660, 1.305440813956220136 ) ) ;
#190886 = CARTESIAN_POINT ( 'NONE',  ( 4.934332944283116973, 1.189700906406887082, -1.977258547338469841 ) ) ;
#190887 = CARTESIAN_POINT ( 'NONE',  ( 5.337069745634900997, 6.255611453776062980, 1.199719254218452047 ) ) ;
#190888 = CARTESIAN_POINT ( 'NONE',  ( 6.555963963954187790, 2.156316573842661732, -0.1517529999496904924 ) ) ;
#190889 = CARTESIAN_POINT ( 'NONE',  ( 6.388916700537700777, 8.476822122092563916, 1.599625672291281386 ) ) ;
#190890 = EDGE_CURVE ( 'NONE', #96623, #33092, #84824, .T. ) ;
#190891 = CARTESIAN_POINT ( 'NONE',  ( 5.519047587058080850, 2.296088720628499669, -0.1051655125834053545 ) ) ;
#190892 = LINE ( 'NONE', #108660, #16822 ) ;
#190893 = CARTESIAN_POINT ( 'NONE',  ( -2.844178363816758814, 6.540234867753325076, -0.7998128361456481317 ) ) ;
#190894 = MECHANICAL_DESIGN_GEOMETRIC_PRESENTATION_REPRESENTATION (  '', ( #73224 ), #42186 ) ;
#190895 = CARTESIAN_POINT ( 'NONE',  ( 5.330866702616011921, 0.1386157390740362649, 1.865562100978317206 ) ) ;
#190896 = ORIENTED_EDGE ( 'NONE', *, *, #88030, .T. ) ;
#190898 = CARTESIAN_POINT ( 'NONE',  ( -4.797606254389363833, 6.690569611577942943, 1.599625672291263179 ) ) ;
#190897 = CARTESIAN_POINT ( 'NONE',  ( 2.390748813209525814, -1.831196095803063528, -0.5514187292172747501 ) ) ;
#190899 = CARTESIAN_POINT ( 'NONE',  ( 3.457846583235091753, 0.5364296187198510646, -2.140574738106671759 ) ) ;
#190900 = CARTESIAN_POINT ( 'NONE',  ( 4.680926624126137803, 1.758507693093620539, -1.179036559061322542 ) ) ;
#190901 = CARTESIAN_POINT ( 'NONE',  ( 1.224999999999935030, 0.7083333340161593883, -0.7072540797573136917 ) ) ;
#190902 = CARTESIAN_POINT ( 'NONE',  ( 6.883263157960393563, 1.268976584491373183, 2.060807272249213451 ) ) ;
#190903 = CARTESIAN_POINT ( 'NONE',  ( -0.2110808730067300354, 7.629137130509040077, -2.397154524934116182 ) ) ;
#190904 = CARTESIAN_POINT ( 'NONE',  ( 5.031484404002878996, 7.923796667095108326, 1.082531754730548412 ) ) ;
#190905 = CARTESIAN_POINT ( 'NONE',  ( -6.414416072596857532, 6.656109304217339151, -0.7216878364870338292 ) ) ;
#190906 = CARTESIAN_POINT ( 'NONE',  ( 2.556097155687846900, 0.6156694008866661072, -2.223864192518353544 ) ) ;
#190907 = CARTESIAN_POINT ( 'NONE',  ( 2.699599903323801620, -1.451799986561516764, -1.319707477925702310 ) ) ;
#190908 = CARTESIAN_POINT ( 'NONE',  ( -4.990283058281743678, 7.979691447040783814, -1.199719254218453823 ) ) ;
#190909 = CARTESIAN_POINT ( 'NONE',  ( 6.596538677256176264, 2.039275035945103731, 0.3085339683557372092 ) ) ;
#190910 = CARTESIAN_POINT ( 'NONE',  ( 3.389175213736297820, 4.977123720824209840, 1.443375672974062551 ) ) ;
#190911 = CARTESIAN_POINT ( 'NONE',  ( 3.444653546323793947, 6.176457016423196222, 1.199719254218451159 ) ) ;
#190912 = ORIENTED_EDGE ( 'NONE', *, *, #168015, .T. ) ;
#190913 = CARTESIAN_POINT ( 'NONE',  ( 4.680875185974167074, 1.673856063443099895, -1.124242729735332347 ) ) ;
#190914 = CARTESIAN_POINT ( 'NONE',  ( -9.215791728987058562, 11.77484298861683598, -1.599625672291263179 ) ) ;
#190915 = CARTESIAN_POINT ( 'NONE',  ( -4.489620702586434753, 8.251817990458562235, -0.01816452336140990040 ) ) ;
#190916 = CARTESIAN_POINT ( 'NONE',  ( -10.45911201557330195, 5.175391108250987138, -5.201428006079835242 ) ) ;
#190917 = CARTESIAN_POINT ( 'NONE',  ( 8.778014389843965759, 12.32843499053828928, 1.199719254218450271 ) ) ;
#190918 = CARTESIAN_POINT ( 'NONE',  ( 2.254941745292405653, -0.5755891407489240885, -2.093346358694737841 ) ) ;
#190919 = FILL_AREA_STYLE ('',( #158443 ) ) ;
#190920 = FILL_AREA_STYLE ('',( #171485 ) ) ;
#190921 = CARTESIAN_POINT ( 'NONE',  ( 4.112618025573818947, 7.490225759230090041, 0.7307243446277329468 ) ) ;
#190922 = CARTESIAN_POINT ( 'NONE',  ( 2.090876104454452378, 1.629797177321444579, -0.9178172146045021629 ) ) ;
#190923 = CARTESIAN_POINT ( 'NONE',  ( 0.3333698182165916735, -1.885181130612986866, 0.8328085122516776240 ) ) ;
#190924 = AXIS2_PLACEMENT_3D ( 'NONE', #34569, #148341, #149396 ) ;
#190925 = CARTESIAN_POINT ( 'NONE',  ( -6.471393748265538370, 5.229711127717889596, -2.499999999999995115 ) ) ;
#190926 = CARTESIAN_POINT ( 'NONE',  ( 1.364683531249986537, 0.6552083336747522857, -0.7879004041258239610 ) ) ;
#190927 = ORIENTED_EDGE ( 'NONE', *, *, #60315, .T. ) ;
#190928 = CARTESIAN_POINT ( 'NONE',  ( 3.879479457080482696, 0.2311173251203814394, -1.898182577502210977 ) ) ;
#190929 =( BOUNDED_CURVE ( )  B_SPLINE_CURVE ( 2, ( #74897, #91167, #39191, #138843, #204860, #141006, #208076, #207013, #58644 ),
 .UNSPECIFIED., .F., .T. ) 
 B_SPLINE_CURVE_WITH_KNOTS ( ( 3, 2, 2, 2, 3 ),
 ( 0.7589285714285713969, 0.7619047619047618625, 0.7678571428571429047, 0.7738095238095238360, 0.7767857142857143016 ),
 .UNSPECIFIED. ) 
 CURVE ( )  GEOMETRIC_REPRESENTATION_ITEM ( )  RATIONAL_B_SPLINE_CURVE ( ( 0.9330127018922194093, 0.9330127018922194093, 1.000000000000000000, 0.8660254037844387076, 1.000000000000000000, 0.8660254037844387076, 1.000000000000000000, 0.9330127018922194093, 0.9330127018922194093 ) ) 
 REPRESENTATION_ITEM ( '' )  );
#190930 = CARTESIAN_POINT ( 'NONE',  ( 4.733122822409558950, -1.617543599503493468, 0.7186682867280795861 ) ) ;
#190931 = CARTESIAN_POINT ( 'NONE',  ( 1.523922206041250949, -1.897707704667614959, 0.2351830868887184178 ) ) ;
#190932 = CARTESIAN_POINT ( 'NONE',  ( -4.952806187693842510, 4.672695395264567786, 0.7998128361456341429 ) ) ;
#190933 = CARTESIAN_POINT ( 'NONE',  ( 0.04005665835727333091, 0.7356861536649759170, 1.769027722964914728 ) ) ;
#190934 = CARTESIAN_POINT ( 'NONE',  ( 0.7499999999999867883, 0.06666666666668707997, -1.299038105676652899 ) ) ;
#190935 = CARTESIAN_POINT ( 'NONE',  ( 1.082579992370054311, 1.234693400583252609, -1.661741702728709802 ) ) ;
#190936 = CARTESIAN_POINT ( 'NONE',  ( 1.499999999999989120, 5.545833333333350268, -0.8660254037844323793 ) ) ;
#190937 = CARTESIAN_POINT ( 'NONE',  ( 5.910993886665249164, 1.650546521282238110, 0.8803886038859505270 ) ) ;
#190938 = CARTESIAN_POINT ( 'NONE',  ( 2.033574986395149775, -1.191784744093337123, -1.383114941912518159 ) ) ;
#190940 = CARTESIAN_POINT ( 'NONE',  ( 4.596835240751270035, 8.371391889155539445, -0.09823007671119071693 ) ) ;
#190939 = CARTESIAN_POINT ( 'NONE',  ( 5.742855475442601332, 0.4270144693867898300, 2.165010647329483895 ) ) ;
#190941 = CARTESIAN_POINT ( 'NONE',  ( 1.364683531249988757, -0.1156249996585798079, 0.000000000000000000 ) ) ;
#190942 = CARTESIAN_POINT ( 'NONE',  ( 2.664570663672768180, -0.7871131050594852852, -1.906781320289064885 ) ) ;
#190943 = CARTESIAN_POINT ( 'NONE',  ( -7.901704598666176693, 8.113076874732334076, 0.7998128361456602331 ) ) ;
#190944 = CARTESIAN_POINT ( 'NONE',  ( 7.377608144130607393, 11.75895993479440982, -0.7998128361456291469 ) ) ;
#190945 = CARTESIAN_POINT ( 'NONE',  ( 1.315349297999212075, 3.546208118371547258, -0.4023297572127010335 ) ) ;
#190946 = DIRECTION ( 'NONE',  ( 8.638326563840814399E-31, -0.000000000000000000, 1.000000000000000000 ) ) ;
#190947 = CARTESIAN_POINT ( 'NONE',  ( 6.855582950365507244, 8.027210192628430718, -1.199719254218452047 ) ) ;
#190948 = CARTESIAN_POINT ( 'NONE',  ( 5.670397268163976712, -0.9275489576153757021, -1.851018422006404096 ) ) ;
#190949 = CARTESIAN_POINT ( 'NONE',  ( 1.364683531249986537, 0.7177083336747527298, -0.7879004041258239610 ) ) ;
#190950 = CARTESIAN_POINT ( 'NONE',  ( 2.302237272444170202, -2.161155982280529297, 0.05054500047013688047 ) ) ;
#190951 = CARTESIAN_POINT ( 'NONE',  ( -4.611386515133914621, 8.374621496872018511, -0.1785149356163841239 ) ) ;
#190953 = CARTESIAN_POINT ( 'NONE',  ( 2.119516022818414669, 0.3384452847540948550, -1.932298432780136244 ) ) ;
#190952 = CARTESIAN_POINT ( 'NONE',  ( 3.176430186773027575, 0.9099569689122315452, 1.803159259486881938 ) ) ;
#190954 = CARTESIAN_POINT ( 'NONE',  ( 7.721398836998391246, -5.907420853759296264, 7.721398836998372595 ) ) ;
#190956 = CARTESIAN_POINT ( 'NONE',  ( 6.317736394288131052, 9.354147645769410602, 1.082531754730558626 ) ) ;
#190955 = CARTESIAN_POINT ( 'NONE',  ( 3.475000000000000533, -1.574999999999999956, 0.000000000000000000 ) ) ;
#190957 = CARTESIAN_POINT ( 'NONE',  ( -7.065734331377342414, 8.272386803808890576, -1.199719254218452047 ) ) ;
#190958 = CARTESIAN_POINT ( 'NONE',  ( 1.727750297885573882, 0.7672897036171549834, -1.865047645237365215 ) ) ;
#190960 = CARTESIAN_POINT ( 'NONE',  ( 5.583573808894983337, -0.9862700065477579825, 1.957137920222583372 ) ) ;
#190959 = CARTESIAN_POINT ( 'NONE',  ( -4.660252114795309097, 6.460046772059735432, -1.599625672291256295 ) ) ;
#190961 = CARTESIAN_POINT ( 'NONE',  ( 0.7499999999999902300, 5.597916667349482900, -1.299038105676658228 ) ) ;
#190962 = CARTESIAN_POINT ( 'NONE',  ( 5.836178160628028522, -1.067892152678026951, -1.586260290404594597 ) ) ;
#190963 = CARTESIAN_POINT ( 'NONE',  ( -3.358669367883384105, 4.941533567329135401, -1.599625672291262513 ) ) ;
#190964 = CARTESIAN_POINT ( 'NONE',  ( 6.453317929980448397, 6.631218461173066459, 1.040834085586084257E-14 ) ) ;
#190966 = CARTESIAN_POINT ( 'NONE',  ( 3.691029940746898053, 1.730877988113326493, 1.034147909374658392 ) ) ;
#190965 = CARTESIAN_POINT ( 'NONE',  ( -9.449669878600623463, 11.08733161553131197, -1.082531754730537976 ) ) ;
#190967 = CARTESIAN_POINT ( 'NONE',  ( 1.499999999999989120, 3.525000000000021227, 1.214306433183764966E-14 ) ) ;
#190968 = CARTESIAN_POINT ( 'NONE',  ( 1.364683531250000303, 13.56770833367473017, -0.7879004041258355073 ) ) ;
#190969 = CARTESIAN_POINT ( 'NONE',  ( 4.946200454639571475, 1.720373684868029329, 0.1241775145462056112 ) ) ;
#190970 = CARTESIAN_POINT ( 'NONE',  ( 5.040599249230596435, 9.102725900736217568, 0.7998128361456341429 ) ) ;
#190971 = CARTESIAN_POINT ( 'NONE',  ( 8.758204044747994743, 12.20135990463928266, 1.082531754730546636 ) ) ;
#190972 = CARTESIAN_POINT ( 'NONE',  ( -0.4516138619288456169, 3.070015318549070393, 0.4124855346667622435 ) ) ;
#190973 = CARTESIAN_POINT ( 'NONE',  ( 4.639837347815604751, 0.8015432297804045980, -1.690266223530467293 ) ) ;
#190974 = CYLINDRICAL_SURFACE ( 'NONE', #33453, 2.250000000000006661 ) ;
#190976 = AXIS2_PLACEMENT_3D ( 'NONE', #13948, #97376, #142949 ) ;
#190975 = CARTESIAN_POINT ( 'NONE',  ( 0.9189038144036645317, -1.502058968113138437, 1.424965263859011122 ) ) ;
#190977 = CARTESIAN_POINT ( 'NONE',  ( -1.420000000000055440, 7.176846818246208848, -4.202462424328208712 ) ) ;
#190978 = ORIENTED_EDGE ( 'NONE', *, *, #201026, .F. ) ;
#190980 = CARTESIAN_POINT ( 'NONE',  ( 3.230585741806197841, 6.991043475407723307, 0.7998128361456271485 ) ) ;
#190979 = CIRCLE ( 'NONE', #97634, 1.249999999999999778 ) ;
#190981 = CARTESIAN_POINT ( 'NONE',  ( 0.01720424586787797083, -1.842442205116225695, 0.8197940039925479816 ) ) ;
#190982 = CARTESIAN_POINT ( 'NONE',  ( 0.6151243592659773052, 1.481389731780102137, 1.042453732408530342 ) ) ;
#190983 = CARTESIAN_POINT ( 'NONE',  ( 4.543390873910894356, 8.314723429622471684, 0.7216878364870317197 ) ) ;
#190984 = CARTESIAN_POINT ( 'NONE',  ( 0.02041557226162492300, 2.519999999999982698, -2.000000000000004885 ) ) ;
#190985 = ORIENTED_EDGE ( 'NONE', *, *, #110539, .F. ) ;
#190986 = CARTESIAN_POINT ( 'NONE',  ( 9.422553571373278203, 11.05569592376608945, -1.082531754730543083 ) ) ;
#190988 = CARTESIAN_POINT ( 'NONE',  ( 6.414979237560321401, 10.63589287712906462, 1.040834085586084257E-14 ) ) ;
#190987 = CARTESIAN_POINT ( 'NONE',  ( 6.830517471914854255, -1.143533572366756124, 1.468690548319721900 ) ) ;
#190989 = CARTESIAN_POINT ( 'NONE',  ( 5.308173953863717820, 1.137349973717050267, -1.541276042019421810 ) ) ;
#190990 = CARTESIAN_POINT ( 'NONE',  ( -11.55950211276791251, 13.87999999999998302, 3.221476510067112109 ) ) ;
#190991 = CYLINDRICAL_SURFACE ( 'NONE', #17738, 6.200000000000000178 ) ;
#190992 = FACE_OUTER_BOUND ( 'NONE', #207143, .T. ) ;
#190994 = ORIENTED_EDGE ( 'NONE', *, *, #92149, .T. ) ;
#190993 = CARTESIAN_POINT ( 'NONE',  ( 4.690757960648224589, 6.495636925554817864, 1.443375672974062551 ) ) ;
#190995 = CARTESIAN_POINT ( 'NONE',  ( -7.782016984564068096, 10.10210578678999482, 1.443375672974090751 ) ) ;
#190996 = CARTESIAN_POINT ( 'NONE',  ( 3.081113354808207916, -0.1575343947536785305, -2.156009052512488200 ) ) ;
#190997 = CARTESIAN_POINT ( 'NONE',  ( -5.418418667316934112, 6.350518529071726981, -1.199719254218453823 ) ) ;
#190998 = CARTESIAN_POINT ( 'NONE',  ( 5.858531774880875176, 9.849054480754103835, -0.7216878364870458196 ) ) ;
#190999 = CARTESIAN_POINT ( 'NONE',  ( 0.07077104593807002908, 0.8175350930016941353, 1.956879683024402183 ) ) ;
#191000 = CARTESIAN_POINT ( 'NONE',  ( 4.295794115256676982, -0.6985059363485807138, 1.686860163339451768 ) ) ;
#191001 = CARTESIAN_POINT ( 'NONE',  ( 8.353377556026719830, 13.12787966248234994, -8.539254890958119404 ) ) ;
#191002 = CARTESIAN_POINT ( 'NONE',  ( 1.194530107633525517, -0.4747795734156860514, -1.913232634659914444 ) ) ;
#191003 = CARTESIAN_POINT ( 'NONE',  ( 3.726736447152957599, 1.348887845406310682, -1.355897031963343213 ) ) ;
#191004 = VERTEX_POINT ( 'NONE', #6710 ) ;
#191005 = CARTESIAN_POINT ( 'NONE',  ( 0.4499999999999800826, 4.000000000000008882, 0.8338124244295482823 ) ) ;
#191006 = CARTESIAN_POINT ( 'NONE',  ( 5.318794011649015552, -1.427836685786993742, 1.356881127696080158 ) ) ;
#191007 = EDGE_LOOP ( 'NONE', ( #118185, #171132, #172104, #89582 ) ) ;
#191008 = CARTESIAN_POINT ( 'NONE',  ( 6.163619218806376310, 1.002299704222510357, 1.663313343435903091 ) ) ;
#191009 = VERTEX_POINT ( 'NONE', #106422 ) ;
#191010 = CARTESIAN_POINT ( 'NONE',  ( -6.622231685632140596, 6.690634819517756959, 0.000000000000000000 ) ) ;
#191012 = CARTESIAN_POINT ( 'NONE',  ( 6.486587849989844834, -1.303813291173651301, 1.673118453357678392 ) ) ;
#191011 = CARTESIAN_POINT ( 'NONE',  ( -3.800028193580205382, 7.655393002477360653, -0.7998128361456481317 ) ) ;
#191014 = EDGE_CURVE ( 'NONE', #195805, #66068, #90135, .T. ) ;
#191013 = CARTESIAN_POINT ( 'NONE',  ( -11.92619526913699879, 10.19999999999998153, 1.328859060402684644 ) ) ;
#191016 = EDGE_LOOP ( 'NONE', ( #166039, #204835, #149604, #40872 ) ) ;
#191015 = CARTESIAN_POINT ( 'NONE',  ( 3.492734469894549942, -1.843672829398453228, -0.5074192597756199685 ) ) ;
#191017 = CARTESIAN_POINT ( 'NONE',  ( 0.1830476545506658226, -2.141193618969746471, -0.5335393285625378290 ) ) ;
#191018 = MECHANICAL_DESIGN_GEOMETRIC_PRESENTATION_REPRESENTATION (  '', ( #94122 ), #114879 ) ;
#191019 = CARTESIAN_POINT ( 'NONE',  ( 1.432836755002402101E-15, 0.7999999999999951594, -11.69999999999999041 ) ) ;
#191020 = CARTESIAN_POINT ( 'NONE',  ( 4.688143804000614701, 1.160868117455503556, 1.644480612105477579 ) ) ;
#191021 = LINE ( 'NONE', #207282, #117335 ) ;
#191023 = CARTESIAN_POINT ( 'NONE',  ( 5.559779856078610472, 1.205038519190555268, 1.616695979245158066 ) ) ;
#191022 = CARTESIAN_POINT ( 'NONE',  ( 6.428339884752386268, 1.046657586246093175, -1.495688092090130095 ) ) ;
#191024 = CARTESIAN_POINT ( 'NONE',  ( 6.727182134110196721, 2.084960209934753284, 2.120171393779949565 ) ) ;
#191025 = CARTESIAN_POINT ( 'NONE',  ( 1.961466609329724164, 1.720096886549182136, 1.151944459977225055 ) ) ;
#191026 = CARTESIAN_POINT ( 'NONE',  ( -7.009729113465285266, 8.136771039586342624, -1.199719254218446718 ) ) ;
#191027 = CARTESIAN_POINT ( 'NONE',  ( -6.087706144486034532, 7.033779493390481363, -0.9955609822858858537 ) ) ;
#191028 = CARTESIAN_POINT ( 'NONE',  ( 4.000000000000012434, 5.499999999999998224, -0.7500000000000006661 ) ) ;
#191029 = CARTESIAN_POINT ( 'NONE',  ( 6.596569749568344854, -0.5012203084251048990, -1.802199723311518786 ) ) ;
#191030 = CARTESIAN_POINT ( 'NONE',  ( 6.257251587906815793, 7.258880593101466161, 1.199719254218462483 ) ) ;
#191031 = CARTESIAN_POINT ( 'NONE',  ( -5.284980951228653190, 5.060232619388524533, 0.000000000000000000 ) ) ;
#191032 = CARTESIAN_POINT ( 'NONE',  ( 4.990809943606266508, 6.915973915664348937, -1.443375672974068769 ) ) ;
#191033 = CARTESIAN_POINT ( 'NONE',  ( -1.772826578343097204, 3.950000000000001954, 0.3999999999999941380 ) ) ;
#191034 = CARTESIAN_POINT ( 'NONE',  ( 0.6823417656249969321, 11.58854166700806765, -1.181850606188757036 ) ) ;
#191036 = CARTESIAN_POINT ( 'NONE',  ( -5.447343857640614573, 9.577261277214532242, -0.7998128361456362523 ) ) ;
#191035 = CARTESIAN_POINT ( 'NONE',  ( 6.925078400183553029, 7.053346220238264408, 2.353806654540433030 ) ) ;
#191037 = CARTESIAN_POINT ( 'NONE',  ( 4.658689525625823613, 1.003974855541647004, 1.413729434382102079 ) ) ;
#191038 = CIRCLE ( 'NONE', #97703, 0.08000000000000020983 ) ;
#191039 = CARTESIAN_POINT ( 'NONE',  ( -5.253948220495577637, 6.088359997788290734, 1.199719254218450271 ) ) ;
#191040 = STYLED_ITEM ( 'NONE', ( #9048 ), #133060 ) ;
#191041 = CARTESIAN_POINT ( 'NONE',  ( 2.676698048161993082, 1.355622082481915847, -1.564734663558226879 ) ) ;
#191042 = CARTESIAN_POINT ( 'NONE',  ( 3.954788147838703249, -1.976257328041197470, -0.7601183944087180899 ) ) ;
#191043 = CARTESIAN_POINT ( 'NONE',  ( 8.776205506747620788, 9.133327934160710981, -0.7998128361456221525 ) ) ;
#191044 = CARTESIAN_POINT ( 'NONE',  ( 0.08814328694727366353, -9.915773547069447247, 10.99964701288573465 ) ) ;
#191045 = CARTESIAN_POINT ( 'NONE',  ( 1.903111606826495938, -1.666530434877494304, 1.049136497343281738 ) ) ;
#191046 = CARTESIAN_POINT ( 'NONE',  ( 6.075519867480115188, 6.040327746143013599, 0.3625371965378897388 ) ) ;
#191048 = CARTESIAN_POINT ( 'NONE',  ( -0.4635785636673758758, -6.836568542495036205, -10.85353573482950829 ) ) ;
#191047 = CARTESIAN_POINT ( 'NONE',  ( 1.737500000000001155, -0.9333333333333346804, 3.009438278150922130 ) ) ;
#191049 = CARTESIAN_POINT ( 'NONE',  ( 3.978722188455630082, -0.2232912938500397904, -2.281366727860510313 ) ) ;
#191050 = CARTESIAN_POINT ( 'NONE',  ( 2.121465551170404140, -1.771062468586531047, 0.4427346646293239818 ) ) ;
#191051 = CARTESIAN_POINT ( 'NONE',  ( 4.518610335104485287, 8.493738834255713854, 0.000000000000000000 ) ) ;
#191052 = CARTESIAN_POINT ( 'NONE',  ( 5.572037945092146671, 8.484166121707415797, -1.082531754730543971 ) ) ;
#191053 = CARTESIAN_POINT ( 'NONE',  ( -7.344766530301162000, 9.591980256816594164, 1.599625672291295375 ) ) ;
#191054 = CARTESIAN_POINT ( 'NONE',  ( 3.129155277828885140, 1.821763076032786977, 0.8570700399232934474 ) ) ;
#191055 = CARTESIAN_POINT ( 'NONE',  ( 2.465611527742004760, -0.4346729355233553416, 1.912824223707191296 ) ) ;
#191056 = CARTESIAN_POINT ( 'NONE',  ( -9.169391961543940539, 9.592045464756413509, 1.040834085586084257E-14 ) ) ;
#191057 = CARTESIAN_POINT ( 'NONE',  ( -6.063521013809733518, 8.097193820909906137, 1.599625672291283607 ) ) ;
#191058 = CARTESIAN_POINT ( 'NONE',  ( 0.07516593201273635838, 0.7223771927552320449, -2.128525933252373381 ) ) ;
#191060 = CARTESIAN_POINT ( 'NONE',  ( 3.397073482672040345, 1.394525624090914961, 1.089649698571172776 ) ) ;
#191059 = CARTESIAN_POINT ( 'NONE',  ( 4.488279598995706721, -0.4578276946864130448, -2.039718000080573912 ) ) ;
#191061 = CARTESIAN_POINT ( 'NONE',  ( -6.671583288098617892, 15.00000000000324718, 9.747470831330359076 ) ) ;
#191062 = CARTESIAN_POINT ( 'NONE',  ( 6.193372188798685229, -0.7780443601670664622, 2.156323934359334338 ) ) ;
#191063 = CARTESIAN_POINT ( 'NONE',  ( 5.296709758707953242, 1.425846067417353868, 0.9975513609157842243 ) ) ;
#191064 = TOROIDAL_SURFACE ( 'NONE', #21588, 0.8299999999999999600, 0.08000000000000000167 ) ;
#191065 = CARTESIAN_POINT ( 'NONE',  ( 6.726816770674637347, 10.99970333242910669, -0.7998128361456291469 ) ) ;
#191066 = CARTESIAN_POINT ( 'NONE',  ( 5.889324137892314681, -0.8237033142024595689, -2.146187584169775953 ) ) ;
#191067 = CARTESIAN_POINT ( 'NONE',  ( 2.970157261343746136, 6.585292010301047938, 0.4235207732182846851 ) ) ;
#191068 = CARTESIAN_POINT ( 'NONE',  ( 5.518767629808705166, 1.731759826824400106, -0.08707812323833011292 ) ) ;
#191069 = CARTESIAN_POINT ( 'NONE',  ( 5.582552312218076018, 1.297699880476494094, -1.740541793301546347 ) ) ;
#191070 = DIRECTION ( 'NONE',  ( -3.491481338843133750E-15, -0.000000000000000000, -1.000000000000000000 ) ) ;
#191071 = CARTESIAN_POINT ( 'NONE',  ( -0.01227199510028028316, -0.5578357038005901103, 2.042509832261687475 ) ) ;
#191072 = CARTESIAN_POINT ( 'NONE',  ( 6.093750000000004441, -1.895863743164213355, -0.7852924748296624680 ) ) ;
#191073 = CARTESIAN_POINT ( 'NONE',  ( -3.602337597214539753E-15, 12.06250000000000178, 1.500000000000001554 ) ) ;
#191074 = CARTESIAN_POINT ( 'NONE',  ( 3.891558735110557610, 1.394649387769153259, 1.329109640543422399 ) ) ;
#191075 = CARTESIAN_POINT ( 'NONE',  ( 0.7500000000000006661, 11.86458333401613174, 1.299038105676657340 ) ) ;
#191076 = CARTESIAN_POINT ( 'NONE',  ( -0.02240927558793281635, -1.987202795932199839, -0.9927825048469391955 ) ) ;
#191077 = ORIENTED_EDGE ( 'NONE', *, *, #169747, .F. ) ;
#191078 = CARTESIAN_POINT ( 'NONE',  ( -1.500000000000011324, 4.920833333333354709, 0.8660254037844403729 ) ) ;
#191079 = CARTESIAN_POINT ( 'NONE',  ( 5.009901455449552010, 5.803638771901306725, -1.199719254218452047 ) ) ;
#191080 = CARTESIAN_POINT ( 'NONE',  ( 6.388916700537700777, 8.476822122092563916, 1.599625672291281386 ) ) ;
#191081 = CARTESIAN_POINT ( 'NONE',  ( 2.543850053281167423, -2.071606161961367043, 0.8020612402455605805 ) ) ;
#191082 = FILL_AREA_STYLE ('',( #208400 ) ) ;
#191083 = CARTESIAN_POINT ( 'NONE',  ( 6.155038550924144758, 8.203964280876741455, 1.443375672974076540 ) ) ;
#191084 = CARTESIAN_POINT ( 'NONE',  ( -9.666600336419303829, 11.34041714965307968, 1.082531754730558626 ) ) ;
#191085 = CARTESIAN_POINT ( 'NONE',  ( 6.536439455564155843, 8.719208346281938304, 1.443375672974065660 ) ) ;
#191086 = CARTESIAN_POINT ( 'NONE',  ( 0.3170300144729014669, 1.034162889623980286, -1.730867746391979933 ) ) ;
#191088 = CARTESIAN_POINT ( 'NONE',  ( 5.564908101581790945, 1.564332607353050131, -1.344557729249852729 ) ) ;
#191087 = CARTESIAN_POINT ( 'NONE',  ( 8.483651433849084711, 10.92067931095586886, 1.599625672291281386 ) ) ;
#191089 = CARTESIAN_POINT ( 'NONE',  ( -11.00029612940780410, -6.479296433800279864, -0.04006801626462446614 ) ) ;
#191090 = CARTESIAN_POINT ( 'NONE',  ( 6.441532379824158383, 9.568852638886589546, -1.082531754730548412 ) ) ;
#191091 = CARTESIAN_POINT ( 'NONE',  ( -2.480760062148275491, 4.021557182957056220, 11.67105848277438795 ) ) ;
#191092 = CARTESIAN_POINT ( 'NONE',  ( -1.364683531250012516, 1.030208333674754062, 0.7879004041258379498 ) ) ;
#191093 = CARTESIAN_POINT ( 'NONE',  ( 1.106321208856683613, 1.344927736385517658, -1.150416400790694960 ) ) ;
#191094 = CARTESIAN_POINT ( 'NONE',  ( -0.05211191391743182078, -1.802403943428915412, -0.9041556775107384425 ) ) ;
#191095 = CARTESIAN_POINT ( 'NONE',  ( 5.759256982813394821, 1.713166593665109705, -0.3060214249656545982 ) ) ;
#191096 = B_SPLINE_CURVE_WITH_KNOTS ( 'NONE', 3,
 ( #42740, #108845, #144526, #77341, #193225, #209451 ),
 .UNSPECIFIED., .F., .F.,
 ( 4, 2, 4 ),
 ( 0.001877801214402442754, 0.002190719108449961511, 0.002503637002497480051 ),
 .UNSPECIFIED. ) ;
#191097 = CARTESIAN_POINT ( 'NONE',  ( 3.667766089696015364, 1.274287168460963127, 1.905377313346041435 ) ) ;
#191098 = CARTESIAN_POINT ( 'NONE',  ( 1.364683531249986537, -0.5947916663252456049, -0.7879004041258309554 ) ) ;
#191099 = CARTESIAN_POINT ( 'NONE',  ( 1.798526679444776954, 1.530131497970032450, 1.023642133485637595 ) ) ;
#191100 = CARTESIAN_POINT ( 'NONE',  ( 8.062294901620731480, 12.55776115186623620, 1.040834085586084257E-14 ) ) ;
#191101 = CARTESIAN_POINT ( 'NONE',  ( 12.00094528747601430, 6.998582067892187730, -0.9367503912666700350 ) ) ;
#191102 = CARTESIAN_POINT ( 'NONE',  ( 3.522295995157864290, 1.158834602800838498, -1.410599190884161969 ) ) ;
#191103 = CARTESIAN_POINT ( 'NONE',  ( 4.184220324914634581, 1.621181886760931778, 1.198861198883696799 ) ) ;
#191104 = CARTESIAN_POINT ( 'NONE',  ( -7.818248136574758256, 12.27303992597924420, 0.000000000000000000 ) ) ;
#191106 = DIRECTION ( 'NONE',  ( 0.000000000000000000, 0.000000000000000000, 1.000000000000000000 ) ) ;
#191105 = CARTESIAN_POINT ( 'NONE',  ( 2.606633135955916725, -0.8653751708443763180, -2.090666874703292599 ) ) ;
#191107 = CARTESIAN_POINT ( 'NONE',  ( 5.122148429244435697, -1.124054950784241891, -1.780691527792167994 ) ) ;
#191108 = CARTESIAN_POINT ( 'NONE',  ( 9.165183341830644537, 14.44137815449902895, 8.758053443030863860 ) ) ;
#191109 =( BOUNDED_CURVE ( )  B_SPLINE_CURVE ( 3, ( #77020, #44555, #74907, #57591 ),
 .UNSPECIFIED., .F., .T. ) 
 B_SPLINE_CURVE_WITH_KNOTS ( ( 4, 4 ),
 ( 4.576839133004758864, 4.599536981099443977 ),
 .UNSPECIFIED. ) 
 CURVE ( )  GEOMETRIC_REPRESENTATION_ITEM ( )  RATIONAL_B_SPLINE_CURVE ( ( 1.000000000000000000, 0.9999570677684579412, 0.9999570677684579412, 1.000000000000000000 ) ) 
 REPRESENTATION_ITEM ( '' )  );
#191110 = CARTESIAN_POINT ( 'NONE',  ( 2.523957353938070192, 2.030885678308389952, -0.4015143504868187718 ) ) ;
#191111 = CARTESIAN_POINT ( 'NONE',  ( 4.864678189204997949, 4.569879397027603929, 0.7998128361456341429 ) ) ;
#191112 = CARTESIAN_POINT ( 'NONE',  ( -1.360316468750038643, 0.4427083336747321130, 0.7853790794158701516 ) ) ;
#191113 = CARTESIAN_POINT ( 'NONE',  ( 5.039744756118590630, -2.013340025477545758, 0.6656774797743277849 ) ) ;
#191114 = ITEM_DEFINED_TRANSFORMATION ( 'NONE', 'NONE', #90213,  #200407 ) ;
#191115 = CARTESIAN_POINT ( 'NONE',  ( 0.4867822013649549251, -0.2347038428511475372, -1.912094274373641323 ) ) ;
#191116 = CARTESIAN_POINT ( 'NONE',  ( -3.657667580636712934, 7.489305620709952649, -0.7998128361456481317 ) ) ;
#191117 = CARTESIAN_POINT ( 'NONE',  ( 9.423080456697809026, 10.95234760669099749, -1.199719254218446718 ) ) ;
#191118 = CARTESIAN_POINT ( 'NONE',  ( 6.007671464186834065, 7.141943142040370063, 1.082531754730549967 ) ) ;
#191119 = CARTESIAN_POINT ( 'NONE',  ( 0.4774187120914303861, 2.800000000000023803, -1.397118404531580316 ) ) ;
#191120 = CARTESIAN_POINT ( 'NONE',  ( -5.904739593951539689, 6.847616600153594746, 1.199719254218450271 ) ) ;
#191121 = CARTESIAN_POINT ( 'NONE',  ( 6.099870585610251084, 1.463495690422533579, 1.534846084132005961 ) ) ;
#191122 = CARTESIAN_POINT ( 'NONE',  ( 1.764816150188710298, -1.489710805432680418, 1.488830988054674620 ) ) ;
#191123 = CARTESIAN_POINT ( 'NONE',  ( -5.306037014901836990, 7.283738832175834510, 1.599625672291263179 ) ) ;
#191124 = CARTESIAN_POINT ( 'NONE',  ( 8.437251666405968464, 8.737881787095446384, 1.040834085586084257E-14 ) ) ;
#191125 = CARTESIAN_POINT ( 'NONE',  ( 6.631710597105570315, 1.780986809720253694, -0.5397248755362458184 ) ) ;
#191126 = CARTESIAN_POINT ( 'NONE',  ( 7.100719765255169236, 9.307259030929609267, -1.599625672291262513 ) ) ;
#191127 = CARTESIAN_POINT ( 'NONE',  ( 11.94105721237523277, 10.19999999999999929, 1.187919463087245386 ) ) ;
#191128 = CARTESIAN_POINT ( 'NONE',  ( -3.471769853551161411, 6.208092708188416076, 1.199719254218452935 ) ) ;
#191129 = CARTESIAN_POINT ( 'NONE',  ( -7.524412065904404479, 11.72230514362308185, 0.000000000000000000 ) ) ;
#191130 = VECTOR ( 'NONE', #172856, 1000.000000000000000 ) ;
#191131 = CARTESIAN_POINT ( 'NONE',  ( 0.1938080739139167730, 1.976361990896974508, -0.7691651810952588875 ) ) ;
#191132 = PRESENTATION_STYLE_ASSIGNMENT (( #193283 ) ) ;
#191134 = CARTESIAN_POINT ( 'NONE',  ( 3.490630252122446375, 1.913478943654752129, 0.4322817992908413176 ) ) ;
#191133 = CARTESIAN_POINT ( 'NONE',  ( -1.225000000000048050, -0.2291666666666410390, 0.7072540797572577365 ) ) ;
#191135 = CARTESIAN_POINT ( 'NONE',  ( 0.9015118058452382677, 1.767791302423503685, 1.243857928393626633 ) ) ;
#191136 = CIRCLE ( 'NONE', #939, 11.09999999999999964 ) ;
#191138 = CARTESIAN_POINT ( 'NONE',  ( -5.710256234166866562, 6.271970132040741497, 1.104226958479601173 ) ) ;
#191137 = CARTESIAN_POINT ( 'NONE',  ( -4.878955176071358757, 6.785476686873604280, -1.599625672291271394 ) ) ;
#191139 = CARTESIAN_POINT ( 'NONE',  ( -1.364683531250014514, 1.488541667008084435, -0.7879004041258289570 ) ) ;
#191140 = CARTESIAN_POINT ( 'NONE',  ( 2.800428594868603405, 1.470281860783069439, 0.9307988129052218174 ) ) ;
#191141 = CARTESIAN_POINT ( 'NONE',  ( 5.666945020832167224, 8.594891043404107478, 1.082531754730558626 ) ) ;
#191142 = CARTESIAN_POINT ( 'NONE',  ( -10.93377262805118555, 5.994763374826558966, -6.297255446303106297 ) ) ;
#191143 = EDGE_CURVE ( 'NONE', #113279, #207870, #81433, .T. ) ;
#191144 = CARTESIAN_POINT ( 'NONE',  ( 2.196638537759632470, -1.314794530490107638, -1.528507974810841219 ) ) ;
#191145 = CARTESIAN_POINT ( 'NONE',  ( -3.094265954482870118, 2.800000000000024691, 2.490342512183699508 ) ) ;
#191146 = CARTESIAN_POINT ( 'NONE',  ( -5.984998465789844069, 5.947196063035064206, 0.7998128361456281477 ) ) ;
#191147 = CARTESIAN_POINT ( 'NONE',  ( 2.659003877371171942, -1.714407010456520108, -0.9732827283935908680 ) ) ;
#191149 = CARTESIAN_POINT ( 'NONE',  ( -4.828112100242283766, 7.686528979374367410, -1.082531754730549967 ) ) ;
#191148 = CARTESIAN_POINT ( 'NONE',  ( 5.853752780977106163, -1.389761788226477002, -1.313969904969368496 ) ) ;
#191150 = B_SPLINE_CURVE_WITH_KNOTS ( 'NONE', 3,
 ( #139583, #122340, #73483, #189371, #188297, #4191, #70261, #205610 ),
 .UNSPECIFIED., .F., .F.,
 ( 4, 2, 2, 4 ),
 ( 0.000000000000000000, 0.0001912162707998985305, 0.0003824325415997970610, 0.0007648650831995943387 ),
 .UNSPECIFIED. ) ;
#191151 = CARTESIAN_POINT ( 'NONE',  ( -4.787437638956920871, 8.599444655509458357, -0.7216878364870338292 ) ) ;
#191152 = CARTESIAN_POINT ( 'NONE',  ( 5.550083779947807550, 7.568460058062819407, -1.599625672291283607 ) ) ;
#191153 = ADVANCED_FACE ( 'NONE', ( #14167 ), #80150, .T. ) ;
#191154 = CARTESIAN_POINT ( 'NONE',  ( -5.387385936583832802, 7.378645907471495846, -1.599625672291271394 ) ) ;
#191155 = CARTESIAN_POINT ( 'NONE',  ( 1.664719335976164283, 0.6358223015159381042, 1.917034779120100341 ) ) ;
#191156 = CARTESIAN_POINT ( 'NONE',  ( -15.75000000000000000, 13.79999999999999893, 0.6999999999999992895 ) ) ;
#191157 = CARTESIAN_POINT ( 'NONE',  ( 5.983493387795983054, 2.135156284703492169, -0.8757408730279289122 ) ) ;
#191158 = CARTESIAN_POINT ( 'NONE',  ( 6.514115657861259123, 1.956686900881845714, -0.1430618042221123987 ) ) ;
#191159 = CARTESIAN_POINT ( 'NONE',  ( 2.887496479553632422, -1.832211488775811414, 0.7015765724691159777 ) ) ;
#191160 = CARTESIAN_POINT ( 'NONE',  ( 9.582915646760733708, 10.07448976417602893, 0.7998128361456462443 ) ) ;
#191161 = CARTESIAN_POINT ( 'NONE',  ( 0.2994542103806375755, 1.388483683912977495, -1.462447666687356485 ) ) ;
#191162 = ORIENTED_EDGE ( 'NONE', *, *, #22105, .T. ) ;
#191163 = CARTESIAN_POINT ( 'NONE',  ( 0.8138397394129359697, -1.348031465540124207, -1.632742428372506049 ) ) ;
#191165 = CARTESIAN_POINT ( 'NONE',  ( -8.016948904382338981, 8.247528564734524892, -0.7998128361456291469 ) ) ;
#191164 = CARTESIAN_POINT ( 'NONE',  ( -2.788173145904702555, 6.404619103530779789, -0.7998128361456281477 ) ) ;
#191166 = CARTESIAN_POINT ( 'NONE',  ( 1.710644026344819046, -0.2265308078298749472, 1.827073587482845207 ) ) ;
#191167 = EDGE_LOOP ( 'NONE', ( #205402, #198446, #62938, #661 ) ) ;
#191168 = CARTESIAN_POINT ( 'NONE',  ( 9.397486876216097684, 13.53113053364065443, 7.462549781540802840 ) ) ;
#191169 = CARTESIAN_POINT ( 'NONE',  ( 2.953504815971871977, -1.868289524550557523, 1.003269902519101864 ) ) ;
#191170 = CARTESIAN_POINT ( 'NONE',  ( 1.499999999999989120, 4.035416667349482012, 0.8660254037844524744 ) ) ;
#191171 = CARTESIAN_POINT ( 'NONE',  ( 6.726816770674637347, 10.99970333242910669, -0.7998128361456291469 ) ) ;
#191172 = CARTESIAN_POINT ( 'NONE',  ( 6.230854113932139171, 9.427024345299638952, 1.199719254218452047 ) ) ;
#191173 = CARTESIAN_POINT ( 'NONE',  ( 3.796211532432732572, -2.058264701994051649, -0.1047273801592675524 ) ) ;
#191175 = CARTESIAN_POINT ( 'NONE',  ( 0.9426144736941791669, -1.451487892885485742, -1.132780452900377099 ) ) ;
#191174 = CARTESIAN_POINT ( 'NONE',  ( -8.389798128758148010, 8.682519326506312751, 0.7998128361456462443 ) ) ;
#191176 = CARTESIAN_POINT ( 'NONE',  ( -0.6823417656249969321, 4.217708333674755394, -1.181850606188749264 ) ) ;
#191177 = CARTESIAN_POINT ( 'NONE',  ( -1.458253848507225392, 8.740113170334302239, 2.549233421402196331 ) ) ;
#191178 = CARTESIAN_POINT ( 'NONE',  ( -0.1007326007325826528, -9.920000000000095852, -10.99953876047305812 ) ) ;
#191179 = CARTESIAN_POINT ( 'NONE',  ( 1.243116305521356990, 0.4334984505205765060, 2.163720904216937857 ) ) ;
#191180 = CARTESIAN_POINT ( 'NONE',  ( 3.058202344463755828, 2.251794067479270911, -0.2186341555679652271 ) ) ;
#191181 = CARTESIAN_POINT ( 'NONE',  ( -8.839552966430012759, 10.37552855133225904, -1.082531754730543971 ) ) ;
#191183 = EDGE_CURVE ( 'NONE', #26370, #186457, #133415, .T. ) ;
#191182 = CARTESIAN_POINT ( 'NONE',  ( 2.531291980686082521, -0.1736719688998221156, 1.803202784768900502 ) ) ;
#191184 = CARTESIAN_POINT ( 'NONE',  ( 3.467908617337426502, -0.9394263201649171169, 1.669454279737823343 ) ) ;
#191185 = CARTESIAN_POINT ( 'NONE',  ( 4.475093801846619535, 1.891600172242546840, 0.8420093967692193759 ) ) ;
#191186 = CARTESIAN_POINT ( 'NONE',  ( 1.364683531249990311, 3.446875000341416584, 1.214306433183764966E-14 ) ) ;
#191187 = CARTESIAN_POINT ( 'NONE',  ( 2.254701366666445939, -1.525215070022269082, 1.249173565255176976 ) ) ;
#191188 = CARTESIAN_POINT ( 'NONE',  ( 0.07700591528353968596, 0.003617085621422307627, -1.910863332519038282 ) ) ;
#191189 = CARTESIAN_POINT ( 'NONE',  ( 3.713615009860570915, -1.843089489661839053, 0.3189824552965599969 ) ) ;
#191191 = CARTESIAN_POINT ( 'NONE',  ( 4.780342502845265074, 8.269896785439653897, -0.8296954209953393278 ) ) ;
#191190 = CARTESIAN_POINT ( 'NONE',  ( 1.788135723919834774, 1.593634496655076171, 1.669289477041531633 ) ) ;
#191192 = CARTESIAN_POINT ( 'NONE',  ( 3.420197418661593769, 0.8345380353566893561, 1.663503485505882118 ) ) ;
#191193 = CARTESIAN_POINT ( 'NONE',  ( 0.6823417656249917140, 4.592708333674755394, 1.181850606188765695 ) ) ;
#191195 = CARTESIAN_POINT ( 'NONE',  ( -4.599240423533815125, 6.388866465587984322, 1.599625672291267398 ) ) ;
#191194 = TOROIDAL_SURFACE ( 'NONE', #66553, 11.92000000000000171, 0.08000000000000000167 ) ;
#191196 = CARTESIAN_POINT ( 'NONE',  ( 6.636879889089462026, 7.701780277814560982, -1.199719254218446718 ) ) ;
#191197 = CARTESIAN_POINT ( 'NONE',  ( 11.21553972792699128, 3.696394713403117649, -3.679259263401860380 ) ) ;
#191198 = CARTESIAN_POINT ( 'NONE',  ( 1.155059408868217119, -1.659095468083382041, 1.297160957089478206 ) ) ;
#191199 = EDGE_CURVE ( 'NONE', #73222, #83914, #57907, .T. ) ;
#191201 = DIRECTION ( 'NONE',  ( 0.000000000000000000, 0.000000000000000000, 1.000000000000000000 ) ) ;
#191200 = CARTESIAN_POINT ( 'NONE',  ( 0.6823417656249899377, 4.238541667008085767, -1.181850606188754593 ) ) ;
#191202 = CARTESIAN_POINT ( 'NONE',  ( 6.643834073375672666, 0.8340821395082242962, -1.994398315854857495 ) ) ;
#191203 = CARTESIAN_POINT ( 'NONE',  ( 2.654661980655496301, 2.105093816413053709, 0.2552270188876659129 ) ) ;
#191204 = CARTESIAN_POINT ( 'NONE',  ( -0.1755239516839811886, -0.8679694584908944632, -1.822324207963136988 ) ) ;
#191205 = CARTESIAN_POINT ( 'NONE',  ( -1.364683531250000748, 0.009375000341420303140, 0.000000000000000000 ) ) ;
#191206 = CARTESIAN_POINT ( 'NONE',  ( -3.633221978782290140, 6.222214161012547429, -1.082531754730549967 ) ) ;
#191207 = EDGE_CURVE ( 'NONE', #212524, #96867, #19098, .T. ) ;
#191208 = CARTESIAN_POINT ( 'NONE',  ( 0.8608787451157871029, -1.566265403972837866, 1.489986575276234460 ) ) ;
#191209 = VECTOR ( 'NONE', #65067, 1000.000000000000000 ) ;
#191212 = CARTESIAN_POINT ( 'NONE',  ( 4.365362273920252889, 4.195270195769483124, 0.7216878364870317197 ) ) ;
#191211 = CARTESIAN_POINT ( 'NONE',  ( -3.285556943750000070, -0.8093749995220431703, 0.000000000000000000 ) ) ;
#191210 = CARTESIAN_POINT ( 'NONE',  ( 6.282224075085741433, 8.422623735723785643, 1.599625672291268286 ) ) ;
#191213 = CARTESIAN_POINT ( 'NONE',  ( -4.679499295372141709, 5.488445928469455559, 1.199719254218452935 ) ) ;
#191214 = CARTESIAN_POINT ( 'NONE',  ( 4.628138809701114020, 2.011451458044950069, 0.1435230606586651581 ) ) ;
#191216 = CARTESIAN_POINT ( 'NONE',  ( -7.241463443030476732, 7.620997903056574430, 0.000000000000000000 ) ) ;
#191215 = CARTESIAN_POINT ( 'NONE',  ( -8.676855123066012254, 12.10645282934361866, -1.082531754730543971 ) ) ;
#191218 = CARTESIAN_POINT ( 'NONE',  ( -1.364683531250000748, 10.35937500034139802, 0.000000000000000000 ) ) ;
#191217 = CARTESIAN_POINT ( 'NONE',  ( 6.368072262247213899, 1.106822706796772193, 1.856716078747308263 ) ) ;
#191219 = CARTESIAN_POINT ( 'NONE',  ( -9.972185678051314284, 11.59297036493672017, 1.199719254218462483 ) ) ;
#191221 = CARTESIAN_POINT ( 'NONE',  ( 0.2455189486357247652, 1.894654674652377135, -0.2817335493821241932 ) ) ;
#191220 = CARTESIAN_POINT ( 'NONE',  ( -5.788968402910818156, 7.776882441527838807, 1.443375672974064550 ) ) ;
#191222 = CARTESIAN_POINT ( 'NONE',  ( -1.201851678989727383E-14, 1.134375000341418582, 1.575800808251672791 ) ) ;
#191223 = CARTESIAN_POINT ( 'NONE',  ( 6.883263157960364254, 2.038911835798001171, 2.358809022084580764 ) ) ;
#191224 = AXIS2_PLACEMENT_3D ( 'NONE', #78348, #113064, #112001 ) ;
#191225 = CARTESIAN_POINT ( 'NONE',  ( -2.324088772396477673E-16, -1.837499999999999245, -3.475000000000000089 ) ) ;
#191226 = CARTESIAN_POINT ( 'NONE',  ( 3.176078081051143531, -1.026819631599368066, 1.385778701376034316 ) ) ;
#191227 = CARTESIAN_POINT ( 'NONE',  ( 4.248501033035879004, 6.049946853332221153, -1.599625672291273171 ) ) ;
#191228 = CARTESIAN_POINT ( 'NONE',  ( 5.692444392891300886, 7.734547439830227411, -1.599625672291281386 ) ) ;
#191229 = CARTESIAN_POINT ( 'NONE',  ( 1.364683531249986537, -0.03229166632525094088, -0.7879004041258309554 ) ) ;
#191230 = CARTESIAN_POINT ( 'NONE',  ( 1.387592303909779279, -0.8018289002829273038, 1.577768680615166952 ) ) ;
#191231 = CARTESIAN_POINT ( 'NONE',  ( 1.928386798537110147, -0.9510432213125822321, -1.774292727131807856 ) ) ;
#191232 = SURFACE_STYLE_FILL_AREA ( #40750 ) ;
#191233 = CARTESIAN_POINT ( 'NONE',  ( 4.208205882762393379, -2.201082536721191474, 0.1591639695062776749 ) ) ;
#191234 = ORIENTED_EDGE ( 'NONE', *, *, #129593, .F. ) ;
#191235 = CARTESIAN_POINT ( 'NONE',  ( -0.7500000000000006661, -0.8916666666666448471, -1.299038105676652011 ) ) ;
#191236 = CARTESIAN_POINT ( 'NONE',  ( 6.900736999231407154, 10.99468423250458038, -0.7216878364870267237 ) ) ;
#191238 = CARTESIAN_POINT ( 'NONE',  ( 3.444935562074178392, -1.779636981393231565, -0.9480232565319337557 ) ) ;
#191237 = CARTESIAN_POINT ( 'NONE',  ( 3.668700845920089826, 0.7647225481513253431, 1.977962425194310203 ) ) ;
#191240 = ORIENTED_EDGE ( 'NONE', *, *, #200733, .T. ) ;
#191239 = CARTESIAN_POINT ( 'NONE',  ( 3.884856352912366972, -1.692463592844297704, -0.6465920371584426007 ) ) ;
#191241 = CARTESIAN_POINT ( 'NONE',  ( 4.386945222473598527, 7.275797305264619652, -1.199719254218452047 ) ) ;
#191242 = ORIENTED_EDGE ( 'NONE', *, *, #79408, .F. ) ;
#191243 = CARTESIAN_POINT ( 'NONE',  ( 0.1099206271272800961, -0.7955684105149689600, -1.691499381818922343 ) ) ;
#191244 = CARTESIAN_POINT ( 'NONE',  ( 6.358013415952256331, 1.820405254634300363, -0.1396899356524081148 ) ) ;
#191246 = CARTESIAN_POINT ( 'NONE',  ( 2.747180457951060362, 0.2762254639866565942, -1.895546175561702018 ) ) ;
#191245 = CARTESIAN_POINT ( 'NONE',  ( -2.279742385392243165, 5.811449882932888222, -0.7998128361456281477 ) ) ;
#191247 = SURFACE_STYLE_FILL_AREA ( #125287 ) ;
#191248 = CARTESIAN_POINT ( 'NONE',  ( -1.201851678989727383E-14, 1.884375000341422135, 1.575800808251672791 ) ) ;
#191249 = CARTESIAN_POINT ( 'NONE',  ( -1.777638883463123598, -0.9165151389911724289, 1.199999999999999734 ) ) ;
#191250 = CARTESIAN_POINT ( 'NONE',  ( 5.234856708652215751, 9.121433570154021453, 0.7216878364870317197 ) ) ;
#191251 = CARTESIAN_POINT ( 'NONE',  ( -6.319508997745553636, 6.545384383557486530, 0.7216878364870257245 ) ) ;
#191252 = CARTESIAN_POINT ( 'NONE',  ( -6.343235766347277149, 8.493804042195527870, -1.599625672291271394 ) ) ;
#191253 = CARTESIAN_POINT ( 'NONE',  ( 2.654661980655496301, 2.105093816413053709, 0.2552270188876659129 ) ) ;
#191255 = CARTESIAN_POINT ( 'NONE',  ( -10.87640920097716091, 5.776148811624420176, 6.414305308649663750 ) ) ;
#191254 = CARTESIAN_POINT ( 'NONE',  ( -0.02988540731097348233, 2.061246921799511966, -2.144091820287073791 ) ) ;
#191256 = CARTESIAN_POINT ( 'NONE',  ( 4.253168938266341570, -1.637241709590877781, -1.097755751903241483 ) ) ;
#191257 = CARTESIAN_POINT ( 'NONE',  ( 6.363533315466952445, -1.540175188624912650, -1.133462061071670579 ) ) ;
#191258 = ORIENTED_EDGE ( 'NONE', *, *, #48534, .T. ) ;
#191259 = CARTESIAN_POINT ( 'NONE',  ( 6.245324861096241520, 0.3598972253578552327, -2.086368836056912368 ) ) ;
#191260 = CARTESIAN_POINT ( 'NONE',  ( 9.020730412796739373, 12.35293633087048271, 7.916875519941681816 ) ) ;
#191261 = CARTESIAN_POINT ( 'NONE',  ( 1.592325325408463055, 1.022198633559557646, -1.800363622228560168 ) ) ;
#191262 = CARTESIAN_POINT ( 'NONE',  ( 3.029168698193057008, -1.304570280419844686, -1.438651077900707120 ) ) ;
#191263 = CARTESIAN_POINT ( 'NONE',  ( 6.229045230835819069, 6.231917288922055320, -0.7998128361456481317 ) ) ;
#191264 = CARTESIAN_POINT ( 'NONE',  ( 6.038177310039780643, 8.137902509836795417, -1.599625672291283607 ) ) ;
#191266 = CARTESIAN_POINT ( 'NONE',  ( 5.309989718046547402, 9.346738437696316737, 0.7998128361456462443 ) ) ;
#191265 = CARTESIAN_POINT ( 'NONE',  ( 3.644548676374514518, -1.708972400646594503, 1.203939368798632836 ) ) ;
#191268 = ADVANCED_FACE ( 'NONE', ( #125906 ), #153538, .F. ) ;
#191267 = CARTESIAN_POINT ( 'NONE',  ( 3.079110283634975964, 6.606396074300548982, 0.7216878364870257245 ) ) ;
#191270 = ORIENTED_EDGE ( 'NONE', *, *, #34539, .F. ) ;
#191269 = CARTESIAN_POINT ( 'NONE',  ( 0.8381711186948238579, 1.079942214367535680, -1.454201162973115524 ) ) ;
#191271 = CARTESIAN_POINT ( 'NONE',  ( 5.813141826352885566, 1.944573597739504889, 1.043518232037063287 ) ) ;
#191272 = CYLINDRICAL_SURFACE ( 'NONE', #26709, 1.250000000000000000 ) ;
#191273 = CARTESIAN_POINT ( 'NONE',  ( 3.012930935654754450, 1.599341701681813666, -1.520756135150652222 ) ) ;
#191274 = CARTESIAN_POINT ( 'NONE',  ( 6.774270308322468459, 11.05506579301824743, 0.7998128361456462443 ) ) ;
#191275 = CARTESIAN_POINT ( 'NONE',  ( 2.824755571612533434, 1.383597569638248315, -1.320258682893655999 ) ) ;
#191276 = CIRCLE ( 'NONE', #90969, 11.09999999999999964 ) ;
#191277 = CARTESIAN_POINT ( 'NONE',  ( 8.561083932025322696, 12.07534945641652158, -1.199719254218446718 ) ) ;
#191278 = CARTESIAN_POINT ( 'NONE',  ( 5.547352688424546763, 1.827615396715172258, -0.9727077141251788683 ) ) ;
#191279 = AXIS2_PLACEMENT_3D ( 'NONE', #666, #118783, #67800 ) ;
#191281 = CARTESIAN_POINT ( 'NONE',  ( 2.852577672069932735, 0.7271573612388192442, 2.035869728763760378 ) ) ;
#191280 = CARTESIAN_POINT ( 'NONE',  ( 9.578206935409037115, -9.746166700193986898, -0.1671882239534273895 ) ) ;
#191282 = CARTESIAN_POINT ( 'NONE',  ( 4.282901435897610298, 1.957309562236182021, -0.9860176978964061423 ) ) ;
#191283 = ORIENTED_EDGE ( 'NONE', *, *, #47045, .T. ) ;
#191284 = ORIENTED_EDGE ( 'NONE', *, *, #212227, .F. ) ;
#191285 = CARTESIAN_POINT ( 'NONE',  ( 10.18233705906309972, 11.83814697611718714, 1.199719254218450271 ) ) ;
#191286 = CARTESIAN_POINT ( 'NONE',  ( -2.324088772396477673E-16, -1.837499999999999245, -3.475000000000000089 ) ) ;
#191287 = CARTESIAN_POINT ( 'NONE',  ( 9.499606459999014874, -9.910930816046773728, -0.08647025586254107610 ) ) ;
#191288 = CARTESIAN_POINT ( 'NONE',  ( 3.874598038455354665, 7.742391154831717692, -0.7998128361456362523 ) ) ;
#191289 = CARTESIAN_POINT ( 'NONE',  ( 1.528150327639969719, -3.232243495192087757, 2.908546201585544999 ) ) ;
#191290 = EDGE_CURVE ( 'NONE', #184155, #93276, #137295, .T. ) ;
#191291 = CARTESIAN_POINT ( 'NONE',  ( -0.2104748580754166598, -0.006608320950483163522, -2.103482951484026753 ) ) ;
#191292 = CARTESIAN_POINT ( 'NONE',  ( -9.219181267612684749, 10.81842823604534765, 1.082531754730558626 ) ) ;
#191293 = CARTESIAN_POINT ( 'NONE',  ( 4.050854035433010480, 7.948023151305657841, 0.000000000000000000 ) ) ;
#191294 = CARTESIAN_POINT ( 'NONE',  ( 5.875854205266583641, -2.021069926245163906, 0.4479438709683660202 ) ) ;
#191295 = CARTESIAN_POINT ( 'NONE',  ( 4.547439623722833169, -1.490282656903282099, -1.220848939070565686 ) ) ;
#191296 = CARTESIAN_POINT ( 'NONE',  ( 6.398082464950202386, -0.9982666083749867081, -1.867140504451180183 ) ) ;
#191297 = CARTESIAN_POINT ( 'NONE',  ( 7.343676480457483002, 8.596652644402405841, -1.199719254218452047 ) ) ;
#191298 = CARTESIAN_POINT ( 'NONE',  ( 5.411747445213322294, 6.143583536729159356, -0.9474050467834894684 ) ) ;
#191299 = CARTESIAN_POINT ( 'NONE',  ( 5.647300209178060193, 1.738727086691471024, -0.9248740175569410971 ) ) ;
#191300 = CARTESIAN_POINT ( 'NONE',  ( 0.1819133275808570704, -1.029140439971199417, 1.934768540691175431 ) ) ;
#191301 = CARTESIAN_POINT ( 'NONE',  ( 5.356004772612798170, 1.823420152956479523, -0.09349780940721277855 ) ) ;
#191302 = CARTESIAN_POINT ( 'NONE',  ( 6.875393295905841917, 7.193916064744513506, 0.000000000000000000 ) ) ;
#191303 = CARTESIAN_POINT ( 'NONE',  ( 3.836594282542914236, 5.499112634431936542, 1.443375672974062551 ) ) ;
#191304 = CARTESIAN_POINT ( 'NONE',  ( -6.306477729012051725, 7.386587434382707151, 1.199719254218452047 ) ) ;
#191305 = CARTESIAN_POINT ( 'NONE',  ( 5.551137550152489553, 5.441024994791534120, 0.7998128361456352531 ) ) ;
#191306 = ORIENTED_EDGE ( 'NONE', *, *, #92980, .T. ) ;
#191308 = CARTESIAN_POINT ( 'NONE',  ( 6.064703285670603350, 0.6354670234634349768, 1.910320939954947228 ) ) ;
#191307 = CARTESIAN_POINT ( 'NONE',  ( 2.296224312773272658, 1.477747569344042278, -1.098160524033331642 ) ) ;
#191309 = CARTESIAN_POINT ( 'NONE',  ( 1.318156941596902998, -1.811358654967555104, 1.414711894558273730 ) ) ;
#191310 = CARTESIAN_POINT ( 'NONE',  ( 5.840667439708360220, -1.913134005453724251, -0.4332900713753874977 ) ) ;
#191311 = CARTESIAN_POINT ( 'NONE',  ( -5.961834861707238531, 7.978559976790334574, -1.599625672291263179 ) ) ;
#191312 = CARTESIAN_POINT ( 'NONE',  ( -5.826172809686546827, 6.253349265757417008, -0.6540019011737445709 ) ) ;
#191313 = CARTESIAN_POINT ( 'NONE',  ( -3.867100128395853709, 5.534702787927018974, -1.599625672291256295 ) ) ;
#191314 = CARTESIAN_POINT ( 'NONE',  ( 0.1509401653462701109, -0.4529219869476922011, -2.027634260368789576 ) ) ;
#191315 = CARTESIAN_POINT ( 'NONE',  ( -5.041653019435350380, 6.975290837464928728, -1.599625672291271394 ) ) ;
#191317 = CARTESIAN_POINT ( 'NONE',  ( 1.094370286708164386, -0.4508366001288487412, -1.815394955969009239 ) ) ;
#191316 = CARTESIAN_POINT ( 'NONE',  ( 1.030938747749777118, -1.888616091942503461, 0.8971857714693499686 ) ) ;
#191318 = CARTESIAN_POINT ( 'NONE',  ( 1.634138513624566302, 0.1511188354343559470, -2.010518437453466589 ) ) ;
#191319 = EDGE_LOOP ( 'NONE', ( #182476, #149177 ) ) ;
#191320 = CARTESIAN_POINT ( 'NONE',  ( 1.364683531249990311, 3.946875000341417028, 1.214306433183764966E-14 ) ) ;
#191321 = CARTESIAN_POINT ( 'NONE',  ( 2.190578792945916842, 1.345991196328416573, 1.103389618610579381 ) ) ;
#191322 = AXIS2_PLACEMENT_3D ( 'NONE', #112023, #95728, #160700 ) ;
#191323 = CARTESIAN_POINT ( 'NONE',  ( 5.392392409933256303, 7.314210449720692786, 1.599625672291267398 ) ) ;
#191324 = CARTESIAN_POINT ( 'NONE',  ( 6.925078400183574345, 7.629137130509068498, 2.744348168701661095 ) ) ;
#191325 = CARTESIAN_POINT ( 'NONE',  ( 3.176078081051143531, -1.026819631599368066, 1.385778701376034316 ) ) ;
#191326 = CARTESIAN_POINT ( 'NONE',  ( 3.263397454411249399, 2.137687552337414587, -0.4822058812353549606 ) ) ;
#191327 = CARTESIAN_POINT ( 'NONE',  ( 5.215527394842717435, -0.3265260713646127022, 2.182469266582609091 ) ) ;
#191328 = CARTESIAN_POINT ( 'NONE',  ( -9.505468521307150809, 5.017170101577987928, -6.783879874543660371 ) ) ;
#191329 = B_SPLINE_CURVE_WITH_KNOTS ( 'NONE', 3,
 ( #165864, #198341, #55052, #178934, #148557, #64105, #66191, #197286, #49981, #182091 ),
 .UNSPECIFIED., .F., .F.,
 ( 4, 3, 3, 4 ),
 ( 0.000000000000000000, 8.893179197954992701E-05, 0.0001334007970840233410, 0.0001778705873658995192 ),
 .UNSPECIFIED. ) ;
#191330 = CARTESIAN_POINT ( 'NONE',  ( 2.307711192815030898, -1.741648834054570605, -1.296000553170826741 ) ) ;
#191331 = CARTESIAN_POINT ( 'NONE',  ( 1.576486190600217663, -1.733098801405801304, -0.5742540608338757568 ) ) ;
#191332 = CARTESIAN_POINT ( 'NONE',  ( 3.731751022097353321, 0.7093996228057770637, -1.995120430414954349 ) ) ;
#191333 = CARTESIAN_POINT ( 'NONE',  ( 6.539320575229250920, 2.072231551265828475, 2.205269387046896679 ) ) ;
#191334 = EDGE_LOOP ( 'NONE', ( #194006, #44689, #102456, #181039 ) ) ;
#191336 = CARTESIAN_POINT ( 'NONE',  ( 1.364683531249986537, 1.217708333674754950, -0.7879004041258239610 ) ) ;
#191335 = CARTESIAN_POINT ( 'NONE',  ( 3.509589594912354116, -2.258262956851801118, 0.3931918642409871212 ) ) ;
#191337 = DIRECTION ( 'NONE',  ( 0.000000000000000000, 0.000000000000000000, 1.000000000000000000 ) ) ;
#191338 = CARTESIAN_POINT ( 'NONE',  ( 2.855963913973019963, 6.483708332943829866, 0.000000000000000000 ) ) ;
#191339 = CARTESIAN_POINT ( 'NONE',  ( 5.426523936546859161, -0.9972995744461101708, -1.984925452567573023 ) ) ;
#191340 = CARTESIAN_POINT ( 'NONE',  ( -4.880572111239580124, 7.677455982212699759, 1.082531754730560403 ) ) ;
#191341 = EDGE_CURVE ( 'NONE', #177076, #139889, #212981, .T. ) ;
#191342 = CARTESIAN_POINT ( 'NONE',  ( 3.036663219780971978, 6.486598156479028709, -0.7216878364870267237 ) ) ;
#191343 = VECTOR ( 'NONE', #178625, 1000.000000000000114 ) ;
#191344 = CARTESIAN_POINT ( 'NONE',  ( -7.510853911846401942, 7.865010440016681592, 1.040834085586084257E-14 ) ) ;
#191345 = AXIS2_PLACEMENT_3D ( 'NONE', #120034, #2979, #88544 ) ;
#191346 = CARTESIAN_POINT ( 'NONE',  ( 0.009341426467586660259, -9.943661027227909344, 10.91969313363970251 ) ) ;
#191347 = ORIENTED_EDGE ( 'NONE', *, *, #140315, .T. ) ;
#191348 = CARTESIAN_POINT ( 'NONE',  ( 4.026017654026761150, -1.753031021560845559, 0.9963007555989014108 ) ) ;
#191350 = CARTESIAN_POINT ( 'NONE',  ( 3.871981579112850458, -2.032873796296597479, 0.3478246332576060973 ) ) ;
#191349 = CARTESIAN_POINT ( 'NONE',  ( 7.284808609244363353, 7.393364887073558656, 0.7998128361456341429 ) ) ;
#191351 = CARTESIAN_POINT ( 'NONE',  ( -5.064290697676250730, 7.960144884870772763, -1.236948567437242907 ) ) ;
#191352 = CARTESIAN_POINT ( 'NONE',  ( 4.462041952228939401, 6.299077925724123617, -1.443375672974068769 ) ) ;
#191353 = CARTESIAN_POINT ( 'NONE',  ( -3.285556943749998737, -3.230208332855375897, 1.896917185911908499 ) ) ;
#191354 = CARTESIAN_POINT ( 'NONE',  ( -0.6823417656249969321, 5.217708333674756283, -1.181850606188749264 ) ) ;
#191355 = CARTESIAN_POINT ( 'NONE',  ( 5.876942531769460132, 2.026063101133714461, -0.8356547683932225024 ) ) ;
#191356 = CARTESIAN_POINT ( 'NONE',  ( 3.235000160576475992, 2.016597019841442240, -0.002811030766311505089 ) ) ;
#191357 = CARTESIAN_POINT ( 'NONE',  ( 1.804012939494209267, 1.363607186100148638, -1.237405090928713092 ) ) ;
#191358 = CARTESIAN_POINT ( 'NONE',  ( 6.174848896020108668, 9.291408581077091000, 1.199719254218460707 ) ) ;
#191359 =( NAMED_UNIT ( * ) PLANE_ANGLE_UNIT ( ) SI_UNIT ( $, .RADIAN. ) );
#191360 = CARTESIAN_POINT ( 'NONE',  ( 5.930640623865813588, 1.760069778787749506, 0.4843501209313359479 ) ) ;
#191361 = CARTESIAN_POINT ( 'NONE',  ( -6.388916700537716764, 8.476822122092563916, 1.599625672291283607 ) ) ;
#191363 = CARTESIAN_POINT ( 'NONE',  ( -5.978219388983010418, 5.939287140093762574, -0.7998128361456362523 ) ) ;
#191362 = CARTESIAN_POINT ( 'NONE',  ( 5.278307949308306490, -1.261584246701217715, 1.877956315871305071 ) ) ;
#191364 = CARTESIAN_POINT ( 'NONE',  ( 2.455815469989936606, 0.5610288669116151317, -2.029897440403311215 ) ) ;
#191365 = CARTESIAN_POINT ( 'NONE',  ( -4.925354943514475003, 8.968274210734028529, 0.000000000000000000 ) ) ;
#191366 = CARTESIAN_POINT ( 'NONE',  ( 8.402302512167096893, 10.82577223566020841, -1.599625672291268286 ) ) ;
#191367 = CARTESIAN_POINT ( 'NONE',  ( 7.987161891782087686, 8.490979426600148372, -0.7216878364870317197 ) ) ;
#191368 = CARTESIAN_POINT ( 'NONE',  ( -5.852315862593199469, 9.979452273000736895, 0.7998128361456481317 ) ) ;
#191369 = CARTESIAN_POINT ( 'NONE',  ( -3.809009402267528710, 7.350678696556900427, -0.7255371203442788630 ) ) ;
#191370 = EDGE_CURVE ( 'NONE', #74569, #196234, #199043, .T. ) ;
#191371 = CARTESIAN_POINT ( 'NONE',  ( 6.385527161912102123, 9.433236874664039817, -1.082531754730537976 ) ) ;
#191372 = CARTESIAN_POINT ( 'NONE',  ( 4.016789712308713511, 7.804715019974644008, -0.2988979438510626085 ) ) ;
#191373 = AXIS2_PLACEMENT_3D ( 'NONE', #25384, #156473, #8062 ) ;
#191374 = CARTESIAN_POINT ( 'NONE',  ( -5.759516327706961647, 5.613857225279885732, -0.7998128361456221525 ) ) ;
#191375 = CARTESIAN_POINT ( 'NONE',  ( 2.514199509032362112, -0.6922678517280489441, 2.110887004458279481 ) ) ;
#191376 = CARTESIAN_POINT ( 'NONE',  ( 0.4521680116954321371, 0.6883007682146925488, -2.096869779678663281 ) ) ;
#191377 = CARTESIAN_POINT ( 'NONE',  ( -4.176793841461789114, 7.030620694084159794, -1.199719254218455378 ) ) ;
#191378 = CARTESIAN_POINT ( 'NONE',  ( 4.364835388595708743, 7.179726155748598515, 1.199719254218462483 ) ) ;
#191379 = CARTESIAN_POINT ( 'NONE',  ( 4.439869198996494681, 1.279870211898268550, 1.486999339763886097 ) ) ;
#191380 = CARTESIAN_POINT ( 'NONE',  ( 7.567422294721922960, 11.98040977715095323, 0.7998128361456462443 ) ) ;
#191381 = CARTESIAN_POINT ( 'NONE',  ( -5.532833371615617502, 6.236068886146576951, 0.9535701153140889730 ) ) ;
#191382 = CARTESIAN_POINT ( 'NONE',  ( 2.171277156482887882, 5.684907115872006145, -0.7998128361456291469 ) ) ;
#191383 = CARTESIAN_POINT ( 'NONE',  ( -0.6823417656250212460, 1.051041667008083325, 1.181850606188755259 ) ) ;
#191384 = CARTESIAN_POINT ( 'NONE',  ( -5.966997003790240228, 6.134120390609613338, -0.7216878364870338292 ) ) ;
#191386 = ORIENTED_EDGE ( 'NONE', *, *, #147671, .T. ) ;
#191385 = CARTESIAN_POINT ( 'NONE',  ( -6.751597309925468693, 6.979211071108916364, 0.7216878364870317197 ) ) ;
#191387 = CARTESIAN_POINT ( 'NONE',  ( 3.340189922722580196, -1.266226476691566738, -1.700888996046201029 ) ) ;
#191388 = CARTESIAN_POINT ( 'NONE',  ( -3.623772196602547346, 7.449761006003425834, 0.000000000000000000 ) ) ;
#191389 = CARTESIAN_POINT ( 'NONE',  ( 6.086834708314957432, -0.3123483334277510348, -2.138898144987111838 ) ) ;
#191390 = CARTESIAN_POINT ( 'NONE',  ( 4.071694929070113211, -1.056692140236010102, 1.507659738195665788 ) ) ;
#191391 = UNCERTAINTY_MEASURE_WITH_UNIT (LENGTH_MEASURE( 1.000000000000000082E-05 ), #163404, 'distance_accuracy_value', 'NONE');
#191392 = CARTESIAN_POINT ( 'NONE',  ( -5.485560113408387117, 6.267152048184752466, 0.9985905309092910631 ) ) ;
#191393 = CARTESIAN_POINT ( 'NONE',  ( 0.6823417656249882723, 1.738541667008083991, -1.181850606188749264 ) ) ;
#191394 = CARTESIAN_POINT ( 'NONE',  ( 6.509682854689390119, -0.8273637111445523162, -1.531083434488962780 ) ) ;
#191395 = CARTESIAN_POINT ( 'NONE',  ( 6.727182134110203826, 7.053687134213418197, 2.309100590371661710 ) ) ;
#191396 = CARTESIAN_POINT ( 'NONE',  ( 4.256897045010922476, 5.029096643009940415, -1.082531754730548412 ) ) ;
#191397 = CARTESIAN_POINT ( 'NONE',  ( -15.75000000000000000, 13.79999999999999893, -3.200000000000001510 ) ) ;
#191398 = CARTESIAN_POINT ( 'NONE',  ( 3.836934241894359054, 0.3148432204054998351, 2.138525872868973998 ) ) ;
#191399 = CARTESIAN_POINT ( 'NONE',  ( 5.518907608433407219, 2.013924273726455549, -0.09612181791086168992 ) ) ;
#191400 = CARTESIAN_POINT ( 'NONE',  ( -7.171900071504738072, 10.35067193585544665, -1.082531754730543083 ) ) ;
#191401 = CARTESIAN_POINT ( 'NONE',  ( 3.256853613824191029, -1.637998819981079990, 1.410756932016984377 ) ) ;
#191402 = CARTESIAN_POINT ( 'NONE',  ( 3.637922374042131590, 0.8895205046622333134, -1.759358583061757519 ) ) ;
#191403 = CARTESIAN_POINT ( 'NONE',  ( 0.1346727191937693857, 0.3808678606769915209, 2.158067550307264604 ) ) ;
#191404 = CARTESIAN_POINT ( 'NONE',  ( 0.7808295286375503963, -1.278884537891399553, 1.920602667021213961 ) ) ;
#191405 = CARTESIAN_POINT ( 'NONE',  ( 2.056002787803516973, 2.055476740694470728, -0.1483529063488266686 ) ) ;
#191406 = CARTESIAN_POINT ( 'NONE',  ( 5.671417317124205937, 1.160065345341480647, 1.557364503162941061 ) ) ;
#191409 = ORIENTED_EDGE ( 'NONE', *, *, #143030, .T. ) ;
#191408 = LINE ( 'NONE', #187413, #56651 ) ;
#191407 = CARTESIAN_POINT ( 'NONE',  ( -7.822691444960696572, 12.07029775252209092, -0.7216878364870267237 ) ) ;
#191410 = CARTESIAN_POINT ( 'NONE',  ( -7.469616286486262524, 7.679250187180907794, 0.7998128361456341429 ) ) ;
#191411 = CARTESIAN_POINT ( 'NONE',  ( 11.81911962874431055, 9.842894265158827594, 1.591749704452489533 ) ) ;
#191412 = EDGE_CURVE ( 'NONE', #1071, #103667, #205886, .T. ) ;
#191414 = ORIENTED_EDGE ( 'NONE', *, *, #194669, .F. ) ;
#191413 = CARTESIAN_POINT ( 'NONE',  ( -4.118644803501354978, 8.027112380718707030, 0.7998128361456352531 ) ) ;
#191415 = CARTESIAN_POINT ( 'NONE',  ( -6.521108698048767138, 10.55178454779148289, -0.7216878364870267237 ) ) ;
#191416 = CARTESIAN_POINT ( 'NONE',  ( 1.993488836774780060, 1.919990754028239488, -1.087721427556323617 ) ) ;
#191417 = CARTESIAN_POINT ( 'NONE',  ( -3.285556943750000514, -0.4885416661887091450, -1.896917185911906500 ) ) ;
#191418 = CARTESIAN_POINT ( 'NONE',  ( 6.192239757033616065, 0.9699301198475211994, -1.705161095427814466 ) ) ;
#191419 = CARTESIAN_POINT ( 'NONE',  ( -0.4019237886466933696, 9.051335450315374231, 1.500000000000005995 ) ) ;
#191420 = CARTESIAN_POINT ( 'NONE',  ( -0.7500000000000215383, 4.222916667349481123, 1.299038105676671107 ) ) ;
#191421 = CARTESIAN_POINT ( 'NONE',  ( 4.286934996870309433, 7.472684718058654418, -1.056577385247484457 ) ) ;
#191423 = CARTESIAN_POINT ( 'NONE',  ( 3.649297074908570321E-15, -6.789018801444764277E-15, 0.2598076211376221800 ) ) ;
#191422 = CARTESIAN_POINT ( 'NONE',  ( 0.07479286986305544449, 2.888457405263197941, -2.344396930208477947 ) ) ;
#191424 = CARTESIAN_POINT ( 'NONE',  ( 5.156134521940135329, -1.331146486249596306, 1.272188372451001026 ) ) ;
#191425 = VERTEX_POINT ( 'NONE', #59216 ) ;
#191426 = CARTESIAN_POINT ( 'NONE',  ( -0.6801582343750074422, -0.8177083329919260235, 1.178068619123834759 ) ) ;
#191427 = CARTESIAN_POINT ( 'NONE',  ( -7.531718027591449705, 8.745758106066849891, 1.199719254218462483 ) ) ;
#191428 = DIRECTION ( 'NONE',  ( 0.000000000000000000, 1.000000000000000000, 0.000000000000000000 ) ) ;
#191429 = CARTESIAN_POINT ( 'NONE',  ( 11.89942855770813956, 11.29999999999999893, 0.6999999999999992895 ) ) ;
#191430 = CARTESIAN_POINT ( 'NONE',  ( 11.80029657321907877, 6.865618457657816975, 1.950723814763024810 ) ) ;
#191431 = CARTESIAN_POINT ( 'NONE',  ( 5.066996723205273057, 6.934582148538044777, 1.599625672291267398 ) ) ;
#191432 = CARTESIAN_POINT ( 'NONE',  ( 1.288041055883992536, -0.9272951443832450069, 1.840570288256936804 ) ) ;
#191435 = CARTESIAN_POINT ( 'NONE',  ( 4.546344060013487898, -1.475942220874026489, 1.100600019281534836 ) ) ;
#191434 = CARTESIAN_POINT ( 'NONE',  ( 1.838117294476193431, -0.9991240133950601843, 1.569924424075196390 ) ) ;
#191433 = DIRECTION ( 'NONE',  ( 1.000000000000000000, 3.451266460341926211E-31, 0.000000000000000000 ) ) ;
#191436 = CARTESIAN_POINT ( 'NONE',  ( 7.793239369756836510, 7.986534107671458216, 0.7998128361456341429 ) ) ;
#191437 = CARTESIAN_POINT ( 'NONE',  ( -9.393996030428326094, 14.54120606779820513, -7.466831080202041449 ) ) ;
#191438 = VECTOR ( 'NONE', #122407, 1000.000000000000000 ) ;
#191439 = CARTESIAN_POINT ( 'NONE',  ( -5.444481204339554736, 8.509589284108232121, 1.199719254218454489 ) ) ;
#191441 = ORIENTED_EDGE ( 'NONE', *, *, #37586, .F. ) ;
#191440 = CARTESIAN_POINT ( 'NONE',  ( -6.580818069394661407, -6.606405293530497325, -7.011678565220725190 ) ) ;
#191442 = AXIS2_PLACEMENT_3D ( 'NONE', #24155, #103297, #105456 ) ;
#191443 = CARTESIAN_POINT ( 'NONE',  ( 4.125739685719872263, -2.112183141943014153, 0.6395159525410462065 ) ) ;
#191444 = CARTESIAN_POINT ( 'NONE',  ( 6.380173838452511959, -1.218392737502610013, 1.906166127322491910 ) ) ;
#191445 = CARTESIAN_POINT ( 'NONE',  ( -5.422898255786198440, 7.349800603215774331, -1.443375672974052559 ) ) ;
#191446 = CARTESIAN_POINT ( 'NONE',  ( 0.4746845637013075159, -1.383529810647101455, 1.320479256824915071 ) ) ;
#191447 = CARTESIAN_POINT ( 'NONE',  ( 0.07540816263147330500, 1.497505997221737273, 1.350731191893522976 ) ) ;
#191448 = CARTESIAN_POINT ( 'NONE',  ( -10.95308175811721085, 9.799999999999982947, 1.799999999999999600 ) ) ;
#191449 = CARTESIAN_POINT ( 'NONE',  ( 0.000000000000000000, 5.939655416065874327, 0.000000000000000000 ) ) ;
#191450 = CARTESIAN_POINT ( 'NONE',  ( 5.637344576021464881, -0.04253375892994575719, 1.911971901805489038 ) ) ;
#191451 = CARTESIAN_POINT ( 'NONE',  ( -0.4382560683119374190, -5.166862915010145052, -10.99126615174919408 ) ) ;
#191452 = CARTESIAN_POINT ( 'NONE',  ( 0.5670072068131201126, 0.1877032549213939472, -1.861219751863735672 ) ) ;
#191453 = CARTESIAN_POINT ( 'NONE',  ( 2.079314900164643820, 1.561883299538204151, 1.275554356156020308 ) ) ;
#191455 = CARTESIAN_POINT ( 'NONE',  ( 3.809285178775764447, 1.806332912941556623, 1.082654235687771749 ) ) ;
#191454 = CARTESIAN_POINT ( 'NONE',  ( -7.506410603460441422, 11.90922947067921278, -0.7998128361456291469 ) ) ;
#191456 = EDGE_CURVE ( 'NONE', #146356, #4353, #105887, .T. ) ;
#191457 = CARTESIAN_POINT ( 'NONE',  ( 8.444030743212801227, 8.745790710036752458, 0.7998128361456462443 ) ) ;
#191459 = CARTESIAN_POINT ( 'NONE',  ( -7.232384877886063990, 10.52520055992070525, -1.199719254218446718 ) ) ;
#191458 = CARTESIAN_POINT ( 'NONE',  ( -1.402160292154681736E-14, -0.1624999999999815481, -1.732050807568870754 ) ) ;
#191460 = CARTESIAN_POINT ( 'NONE',  ( 2.812765223479243737, -0.5904890161391795900, -1.931511402468567340 ) ) ;
#191461 = CARTESIAN_POINT ( 'NONE',  ( -0.6823417656249969321, 3.967708333674754950, -1.181850606188749264 ) ) ;
#191462 = EDGE_CURVE ( 'NONE', #205532, #199393, #73325, .T. ) ;
#191463 = CARTESIAN_POINT ( 'NONE',  ( 8.256552361042350796, 12.57646882128404187, 1.040834085586084257E-14 ) ) ;
#191464 = CARTESIAN_POINT ( 'NONE',  ( 4.042369558984196587, 2.150769235480045616, 0.2162802025119994753 ) ) ;
#191465 = CARTESIAN_POINT ( 'NONE',  ( 7.014364370223726830, 9.276787413384745662, -1.599625672291269396 ) ) ;
#191466 = CARTESIAN_POINT ( 'NONE',  ( 1.499999999999989120, 5.545833333333350268, -0.8660254037844323793 ) ) ;
#191468 = CARTESIAN_POINT ( 'NONE',  ( -9.622374086701562135, -9.063146643177661943, 0.5328106107931148694 ) ) ;
#191467 = CARTESIAN_POINT ( 'NONE',  ( 5.643937085038755797, 9.806620042512378177, -0.7998128361456481317 ) ) ;
#191469 = CARTESIAN_POINT ( 'NONE',  ( 9.368320956918616105, 10.03205532593431037, 0.7216878364870458196 ) ) ;
#191471 = CARTESIAN_POINT ( 'NONE',  ( 8.627580382214878441, 15.01093739429174079, -8.342115253638150207 ) ) ;
#191470 = CARTESIAN_POINT ( 'NONE',  ( 1.856167715545921748, -0.7324389044234179691, 2.044012385327702575 ) ) ;
#191473 = CARTESIAN_POINT ( 'NONE',  ( 1.241482983173985533, 1.839155304979672501, 0.08999620058360720265 ) ) ;
#191472 = CARTESIAN_POINT ( 'NONE',  ( -5.734735788900501952, 9.634349487118505806, 0.000000000000000000 ) ) ;
#191474 = CARTESIAN_POINT ( 'NONE',  ( -1.364683531250012516, 2.238541667008087988, -0.7879004041258289570 ) ) ;
#191475 = CARTESIAN_POINT ( 'NONE',  ( 1.628746693258641853, 0.2190750365392846177, 2.180598679842937759 ) ) ;
#191476 = CARTESIAN_POINT ( 'NONE',  ( 6.883263157960381129, 0.5832772681763243039, 2.006853359411898463 ) ) ;
#191477 = CARTESIAN_POINT ( 'NONE',  ( 3.239431411193524735, -1.996134195211620721, 1.065073381557869903 ) ) ;
#191478 = CARTESIAN_POINT ( 'NONE',  ( -6.235860587281615075, 9.362588887548838557, -1.199719254218440723 ) ) ;
#191479 = CARTESIAN_POINT ( 'NONE',  ( -1.001543065824772872E-14, 4.634375000341418804, 1.575800808251672791 ) ) ;
#191480 = CARTESIAN_POINT ( 'NONE',  ( 5.448178351099921102, 7.506598249424609293, 1.250114376932524252 ) ) ;
#191481 = CARTESIAN_POINT ( 'NONE',  ( 1.499999999999997113, 12.14583333333333748, -0.8660254037844378194 ) ) ;
#191482 = CARTESIAN_POINT ( 'NONE',  ( 7.688882512725796481, 8.142986817701137525, 0.000000000000000000 ) ) ;
#191483 = CARTESIAN_POINT ( 'NONE',  ( 4.780378767880190338, -1.716399873034094803, -0.4305553870933165883 ) ) ;
#191484 = CARTESIAN_POINT ( 'NONE',  ( 9.745613490124728884, 10.26430391476735338, 0.7998128361456462443 ) ) ;
#191485 = CARTESIAN_POINT ( 'NONE',  ( 0.9914056592630847708, 1.857388527897243291, -0.9925227068504693939 ) ) ;
#191487 = CARTESIAN_POINT ( 'NONE',  ( -1.500000000000013101, 1.629166666666691077, -0.8660254037844313801 ) ) ;
#191486 = CARTESIAN_POINT ( 'NONE',  ( 1.364683531250000303, 10.25520833367473017, -0.7879004041258355073 ) ) ;
#191488 = CARTESIAN_POINT ( 'NONE',  ( -4.339491684825780737, 7.220434844675483355, -1.199719254218455378 ) ) ;
#191489 = CARTESIAN_POINT ( 'NONE',  ( 6.310172759758509109, 1.158674036163497734, -1.650093421473826316 ) ) ;
#191491 = ORIENTED_EDGE ( 'NONE', *, *, #185383, .F. ) ;
#191490 = CARTESIAN_POINT ( 'NONE',  ( 5.203285271772914555, 1.593979872821064570, -0.8609055379997750945 ) ) ;
#191492 = CARTESIAN_POINT ( 'NONE',  ( 7.619319141200072920, 7.991553207595983643, 0.7216878364870317197 ) ) ;
#191493 = CARTESIAN_POINT ( 'NONE',  ( 10.39640486358069360, 11.02356051713265650, 0.7998128361456462443 ) ) ;
#191494 = CARTESIAN_POINT ( 'NONE',  ( 3.994877460428855720, 1.580554378303768770, -1.000287695324620252 ) ) ;
#191495 = AXIS2_PLACEMENT_3D ( 'NONE', #40174, #73730, #24970 ) ;
#191496 = CARTESIAN_POINT ( 'NONE',  ( 3.942288228968212849, -1.024710522258945655, 1.798826465557185506 ) ) ;
#191497 = TOROIDAL_SURFACE ( 'NONE', #22022, 1.749999999999999778, 0.5000000000000007772 ) ;
#191498 = CARTESIAN_POINT ( 'NONE',  ( -6.251718229232856139, 8.387033582228697881, -1.443375672974066548 ) ) ;
#191499 = CARTESIAN_POINT ( 'NONE',  ( -0.7500000000000179856, 10.82291666734946212, 1.299038105676658228 ) ) ;
#191500 = CARTESIAN_POINT ( 'NONE',  ( 9.399880572976245574, 9.860948844760784482, 0.7998128361456462443 ) ) ;
#191501 = CARTESIAN_POINT ( 'NONE',  ( -8.631737353394710155, 13.22211067893587533, 1.040834085586084257E-14 ) ) ;
#191502 = CARTESIAN_POINT ( 'NONE',  ( 7.343676480457483002, 8.596652644402405841, -1.199719254218452047 ) ) ;
#191503 = VECTOR ( 'NONE', #211371, 1000.000000000000000 ) ;
#191504 = FACE_OUTER_BOUND ( 'NONE', #89148, .T. ) ;
#191505 = CARTESIAN_POINT ( 'NONE',  ( -0.6823417656250212460, 5.363541667008087543, 1.181850606188767472 ) ) ;
#191506 = CARTESIAN_POINT ( 'NONE',  ( 3.824618516750320385, -1.319357783791510697, 1.452116237791359010 ) ) ;
#191507 = CARTESIAN_POINT ( 'NONE',  ( 1.704453651327157537, -1.458331393932917885, -1.392334588655015803 ) ) ;
#191508 = CARTESIAN_POINT ( 'NONE',  ( 11.94105721237523277, 10.90000000000000036, 1.187919463087248273 ) ) ;
#191509 = CARTESIAN_POINT ( 'NONE',  ( 7.583016927391839523, -5.196967604326695245, 7.968844136639797959 ) ) ;
#191510 = CARTESIAN_POINT ( 'NONE',  ( 0.5791066246769066561, 1.747692025923882841, -0.6672336632058751826 ) ) ;
#191511 = CARTESIAN_POINT ( 'NONE',  ( -1.364683531250012516, 3.488541667008085767, -0.7879004041258300672 ) ) ;
#191512 = CARTESIAN_POINT ( 'NONE',  ( 2.865492421389451039, -1.648320183868864364, -1.155634683092461978 ) ) ;
#191514 = CARTESIAN_POINT ( 'NONE',  ( 3.655961130333235776, 1.178038043211126817, 1.759042251235248600 ) ) ;
#191513 = CARTESIAN_POINT ( 'NONE',  ( -5.666945020832185875, 7.634521829102760115, 1.443375672974064550 ) ) ;
#191515 = CARTESIAN_POINT ( 'NONE',  ( 6.825078400183578253, 1.241995729952071414, 2.258014901253778017 ) ) ;
#191516 = CARTESIAN_POINT ( 'NONE',  ( 5.459458695672200435, 1.690470114046587646, 1.195012289465044564 ) ) ;
#191517 = CARTESIAN_POINT ( 'NONE',  ( 6.994027139803230320, 9.253060644560830994, -1.599625672291267398 ) ) ;
#191519 = CARTESIAN_POINT ( 'NONE',  ( 3.704402285031850539, 5.344888637335695414, -1.599625672291262513 ) ) ;
#191518 = CARTESIAN_POINT ( 'NONE',  ( 0.3981334665579424059, -0.7082897861981848342, -1.967241634975321452 ) ) ;
#191521 = VERTEX_POINT ( 'NONE', #158863 ) ;
#191520 = CARTESIAN_POINT ( 'NONE',  ( 4.840742024777624053, 0.3130767520662172121, 1.798364180563789327 ) ) ;
#191522 = CARTESIAN_POINT ( 'NONE',  ( 7.214910300766615769, 11.56914578420308715, -0.7998128361456291469 ) ) ;
#191523 = FACE_OUTER_BOUND ( 'NONE', #172118, .T. ) ;
#191524 = CARTESIAN_POINT ( 'NONE',  ( 10.18750394041541441, 13.31248422858857694, -7.180467324466926371 ) ) ;
#191525 = CARTESIAN_POINT ( 'NONE',  ( -10.87092197480563271, 4.494752981060541330, 4.557748927716649412 ) ) ;
#191527 =( BOUNDED_SURFACE ( )  B_SPLINE_SURFACE ( 3, 2, ( 
 ( #2292, #1233, #149652 ),
 ( #116139, #186396, #68369 ),
 ( #152849, #200505, #185330 ),
 ( #168029, #151792, #20687 ),
 ( #104103, #135541, #86778 ),
 ( #53212, #119343, #103033 ),
 ( #70494, #21739, #87848 ),
 ( #158, #182128, #99834 ),
 ( #7637, #203699, #191722 ),
 ( #156048, #71570, #187469 ),
 ( #157125, #55345, #27096 ),
 ( #189603, #121497, #39099 ) ),
 .UNSPECIFIED., .F., .F., .T. ) 
 B_SPLINE_SURFACE_WITH_KNOTS ( ( 4, 2, 2, 2, 2, 4 ),
 ( 3, 3 ),
 ( -1.951563910473907981E-18, 0.0007589766761258975305, 0.001517953352251797013, 0.001897441690314746916, 0.002276930028377696820, 0.003035906704503596194 ),
 ( 0.000000000000000000, 1.000000000000000000 ),
 .UNSPECIFIED. ) 
 GEOMETRIC_REPRESENTATION_ITEM ( )  RATIONAL_B_SPLINE_SURFACE ( (
 ( 1.000000000000000000, 0.8462407054814394813, 1.000000000000000000),
 ( 1.000000000000000000, 0.8467927744362970799, 1.000000000000000000),
 ( 1.000000000000000000, 0.8474042438982406500, 1.000000000000000000),
 ( 1.000000000000000000, 0.8486200509115283674, 1.000000000000000000),
 ( 1.000000000000000000, 0.8492421577839870395, 1.000000000000000000),
 ( 1.000000000000000000, 0.8499339144819614278, 1.000000000000000000),
 ( 1.000000000000000000, 0.8500877183792072689, 1.000000000000000000),
 ( 1.000000000000000000, 0.8503387282033902927, 1.000000000000000000),
 ( 1.000000000000000000, 0.8504341930334453625, 1.000000000000000000),
 ( 1.000000000000000000, 0.8507248712736660279, 1.000000000000000000),
 ( 1.000000000000000000, 0.8508901730824002252, 1.000000000000000000),
 ( 1.000000000000000000, 0.8509629433086481898, 1.000000000000000000) ) ) 
 REPRESENTATION_ITEM ( '' )  SURFACE ( )  );
#191526 = CARTESIAN_POINT ( 'NONE',  ( 1.364683531249996529, 12.27604166700805877, 0.7879004041258403923 ) ) ;
#191528 = CARTESIAN_POINT ( 'NONE',  ( 6.375647946566726176, 0.3219878414668366773, -1.884816399834337908 ) ) ;
#191529 = CARTESIAN_POINT ( 'NONE',  ( -7.971304249830880373, 11.38727316052296601, 1.199719254218453823 ) ) ;
#191530 = CARTESIAN_POINT ( 'NONE',  ( 5.795220594837462436, 8.848508896363995291, -1.199719254218440723 ) ) ;
#191531 = CARTESIAN_POINT ( 'NONE',  ( 3.449547071718272573, 5.999999999999998224, -2.024999999999992806 ) ) ;
#191532 = CARTESIAN_POINT ( 'NONE',  ( 4.080641047588898118, 5.783833860318930320, -1.443375672974051449 ) ) ;
#191533 = CARTESIAN_POINT ( 'NONE',  ( 9.488641820551087847, -8.200000000000001066, -0.4644097342742986578 ) ) ;
#191534 = CARTESIAN_POINT ( 'NONE',  ( 2.998324526916512411, 6.649795714711241423, 0.000000000000000000 ) ) ;
#191535 = EDGE_LOOP ( 'NONE', ( #74765, #212002, #213100, #132470 ) ) ;
#191536 = CARTESIAN_POINT ( 'NONE',  ( -5.966470118465691641, 9.118576350588734059, -1.199719254218452047 ) ) ;
#191537 = CARTESIAN_POINT ( 'NONE',  ( 0.07700591528351626025, 0.2537022344677486996, -1.946355950789683043 ) ) ;
#191539 = CARTESIAN_POINT ( 'NONE',  ( 4.830447868218803897, 8.857549289555754157, -0.7998128361456481317 ) ) ;
#191538 = FACE_OUTER_BOUND ( 'NONE', #202067, .T. ) ;
#191540 = CARTESIAN_POINT ( 'NONE',  ( -7.253312916980312330, -6.796015482748900993, 7.253312916980332758 ) ) ;
#191541 = CARTESIAN_POINT ( 'NONE',  ( 0.1399997263885795762, 1.361443548867202979, -2.255028951473649901 ) ) ;
#191542 = CARTESIAN_POINT ( 'NONE',  ( -5.504247177468192476, 7.444707678511436555, 1.443375672974064550 ) ) ;
#191543 = CARTESIAN_POINT ( 'NONE',  ( 2.686486993802192913, 6.285985259411197568, 0.7998128361456362523 ) ) ;
#191544 = CARTESIAN_POINT ( 'NONE',  ( 1.885543262503614592, -1.856164082770836110, 0.6587638493158411990 ) ) ;
#191545 = CARTESIAN_POINT ( 'NONE',  ( 3.691029940746898053, 1.730877988113326493, 1.034147909374658392 ) ) ;
#191546 = CARTESIAN_POINT ( 'NONE',  ( -7.965578943228732278, 9.251929174310385307, -1.199719254218446718 ) ) ;
#191547 = CARTESIAN_POINT ( 'NONE',  ( 6.827182134110223899, 2.937564492898884438, 2.740749177975018380 ) ) ;
#191548 = CARTESIAN_POINT ( 'NONE',  ( 3.345827479060593301, 2.191629467292684819, -0.0001215010576177677764 ) ) ;
#191549 = FILL_AREA_STYLE ('',( #109330 ) ) ;
#191550 = CARTESIAN_POINT ( 'NONE',  ( 1.870020283345479539, 0.9883514471830873171, 1.653387599232780447 ) ) ;
#191551 = CARTESIAN_POINT ( 'NONE',  ( -7.537443334193545397, 10.88110209227943770, -1.199719254218446718 ) ) ;
#191552 = FILL_AREA_STYLE_COLOUR ( '', #82876 ) ;
#191553 = CARTESIAN_POINT ( 'NONE',  ( 0.2329586101569866563, 0.2513371725885656938, -1.880733749865989068 ) ) ;
#191554 = CARTESIAN_POINT ( 'NONE',  ( -3.101842500994827390, 15.51993578035120791, -11.60075130251052755 ) ) ;
#191555 = CARTESIAN_POINT ( 'NONE',  ( 6.584456157731144899, 10.83361595066169514, -0.7998128361456291469 ) ) ;
#191556 = CARTESIAN_POINT ( 'NONE',  ( 4.690231075323689325, 7.559354456931247412, 1.199719254218462483 ) ) ;
#191557 = CARTESIAN_POINT ( 'NONE',  ( -7.005920419302424484, -8.176248043969003731, 6.451695228974702268 ) ) ;
#191558 = CARTESIAN_POINT ( 'NONE',  ( 4.990809943606266508, 6.915973915664348937, -1.443375672974068769 ) ) ;
#191559 = ORIENTED_EDGE ( 'NONE', *, *, #202741, .F. ) ;
#191561 = CARTESIAN_POINT ( 'NONE',  ( 3.475247029965710777, -1.776355867393118126, -0.9471225605895690070 ) ) ;
#191560 = CARTESIAN_POINT ( 'NONE',  ( 6.567912610837368881, -1.126952994821692533, 1.456688911285822119 ) ) ;
#191562 = CARTESIAN_POINT ( 'NONE',  ( 4.183220704542046420, -1.177475575078859027, -1.973740397952013836 ) ) ;
#191564 = CARTESIAN_POINT ( 'NONE',  ( 3.485049009367678252, 0.04119252264746588871, 1.860649646085434039 ) ) ;
#191563 = CARTESIAN_POINT ( 'NONE',  ( -0.1291982275798625457, 7.629137130509075604, -2.673995287120598086 ) ) ;
#191565 = CARTESIAN_POINT ( 'NONE',  ( -3.285556943750000514, -0.1385416661887106660, -1.896917185911906500 ) ) ;
#191566 = DIRECTION ( 'NONE',  ( 1.000000000000000000, -0.000000000000000000, -0.000000000000000000 ) ) ;
#191567 = CARTESIAN_POINT ( 'NONE',  ( 6.345967646908174054, -1.254484226688237447, -1.443505786478386899 ) ) ;
#191568 = CARTESIAN_POINT ( 'NONE',  ( -7.374745490829552885, 10.69128794168811680, -1.199719254218446718 ) ) ;
#191569 = CARTESIAN_POINT ( 'NONE',  ( -4.936577329151611515, 7.813071746435248599, 1.082531754730549967 ) ) ;
#191570 = CARTESIAN_POINT ( 'NONE',  ( 5.759345132242938092, 2.059656548118168562, -0.3582877099650525476 ) ) ;
#191571 = CARTESIAN_POINT ( 'NONE',  ( 5.002595493762530765, 8.780185809457538681, 1.040834085586084257E-14 ) ) ;
#191572 = EDGE_CURVE ( 'NONE', #59479, #209385, #163821, .T. ) ;
#191573 = DIRECTION ( 'NONE',  ( 0.000000000000000000, 1.000000000000000000, 0.000000000000000000 ) ) ;
#191574 = CARTESIAN_POINT ( 'NONE',  ( -11.06305611892948448, 12.34238460445608609, 0.9079708613958296093 ) ) ;
#191575 = CARTESIAN_POINT ( 'NONE',  ( 5.742733201377892449, 0.3429454505429993527, 1.690258806964558547 ) ) ;
#191576 = CARTESIAN_POINT ( 'NONE',  ( -5.274285450916075035, 6.112086766612214284, 1.199719254218450271 ) ) ;
#191577 = CARTESIAN_POINT ( 'NONE',  ( 1.388881788488422586, -0.6239178774879328149, -1.618199924151533686 ) ) ;
#191578 = CARTESIAN_POINT ( 'NONE',  ( -11.84100621633422179, 11.11041574223335893, -1.444132586618106728 ) ) ;
#191579 = CARTESIAN_POINT ( 'NONE',  ( 0.000000000000000000, 0.08000000000000020983, 11.18000000000000149 ) ) ;
#191580 = PRESENTATION_STYLE_ASSIGNMENT (( #163374 ) ) ;
#191581 = CARTESIAN_POINT ( 'NONE',  ( 5.717690620771469945, 0.4309847871033903877, -2.127713340945025511 ) ) ;
#191582 = CARTESIAN_POINT ( 'NONE',  ( 4.459475772512963232, 0.3974328844052883447, -1.781742007231662983 ) ) ;
#191583 = CARTESIAN_POINT ( 'NONE',  ( 2.483191118468269565, -0.005009705968514814069, 1.961936380092830001 ) ) ;
#191584 = EDGE_CURVE ( 'NONE', #3254, #31095, #41935, .T. ) ;
#191585 = SURFACE_STYLE_USAGE ( .BOTH. , #9646 ) ;
#191586 = CARTESIAN_POINT ( 'NONE',  ( -10.31505594189871111, 10.92865344183699428, -0.7998128361456291469 ) ) ;
#191587 = CARTESIAN_POINT ( 'NONE',  ( 6.753933077901968396, 11.03133902419432566, 0.7998128361456462443 ) ) ;
#191588 = CARTESIAN_POINT ( 'NONE',  ( 3.035902975225315714, -2.043024508941180706, 0.5676086983019896781 ) ) ;
#191589 = CARTESIAN_POINT ( 'NONE',  ( -0.08058608058608175695, -6.271284633940164888, 10.99970480893082225 ) ) ;
#191590 = EDGE_CURVE ( 'NONE', #100328, #64278, #160494, .T. ) ;
#191591 = CARTESIAN_POINT ( 'NONE',  ( 5.339274934379788269E-16, -0.5000000000000004441, -3.000000000000000444 ) ) ;
#191592 = CARTESIAN_POINT ( 'NONE',  ( -4.409912583257236562, 7.141888050452717351, -1.077592642408040424 ) ) ;
#191593 = CARTESIAN_POINT ( 'NONE',  ( 0.3564121386029559524, -2.069725681613205470, -0.05427943458365809548 ) ) ;
#191595 = CARTESIAN_POINT ( 'NONE',  ( 1.500000000000001332, 14.15625000068279604, 0.000000000000000000 ) ) ;
#191594 = CARTESIAN_POINT ( 'NONE',  ( -9.907867159398911383, 3.530917919964545071, 6.788957344969876573 ) ) ;
#191597 = ORIENTED_EDGE ( 'NONE', *, *, #153901, .T. ) ;
#191596 = CARTESIAN_POINT ( 'NONE',  ( 3.282088111431053612, 2.166828800601192206, -0.4882270792503102808 ) ) ;
#191598 = CARTESIAN_POINT ( 'NONE',  ( 0.9854702925387841539, -2.298851036028260353, 0.006955682198207107335 ) ) ;
#191600 = CARTESIAN_POINT ( 'NONE',  ( 6.491093265613332441, 0.1965012520625461223, 2.053163312798581774 ) ) ;
#191599 = CARTESIAN_POINT ( 'NONE',  ( 9.951321562750607086, 11.67259191370631477, -1.082531754730537088 ) ) ;
#191602 = CARTESIAN_POINT ( 'NONE',  ( 1.001543065824772753E-15, -2.362500000000001155, 4.012584370867899430 ) ) ;
#191601 = CARTESIAN_POINT ( 'NONE',  ( 4.878955176071345434, 6.785476686873604280, -1.599625672291269396 ) ) ;
#191603 = CARTESIAN_POINT ( 'NONE',  ( 0.000000000000000000, 13.49999999999999822, 0.000000000000000000 ) ) ;
#191604 = CARTESIAN_POINT ( 'NONE',  ( 5.249485218566787736, 1.838879873951341004, -0.09611505855997715120 ) ) ;
#191605 =( NAMED_UNIT ( * ) PLANE_ANGLE_UNIT ( ) SI_UNIT ( $, .RADIAN. ) );
#191606 = CARTESIAN_POINT ( 'NONE',  ( -0.2102771530458277249, 5.719403664101017526, -2.797728457938574387 ) ) ;
#191607 = CARTESIAN_POINT ( 'NONE',  ( 3.346439682166453711, 0.4181539295537542444, 1.673179028346531538 ) ) ;
#191608 = CARTESIAN_POINT ( 'NONE',  ( 0.6554828803995507158, 1.942095732595986890, -0.5424746339172461518 ) ) ;
#191609 = CARTESIAN_POINT ( 'NONE',  ( 3.393488084526240733, -0.9333142364225041065, -2.100862151682027612 ) ) ;
#191610 = CARTESIAN_POINT ( 'NONE',  ( 2.952682139456219268, 0.7592856210697115360, 2.131335665991466843 ) ) ;
#191611 = CARTESIAN_POINT ( 'NONE',  ( 5.057299757384343231, -1.778698004947255162, -1.127411927216742216 ) ) ;
#191612 = CARTESIAN_POINT ( 'NONE',  ( -6.536439455564198475, 8.719208346281938304, 1.443375672974064550 ) ) ;
#191613 = CARTESIAN_POINT ( 'NONE',  ( 3.936565515923634795, 0.2574710272360211105, 1.750749954138763442 ) ) ;
#191615 = CARTESIAN_POINT ( 'NONE',  ( 6.304234482382112148, 1.701787343685069009, -1.536020108501337855 ) ) ;
#191614 = CARTESIAN_POINT ( 'NONE',  ( 4.868786560638896255, 5.813244087901094481, 1.082531754730549078 ) ) ;
#191616 = CARTESIAN_POINT ( 'NONE',  ( 5.033073903806924321, -1.304366766181121573, -1.299653785596634137 ) ) ;
#191617 = CARTESIAN_POINT ( 'NONE',  ( -4.948889764188092677, 5.732458465429559169, 1.199719254218462483 ) ) ;
#191618 = CARTESIAN_POINT ( 'NONE',  ( 5.138177029454841893, 7.017625839162543677, 1.443375672974062551 ) ) ;
#191619 = CARTESIAN_POINT ( 'NONE',  ( 1.499999999999989120, 3.525000000000021227, 1.214306433183764966E-14 ) ) ;
#191620 = CARTESIAN_POINT ( 'NONE',  ( 4.892620165872568094, 1.823077252308364482, -1.215776859382920794 ) ) ;
#191621 = CARTESIAN_POINT ( 'NONE',  ( -2.286521462199063492, 5.819358805874190743, 1.040834085586084257E-14 ) ) ;
#191622 = DIRECTION ( 'NONE',  ( 0.000000000000000000, 0.000000000000000000, -1.000000000000000000 ) ) ;
#191623 = CARTESIAN_POINT ( 'NONE',  ( 4.545415791725802457, 1.850806902094417783, -0.9279678557222792445 ) ) ;
#191624 = CARTESIAN_POINT ( 'NONE',  ( 0.1632964843477149597, 1.879801964727344732, -0.7303121171872913875 ) ) ;
#191625 = CARTESIAN_POINT ( 'NONE',  ( -0.6823417656249969321, 4.217708333674755394, -1.181850606188749264 ) ) ;
#191626 = CARTESIAN_POINT ( 'NONE',  ( 3.668508669297173341, -1.293070320541231721, 1.428231264829373126 ) ) ;
#191627 = CARTESIAN_POINT ( 'NONE',  ( 0.6823417656249969321, 9.776041667008065872, -1.181850606188757036 ) ) ;
#191628 = CARTESIAN_POINT ( 'NONE',  ( -3.090895834235680262, 5.589500325708124606, 1.082531754730560403 ) ) ;
#191629 = CARTESIAN_POINT ( 'NONE',  ( 6.433838290133602200, -2.056603270127650429, 0.5165238393732355382 ) ) ;
#191630 = VERTEX_POINT ( 'NONE', #40865 ) ;
#191632 = CARTESIAN_POINT ( 'NONE',  ( 0.000000000000000000, 13.49999999999999822, -1.500000000000000222 ) ) ;
#191631 = CARTESIAN_POINT ( 'NONE',  ( -3.472296738875691346, 6.104744391113324120, 1.082531754730549967 ) ) ;
#191633 = CARTESIAN_POINT ( 'NONE',  ( 4.379447312414087357, 5.068108938359919158, -1.199719254218452047 ) ) ;
#191634 = CARTESIAN_POINT ( 'NONE',  ( -1.889141968554442386, 3.755428628636585220, -0.4000000000000271116 ) ) ;
#191635 = CARTESIAN_POINT ( 'NONE',  ( 3.914243274428867103, 2.801588762746437311, -0.7749999999999935829 ) ) ;
#191636 = CARTESIAN_POINT ( 'NONE',  ( 10.18181017373857067, 11.94149529319227909, 1.082531754730548412 ) ) ;
#191637 = CARTESIAN_POINT ( 'NONE',  ( 1.592165322863370980, 0.9698756732311950568, -1.705302290208744687 ) ) ;
#191638 = CARTESIAN_POINT ( 'NONE',  ( 1.364683531249986537, 1.717708333674749399, -0.7879004041258239610 ) ) ;
#191639 = CARTESIAN_POINT ( 'NONE',  ( 0.3999999999999883649, 3.251480759208426274, -0.4649507210925284961 ) ) ;
#191640 = CARTESIAN_POINT ( 'NONE',  ( 5.090269282739749102, 1.010147525469132557, -1.681691772506640481 ) ) ;
#191641 = CARTESIAN_POINT ( 'NONE',  ( -8.833300774503376473, 10.26427131079744193, 1.199719254218462483 ) ) ;
#191642 = CARTESIAN_POINT ( 'NONE',  ( -5.870317324592821073, 6.911420302522161663, -1.082531754730543083 ) ) ;
#191643 = CARTESIAN_POINT ( 'NONE',  ( 6.772347375734490527, -1.334533509509854943, 1.701269717329929820 ) ) ;
#191645 = VERTEX_POINT ( 'NONE', #176191 ) ;
#191644 = CARTESIAN_POINT ( 'NONE',  ( -0.2106725631050307412, 6.947230693896488951, -2.598707507344534040 ) ) ;
#191646 = CARTESIAN_POINT ( 'NONE',  ( 0.6823417656249899377, 4.176041667008085767, -1.181850606188754593 ) ) ;
#191647 = CARTESIAN_POINT ( 'NONE',  ( 6.696557531595894730, -0.5234078932761144776, -1.900562160593147754 ) ) ;
#191648 = CARTESIAN_POINT ( 'NONE',  ( 6.450542193449531503, 1.198949306261879455, 1.252755643323471668 ) ) ;
#191649 = AXIS2_PLACEMENT_3D ( 'NONE', #206409, #123146, #58033 ) ;
#191651 = CARTESIAN_POINT ( 'NONE',  ( 3.562233144267571650, -1.470601008620987749, 1.625073949779440419 ) ) ;
#191650 = CARTESIAN_POINT ( 'NONE',  ( -1.360316468750007779, 0.1406250003413919702, -1.734723475976807094E-15 ) ) ;
#191652 = CARTESIAN_POINT ( 'NONE',  ( 4.858593139428769803, 0.8780750695473713563, 2.134189430172124702 ) ) ;
#191653 = CARTESIAN_POINT ( 'NONE',  ( 6.397740692956204178, -0.6987371234766488470, 1.938827229339795455 ) ) ;
#191654 = CARTESIAN_POINT ( 'NONE',  ( 1.833828351339358287, 1.920785844388651409, 0.2851290042146270576 ) ) ;
#191655 = CARTESIAN_POINT ( 'NONE',  ( -4.243338890952901288, 6.934017225211593249, -1.082531754730548412 ) ) ;
#191656 = CARTESIAN_POINT ( 'NONE',  ( 5.577698110520374897, 5.843467644431432184, -0.7819401572049750060 ) ) ;
#191657 = EDGE_CURVE ( 'NONE', #143389, #51765, #208654, .T. ) ;
#191658 = CARTESIAN_POINT ( 'NONE',  ( 5.027636390373714903, -0.3086946445357250379, 2.097867224209007730 ) ) ;
#191659 = SURFACE_SIDE_STYLE ('',( #211111 ) ) ;
#191660 = CARTESIAN_POINT ( 'NONE',  ( 3.709611425391425854, 1.915599900965975433, 0.6298755557959597740 ) ) ;
#191661 = CARTESIAN_POINT ( 'NONE',  ( -4.216222583725562245, 7.862750747747711877, 0.7216878364870317197 ) ) ;
#191662 = CARTESIAN_POINT ( 'NONE',  ( -6.607619761813764647, 8.802252036906432764, 1.599625672291269396 ) ) ;
#191663 = DIRECTION ( 'NONE',  ( 0.000000000000000000, 0.000000000000000000, 1.000000000000000000 ) ) ;
#191664 = CARTESIAN_POINT ( 'NONE',  ( 1.734723475976807094E-15, 14.57308041853048231, 11.91973154060107376 ) ) ;
#191665 = CARTESIAN_POINT ( 'NONE',  ( -6.635789839245807897, 6.706452665400368218, 0.7998128361456341429 ) ) ;
#191666 = CARTESIAN_POINT ( 'NONE',  ( -6.493429226302317225, 6.540365283632955773, 0.7998128361456341429 ) ) ;
#191667 = CARTESIAN_POINT ( 'NONE',  ( 3.469446951953614189E-15, 5.229711127717882491, 1.214306433183764966E-14 ) ) ;
#191668 = VERTEX_POINT ( 'NONE', #25645 ) ;
#191669 = CARTESIAN_POINT ( 'NONE',  ( 5.717669251203768788, -2.011168408518650974, 0.4492202366306179417 ) ) ;
#191670 = B_SPLINE_CURVE_WITH_KNOTS ( 'NONE', 3,
 ( #162228, #49525, #112465, #212008, #127681, #32214, #129805, #163288, #143884, #96177, #196843, #131888, #164349, #47422, #62571, #64704, #181643, #31162, #113536, #194708, #114600, #45283, #177407, #78817, #165405, #180591 ),
 .UNSPECIFIED., .F., .F.,
 ( 4, 2, 2, 2, 2, 2, 2, 2, 2, 2, 1, 1, 2, 4 ),
 ( 0.1391494940249573542, 0.1534303038895106774, 0.1677111137540640007, 0.1819919236186173239, 0.1962727334831706472, 0.2105535433477239704, 0.2248343532122772659, 0.2391151630768305891, 0.2462555680091072507, 0.2498257704752456232, 0.2516108717083147539, 0.2525034223248493470, 0.2529496976331166436, 0.2533959729413839401 ),
 .UNSPECIFIED. ) ;
#191671 = CARTESIAN_POINT ( 'NONE',  ( -5.424670858799220063, 9.342883411992149334, 0.000000000000000000 ) ) ;
#191672 = UNCERTAINTY_MEASURE_WITH_UNIT (LENGTH_MEASURE( 1.000000000000000082E-05 ), #196303, 'distance_accuracy_value', 'NONE');
#191673 = CARTESIAN_POINT ( 'NONE',  ( 6.143253000323500856, 10.18122924377050609, -0.7216878364870458196 ) ) ;
#191674 = CARTESIAN_POINT ( 'NONE',  ( -4.928552533767591726, 5.708731696605642725, 1.199719254218462483 ) ) ;
#191675 = CARTESIAN_POINT ( 'NONE',  ( -4.004454267989906668, 5.765225627445230927, 1.599625672291270506 ) ) ;
#191676 = CARTESIAN_POINT ( 'NONE',  ( 4.336585317048437638, 1.240917556630851237, -1.593414756171371183 ) ) ;
#191678 = ORIENTED_EDGE ( 'NONE', *, *, #31143, .F. ) ;
#191677 = CARTESIAN_POINT ( 'NONE',  ( -1.201851678989727383E-14, 0.7125000000000225597, 1.732050807568877637 ) ) ;
#191680 = CARTESIAN_POINT ( 'NONE',  ( 8.107412671292031803, 11.44210330227398487, 1.082531754730557072 ) ) ;
#191679 = CARTESIAN_POINT ( 'NONE',  ( -3.644109427023046521, 7.473487774827342278, 0.000000000000000000 ) ) ;
#191681 = CARTESIAN_POINT ( 'NONE',  ( 7.305145839664861640, 7.417091655897478653, 0.7998128361456341429 ) ) ;
#191682 = CARTESIAN_POINT ( 'NONE',  ( 4.188392892783887156, -2.038203232304033108, -0.3041262925047826249 ) ) ;
#191683 = CARTESIAN_POINT ( 'NONE',  ( 2.584611472894111195, -0.6298744119781033435, 1.915600275669691488 ) ) ;
#191684 = EDGE_LOOP ( 'NONE', ( #137554, #170000, #121004, #130327, #145390, #138185 ) ) ;
#191685 = EDGE_CURVE ( 'NONE', #209652, #99096, #109116, .T. ) ;
#191686 = DIRECTION ( 'NONE',  ( 5.551115123125764829E-17, 0.000000000000000000, -1.000000000000000000 ) ) ;
#191687 = CARTESIAN_POINT ( 'NONE',  ( 4.273844736805816780, 6.009238164405336313, 1.599625672291267398 ) ) ;
#191689 = ORIENTED_EDGE ( 'NONE', *, *, #168266, .F. ) ;
#191688 = CARTESIAN_POINT ( 'NONE',  ( -0.2089193878862168341, 7.199905994521426322, -1.991006660531114747 ) ) ;
#191690 = CARTESIAN_POINT ( 'NONE',  ( 2.723982329760873178, -1.752761823190003287, -0.9961495992579154635 ) ) ;
#191691 = CARTESIAN_POINT ( 'NONE',  ( 2.009460956091331685, -0.8672641894471898594, -1.624084198382821587 ) ) ;
#191692 = CARTESIAN_POINT ( 'NONE',  ( 1.049971938256549109, -1.822247386521518298, -1.415841994891045674 ) ) ;
#191693 = CARTESIAN_POINT ( 'NONE',  ( 4.386945222473598527, 7.275797305264619652, -1.199719254218452047 ) ) ;
#191694 = CARTESIAN_POINT ( 'NONE',  ( 3.743588348364734752, -1.634107004491680115, -1.415051943026650161 ) ) ;
#191695 = CARTESIAN_POINT ( 'NONE',  ( 7.574201371528760163, 11.98831870009225931, 1.040834085586084257E-14 ) ) ;
#191696 = CARTESIAN_POINT ( 'NONE',  ( -7.413611068574208041, 7.543634422958360730, 0.7998128361456341429 ) ) ;
#191697 = CARTESIAN_POINT ( 'NONE',  ( 3.058317229773829471, 1.972480788633700577, -1.179572646267361025 ) ) ;
#191698 = ORIENTED_EDGE ( 'NONE', *, *, #159427, .T. ) ;
#191699 = DIRECTION ( 'NONE',  ( -1.000000000000000000, -0.000000000000000000, 0.000000000000000000 ) ) ;
#191700 = CARTESIAN_POINT ( 'NONE',  ( 1.006479672118578916, 1.419055151971573059, -1.218976214888117804 ) ) ;
#191701 = CARTESIAN_POINT ( 'NONE',  ( 6.051636762666342761, 0.5725952485956290472, -1.886469267683591466 ) ) ;
#191702 = VECTOR ( 'NONE', #108355, 1000.000000000000000 ) ;
#191704 = CARTESIAN_POINT ( 'NONE',  ( 9.693716643646601128, 10.41168362711695750, 0.7216878364870438212 ) ) ;
#191703 = CARTESIAN_POINT ( 'NONE',  ( -1.364683531250010295, 4.780208333674755394, 0.7879004041258379498 ) ) ;
#191706 = CARTESIAN_POINT ( 'NONE',  ( 0.5576012004645107822, -1.866542136390366036, -1.177153700605698461 ) ) ;
#191705 = CARTESIAN_POINT ( 'NONE',  ( -7.088215381846223906, 7.164006121775713609, 0.7998128361456341429 ) ) ;
#191707 = ADVANCED_FACE ( 'NONE', ( #27791 ), #140210, .T. ) ;
#191708 = DIRECTION ( 'NONE',  ( 0.000000000000000000, -1.000000000000000000, 0.000000000000000000 ) ) ;
#191709 = CARTESIAN_POINT ( 'NONE',  ( 5.952193131599331721, 6.902979060742733708, 1.199719254218462483 ) ) ;
#191710 = CARTESIAN_POINT ( 'NONE',  ( -4.713430959045263435, 8.650753218861462202, 0.7998128361456481317 ) ) ;
#191711 = DIRECTION ( 'NONE',  ( 0.9632918427306580433, 0.000000000000000000, -0.2684563758389303945 ) ) ;
#191712 = CARTESIAN_POINT ( 'NONE',  ( 5.471542181860619358, 1.900225975651721244, -0.5249898485142224791 ) ) ;
#191713 = CARTESIAN_POINT ( 'NONE',  ( 4.073124928733475869, -2.152535440544633971, -0.8323431910086924734 ) ) ;
#191714 = CARTESIAN_POINT ( 'NONE',  ( 6.004338076955692216, 1.858996105215251493, 0.09048898905416635774 ) ) ;
#191715 = EDGE_CURVE ( 'NONE', #125736, #149597, #206033, .T. ) ;
#191716 = CARTESIAN_POINT ( 'NONE',  ( 3.256738233524118620, -0.5941274279437200878, -1.975181216424357400 ) ) ;
#191717 = CARTESIAN_POINT ( 'NONE',  ( 5.016153647376196290, 8.796003655340152605, 0.7216878364870438212 ) ) ;
#191718 = CARTESIAN_POINT ( 'NONE',  ( 6.527324610336440180, 6.579909898339485252, 0.7998128361456331437 ) ) ;
#191719 = CARTESIAN_POINT ( 'NONE',  ( 3.250922972226694352, 7.014770244231638863, 0.7998128361456281477 ) ) ;
#191720 =( BOUNDED_SURFACE ( )  B_SPLINE_SURFACE ( 3, 2, ( 
 ( #196685, #48324, #114435 ),
 ( #164189, #83980, #181483 ),
 ( #118685, #65579, #33112 ),
 ( #168437, #166305, #132776 ) ),
 .UNSPECIFIED., .F., .F., .T. ) 
 B_SPLINE_SURFACE_WITH_KNOTS ( ( 4, 4 ),
 ( 3, 3 ),
 ( 0.000000000000000000, 9.170893476604520501E-05 ),
 ( 0.000000000000000000, 1.000000000000000000 ),
 .UNSPECIFIED. ) 
 GEOMETRIC_REPRESENTATION_ITEM ( )  RATIONAL_B_SPLINE_SURFACE ( (
 ( 1.000000000000000000, 0.7100530722026773267, 1.000000000000000000),
 ( 1.000000000000000000, 0.6998898451682598054, 1.000000000000000000),
 ( 1.000000000000000000, 0.6894756946157374333, 1.000000000000000000),
 ( 1.000000000000000000, 0.6787756258918233865, 1.000000000000000000) ) ) 
 REPRESENTATION_ITEM ( '' )  SURFACE ( )  );
#191721 = CARTESIAN_POINT ( 'NONE',  ( -1.402160292154681736E-14, 2.009375000341422801, -1.575800808251660134 ) ) ;
#191722 = CARTESIAN_POINT ( 'NONE',  ( -10.11125148033187315, 3.596105362421267326, -6.463595993774343462 ) ) ;
#191723 = CARTESIAN_POINT ( 'NONE',  ( 5.382223794500827552, 7.302347065049529462, -1.443375672974051449 ) ) ;
#191724 = CARTESIAN_POINT ( 'NONE',  ( 5.687976231080541289, -1.372897218612447290, -1.682037316681925132 ) ) ;
#191726 = CARTESIAN_POINT ( 'NONE',  ( 4.071694929070113211, -1.056692140236010102, 1.507659738195665788 ) ) ;
#191725 = CARTESIAN_POINT ( 'NONE',  ( -3.389175213736311587, 4.977123720824209840, 1.443375672974064550 ) ) ;
#191728 = CARTESIAN_POINT ( 'NONE',  ( 6.620655732516611103, 3.701195159515461075, 2.440764268381501179 ) ) ;
#191727 = CARTESIAN_POINT ( 'NONE',  ( -1.364683531249997417, 5.509375000341417916, 1.214306433183764966E-14 ) ) ;
#191729 = CARTESIAN_POINT ( 'NONE',  ( 6.128506746050899068, 0.2130254606748181456, 2.181202035047181020 ) ) ;
#191730 = CARTESIAN_POINT ( 'NONE',  ( 0.000000000000000000, 5.999999999999998224, 10.25000000000000000 ) ) ;
#191731 = CARTESIAN_POINT ( 'NONE',  ( 0.3689490567273964738, -1.476270946665221517, 1.714425361395756964 ) ) ;
#191732 = CARTESIAN_POINT ( 'NONE',  ( -4.182100719528288657, 7.584231438125928371, -0.9338283797597360936 ) ) ;
#191733 = DIRECTION ( 'NONE',  ( -0.8660254037844384856, 0.000000000000000000, 0.5000000000000004441 ) ) ;
#191734 = CARTESIAN_POINT ( 'NONE',  ( 6.177100234330334061, 7.056796855232915888, 1.058592334412721936 ) ) ;
#191735 = CARTESIAN_POINT ( 'NONE',  ( -4.706088717274938382, 6.583799151611112954, 1.443375672974058777 ) ) ;
#191736 = CARTESIAN_POINT ( 'NONE',  ( 3.445180431648323882, 6.073108699348104267, 1.082531754730549078 ) ) ;
#191737 = CARTESIAN_POINT ( 'NONE',  ( 0.5668360377511200143, 0.1796360565177144708, -1.760708420565498589 ) ) ;
#191738 = CARTESIAN_POINT ( 'NONE',  ( 5.285796247307868789, 1.939527786139252585, -0.5389555323440149426 ) ) ;
#191739 = B_SPLINE_CURVE_WITH_KNOTS ( 'NONE', 3,
 ( #51944, #32486, #82289, #118067 ),
 .UNSPECIFIED., .F., .F.,
 ( 4, 4 ),
 ( 0.0006045091498275825597, 0.001203384219977627961 ),
 .UNSPECIFIED. ) ;
#191740 = CARTESIAN_POINT ( 'NONE',  ( 4.808338034340912337, 8.761478140039733020, 1.040834085586084257E-14 ) ) ;
#191741 = CARTESIAN_POINT ( 'NONE',  ( 3.979594558520031189, 1.983667836772174509, -0.7075980189445835178 ) ) ;
#191742 = CARTESIAN_POINT ( 'NONE',  ( 2.759290930233889494, 1.818065234828979637, -0.6036251144310407213 ) ) ;
#191743 = CARTESIAN_POINT ( 'NONE',  ( -1.500000000000022204, 7.240846818246208905, 4.154462424328226433 ) ) ;
#191744 = CARTESIAN_POINT ( 'NONE',  ( 4.439879492920996817, 1.284938098365424164, 1.492779756951348125 ) ) ;
#191745 = CARTESIAN_POINT ( 'NONE',  ( 5.783464979101770709, 0.1443126057797445849, -2.014664192723765623 ) ) ;
#191746 = CARTESIAN_POINT ( 'NONE',  ( 1.656895194024514906, -1.602792776363659133, -0.9643473572949823325 ) ) ;
#191749 = ORIENTED_EDGE ( 'NONE', *, *, #71027, .F. ) ;
#191748 = CARTESIAN_POINT ( 'NONE',  ( 1.265713261412576562, 0.5522810963098608861, -1.830935845731461953 ) ) ;
#191747 = CARTESIAN_POINT ( 'NONE',  ( 4.670341630432963242, -1.123608009272176078, 1.308792564452855522 ) ) ;
#191751 = CARTESIAN_POINT ( 'NONE',  ( 5.368665641331531013, 5.365790791082654998, -0.7216878364870207285 ) ) ;
#191750 = CARTESIAN_POINT ( 'NONE',  ( 2.069229996397306426, -2.018448871333050842, -0.8927042923378907258 ) ) ;
#191752 = CARTESIAN_POINT ( 'NONE',  ( 1.364683531249988535, 2.426041667008088432, 0.7879004041258500513 ) ) ;
#191753 = CARTESIAN_POINT ( 'NONE',  ( 6.707479306934847507, -1.574971382793718178, -1.169550641929931079 ) ) ;
#191754 = CARTESIAN_POINT ( 'NONE',  ( 8.586391356156291010, 8.911878091804165791, 0.7998128361456481317 ) ) ;
#191755 = CARTESIAN_POINT ( 'NONE',  ( -9.130526383799315582, 12.73969898348616070, 1.199719254218462483 ) ) ;
#191756 = CARTESIAN_POINT ( 'NONE',  ( -3.378415862307731832, 6.366559134822412425, -0.8608806284970575984 ) ) ;
#191757 = CARTESIAN_POINT ( 'NONE',  ( -5.928993247877787809, 5.811580298812519807, 0.7998128361456341429 ) ) ;
#191759 = EDGE_LOOP ( 'NONE', ( #25987, #212066, #165678, #189941 ) ) ;
#191758 = CLOSED_SHELL ( 'NONE', ( #56184, #198258, #178564, #29591, #2951, #103662, #146633, #33046 ) ) ;
#191760 = ORIENTED_EDGE ( 'NONE', *, *, #147466, .T. ) ;
#191761 = CARTESIAN_POINT ( 'NONE',  ( 2.277862540309500083, -2.008769142935047380, 0.5008063122204224893 ) ) ;
#191762 = CARTESIAN_POINT ( 'NONE',  ( -0.7500000000000215383, 2.691666666666689522, 1.299038105676671107 ) ) ;
#191763 = CARTESIAN_POINT ( 'NONE',  ( 4.950698647284403009, 8.927565521807144577, 1.040834085586084257E-14 ) ) ;
#191764 = CARTESIAN_POINT ( 'NONE',  ( -6.256197817702116026, 9.386315656372753224, -1.199719254218440723 ) ) ;
#191765 = B_SPLINE_CURVE_WITH_KNOTS ( 'NONE', 3,
 ( #29658, #178042, #61080, #14439, #159651, #131464, #197465, #163929, #31794, #94674, #145578, #46985, #196417, #65315, #49109, #95744, #180168, #143439, #79462, #179107, #27506, #161795, #28586, #93606, #213693, #13386, #48061, #112041 ),
 .UNSPECIFIED., .F., .F.,
 ( 4, 2, 2, 2, 2, 2, 2, 2, 2, 2, 2, 2, 2, 4 ),
 ( -5.999999999696835784E-08, 0.001605602215309425698, 0.002408433322964136092, 0.003211264430618846703, 0.004014095538273557313, 0.004816926645928267491, 0.005619757753582977668, 0.006422588861237687845, 0.008028251076547109066, 0.008831082184201819243, 0.009633913291856527686, 0.01043674439951123786, 0.01123957550716594804, 0.01284523772247536492 ),
 .UNSPECIFIED. ) ;
#191766 = CARTESIAN_POINT ( 'NONE',  ( 3.542423274920540432, 7.354853930707762721, -1.734723475976807094E-15 ) ) ;
#191767 = CARTESIAN_POINT ( 'NONE',  ( 6.445950376775947177, -1.384621037358444662, -1.606076714075025613 ) ) ;
#191768 = FILL_AREA_STYLE ('',( #91109 ) ) ;
#191769 = CARTESIAN_POINT ( 'NONE',  ( 0.6823417656249882723, 1.926041667008083991, -1.181850606188749264 ) ) ;
#191771 = CARTESIAN_POINT ( 'NONE',  ( 3.358669367883368118, 4.941533567329135401, -1.599625672291262513 ) ) ;
#191770 = CARTESIAN_POINT ( 'NONE',  ( -0.7500000000000179856, 11.79166666666666607, 1.299038105676658228 ) ) ;
#191772 = CARTESIAN_POINT ( 'NONE',  ( 5.466172646012215530, 1.646588110366095314, 1.163089216160061001 ) ) ;
#191773 = CARTESIAN_POINT ( 'NONE',  ( 4.346842662630929333, -1.713972709756344859, -0.8558225519783541069 ) ) ;
#191774 = CARTESIAN_POINT ( 'NONE',  ( 3.210657068901449307, 1.982179491636561819, 0.9350799695589939731 ) ) ;
#191775 = DIRECTION ( 'NONE',  ( 1.000000000000000000, -0.000000000000000000, -0.000000000000000000 ) ) ;
#191776 = CARTESIAN_POINT ( 'NONE',  ( 0.7499999999999885647, 1.347916667349485786, -1.299038105676652899 ) ) ;
#191777 = CARTESIAN_POINT ( 'NONE',  ( 5.801044709096109031, -0.2997443204828981189, -1.990672168044338886 ) ) ;
#191778 = CARTESIAN_POINT ( 'NONE',  ( 1.160255710619631397, 1.910328232974867868, 0.09094507755665059978 ) ) ;
#191779 = CARTESIAN_POINT ( 'NONE',  ( -5.311043488251275591, 7.219303374425030562, -1.599625672291256295 ) ) ;
#191781 = CARTESIAN_POINT ( 'NONE',  ( 0.01720424586787797083, -1.842442205116225695, 0.8197940039925479816 ) ) ;
#191780 = CARTESIAN_POINT ( 'NONE',  ( -3.633221978782304351, 4.301475732409860697, -1.082531754730549967 ) ) ;
#191782 = CARTESIAN_POINT ( 'NONE',  ( -1.402160292154681736E-14, 10.23437500034139447, 1.575800808251682339 ) ) ;
#191784 = CARTESIAN_POINT ( 'NONE',  ( -5.794130544993808307, 7.853181283949808744, 1.599625672291263179 ) ) ;
#191783 = CARTESIAN_POINT ( 'NONE',  ( 3.720331632570073932, 1.985922124624572627, 0.6539709493295197129 ) ) ;
#191786 = ORIENTED_EDGE ( 'NONE', *, *, #7268, .F. ) ;
#191785 = CARTESIAN_POINT ( 'NONE',  ( 2.027930484333416050, 0.9963118489298377067, -1.407687550210996230 ) ) ;
#191787 = CARTESIAN_POINT ( 'NONE',  ( 1.806654366501771136, 9.001999999999998892, 2.419999999999998597 ) ) ;
#191788 = CARTESIAN_POINT ( 'NONE',  ( 5.961834861707224320, 7.978559976790334574, -1.599625672291262513 ) ) ;
#191789 = CARTESIAN_POINT ( 'NONE',  ( 10.62873463776380056, 13.79999999999999893, -3.200000000000001510 ) ) ;
#191790 = CARTESIAN_POINT ( 'NONE',  ( -4.448483798615272100, 8.203998508444197313, 0.000000000000000000 ) ) ;
#191791 = CARTESIAN_POINT ( 'NONE',  ( 5.952193131599331721, 6.902979060742733708, 1.199719254218462483 ) ) ;
#191792 = FACE_OUTER_BOUND ( 'NONE', #171035, .T. ) ;
#191793 = CARTESIAN_POINT ( 'NONE',  ( 2.437905218827548737, -1.044187398466125627, -1.480012136316358085 ) ) ;
#191794 = ORIENTED_EDGE ( 'NONE', *, *, #202148, .T. ) ;
#191795 = CARTESIAN_POINT ( 'NONE',  ( 2.758194185376297902, 5.305311418659259814, 1.199719254218452047 ) ) ;
#191796 = CARTESIAN_POINT ( 'NONE',  ( 4.899292406491845497, 6.809203455697518947, -1.599625672291273171 ) ) ;
#191797 = CARTESIAN_POINT ( 'NONE',  ( 3.949720763895887110, -1.252031560403286337, -1.309370340798710730 ) ) ;
#191798 = CARTESIAN_POINT ( 'NONE',  ( -10.98633066092102872, -7.699791778944246268, 0.5535395452644350511 ) ) ;
#191799 = CARTESIAN_POINT ( 'NONE',  ( 5.275030131637754138, 6.378586025900190748, 1.136986337720545581 ) ) ;
#191800 = CARTESIAN_POINT ( 'NONE',  ( 4.158551126772993989, -0.5825245785200537929, -1.767622772031415490 ) ) ;
#191801 = CARTESIAN_POINT ( 'NONE',  ( 1.282674911181800104, 1.565081248417903081, -1.104254300028691071 ) ) ;
#191802 = CARTESIAN_POINT ( 'NONE',  ( 0.4108170757193031486, 1.585627777896590151, 0.9046078287104839522 ) ) ;
#191803 = AXIS2_PLACEMENT_3D ( 'NONE', #211546, #96781, #51202 ) ;
#191804 = CARTESIAN_POINT ( 'NONE',  ( -11.94105721237523454, 13.52740784401789220, 1.187919463087248273 ) ) ;
#191805 = FACE_OUTER_BOUND ( 'NONE', #197390, .T. ) ;
#191806 = CARTESIAN_POINT ( 'NONE',  ( 5.732961426666957294, 7.278201736375829789, 1.206439608388230500 ) ) ;
#191807 = CARTESIAN_POINT ( 'NONE',  ( 9.680359324772703999, 13.43752487939449836, 8.167046318416048223 ) ) ;
#191808 = CARTESIAN_POINT ( 'NONE',  ( -6.385527162356468445, 10.39360608948380538, 1.040834085586084257E-14 ) ) ;
#191809 = DIRECTION ( 'NONE',  ( 0.000000000000000000, 1.000000000000000000, -8.546850786086437571E-32 ) ) ;
#191810 = AXIS2_PLACEMENT_3D ( 'NONE', #2320, #82529, #162745 ) ;
#191811 = CARTESIAN_POINT ( 'NONE',  ( 7.456621297836067086, 10.68284669990868174, 1.082531754730558626 ) ) ;
#191812 = CARTESIAN_POINT ( 'NONE',  ( 5.752784996495730496, -0.4749413952093975433, -1.911207028377271522 ) ) ;
#191813 = CARTESIAN_POINT ( 'NONE',  ( -5.739179097286464248, 5.590130456455974617, -0.7998128361456221525 ) ) ;
#191814 = DIRECTION ( 'NONE',  ( 0.1510067114093955887, -0.000000000000000000, 0.9885327375000383388 ) ) ;
#191815 = CARTESIAN_POINT ( 'NONE',  ( 0.5684512833941969268, -1.969177116664261762, -0.7025944222667882544 ) ) ;
#191816 = CARTESIAN_POINT ( 'NONE',  ( 8.392660782059197189, 9.750191319612612872, 1.199719254218462483 ) ) ;
#191817 = CARTESIAN_POINT ( 'NONE',  ( 5.385741010672205675, 1.293702408046822239, 1.427520146239504184 ) ) ;
#191818 = CARTESIAN_POINT ( 'NONE',  ( -5.961834861707238531, 7.978559976790334574, -1.599625672291263179 ) ) ;
#191819 = CARTESIAN_POINT ( 'NONE',  ( 1.483130931141176889, 1.688290157389197077, -0.6950536248920418103 ) ) ;
#191820 = CARTESIAN_POINT ( 'NONE',  ( 2.719571217284349363, -0.2154062111461417239, 2.196339928330424129 ) ) ;
#191821 = EDGE_CURVE ( 'NONE', #15788, #177320, #74478, .T. ) ;
#191822 = CARTESIAN_POINT ( 'NONE',  ( 11.96535697748089078, 12.34737332935543286, 0.9148528286453676550 ) ) ;
#191823 = CARTESIAN_POINT ( 'NONE',  ( 0.5274218815167727170, -0.2782315536139517431, 1.891897276498944347 ) ) ;
#191824 = CIRCLE ( 'NONE', #91522, 2.000000000000000000 ) ;
#191825 = CARTESIAN_POINT ( 'NONE',  ( 0.1859136753566691391, -1.208741973239912726, -1.555490313720475415 ) ) ;
#191826 = CARTESIAN_POINT ( 'NONE',  ( 2.138135174613201350, 0.4275120379338535614, 1.894264587998186089 ) ) ;
#191827 = ORIENTED_EDGE ( 'NONE', *, *, #76416, .F. ) ;
#191828 = CARTESIAN_POINT ( 'NONE',  ( 1.089219988750099732, 1.203171814842165288, -1.617568698395126292 ) ) ;
#191830 = CARTESIAN_POINT ( 'NONE',  ( 6.069184012654499583, 1.640672622335254793, 0.8782983229575453965 ) ) ;
#191829 = CARTESIAN_POINT ( 'NONE',  ( -5.926849427829407269, 6.943687749669614995, -1.199719254218453823 ) ) ;
#191831 = CARTESIAN_POINT ( 'NONE',  ( 5.734172623936983904, 5.654565914206774124, 0.7998128361456352531 ) ) ;
#191832 = DIRECTION ( 'NONE',  ( 0.000000000000000000, -1.000000000000000000, -1.804652791718263484E-16 ) ) ;
#191833 = CARTESIAN_POINT ( 'NONE',  ( 8.563946585326370098, 13.14302144952281814, 0.7998128361456462443 ) ) ;
#191834 = CARTESIAN_POINT ( 'NONE',  ( -5.525111292768871252, 6.404716915440499037, -1.199719254218446718 ) ) ;
#191835 = CARTESIAN_POINT ( 'NONE',  ( -8.072954122294394352, 8.383144328957069291, -0.7998128361456362523 ) ) ;
#191836 = CARTESIAN_POINT ( 'NONE',  ( 2.068174269828721101, -1.345378145056834063, 1.729934933326432445 ) ) ;
#191837 = CARTESIAN_POINT ( 'NONE',  ( 4.392478581147586603, 4.226905887534702977, -0.7216878364870188411 ) ) ;
#191838 = DIRECTION ( 'NONE',  ( -0.3281536732072464768, 0.000000000000000000, -0.9446243521954066358 ) ) ;
#191839 = CARTESIAN_POINT ( 'NONE',  ( 1.466069532605751007E-15, 14.48154074412737558, 12.00000000000000178 ) ) ;
#191840 = CARTESIAN_POINT ( 'NONE',  ( 2.930095790256614485, 1.013914413367119627, -1.518051517300327502 ) ) ;
#191841 = CARTESIAN_POINT ( 'NONE',  ( -1.500000000000001110, 13.05208333401612997, 0.8660254037844418162 ) ) ;
#191842 = CARTESIAN_POINT ( 'NONE',  ( -2.767835915484202047, 6.380892334706859792, -0.7998128361456281477 ) ) ;
#191843 = CARTESIAN_POINT ( 'NONE',  ( -5.628650723579520232, 7.468463085569896798, -1.343613510788654875 ) ) ;
#191844 = CARTESIAN_POINT ( 'NONE',  ( -0.02968770228137587730, 2.889947918782026726, -2.315223470976325526 ) ) ;
#191845 = CARTESIAN_POINT ( 'NONE',  ( 9.752392566931574081, 10.27221283770866300, -0.7998128361456281477 ) ) ;
#191846 = CARTESIAN_POINT ( 'NONE',  ( 0.4867822013649549251, -0.2347038428511475372, -1.912094274373641323 ) ) ;
#191847 = CARTESIAN_POINT ( 'NONE',  ( 5.278158119090741174, -1.046208158741080529, -1.659298866772864756 ) ) ;
#191848 = EDGE_CURVE ( 'NONE', #53173, #193311, #86296, .T. ) ;
#191849 = CARTESIAN_POINT ( 'NONE',  ( -6.009258394948636914E-15, 14.93749999999999822, -1.732050807568875195 ) ) ;
#191850 = CARTESIAN_POINT ( 'NONE',  ( -5.852315862593199469, 9.979452273000736895, 0.7998128361456481317 ) ) ;
#191851 = CARTESIAN_POINT ( 'NONE',  ( 5.996784015946103885, 5.890669528225568996, 1.040834085586084257E-14 ) ) ;
#191852 = CARTESIAN_POINT ( 'NONE',  ( 5.530878137806295669, -1.981686641427220286, 0.9361944923952856268 ) ) ;
#191853 = CIRCLE ( 'NONE', #202190, 0.2000000000000005107 ) ;
#191854 = CARTESIAN_POINT ( 'NONE',  ( -1.999999999999996669, 6.400000000000024336, 1.214306433183764966E-14 ) ) ;
#191855 = CARTESIAN_POINT ( 'NONE',  ( 3.608316154870555792, 2.070434559819031684, 0.004826415812286819970 ) ) ;
#191857 = CARTESIAN_POINT ( 'NONE',  ( -1.364683531250000748, 2.071875000341422357, 1.214306433183764966E-14 ) ) ;
#191856 = CARTESIAN_POINT ( 'NONE',  ( 7.872797348053842015, 14.38630072364382784, 9.000752197161077106 ) ) ;
#191858 = VERTEX_POINT ( 'NONE', #28862 ) ;
#191859 = CARTESIAN_POINT ( 'NONE',  ( 4.377739380128500279, -0.5030580445687399260, -2.242836179151234344 ) ) ;
#191860 = CARTESIAN_POINT ( 'NONE',  ( 6.480434237652121787, 9.543961796360731498, 1.082531754730558626 ) ) ;
#191862 = DIRECTION ( 'NONE',  ( 0.7592566023653044560, -0.6507913734559596097, -1.725633230170963762E-31 ) ) ;
#191861 = CARTESIAN_POINT ( 'NONE',  ( 6.061904079085887354, 6.244845311787889486, 0.000000000000000000 ) ) ;
#191863 = CARTESIAN_POINT ( 'NONE',  ( 6.620655732516620873, 0.004685112605665174221, 1.926407831898164558 ) ) ;
#191864 = CARTESIAN_POINT ( 'NONE',  ( -6.400331034103001748, 9.624747418832267698, 1.199719254218452935 ) ) ;
#191865 = CARTESIAN_POINT ( 'NONE',  ( 5.156170417566459108, -1.405356202774979524, 1.340433341176451520 ) ) ;
#191866 = ORIENTED_EDGE ( 'NONE', *, *, #118204, .T. ) ;
#191868 = CARTESIAN_POINT ( 'NONE',  ( 9.720832950873944611, 10.44331931888218001, -0.7216878364870257245 ) ) ;
#191867 = CIRCLE ( 'NONE', #150300, 2.000000000000000000 ) ;
#191869 = ADVANCED_FACE ( 'NONE', ( #177250 ), #181488, .F. ) ;
#191870 = VERTEX_POINT ( 'NONE', #179389 ) ;
#191871 = CARTESIAN_POINT ( 'NONE',  ( 5.554919272666569263, 0.3793472168572444292, 1.874222000232607765 ) ) ;
#191872 = CARTESIAN_POINT ( 'NONE',  ( 6.651377187556704484, -1.389000575594327103, -1.022263415358831473 ) ) ;
#191873 = CARTESIAN_POINT ( 'NONE',  ( 4.364470425680367249, -1.957169923074707274, -0.4852690807995581057 ) ) ;
#191875 = FACE_OUTER_BOUND ( 'NONE', #18060, .T. ) ;
#191874 = CARTESIAN_POINT ( 'NONE',  ( -8.503988664269602538, 10.94440607977979063, 1.599625672291269396 ) ) ;
#191876 = CARTESIAN_POINT ( 'NONE',  ( 1.001543065824772753E-15, -3.959374999522043304, 3.793834371823811669 ) ) ;
#191878 = CARTESIAN_POINT ( 'NONE',  ( 6.573528787226094572, 1.692674132781073260, -0.5166258990680439034 ) ) ;
#191877 = CARTESIAN_POINT ( 'NONE',  ( 1.482492212676550070, -0.3080716119066116421, -2.067685480015791111 ) ) ;
#191879 = CARTESIAN_POINT ( 'NONE',  ( 6.240861317752083970, 2.010826688392798101, -0.1511364921914087889 ) ) ;
#191881 = CARTESIAN_POINT ( 'NONE',  ( 3.135043019019596144, -2.021410203770683367, 1.080917199049796107 ) ) ;
#191880 = CARTESIAN_POINT ( 'NONE',  ( 4.980641328173811999, 6.904110530993182948, 1.599625672291269396 ) ) ;
#191882 = CARTESIAN_POINT ( 'NONE',  ( 1.692878195147719422, -0.5885122380313506651, 1.637943671576999272 ) ) ;
#191883 = CARTESIAN_POINT ( 'NONE',  ( 2.934188532424650830, 6.448561212153446576, -0.2786481428285088047 ) ) ;
#191884 = CARTESIAN_POINT ( 'NONE',  ( 0.8250588069352093878, -1.261192405561472274, 1.190076739608906697 ) ) ;
#191885 = CARTESIAN_POINT ( 'NONE',  ( -1.360316468749998675, 1.442708333674736831, 0.7853790794158961308 ) ) ;
#191886 = CARTESIAN_POINT ( 'NONE',  ( 1.504125588540955683, 1.858726126767410669, 0.09586466133617438379 ) ) ;
#191887 = CARTESIAN_POINT ( 'NONE',  ( 2.154941862968827504, -0.5775488349282401623, -2.092905974620140164 ) ) ;
#191888 = CARTESIAN_POINT ( 'NONE',  ( 3.063685658700274761, 1.282989771343697294, 1.555699169480361022 ) ) ;
#191889 = CARTESIAN_POINT ( 'NONE',  ( 5.218750000000002665, -0.7852924748297095414, 1.895863743164193371 ) ) ;
#191890 = CARTESIAN_POINT ( 'NONE',  ( -1.201851678989727383E-14, 1.493750000682814383, 1.732050807568877637 ) ) ;
#191891 = CARTESIAN_POINT ( 'NONE',  ( 0.3231025844343059505, -0.09812569541690382979, 1.924018777033975836 ) ) ;
#191892 = CARTESIAN_POINT ( 'NONE',  ( -1.402160292154681736E-14, 14.42187500034139980, 1.575800808251682339 ) ) ;
#191893 = CARTESIAN_POINT ( 'NONE',  ( 3.357896860617498369, -1.684415915708385114, -1.448384614443619434 ) ) ;
#191894 = ORIENTED_EDGE ( 'NONE', *, *, #8784, .F. ) ;
#191895 =( NAMED_UNIT ( * ) PLANE_ANGLE_UNIT ( ) SI_UNIT ( $, .RADIAN. ) );
#191896 = CARTESIAN_POINT ( 'NONE',  ( -0.7500000000000006661, 0.1083333333333560966, -1.299038105676652011 ) ) ;
#191897 = CARTESIAN_POINT ( 'NONE',  ( 8.565000355531088516, 11.01558638625153286, -1.599625672291257406 ) ) ;
#191898 = CARTESIAN_POINT ( 'NONE',  ( 1.364683531249988757, 0.1343750003414204142, 0.000000000000000000 ) ) ;
#191899 = CARTESIAN_POINT ( 'NONE',  ( 6.310783679736120533, -0.5911123833974815112, -2.141223572898354188 ) ) ;
#191900 = CARTESIAN_POINT ( 'NONE',  ( 4.246505328441081417, -1.940195102956907336, -0.2900488188990399396 ) ) ;
#191902 = CARTESIAN_POINT ( 'NONE',  ( -6.900736999675794792, 7.153207375817628666, 1.040834085586084257E-14 ) ) ;
#191901 = CARTESIAN_POINT ( 'NONE',  ( 10.54788032175191326, 11.40820791823982994, 0.7216878364870317197 ) ) ;
#191903 = CARTESIAN_POINT ( 'NONE',  ( -1.430889623655251075, 3.675352821211156140, -0.4691377289697510888 ) ) ;
#191904 = CARTESIAN_POINT ( 'NONE',  ( 5.747450795320371064, -1.778423256021565813, -1.398359773074304480 ) ) ;
#191905 = CARTESIAN_POINT ( 'NONE',  ( 2.646997546006967905, -0.3502154465670388461, -2.032575613165943818 ) ) ;
#191906 = CARTESIAN_POINT ( 'NONE',  ( -5.096975683733680818, 8.033889833409558534, -1.199719254218452047 ) ) ;
#191907 = ORIENTED_EDGE ( 'NONE', *, *, #158080, .F. ) ;
#191908 = CARTESIAN_POINT ( 'NONE',  ( 0.7499999999999902300, 3.264583334016149418, 1.299038105676669330 ) ) ;
#191909 = CARTESIAN_POINT ( 'NONE',  ( 3.708139779478221598, -0.7553879706188313392, -1.711406342686023541 ) ) ;
#191910 = CARTESIAN_POINT ( 'NONE',  ( 2.848001011750156408, 0.2514756280368075081, -1.715647774213580501 ) ) ;
#191911 = CARTESIAN_POINT ( 'NONE',  ( 6.614806895146394972, -0.1608752592793839531, 2.155998228907447523 ) ) ;
#191912 = CARTESIAN_POINT ( 'NONE',  ( 1.132168909276673796, -1.401036632855560349, -1.704990472574128502 ) ) ;
#191913 = CARTESIAN_POINT ( 'NONE',  ( 6.228462243142912413, 0.1929387083638624822, 1.932343765256574697 ) ) ;
#191915 = VERTEX_POINT ( 'NONE', #160997 ) ;
#191914 = DIRECTION ( 'NONE',  ( 0.7592566023652994600, 0.6507913734559651608, 0.000000000000000000 ) ) ;
#191916 = CARTESIAN_POINT ( 'NONE',  ( 0.7740648250077889481, 1.777010169924503558, -0.9530137779002674225 ) ) ;
#191917 = EDGE_CURVE ( 'NONE', #147946, #93554, #62889, .T. ) ;
#191918 = CARTESIAN_POINT ( 'NONE',  ( 6.142902043169038429, 7.013529245237516641, 0.9864344219776898237 ) ) ;
#191919 = CARTESIAN_POINT ( 'NONE',  ( 6.363907750917786821, -0.1017471579566435469, -2.013986097687201049 ) ) ;
#191920 = CARTESIAN_POINT ( 'NONE',  ( -8.422639742587602285, 10.84949900448412841, -1.599625672291263179 ) ) ;
#191921 = CARTESIAN_POINT ( 'NONE',  ( 6.337546739384100292, 9.481222731668410120, 1.199719254218460707 ) ) ;
#191922 = CARTESIAN_POINT ( 'NONE',  ( 1.040949779275250140E-15, 7.999999999999992895, 8.500000000000000000 ) ) ;
#191923 = CARTESIAN_POINT ( 'NONE',  ( 3.633261591126951018, -1.686358373764598406, 0.7000054678709469735 ) ) ;
#191924 = CARTESIAN_POINT ( 'NONE',  ( 2.327434156339613924, -0.0004056629378437063877, 2.206952907597827362 ) ) ;
#191925 = ORIENTED_EDGE ( 'NONE', *, *, #198311, .F. ) ;
#191926 = CARTESIAN_POINT ( 'NONE',  ( -5.139949632912262700, 5.169231791251960750, 0.7216878364870257245 ) ) ;
#191927 = UNCERTAINTY_MEASURE_WITH_UNIT (LENGTH_MEASURE( 1.000000000000000082E-05 ), #38477, 'distance_accuracy_value', 'NONE');
#191928 = CARTESIAN_POINT ( 'NONE',  ( 1.001543065824772753E-15, -1.859374999522040550, 3.793834371823811669 ) ) ;
#191929 = CARTESIAN_POINT ( 'NONE',  ( -7.857113714319432063, 9.125386407249497012, 1.199719254218462483 ) ) ;
#191930 = CARTESIAN_POINT ( 'NONE',  ( 1.142838682686732277, 1.947676595115959586, 0.5347052314127549444 ) ) ;
#191931 = CARTESIAN_POINT ( 'NONE',  ( -10.91944002402978775, -8.407420853759269619, 0.1905873483556677628 ) ) ;
#191932 = CARTESIAN_POINT ( 'NONE',  ( -3.461074353238556167, 7.259946855412102273, 0.000000000000000000 ) ) ;
#191933 = CARTESIAN_POINT ( 'NONE',  ( 2.465471660774602558, -0.4132369024843309258, 1.814301444843221089 ) ) ;
#191934 = CARTESIAN_POINT ( 'NONE',  ( 3.192055101013606233, 5.811482486902795230, -1.199719254218446718 ) ) ;
#191935 = CARTESIAN_POINT ( 'NONE',  ( 6.504528880466823537, -1.955196382115764964, 0.4926337920100053447 ) ) ;
#191936 = ORIENTED_EDGE ( 'NONE', *, *, #102584, .F. ) ;
#191937 = ORIENTED_EDGE ( 'NONE', *, *, #127587, .T. ) ;
#191938 = CARTESIAN_POINT ( 'NONE',  ( -8.995998617867369873, 10.45408546138876993, 1.199719254218462483 ) ) ;
#191939 = CARTESIAN_POINT ( 'NONE',  ( 4.266095019097836172, 0.8626762044917112293, 1.609013669381313294 ) ) ;
#191941 = CARTESIAN_POINT ( 'NONE',  ( -5.122186659821378996, 6.697499048860120041, -1.435703471572645551 ) ) ;
#191940 = CARTESIAN_POINT ( 'NONE',  ( -6.140917232347002042, 6.129101290685087911, -0.7998128361456362523 ) ) ;
#191942 = CARTESIAN_POINT ( 'NONE',  ( 5.646014316602349759, 7.456765758048159221, -1.329534273556526758 ) ) ;
#191943 = CARTESIAN_POINT ( 'NONE',  ( 6.380232485702068246, -0.2495653932444163448, 2.000551205290925783 ) ) ;
#191944 = CARTESIAN_POINT ( 'NONE',  ( 5.419803763747102821, 1.093575605593154920, -1.481025086994464113 ) ) ;
#191945 = CARTESIAN_POINT ( 'NONE',  ( 4.037936217472848810, -1.589972691411502659, -1.672771819537349325 ) ) ;
#191946 = CARTESIAN_POINT ( 'NONE',  ( 5.180097208873055692, 8.201141289397330780, -1.199719254218450271 ) ) ;
#191947 = CARTESIAN_POINT ( 'NONE',  ( 0.7200824656817590430, -1.100121004815158177, -1.742362558145001294 ) ) ;
#191948 = CARTESIAN_POINT ( 'NONE',  ( 7.467843683028853263, 7.606905806488803101, 0.7998128361456341429 ) ) ;
#191949 = CARTESIAN_POINT ( 'NONE',  ( 2.665492718168083641, 1.041058713608807418, 1.639284265488485381 ) ) ;
#191950 = CARTESIAN_POINT ( 'NONE',  ( 5.272985406448559509, -2.287992931341980896, 0.2183071761258491283 ) ) ;
#191951 = CARTESIAN_POINT ( 'NONE',  ( 0.000000000000000000, 7.999999999999992895, 0.000000000000000000 ) ) ;
#191952 = CARTESIAN_POINT ( 'NONE',  ( -6.291865805193673111, 9.498204651771386509, -1.199719254218452047 ) ) ;
#191953 = CARTESIAN_POINT ( 'NONE',  ( 4.117926171558832671, -0.9613396577640184182, -1.604580606731422554 ) ) ;
#191954 = VERTEX_POINT ( 'NONE', #14720 ) ;
#191955 =( GEOMETRIC_REPRESENTATION_CONTEXT ( 3 ) GLOBAL_UNCERTAINTY_ASSIGNED_CONTEXT ( ( #182641 ) ) GLOBAL_UNIT_ASSIGNED_CONTEXT ( ( #164668, #45606, #82336 ) ) REPRESENTATION_CONTEXT ( 'NONE', 'WORKASPACE' ) );
#191958 = CARTESIAN_POINT ( 'NONE',  ( -4.716257332707368910, 6.595662536282280719, -1.599625672291271394 ) ) ;
#191957 = CARTESIAN_POINT ( 'NONE',  ( -1.500000000000001332, 0.9312500006828163812, 0.000000000000000000 ) ) ;
#191956 = CARTESIAN_POINT ( 'NONE',  ( 2.601700882821424976, 1.355260107747566334, 1.349524769375435973 ) ) ;
#191959 = CARTESIAN_POINT ( 'NONE',  ( 3.739080281021701868, 0.3231575147602770426, 2.182976880621155136 ) ) ;
#191960 = CARTESIAN_POINT ( 'NONE',  ( -1.225000000000028066, 0.3125000006828221322, -4.336808689942017736E-14 ) ) ;
#191961 = EDGE_CURVE ( 'NONE', #79391, #105851, #46194, .T. ) ;
#191962 = B_SPLINE_CURVE_WITH_KNOTS ( 'NONE', 3,
 ( #26840, #27916, #11655, #63616 ),
 .UNSPECIFIED., .F., .F.,
 ( 4, 4 ),
 ( 0.000000000000000000, 0.0002908967400263861051 ),
 .UNSPECIFIED. ) ;
#191963 = CARTESIAN_POINT ( 'NONE',  ( 6.883263157960366918, 3.696842586722656865, 2.460469087180997327 ) ) ;
#191964 = CARTESIAN_POINT ( 'NONE',  ( 6.061904078641523697, 7.205214525570814210, -1.082531754730548412 ) ) ;
#191965 = CARTESIAN_POINT ( 'NONE',  ( -5.763624699140874164, 8.777960344756069233, -1.082531754730549967 ) ) ;
#191966 = CARTESIAN_POINT ( 'NONE',  ( 1.897670943237000918, -0.6677869454260307869, 1.854917580456706183 ) ) ;
#191967 = CARTESIAN_POINT ( 'NONE',  ( 2.169360633853111509, -2.109970246048063380, -0.9347365353246681607 ) ) ;
#191968 = CARTESIAN_POINT ( 'NONE',  ( 2.892962425504439050, 0.2373818416543191367, 1.947367909387688112 ) ) ;
#191969 = DIRECTION ( 'NONE',  ( -5.578564026256490882E-16, -1.000000000000000000, -9.066213480720158442E-32 ) ) ;
#191970 = CARTESIAN_POINT ( 'NONE',  ( 6.051645708474242547, 1.558200330177769377, 1.351431136778310726 ) ) ;
#191971 = CARTESIAN_POINT ( 'NONE',  ( 2.711267533052988732, 6.106969855296372707, -0.7216878364870267237 ) ) ;
#191972 = CARTESIAN_POINT ( 'NONE',  ( 4.553559489343365740, 6.405848385690952718, -1.599625672291269396 ) ) ;
#191973 = ORIENTED_EDGE ( 'NONE', *, *, #110985, .T. ) ;
#191974 = CARTESIAN_POINT ( 'NONE',  ( 5.102750050473856547, 1.865045247124358818, 0.7672954931761333253 ) ) ;
#191975 = CARTESIAN_POINT ( 'NONE',  ( 0.4019237886466816012, 10.17633545031537246, -1.499999999999998668 ) ) ;
#191976 = DIRECTION ( 'NONE',  ( 2.949029909160572061E-17, 1.000000000000000000, -8.673600428462616880E-15 ) ) ;
#191977 = CARTESIAN_POINT ( 'NONE',  ( 1.378881877344245277, 3.612814789602863730, 0.5904953584335879135 ) ) ;
#191978 = CARTESIAN_POINT ( 'NONE',  ( 8.075853055234393452, 12.57357899774884658, 0.7998128361456462443 ) ) ;
#191979 = CARTESIAN_POINT ( 'NONE',  ( 2.307711192815030898, -1.741648834054570605, -1.296000553170826741 ) ) ;
#191980 = CARTESIAN_POINT ( 'NONE',  ( 4.746236293235721604, 7.694970221153795364, 1.199719254218451159 ) ) ;
#191981 = ADVANCED_FACE ( 'NONE', ( #146901 ), #207302, .T. ) ;
#191982 = CARTESIAN_POINT ( 'NONE',  ( -11.86687934130374167, 9.990480503834417547, -1.056332641424308827 ) ) ;
#191983 = CARTESIAN_POINT ( 'NONE',  ( 2.073319367481298858, 1.791407343212477077, -0.5384048943791116537 ) ) ;
#191984 = CARTESIAN_POINT ( 'NONE',  ( 6.854756222516505737, -1.675677847961650313, 1.365199464886861946 ) ) ;
#191986 = CARTESIAN_POINT ( 'NONE',  ( 6.727182134110209155, 1.290711256955964448, 1.927001067762003972 ) ) ;
#191985 = FACE_OUTER_BOUND ( 'NONE', #17462, .T. ) ;
#191987 = CARTESIAN_POINT ( 'NONE',  ( 1.364683531249986537, 0.6135416670080880985, 0.7879004041258500513 ) ) ;
#191988 = DIRECTION ( 'NONE',  ( -3.451266460341926649E-31, -5.200010849845536803E-32, 1.000000000000000000 ) ) ;
#191989 = CARTESIAN_POINT ( 'NONE',  ( 3.211475575234080004, 1.509012206799903666, 1.174515185244667581 ) ) ;
#191990 = CARTESIAN_POINT ( 'NONE',  ( 3.678344558940789266, -1.705506331563589661, -0.4725282708486245875 ) ) ;
#191991 = VECTOR ( 'NONE', #139850, 1000.000000000000000 ) ;
#191992 = CARTESIAN_POINT ( 'NONE',  ( 2.139182944796279351, 0.001596215867826628054, 1.912461472203148771 ) ) ;
#191993 = CARTESIAN_POINT ( 'NONE',  ( -3.581325132304157943, 7.329963087663487364, -0.7998128361456281477 ) ) ;
#191995 = CARTESIAN_POINT ( 'NONE',  ( 6.415652790497161639, -1.255571041358375384, -1.446825450776100919 ) ) ;
#191994 = DIRECTION ( 'NONE',  ( 0.000000000000000000, 1.000000000000000000, 0.000000000000000000 ) ) ;
#191996 = CARTESIAN_POINT ( 'NONE',  ( -1.500000000000015099, -0.3708333333333105331, -0.8660254037844383745 ) ) ;
#191997 = CARTESIAN_POINT ( 'NONE',  ( 1.398975865466948632, 0.4019745351953528112, 2.030794141931663521 ) ) ;
#191998 = CARTESIAN_POINT ( 'NONE',  ( -1.001543065824772872E-14, 5.462500000000020783, 1.732050807568877637 ) ) ;
#191999 = CARTESIAN_POINT ( 'NONE',  ( 5.823093596695693819, -0.04436734784114480107, 1.870300906237104988 ) ) ;
#192000 = CARTESIAN_POINT ( 'NONE',  ( 1.312830284664792790, 1.609138963534262778, 0.8624270714618911260 ) ) ;
#192002 = CARTESIAN_POINT ( 'NONE',  ( 4.716601407767927689, 8.224641112169805979, 0.6639617910879731522 ) ) ;
#192001 = CARTESIAN_POINT ( 'NONE',  ( 5.936183876523434932, 1.091049494364674466, -1.918236432931222257 ) ) ;
#192003 = CARTESIAN_POINT ( 'NONE',  ( 1.364683531249986537, -0.3864583329919166199, 0.7879004041258500513 ) ) ;
#192004 = CARTESIAN_POINT ( 'NONE',  ( 2.980982186342299833, 1.941357688518682290, 0.6972846330933372139 ) ) ;
#192005 = CARTESIAN_POINT ( 'NONE',  ( -8.376239975144482486, 8.666701480623698828, 1.040834085586084257E-14 ) ) ;
#192006 = CARTESIAN_POINT ( 'NONE',  ( 1.419999999999989049, 6.280000000000042881, -2.873333333333329520 ) ) ;
#192007 = CARTESIAN_POINT ( 'NONE',  ( 9.348510611822643313, 10.86534945433664134, 1.199719254218453823 ) ) ;
#192008 = CARTESIAN_POINT ( 'NONE',  ( 1.476450096886796626, 3.427809906544330598, -0.2781497094537699333 ) ) ;
#192009 = EDGE_CURVE ( 'NONE', #124966, #8666, #60194, .T. ) ;
#192011 = CARTESIAN_POINT ( 'NONE',  ( -0.01492041558615165263, -9.953728265215222137, -10.91968477554607730 ) ) ;
#192010 = STYLED_ITEM ( 'NONE', ( #18857 ), #86694 ) ;
#192012 = CARTESIAN_POINT ( 'NONE',  ( 6.801350335910821165, 7.963938809097990124, 1.199719254218452047 ) ) ;
#192013 = ORIENTED_EDGE ( 'NONE', *, *, #172073, .F. ) ;
#192014 = CARTESIAN_POINT ( 'NONE',  ( 5.898901817742318698, 0.4001337562283372451, 2.031160294743330486 ) ) ;
#192015 = CARTESIAN_POINT ( 'NONE',  ( -1.364683531250000748, -0.1781249996585798634, 0.000000000000000000 ) ) ;
#192016 = CARTESIAN_POINT ( 'NONE',  ( 2.267066545249882381, -1.975312647937790933, -0.8782872871702239737 ) ) ;
#192017 = CARTESIAN_POINT ( 'NONE',  ( -4.610539993796915148, 8.375707290415371986, 0.1689211187793551172 ) ) ;
#192018 = CARTESIAN_POINT ( 'NONE',  ( 2.613930769413209898, -0.6315753767559011411, 1.918467498408537919 ) ) ;
#192019 = CARTESIAN_POINT ( 'NONE',  ( 6.720655732516659597, 0.5653683226944251627, 2.225905711026022971 ) ) ;
#192020 =( GEOMETRIC_REPRESENTATION_CONTEXT ( 3 ) GLOBAL_UNCERTAINTY_ASSIGNED_CONTEXT ( ( #72597 ) ) GLOBAL_UNIT_ASSIGNED_CONTEXT ( ( #129868, #161223, #179605 ) ) REPRESENTATION_CONTEXT ( 'NONE', 'WORKASPACE' ) );
#192023 = CARTESIAN_POINT ( 'NONE',  ( 6.426201623197458801, 9.480690412830290015, -1.082531754730537088 ) ) ;
#192022 = CARTESIAN_POINT ( 'NONE',  ( 1.001543065824772753E-15, -1.312499999999998224, 4.012584370867899430 ) ) ;
#192021 = CARTESIAN_POINT ( 'NONE',  ( 1.499999999999990896, 3.806250000682819046, 1.214306433183764966E-14 ) ) ;
#192024 = CARTESIAN_POINT ( 'NONE',  ( -5.284646014276622950, 9.387447126623207794, -0.7998128361456362523 ) ) ;
#192025 = CARTESIAN_POINT ( 'NONE',  ( 1.024625454658374624, 0.3981145430279106057, 1.976669095394629982 ) ) ;
#192027 = CARTESIAN_POINT ( 'NONE',  ( 5.566036750361066154, -1.391122746885119499, 1.693456055751572986 ) ) ;
#192026 = CARTESIAN_POINT ( 'NONE',  ( -3.744022975668147790, 7.519777238254810925, -0.7998128361456281477 ) ) ;
#192028 = CARTESIAN_POINT ( 'NONE',  ( 3.823036128929238942, 7.404033217152015567, 1.040834085586084257E-14 ) ) ;
#192029 = CARTESIAN_POINT ( 'NONE',  ( 4.974826827724895928, -1.381046924789817831, 1.323090558688621909 ) ) ;
#192030 = CARTESIAN_POINT ( 'NONE',  ( -4.733481511527885210, 4.890303307122107590, -0.5491554243041256722 ) ) ;
#192031 = CARTESIAN_POINT ( 'NONE',  ( 6.114364089638798738, 6.235772314107808079, 0.7216878364870317197 ) ) ;
#192033 = CARTESIAN_POINT ( 'NONE',  ( 3.796500049179197589, 1.423950305759081214, -1.427950143821264506 ) ) ;
#192032 = CARTESIAN_POINT ( 'NONE',  ( -9.639484029191951464, 10.34841224358651601, 0.7216878364870438212 ) ) ;
#192034 = CARTESIAN_POINT ( 'NONE',  ( 0.6823417656249969321, 13.08854166700806942, -1.181850606188757036 ) ) ;
#192035 = CARTESIAN_POINT ( 'NONE',  ( 5.702095886272589453, -1.724958192454665085, 0.004281591079305368218 ) ) ;
#192036 = CARTESIAN_POINT ( 'NONE',  ( 7.361151057576892143, 7.552707420120024828, 0.7998128361456291469 ) ) ;
#192037 = CARTESIAN_POINT ( 'NONE',  ( 8.256552361042350796, 12.57646882128404187, 1.040834085586084257E-14 ) ) ;
#192038 = CARTESIAN_POINT ( 'NONE',  ( -0.7500000000000215383, 4.691666666666684193, 1.299038105676671107 ) ) ;
#192039 = CARTESIAN_POINT ( 'NONE',  ( 4.006994748872731549, 1.602975652146242380, 0.9638501484771769823 ) ) ;
#192040 = CARTESIAN_POINT ( 'NONE',  ( 0.000000000000000000, 0.000000000000000000, 0.000000000000000000 ) ) ;
#192041 = CARTESIAN_POINT ( 'NONE',  ( 1.112269271232646739, 2.068042923180101411, -0.09779880236997220977 ) ) ;
#192042 = CARTESIAN_POINT ( 'NONE',  ( 11.84668730067608600, 10.90000000000000036, -1.400000000000001910 ) ) ;
#192043 = VERTEX_POINT ( 'NONE', #37161 ) ;
#192044 = CARTESIAN_POINT ( 'NONE',  ( -0.2110808730067273986, 0.0005491059566040295322, -1.796958327270286704 ) ) ;
#192045 = CARTESIAN_POINT ( 'NONE',  ( 3.390420931869152721, 6.113185632892752075, -1.199719254218452047 ) ) ;
#192046 = DIRECTION ( 'NONE',  ( 1.000000000000000000, 0.000000000000000000, -4.336808689942017736E-15 ) ) ;
#192047 = CARTESIAN_POINT ( 'NONE',  ( -0.08802119743880723601, -1.811174541614871236, -0.04475806069833241502 ) ) ;
#192048 = CARTESIAN_POINT ( 'NONE',  ( 5.858531774436539052, 6.007577623030311287, 0.000000000000000000 ) ) ;
#192049 = CARTESIAN_POINT ( 'NONE',  ( 0.04091653908484670782, 2.521406394469414725, -1.999686568719554192 ) ) ;
#192050 = ORIENTED_EDGE ( 'NONE', *, *, #87853, .T. ) ;
#192051 = CARTESIAN_POINT ( 'NONE',  ( 9.707274797260268429, 10.42750147299956964, 0.000000000000000000 ) ) ;
#192053 = CARTESIAN_POINT ( 'NONE',  ( 6.591235234537977661, 10.84152487360300299, 0.7998128361456462443 ) ) ;
#192052 = CARTESIAN_POINT ( 'NONE',  ( 0.6605093422152423788, -0.6574743052488278838, -1.848563176889833626 ) ) ;
#192054 = AXIS2_PLACEMENT_3D ( 'NONE', #69154, #151516, #22546 ) ;
#192055 = CARTESIAN_POINT ( 'NONE',  ( 4.833546035289306708, 0.5969252065377036454, -1.820314225251006945 ) ) ;
#192056 =( NAMED_UNIT ( * ) SI_UNIT ( $, .STERADIAN. ) SOLID_ANGLE_UNIT ( ) );
#192057 = CARTESIAN_POINT ( 'NONE',  ( -6.325812300595961446, 6.871976577178664058, 0.6903976412777796945 ) ) ;
#192058 = DIRECTION ( 'NONE',  ( 1.000000000000000000, 0.000000000000000000, 0.000000000000000000 ) ) ;
#192060 = ORIENTED_EDGE ( 'NONE', *, *, #60919, .F. ) ;
#192059 = CARTESIAN_POINT ( 'NONE',  ( 3.199361063144961825, 6.676412307070352270, -0.7216878364870267237 ) ) ;
#192061 = CARTESIAN_POINT ( 'NONE',  ( -8.012505595996376684, 12.29174759539704986, 0.000000000000000000 ) ) ;
#192062 = CARTESIAN_POINT ( 'NONE',  ( 1.481558191429488192, 1.997200094811113491, -0.8276061316847342919 ) ) ;
#192063 = CARTESIAN_POINT ( 'NONE',  ( -4.767627293860968507, 5.591261926706423857, -1.199719254218453823 ) ) ;
#192064 = CARTESIAN_POINT ( 'NONE',  ( 7.526184669361807522, 7.953172667109813077, 0.000000000000000000 ) ) ;
#192065 = CARTESIAN_POINT ( 'NONE',  ( 0.2289750728588327566, 1.457791096766167360, -1.540313549178488284 ) ) ;
#192066 = CARTESIAN_POINT ( 'NONE',  ( 4.225493254642153751, -1.746956894163293361, 0.5300125199643388463 ) ) ;
#192067 = CARTESIAN_POINT ( 'NONE',  ( 8.916730223294068836, 12.80236288771289743, -7.560066957809561394 ) ) ;
#192068 = CARTESIAN_POINT ( 'NONE',  ( 0.8429695343807745989, -1.692941477971823483, 1.009804834249914851 ) ) ;
#192069 = CARTESIAN_POINT ( 'NONE',  ( 3.656429697474584017, 1.903630103707624865, 0.1825790434749063051 ) ) ;
#192070 = ORIENTED_EDGE ( 'NONE', *, *, #182709, .F. ) ;
#192071 = CARTESIAN_POINT ( 'NONE',  ( 1.737500000000001155, -2.683333333333332682, 3.009438278150922130 ) ) ;
#192072 = CARTESIAN_POINT ( 'NONE',  ( 3.736728436007582310, -1.897426337869069668, -0.5277852043128227200 ) ) ;
#192073 = ORIENTED_EDGE ( 'NONE', *, *, #96073, .F. ) ;
#192074 = CARTESIAN_POINT ( 'NONE',  ( 6.339402847020720877, 0.7390441267520877489, -1.796137868246181046 ) ) ;
#192075 = ORIENTED_EDGE ( 'NONE', *, *, #168226, .F. ) ;
#192076 = CARTESIAN_POINT ( 'NONE',  ( -7.123883369337781879, 7.275895117174344229, 0.7998128361456341429 ) ) ;
#192078 = CARTESIAN_POINT ( 'NONE',  ( 6.029554895997981667, -0.2579198037528374066, 2.104758538420265168 ) ) ;
#192077 = CARTESIAN_POINT ( 'NONE',  ( -3.935609729716867289, 7.813571461303467913, 0.7998128361456352531 ) ) ;
#192079 = CARTESIAN_POINT ( 'NONE',  ( 5.817857313595521163, 9.801600942587855414, -0.7216878364870458196 ) ) ;
#192080 = CARTESIAN_POINT ( 'NONE',  ( 3.967365900211225593, -1.591558630706500832, -1.059764132600553355 ) ) ;
#192081 = CARTESIAN_POINT ( 'NONE',  ( 0.000000000000000000, 0.4330127018922214077, 6.200000000000000178 ) ) ;
#192082 = PLANE ( 'NONE',  #53787 ) ;
#192083 = CYLINDRICAL_SURFACE ( 'NONE', #196641, 1.224999999999996980 ) ;
#192084 = CARTESIAN_POINT ( 'NONE',  ( 5.619794420184654804, -0.4867899507037063422, 1.953244479579784976 ) ) ;
#192085 = DIRECTION ( 'NONE',  ( 0.000000000000000000, 1.496258514059622730E-16, -1.000000000000000000 ) ) ;
#192087 = CARTESIAN_POINT ( 'NONE',  ( 5.682827415814322158, 1.645762192317705486, -1.164983060713747909 ) ) ;
#192086 = CARTESIAN_POINT ( 'NONE',  ( 5.672426548614882158, -1.154804106291613675, 1.414059844683832834 ) ) ;
#192088 = CARTESIAN_POINT ( 'NONE',  ( 1.434126425884488354, 1.231690216755284562, 1.664001042209894088 ) ) ;
#192089 = CARTESIAN_POINT ( 'NONE',  ( -6.561783159334121152, 10.59923808595773664, -0.7216878364870278340 ) ) ;
#192090 = CARTESIAN_POINT ( 'NONE',  ( -6.290641498436300161, 6.895329709839009169, -0.7498213622291228786 ) ) ;
#192091 = CARTESIAN_POINT ( 'NONE',  ( 1.224999999999955014, 1.895833333333313053, -0.7072540797573217963 ) ) ;
#192092 = CARTESIAN_POINT ( 'NONE',  ( 6.297708355432167338, -0.6282832542035889922, 1.762108908958268216 ) ) ;
#192093 = CARTESIAN_POINT ( 'NONE',  ( 6.823831386379729302, 6.855558127064808716, -0.7998128361456281477 ) ) ;
#192094 = SURFACE_SIDE_STYLE ('',( #208349 ) ) ;
#192095 = CARTESIAN_POINT ( 'NONE',  ( 4.258669648468268676, 7.982548666606070320, 0.7216878364870257245 ) ) ;
#192096 = EDGE_CURVE ( 'NONE', #122076, #204354, #102287, .T. ) ;
#192097 = CARTESIAN_POINT ( 'NONE',  ( 2.205172540517054802, 5.724451730578533848, 1.040834085586084257E-14 ) ) ;
#192098 = CARTESIAN_POINT ( 'NONE',  ( -1.364683531250010295, 11.44270833367472662, 0.7879004041258445001 ) ) ;
#192099 = CARTESIAN_POINT ( 'NONE',  ( -5.284980951228653190, 5.060232619388524533, 0.000000000000000000 ) ) ;
#192101 = CARTESIAN_POINT ( 'NONE',  ( -6.095272577795516789, 9.268845886473535245, 1.199719254218452047 ) ) ;
#192100 = FILL_AREA_STYLE ('',( #128289 ) ) ;
#192102 = CARTESIAN_POINT ( 'NONE',  ( 3.357800782942537143, 0.03855433513636970927, -1.733892557700001502 ) ) ;
#192103 = CARTESIAN_POINT ( 'NONE',  ( -3.741160322367112379, 6.452105245148518797, 1.199719254218464037 ) ) ;
#192104 = CARTESIAN_POINT ( 'NONE',  ( 2.149362472714404504, 1.803301116200561882, -1.016697834320609894 ) ) ;
#192105 =( BOUNDED_SURFACE ( )  B_SPLINE_SURFACE ( 3, 2, ( 
 ( #131456, #167112, #115218 ),
 ( #49098, #32836, #99970 ),
 ( #168169, #199579, #50154 ),
 ( #181208, #166035, #200639 ),
 ( #65307, #51223, #184401 ),
 ( #148724, #31785, #36021 ) ),
 .UNSPECIFIED., .F., .F., .T. ) 
 B_SPLINE_SURFACE_WITH_KNOTS ( ( 4, 2, 4 ),
 ( 3, 3 ),
 ( -6.938893903907228378E-18, 0.002403677751102540304, 0.004807355502205087547 ),
 ( 0.000000000000000000, 1.000000000000000000 ),
 .UNSPECIFIED. ) 
 GEOMETRIC_REPRESENTATION_ITEM ( )  RATIONAL_B_SPLINE_SURFACE ( (
 ( 1.000000000000000000, 0.7789607113619948509, 1.000000000000000000),
 ( 1.000000000000000000, 0.7844575505954650696, 1.000000000000000000),
 ( 1.000000000000000000, 0.7910273759756671907, 1.000000000000000000),
 ( 1.000000000000000000, 0.8087931444444149687, 1.000000000000000000),
 ( 1.000000000000000000, 0.8199986536752983390, 1.000000000000000000),
 ( 1.000000000000000000, 0.8356624583022056463, 1.000000000000000000) ) ) 
 REPRESENTATION_ITEM ( '' )  SURFACE ( )  );
#192106 = CARTESIAN_POINT ( 'NONE',  ( 2.970428505833659472, -2.086373159142587586, -0.3592635996705355050 ) ) ;
#192107 =( GEOMETRIC_REPRESENTATION_CONTEXT ( 3 ) GLOBAL_UNCERTAINTY_ASSIGNED_CONTEXT ( ( #100335 ) ) GLOBAL_UNIT_ASSIGNED_CONTEXT ( ( #107185, #125589, #156952 ) ) REPRESENTATION_CONTEXT ( 'NONE', 'WORKASPACE' ) );
#192108 = CARTESIAN_POINT ( 'NONE',  ( 8.586391356156291010, 8.911878091804165791, 0.7998128361456481317 ) ) ;
#192109 = CARTESIAN_POINT ( 'NONE',  ( 1.364683531249988535, 3.905208333674751842, -0.7879004041258239610 ) ) ;
#192110 = CARTESIAN_POINT ( 'NONE',  ( 0.9714669389824581724, -0.2943045352901324518, 1.947222615934702139 ) ) ;
#192111 = CARTESIAN_POINT ( 'NONE',  ( 5.670051627282618689, 6.304626411287498122, 1.111461560052000586 ) ) ;
#192112 = CARTESIAN_POINT ( 'NONE',  ( 3.714570900464278846, 5.356752022006865843, 1.443375672974062551 ) ) ;
#192114 = CARTESIAN_POINT ( 'NONE',  ( -0.4652101495396395725, -7.972382850425336009, -9.716492259128731490 ) ) ;
#192113 = CARTESIAN_POINT ( 'NONE',  ( 1.737499999999999378, -0.8166666666666668739, -3.009438278150925683 ) ) ;
#192115 = CARTESIAN_POINT ( 'NONE',  ( 3.855682016854941274, 2.275109001451373292, -0.2794487578934058969 ) ) ;
#192116 = CARTESIAN_POINT ( 'NONE',  ( 1.137010146156680834, -1.651496384925277283, 0.7785749969668461778 ) ) ;
#192117 = CARTESIAN_POINT ( 'NONE',  ( 2.882959773793275726, -1.768624019741386277, -0.7279546805132871556 ) ) ;
#192118 = CARTESIAN_POINT ( 'NONE',  ( 6.475954649182838807, 7.584310507915338562, 1.199719254218452047 ) ) ;
#192119 = CARTESIAN_POINT ( 'NONE',  ( 4.975479186090839612, 8.748550117173898855, 0.7216878364870438212 ) ) ;
#192120 = CARTESIAN_POINT ( 'NONE',  ( -8.025536864285518490, 11.45054454405341282, -1.199719254218446718 ) ) ;
#192121 = CARTESIAN_POINT ( 'NONE',  ( 2.162360077456865870, 2.012843401649004882, 0.04526349954376075735 ) ) ;
#192122 = CARTESIAN_POINT ( 'NONE',  ( 2.078885752709497492, 1.828579749420868872, 0.7109141669488158177 ) ) ;
#192123 = CARTESIAN_POINT ( 'NONE',  ( -6.808165692356648258, 11.09461040772476714, 0.7998128361456481317 ) ) ;
#192124 = TRIMMED_CURVE ( 'NONE', #45076, ( PARAMETER_VALUE ( 3.141592653589793116 ), #94716 ), ( PARAMETER_VALUE ( 4.069539037113614199 ), #192169 ), .T., .PARAMETER. ) ;
#192125 = CARTESIAN_POINT ( 'NONE',  ( -7.576308911938196999, 7.733448573549685179, 0.7998128361456462443 ) ) ;
#192126 = CARTESIAN_POINT ( 'NONE',  ( 0.1751657365761495888, 6.947016338497860488, -2.639079955608885975 ) ) ;
#192128 = CARTESIAN_POINT ( 'NONE',  ( 3.906921071489596997, 1.517988030950194744, 0.9097272527330434455 ) ) ;
#192127 = CARTESIAN_POINT ( 'NONE',  ( 5.560518711993346130, -1.889693770910952253, -0.8946095687128383656 ) ) ;
#192129 = CARTESIAN_POINT ( 'NONE',  ( -7.247736482492920018, 16.00000000000182254, 10.57961706324668150 ) ) ;
#192130 = CARTESIAN_POINT ( 'NONE',  ( 6.105493113454719456, -2.275700256682281264, 0.2746985183333852110 ) ) ;
#192131 = CARTESIAN_POINT ( 'NONE',  ( 5.419757389058348807, 1.032087642559690543, -1.401099660988463169 ) ) ;
#192132 = CARTESIAN_POINT ( 'NONE',  ( 8.535021395002688749, 9.916278701380017324, 1.199719254218462483 ) ) ;
#192133 = FILL_AREA_STYLE ('',( #81599 ) ) ;
#192134 = CARTESIAN_POINT ( 'NONE',  ( 5.975915019019427454, 1.530855338724030457, 0.8140783706773281336 ) ) ;
#192135 = CARTESIAN_POINT ( 'NONE',  ( 5.705598495378635171, -1.708133787927707647, -1.340148157549289953 ) ) ;
#192136 = CARTESIAN_POINT ( 'NONE',  ( -3.824766175154623582, 7.348582304423016964, -0.7466790275774716212 ) ) ;
#192137 = CARTESIAN_POINT ( 'NONE',  ( 6.421112215724263272, -1.799107166270615732, 0.9110519380226205222 ) ) ;
#192139 =( GEOMETRIC_REPRESENTATION_CONTEXT ( 3 ) GLOBAL_UNCERTAINTY_ASSIGNED_CONTEXT ( ( #34464 ) ) GLOBAL_UNIT_ASSIGNED_CONTEXT ( ( #22875, #133496, #142025 ) ) REPRESENTATION_CONTEXT ( 'NONE', 'WORKASPACE' ) );
#192138 = CARTESIAN_POINT ( 'NONE',  ( 4.687500000000003553, -1.451031289060926488, 1.451031289061301521 ) ) ;
#192140 = CARTESIAN_POINT ( 'NONE',  ( -1.201851678989727383E-14, 5.368750000682816825, -1.732050807568863648 ) ) ;
#192141 = CARTESIAN_POINT ( 'NONE',  ( 3.768508550381458821, -1.294476758928708060, 1.426794059921440594 ) ) ;
#192142 = CARTESIAN_POINT ( 'NONE',  ( -1.402160292154681736E-14, 11.09375000068279249, 1.732050807568881190 ) ) ;
#192143 = CARTESIAN_POINT ( 'NONE',  ( -0.03994651564155191764, -1.721383993196375251, -1.403517996469628493 ) ) ;
#192144 = ORIENTED_EDGE ( 'NONE', *, *, #160757, .F. ) ;
#192145 = CARTESIAN_POINT ( 'NONE',  ( -1.500000000000013101, 3.879166666666685970, -0.8660254037844313801 ) ) ;
#192146 = CARTESIAN_POINT ( 'NONE',  ( 5.148345644887269756, 7.029489223833707001, -1.599625672291256295 ) ) ;
#192147 = CARTESIAN_POINT ( 'NONE',  ( 6.174848896020108668, 9.291408581077091000, 1.199719254218460707 ) ) ;
#192148 = CARTESIAN_POINT ( 'NONE',  ( 2.297798353768167434, 2.029563722251678026, -0.9032078376340900716 ) ) ;
#192149 = PLANE ( 'NONE',  #205177 ) ;
#192150 = CARTESIAN_POINT ( 'NONE',  ( 8.283668668269706714, 8.766627655843892697, 1.040834085586084257E-14 ) ) ;
#192151 = CARTESIAN_POINT ( 'NONE',  ( -8.636180661780660017, 11.09863007687603087, -1.443375672974058777 ) ) ;
#192152 = CARTESIAN_POINT ( 'NONE',  ( 5.709392085130549077, 9.675058176045386205, 0.000000000000000000 ) ) ;
#192153 = VECTOR ( 'NONE', #68186, 1000.000000000000000 ) ;
#192154 = CARTESIAN_POINT ( 'NONE',  ( 1.213517774399593740, 1.944071949784083264, 0.5350861613380719639 ) ) ;
#192156 = CARTESIAN_POINT ( 'NONE',  ( 5.090308526370699305, 1.063348096890677441, -1.767349029039886110 ) ) ;
#192155 = CARTESIAN_POINT ( 'NONE',  ( 7.879259827836241570, 12.34422023245099176, 1.040834085586084257E-14 ) ) ;
#192157 =( NAMED_UNIT ( * ) PLANE_ANGLE_UNIT ( ) SI_UNIT ( $, .RADIAN. ) );
#192158 = CARTESIAN_POINT ( 'NONE',  ( -4.060830702492950195, 4.696389560118578999, -1.199719254218452047 ) ) ;
#192159 = B_SPLINE_CURVE_WITH_KNOTS ( 'NONE', 3,
 ( #80791, #160977, #129624, #81844, #65564, #94928, #14696, #213943, #131711, #127499 ),
 .UNSPECIFIED., .F., .F.,
 ( 4, 2, 2, 2, 4 ),
 ( 0.000000000000000000, 0.0002216178067634644539, 0.0004432356135269289077, 0.0006648534202903933887, 0.0008864712270538578154 ),
 .UNSPECIFIED. ) ;
#192160 = DIRECTION ( 'NONE',  ( -0.000000000000000000, -1.000000000000000000, -0.000000000000000000 ) ) ;
#192161 = CARTESIAN_POINT ( 'NONE',  ( 0.6823417656249882723, 0.4260416670080896528, -1.181850606188749264 ) ) ;
#192162 = CARTESIAN_POINT ( 'NONE',  ( 0.7371257246046484246, -1.245724469572104587, -1.257322912719664787 ) ) ;
#192163 = CARTESIAN_POINT ( 'NONE',  ( 5.854130254062820171, 0.1179724184225266898, -1.730206517700397795 ) ) ;
#192164 = CARTESIAN_POINT ( 'NONE',  ( 5.513164599239865460, -1.696177307367072506, 0.3892859123911066588 ) ) ;
#192165 = CARTESIAN_POINT ( 'NONE',  ( 2.683473709500754367, 1.623236604230539282, 1.618912294457574674 ) ) ;
#192166 = CARTESIAN_POINT ( 'NONE',  ( 1.364683531249986537, -0.09479166632524321789, -0.7879004041258309554 ) ) ;
#192167 = CARTESIAN_POINT ( 'NONE',  ( 1.763359053103892293, 0.9455654613358072114, 1.579637215005654349 ) ) ;
#192168 = CARTESIAN_POINT ( 'NONE',  ( 9.480175724453529185, 12.08329098332774265, 1.599625672291279388 ) ) ;
#192169 = CARTESIAN_POINT ( 'NONE',  ( -9.604686356149278126, 3.999999999999997335, -7.193747284969076894 ) ) ;
#192170 = CARTESIAN_POINT ( 'NONE',  ( 2.537895388257872753, 0.8626947210231518115, -1.608888323311054691 ) ) ;
#192171 = CARTESIAN_POINT ( 'NONE',  ( 3.322888845334175389, 0.9041102021897020613, -1.802417075407992897 ) ) ;
#192172 = CARTESIAN_POINT ( 'NONE',  ( -3.917943204224928699, 4.633650495426258509, -1.082531754730548412 ) ) ;
#192173 = DIRECTION ( 'NONE',  ( 1.224646799147343593E-16, 0.000000000000000000, -1.000000000000000000 ) ) ;
#192174 = CARTESIAN_POINT ( 'NONE',  ( 5.965875410913440646, 2.075401660611264631, -0.3564754433343624296 ) ) ;
#192175 = CARTESIAN_POINT ( 'NONE',  ( -5.551173829791513192, 8.563787670477010394, 1.199719254218452047 ) ) ;
#192176 = CARTESIAN_POINT ( 'NONE',  ( 10.13617411650463396, 13.69189752474446742, 7.314094131634138130 ) ) ;
#192177 = CARTESIAN_POINT ( 'NONE',  ( 2.172408243068229439, -0.9739482337229148357, -1.826950231780352762 ) ) ;
#192178 = CARTESIAN_POINT ( 'NONE',  ( 4.704842999142070603, 5.447737239542574272, -1.199719254218452047 ) ) ;
#192179 = CARTESIAN_POINT ( 'NONE',  ( -0.6801582343750316451, 0.8802083336747270614, -1.178068619123876282 ) ) ;
#192180 = CARTESIAN_POINT ( 'NONE',  ( 5.022192282182047940, -2.110239842997441606, 0.2083548542347323507 ) ) ;
#192181 = CARTESIAN_POINT ( 'NONE',  ( 1.418447215319606602, 1.294224929256732493, -1.427187236927564440 ) ) ;
#192182 = EDGE_LOOP ( 'NONE', ( #152141, #179880, #27839, #139424, #134041 ) ) ;
#192183 = CARTESIAN_POINT ( 'NONE',  ( -5.978219388983010418, 5.939287140093762574, -0.7998128361456362523 ) ) ;
#192184 = CARTESIAN_POINT ( 'NONE',  ( 9.447334110624092673, 9.916311305349925220, -0.7998128361456281477 ) ) ;
#192185 = CARTESIAN_POINT ( 'NONE',  ( 6.495764994278809823, 6.751016379513001375, 0.7216878364870328300 ) ) ;
#192186 = CARTESIAN_POINT ( 'NONE',  ( -1.737500000000000266, -1.414583332377417735, -3.009438278150923907 ) ) ;
#192187 = CARTESIAN_POINT ( 'NONE',  ( -6.552668314106420588, 6.539201209412602189, -0.7998128361456291469 ) ) ;
#192188 = CARTESIAN_POINT ( 'NONE',  ( 6.293239850429793947, -0.1054838202379469042, -2.118119863012501991 ) ) ;
#192189 = CARTESIAN_POINT ( 'NONE',  ( 2.327300794530688055, -0.001011052439145453856, 2.106147100168444197 ) ) ;
#192190 = CARTESIAN_POINT ( 'NONE',  ( -4.305596300791617814, 7.180890229968955651, 1.199719254218452935 ) ) ;
#192191 = CARTESIAN_POINT ( 'NONE',  ( 7.588813295347141441, 9.876701482703580837, -1.599625672291262513 ) ) ;
#192192 = CARTESIAN_POINT ( 'NONE',  ( 6.596546450148484730, 1.840605976333910654, 0.2736291870141689397 ) ) ;
#192193 = CARTESIAN_POINT ( 'NONE',  ( 7.344766530301147789, 9.591980256816594164, 1.599625672291281386 ) ) ;
#192194 = CARTESIAN_POINT ( 'NONE',  ( 3.719872605471106208, 6.605953636083950364, 7.500000000000000000 ) ) ;
#192195 = CARTESIAN_POINT ( 'NONE',  ( -3.298376509874564988, 7.070132704820777825, 0.000000000000000000 ) ) ;
#192196 = CARTESIAN_POINT ( 'NONE',  ( -8.663296969452339624, 13.05100419776235299, 1.040834085586084257E-14 ) ) ;
#192197 =( BOUNDED_CURVE ( )  B_SPLINE_CURVE ( 2, ( #27966, #7432, #9579, #177421, #15949, #29039, #148126 ),
 .UNSPECIFIED., .F., .T. ) 
 B_SPLINE_CURVE_WITH_KNOTS ( ( 3, 2, 2, 3 ),
 ( 0.5146539602424855531, 0.5166666666666667185, 0.5250000000000000222, 0.5292933853275720857 ),
 .UNSPECIFIED. ) 
 CURVE ( )  GEOMETRIC_REPRESENTATION_ITEM ( )  RATIONAL_B_SPLINE_CURVE ( ( 0.9509142384741717802, 0.9676418163423837759, 1.000000000000000000, 0.8660254037844387076, 1.000000000000000000, 0.9309754521208858380, 0.9330746597073281690 ) ) 
 REPRESENTATION_ITEM ( '' )  );
#192198 = CARTESIAN_POINT ( 'NONE',  ( -0.08743476694611679312, -2.120266877281291595, -0.04547849331201780226 ) ) ;
#192199 = FILL_AREA_STYLE ('',( #109977 ) ) ;
#192201 = CARTESIAN_POINT ( 'NONE',  ( 2.031626174157370457, 1.878314540015123102, -0.5664888411779643862 ) ) ;
#192200 = CARTESIAN_POINT ( 'NONE',  ( 1.360316468749961816, 2.817708333674743493, -0.7853790794159141164 ) ) ;
#192202 = CARTESIAN_POINT ( 'NONE',  ( 1.129994055010040022, -1.371941552271437770, -1.670562328977095445 ) ) ;
#192204 = CARTESIAN_POINT ( 'NONE',  ( -6.063230027062802563, 6.042581475280591086, 0.5001817740485012820 ) ) ;
#192203 = CARTESIAN_POINT ( 'NONE',  ( -5.204350862799341115, 7.165104988056252289, -1.599625672291271394 ) ) ;
#192205 = CARTESIAN_POINT ( 'NONE',  ( 0.6823417656249899377, 1.842708333674752952, 1.181850606188755259 ) ) ;
#192206 = CARTESIAN_POINT ( 'NONE',  ( 4.411323335215872277, 0.4626541248624673752, 1.670896574705359461 ) ) ;
#192207 = CARTESIAN_POINT ( 'NONE',  ( 2.290578643201816256, 1.344622755191619445, 1.104862870798990260 ) ) ;
#192208 = CARTESIAN_POINT ( 'NONE',  ( 7.483737605063422116, 7.833374748769873719, -0.7216878364870257245 ) ) ;
#192209 = CARTESIAN_POINT ( 'NONE',  ( -11.47199464713663453, 5.776720398841780124, 5.393175811422019628 ) ) ;
#192210 = CARTESIAN_POINT ( 'NONE',  ( 2.003279617838377824, 1.993765885540278004, 0.2985825316763612847 ) ) ;
#192211 = CARTESIAN_POINT ( 'NONE',  ( -0.08359363160203592269, -9.910747646673586431, -10.99968245379460186 ) ) ;
#192212 = CARTESIAN_POINT ( 'NONE',  ( -5.822300622425855110, 5.757381912443740646, 0.7998128361456281477 ) ) ;
#192213 = CARTESIAN_POINT ( 'NONE',  ( 1.287891803077842345, -0.8884654817012342942, 1.759997859036799284 ) ) ;
#192214 = EDGE_CURVE ( 'NONE', #97926, #146015, #102285, .T. ) ;
#192216 = CARTESIAN_POINT ( 'NONE',  ( -5.804299160426237059, 7.865044668620976509, -1.443375672974066548 ) ) ;
#192215 = CARTESIAN_POINT ( 'NONE',  ( 5.537344615273096515, -0.04053095765194079242, 1.912125305397804009 ) ) ;
#192217 = CARTESIAN_POINT ( 'NONE',  ( -4.936577328707246082, 8.773440960218172435, 0.000000000000000000 ) ) ;
#192218 = CARTESIAN_POINT ( 'NONE',  ( 5.794130544993763898, 7.853181283949808744, 1.599625672291269396 ) ) ;
#192219 = CARTESIAN_POINT ( 'NONE',  ( -5.257529707049291900, 9.355811434857983500, 0.7998128361456291469 ) ) ;
#192220 = CARTESIAN_POINT ( 'NONE',  ( 1.330729578248716960, 1.354828421643257119, -1.498027418808007605 ) ) ;
#192221 = CYLINDRICAL_SURFACE ( 'NONE', #128820, 0.3999999999999997446 ) ;
#192222 = CARTESIAN_POINT ( 'NONE',  ( 6.053837855137599533, 0.6775820993057954933, -2.205875079116952797 ) ) ;
#192223 = CARTESIAN_POINT ( 'NONE',  ( 5.582460749670235423, 1.169929261559121247, -1.574690175210855747 ) ) ;
#192224 = CARTESIAN_POINT ( 'NONE',  ( 2.852341167582587378, -1.956174252073937359, -0.1491622203949396763 ) ) ;
#192225 = CARTESIAN_POINT ( 'NONE',  ( 7.750457368506414646, 12.19395069656619945, 0.7998128361456462443 ) ) ;
#192226 = CARTESIAN_POINT ( 'NONE',  ( 0.6685925339881376717, 1.356301626434471164, 1.492253803477984864 ) ) ;
#192227 = ORIENTED_EDGE ( 'NONE', *, *, #30501, .T. ) ;
#192228 = CARTESIAN_POINT ( 'NONE',  ( 1.253280101782401124, 0.1498745247594003016, -2.112069961602327517 ) ) ;
#192230 = CARTESIAN_POINT ( 'NONE',  ( -5.831978632172702071, 9.955725504176825780, 0.7998128361456481317 ) ) ;
#192229 = CARTESIAN_POINT ( 'NONE',  ( -2.937312835655025101, 6.578615408239493867, 1.040834085586084257E-14 ) ) ;
#192231 = CARTESIAN_POINT ( 'NONE',  ( 2.536835285771391835, -1.364265644482412387, -1.236541980112846328 ) ) ;
#192232 = ORIENTED_EDGE ( 'NONE', *, *, #108284, .T. ) ;
#192233 = CARTESIAN_POINT ( 'NONE',  ( 11.07015750233977691, 9.209416967217014971, 4.635152785948085885 ) ) ;
#192235 = EDGE_CURVE ( 'NONE', #34591, #96990, #13773, .T. ) ;
#192234 = CARTESIAN_POINT ( 'NONE',  ( 3.076547362214879566, 0.9570632234598417387, 1.892448740577145738 ) ) ;
#192236 = CARTESIAN_POINT ( 'NONE',  ( 0.7499999999999920064, 4.264583334016150751, 1.299038105676669330 ) ) ;
#192237 = CARTESIAN_POINT ( 'NONE',  ( 6.591235234537977661, 10.84152487360300299, 0.7998128361456462443 ) ) ;
#192238 = CARTESIAN_POINT ( 'NONE',  ( 7.635176783151273128, 8.936736330878529699, 1.199719254218452935 ) ) ;
#192239 = CARTESIAN_POINT ( 'NONE',  ( 3.286453515990275243, -2.029689310919643219, -0.3557144749045982879 ) ) ;
#192241 = CARTESIAN_POINT ( 'NONE',  ( 0.7668492355173107677, 1.774547462407764842, -0.4907661837717376407 ) ) ;
#192240 = CARTESIAN_POINT ( 'NONE',  ( -7.853197290813634268, 10.18514947741448573, 1.599625672291295375 ) ) ;
#192242 = CARTESIAN_POINT ( 'NONE',  ( 0.6823417656249899377, 4.176041667008085767, -1.181850606188754593 ) ) ;
#192243 = CARTESIAN_POINT ( 'NONE',  ( 0.000000000000000000, 0.000000000000000000, 0.000000000000000000 ) ) ;
#192244 = LINE ( 'NONE', #77444, #11392 ) ;
#192245 = CARTESIAN_POINT ( 'NONE',  ( 0.7685542157043163680, 1.090964843879228097, 1.918292034055509632 ) ) ;
#192246 = CARTESIAN_POINT ( 'NONE',  ( 3.146068640573984165, 0.8174054641026907708, -2.109740015476600838 ) ) ;
#192247 = CARTESIAN_POINT ( 'NONE',  ( -7.782016984564068096, 10.10210578678999482, 1.443375672974090751 ) ) ;
#192248 = CARTESIAN_POINT ( 'NONE',  ( 2.988311359655666077, -1.075548189349010864, 1.457604102852279926 ) ) ;
#192249 = CARTESIAN_POINT ( 'NONE',  ( 3.045994482203842502, 0.8657459236516149570, 1.709044100283881429 ) ) ;
#192250 = CARTESIAN_POINT ( 'NONE',  ( 4.211429588753928144, -1.719575573843846072, -1.152724658989822348 ) ) ;
#192251 = CARTESIAN_POINT ( 'NONE',  ( 1.364683531249986537, 2.717708333674754062, -0.7879004041258239610 ) ) ;
#192252 = CARTESIAN_POINT ( 'NONE',  ( 3.168780698033875076, -1.820990468880798296, -0.7558852700480926945 ) ) ;
#192253 = CARTESIAN_POINT ( 'NONE',  ( 6.322878010905701451, 1.798576545740763644, 0.6907619847127777213 ) ) ;
#192254 = CARTESIAN_POINT ( 'NONE',  ( 2.799504582125960095, -0.5885537693137884441, 1.775713401224961574 ) ) ;
#192256 = CARTESIAN_POINT ( 'NONE',  ( 4.684384365712907616, 8.380862967975740929, 0.5977175665230231028 ) ) ;
#192255 = CARTESIAN_POINT ( 'NONE',  ( 2.526355290359350025, -1.329941221805782892, -1.885751665715528880 ) ) ;
#192257 = CARTESIAN_POINT ( 'NONE',  ( 3.103785861066649776, 0.6724651444435655323, -1.735490194124859054 ) ) ;
#192258 = CARTESIAN_POINT ( 'NONE',  ( -0.6823417656250212460, 2.551041667008084435, 1.181850606188767472 ) ) ;
#192259 = CIRCLE ( 'NONE', #102279, 1.600000000000005196 ) ;
#192260 = CARTESIAN_POINT ( 'NONE',  ( 6.514137810226229064, 2.057410315668557921, -0.1480156956644717581 ) ) ;
#192261 = CARTESIAN_POINT ( 'NONE',  ( -4.141125853970233806, 6.918731698685530063, -1.199719254218452047 ) ) ;
#192262 = CARTESIAN_POINT ( 'NONE',  ( 7.070740804726770357, 8.207951346058097286, 1.199719254218462483 ) ) ;
#192263 = CARTESIAN_POINT ( 'NONE',  ( -1.425171720896323491, 3.966122586717212073, 0.4907744223921879922 ) ) ;
#192264 = EDGE_CURVE ( 'NONE', #85555, #12149, #140424, .T. ) ;
#192265 = CARTESIAN_POINT ( 'NONE',  ( 1.032015147355441309, -1.337601665653989302, -1.626754097558680057 ) ) ;
#192266 = CARTESIAN_POINT ( 'NONE',  ( 0.6823417656249899377, 3.988541667008085767, -1.181850606188754593 ) ) ;
#192267 = CARTESIAN_POINT ( 'NONE',  ( 6.555963963954187790, 2.156316573842661732, -0.1517529999496904924 ) ) ;
#192268 = CARTESIAN_POINT ( 'NONE',  ( -0.2106725631050176961, -0.004273297132588448587, -2.003483006309704439 ) ) ;
#192269 = CARTESIAN_POINT ( 'NONE',  ( 1.364683531249986537, -0.8864583329919110133, 0.7879004041258500513 ) ) ;
#192270 = CARTESIAN_POINT ( 'NONE',  ( -3.456965981804629884, 6.976951378839947537, 1.040834085586084257E-14 ) ) ;
#192273 = CARTESIAN_POINT ( 'NONE',  ( 2.887523530030648988, 6.312601851770308414, 0.000000000000000000 ) ) ;
#192272 = CARTESIAN_POINT ( 'NONE',  ( 6.925078400183548588, 0.0006614011395407459748, 1.855452278108092656 ) ) ;
#192271 = CARTESIAN_POINT ( 'NONE',  ( 5.688527969385528849, 8.794310509995222347, -1.199719254218452047 ) ) ;
#192274 = CARTESIAN_POINT ( 'NONE',  ( -0.2104748580754166598, -0.006608320950483163522, -2.103482951484026753 ) ) ;
#192275 = CARTESIAN_POINT ( 'NONE',  ( 4.382046175016578005, -2.016188710442788246, -0.04465648322755921829 ) ) ;
#192277 = CARTESIAN_POINT ( 'NONE',  ( -6.197485614778184271, 9.284131412999601096, 1.082531754730549967 ) ) ;
#192276 = CARTESIAN_POINT ( 'NONE',  ( -8.839552966430002101, 12.29626697993494666, -1.082531754730543971 ) ) ;
#192278 =( NAMED_UNIT ( * ) SI_UNIT ( $, .STERADIAN. ) SOLID_ANGLE_UNIT ( ) );
#192280 = CARTESIAN_POINT ( 'NONE',  ( -8.012344526598182026E-15, 10.79687500034139802, -1.575800808251669460 ) ) ;
#192279 = CARTESIAN_POINT ( 'NONE',  ( 6.543834100630380846, 0.8322713294773576020, -1.995267709627518427 ) ) ;
#192281 = CARTESIAN_POINT ( 'NONE',  ( 10.49201538390852129, 0.9691415390508777428, -5.610609371109157806 ) ) ;
#192282 = CARTESIAN_POINT ( 'NONE',  ( -11.26709733201210284, 6.404816583109345096, 4.000485531852068455 ) ) ;
#192284 = CARTESIAN_POINT ( 'NONE',  ( 6.468375372808552903, -1.978050569928070379, -0.3905794195708453542 ) ) ;
#192283 = CARTESIAN_POINT ( 'NONE',  ( -6.412643469139482910, 7.544134137826577380, 1.082531754730549967 ) ) ;
#192285 = CARTESIAN_POINT ( 'NONE',  ( -1.364683531250000748, 0.3218750003414205807, 0.000000000000000000 ) ) ;
#192286 = CARTESIAN_POINT ( 'NONE',  ( 6.883263157960367806, 6.035304072343574688, 2.648703854151325032 ) ) ;
#192287 = CARTESIAN_POINT ( 'NONE',  ( -0.7500000000000006661, 8.958333333333332149, -1.299038105676657340 ) ) ;
#192288 = CARTESIAN_POINT ( 'NONE',  ( 1.242334483997083572, 0.3330332824765611099, 1.692230457194281223 ) ) ;
#192289 = CARTESIAN_POINT ( 'NONE',  ( 6.831329296439236032, 9.063246493969506545, -1.599625672291267398 ) ) ;
#192290 = CARTESIAN_POINT ( 'NONE',  ( 5.367048706163317640, 7.354919138647580290, -1.599625672291281386 ) ) ;
#192291 = CARTESIAN_POINT ( 'NONE',  ( -1.364683531250014514, -0.6989583329919100141, -0.7879004041258359514 ) ) ;
#192292 = CARTESIAN_POINT ( 'NONE',  ( 0.5789240690485557561, 1.654349777479852346, -0.6291145533634836529 ) ) ;
#192293 = CARTESIAN_POINT ( 'NONE',  ( 2.350245942676463695, 0.9471468416194218642, -1.776342852653712168 ) ) ;
#192294 = PRESENTATION_STYLE_ASSIGNMENT (( #91649 ) ) ;
#192296 = VECTOR ( 'NONE', #92930, 1000.000000000000000 ) ;
#192295 = CARTESIAN_POINT ( 'NONE',  ( 3.839080194659278966, 0.3211572903306300075, 2.183152695405643051 ) ) ;
#192297 = CARTESIAN_POINT ( 'NONE',  ( 4.838842012204412235, -2.104300398676747896, -0.5337788192065362480 ) ) ;
#192298 = ORIENTED_EDGE ( 'NONE', *, *, #54326, .F. ) ;
#192299 = CARTESIAN_POINT ( 'NONE',  ( -1.402160292154681736E-14, -0.6624999999999758860, -1.732050807568870754 ) ) ;
#192300 = CARTESIAN_POINT ( 'NONE',  ( 7.076992996209058973, 11.20031622897851165, 1.040834085586084257E-14 ) ) ;
#192302 = CARTESIAN_POINT ( 'NONE',  ( 2.794546173781168541, 1.458544728081469177, -1.392559875802508396 ) ) ;
#192301 = CARTESIAN_POINT ( 'NONE',  ( 3.158948766716848766, 0.5171890032967979556, 2.056314737185329644 ) ) ;
#192304 = ORIENTED_EDGE ( 'NONE', *, *, #27811, .F. ) ;
#192303 = CARTESIAN_POINT ( 'NONE',  ( 3.779414081507098011, 0.2159278537227064809, -1.798573134706340504 ) ) ;
#192305 = CARTESIAN_POINT ( 'NONE',  ( 7.225569521440261767, 7.394528961293920233, -0.7998128361456341429 ) ) ;
#192306 = ORIENTED_EDGE ( 'NONE', *, *, #149140, .F. ) ;
#192307 = CARTESIAN_POINT ( 'NONE',  ( 0.4087956859853311142, 1.625333209436867321, 0.9259686016569528277 ) ) ;
#192308 = CARTESIAN_POINT ( 'NONE',  ( 4.476163270806094552, 8.373940915915776273, 0.7998128361456462443 ) ) ;
#192309 = VECTOR ( 'NONE', #168937, 1000.000000000000000 ) ;
#192310 = CARTESIAN_POINT ( 'NONE',  ( 6.252569598636129378, 0.5776572744066664766, 1.731972519516040032 ) ) ;
#192312 = CARTESIAN_POINT ( 'NONE',  ( 1.006889752881213296, -0.04349654304135543159, 1.915380135637449799 ) ) ;
#192311 = CARTESIAN_POINT ( 'NONE',  ( -2.428882075142555497, 5.985446187641602300, 1.040834085586084257E-14 ) ) ;
#192313 = FACE_OUTER_BOUND ( 'NONE', #79746, .T. ) ;
#192314 = CARTESIAN_POINT ( 'NONE',  ( -0.6823417656250003738, 1.780208333674752952, -1.181850606188749264 ) ) ;
#192315 = CARTESIAN_POINT ( 'NONE',  ( 2.020417662918754687, 3.956598013261175772, -11.36521191596581737 ) ) ;
#192316 = AXIS2_PLACEMENT_3D ( 'NONE', #25070, #91172, #74903 ) ;
#192317 = CARTESIAN_POINT ( 'NONE',  ( 5.506754051192107369, 1.639644015412666800, -1.408845030788405506 ) ) ;
#192318 = CARTESIAN_POINT ( 'NONE',  ( -4.150204419558982671, 7.856005899545188242, 0.7216878364870338292 ) ) ;
#192319 = CARTESIAN_POINT ( 'NONE',  ( -6.912678218121246942, 9.158153569265168770, 1.599625672291269396 ) ) ;
#192320 = CARTESIAN_POINT ( 'NONE',  ( 3.480829117359967917, -1.421471314662653196, 1.573842340227212366 ) ) ;
#192322 = CARTESIAN_POINT ( 'NONE',  ( -11.21412923722849619, 8.995494058042485364, 2.499828665724475485 ) ) ;
#192321 = CARTESIAN_POINT ( 'NONE',  ( -0.1298852118743893114, 2.060165343084968459, -2.144168685196511159 ) ) ;
#192323 = CARTESIAN_POINT ( 'NONE',  ( 4.341064969683814390, -1.716640784620737659, 0.9690559893368445588 ) ) ;
#192324 = CARTESIAN_POINT ( 'NONE',  ( 6.047114369478562956, 0.1942372860762129894, 1.902532258075719351 ) ) ;
#192325 = ORIENTED_EDGE ( 'NONE', *, *, #83669, .F. ) ;
#192326 = CARTESIAN_POINT ( 'NONE',  ( 5.717987565503318770, 1.041469840191568963, -1.843387895306993318 ) ) ;
#192327 = FILL_AREA_STYLE ('',( #140441 ) ) ;
#192328 = CARTESIAN_POINT ( 'NONE',  ( 0.3442982867475213871, -0.9772804826688463731, 1.825211318103404867 ) ) ;
#192329 = CARTESIAN_POINT ( 'NONE',  ( 2.413922445368326564, 1.268163163618090561, -1.470779158573028322 ) ) ;
#192330 = ORIENTED_EDGE ( 'NONE', *, *, #129470, .F. ) ;
#192331 = CARTESIAN_POINT ( 'NONE',  ( 5.773793314573267388, 7.829454515125894964, 1.599625672291268286 ) ) ;
#192332 = CARTESIAN_POINT ( 'NONE',  ( 7.388267364804250725, 7.584343111885245570, -0.7998128361456341429 ) ) ;
#192334 = CARTESIAN_POINT ( 'NONE',  ( 6.765682348419287173, 7.852049813699357728, 1.199719254218462483 ) ) ;
#192333 = CARTESIAN_POINT ( 'NONE',  ( 3.380887635974954453, 1.889918501611790536, -0.8941524261326051493 ) ) ;
#192335 = CARTESIAN_POINT ( 'NONE',  ( 5.194182247366881278, 5.232503174782402233, 0.7216878364870328300 ) ) ;
#192337 = ORIENTED_EDGE ( 'NONE', *, *, #38322, .T. ) ;
#192336 = CARTESIAN_POINT ( 'NONE',  ( 0.9260600326868747567, -0.8135480099433598511, -1.618595788997332363 ) ) ;
#192338 = CARTESIAN_POINT ( 'NONE',  ( 5.391335350415090488, 1.947751002805158560, -1.037606470750504606 ) ) ;
#192339 = CARTESIAN_POINT ( 'NONE',  ( -0.09510031644103759951, -6.698521824825871107, -10.99968117833243042 ) ) ;
#192340 = CARTESIAN_POINT ( 'NONE',  ( 3.382038520680182181, 1.398480293485371284, 1.707083182650385389 ) ) ;
#192341 = CARTESIAN_POINT ( 'NONE',  ( 8.284195553149872993, 9.623648552551724578, -1.199719254218445830 ) ) ;
#192342 = CARTESIAN_POINT ( 'NONE',  ( -1.249999999999964695, 8.500000000000000000, 12.00100000000000122 ) ) ;
#192343 = CARTESIAN_POINT ( 'NONE',  ( 1.436035868020806738, -1.063167577064242142, -1.589284522738307448 ) ) ;
#192344 = CARTESIAN_POINT ( 'NONE',  ( 8.503988664269582998, 10.94440607977979063, 1.599625672291281386 ) ) ;
#192345 = CARTESIAN_POINT ( 'NONE',  ( 4.773920332862017446, -2.031068740936771366, 0.4005940302675218834 ) ) ;
#192347 = CARTESIAN_POINT ( 'NONE',  ( 2.782270202741622178, -1.112240752214749273, 1.853481441253836071 ) ) ;
#192346 = CARTESIAN_POINT ( 'NONE',  ( 9.622669940282555956, -9.063128755109502777, -0.5283818209470574345 ) ) ;
#192348 = CARTESIAN_POINT ( 'NONE',  ( 4.616832073239669043, -0.1072513232249286408, 2.189039617437993357 ) ) ;
#192349 = VERTEX_POINT ( 'NONE', #133643 ) ;
#192350 = DIRECTION ( 'NONE',  ( 0.9632918427306580433, 0.000000000000000000, 0.2684563758389303945 ) ) ;
#192351 = CARTESIAN_POINT ( 'NONE',  ( 6.115103934187892776, 6.015625209457229339, 1.345820777640227805E-10 ) ) ;
#192352 = CARTESIAN_POINT ( 'NONE',  ( 0.4019237886466850984, 12.92633545031536713, -1.499999999999996669 ) ) ;
#192353 = EDGE_CURVE ( 'NONE', #127623, #126977, #100037, .T. ) ;
#192354 = CARTESIAN_POINT ( 'NONE',  ( 3.386504508363381571, 7.172948703057747011, -0.7998128361456362523 ) ) ;
#192355 = CARTESIAN_POINT ( 'NONE',  ( 0.000000000000000000, 0.9000000000000014655, 0.000000000000000000 ) ) ;
#192356 = CARTESIAN_POINT ( 'NONE',  ( -3.383641855062333281, 6.105276709951447778, -1.199719254218452047 ) ) ;
#192357 = CARTESIAN_POINT ( 'NONE',  ( -7.836249599018719536, 12.08611559892311504, 0.7216878364870478180 ) ) ;
#192358 = CARTESIAN_POINT ( 'NONE',  ( 5.468734858265785093, 7.473552982767158070, 1.599625672291269396 ) ) ;
#192359 = CARTESIAN_POINT ( 'NONE',  ( 5.805552407531882508, -1.628464769346991581, -1.278160613847306504 ) ) ;
#192360 = CARTESIAN_POINT ( 'NONE',  ( 4.740804336882096237, 0.3310356755545171836, 1.897698676112127725 ) ) ;
#192361 = CARTESIAN_POINT ( 'NONE',  ( 6.327753876788817955, 0.8101538176374730726, -1.956283944203747849 ) ) ;
#192362 = CARTESIAN_POINT ( 'NONE',  ( 4.985647801523278133, 6.839675073242382553, -1.599625672291256295 ) ) ;
#192363 = CARTESIAN_POINT ( 'NONE',  ( 1.749999999999999778, 0.000000000000000000, 0.000000000000000000 ) ) ;
#192364 = CARTESIAN_POINT ( 'NONE',  ( 4.821133434317745881, -1.757446901322982979, -0.8890814742016742711 ) ) ;
#192365 = CARTESIAN_POINT ( 'NONE',  ( 0.6565081633774123571, -1.584678946828571133, 1.513927167823600595 ) ) ;
#192366 = CARTESIAN_POINT ( 'NONE',  ( 3.809063337113669068, 1.566667275063510445, 0.9371452329686792426 ) ) ;
#192367 = B_SPLINE_CURVE_WITH_KNOTS ( 'NONE', 3,
 ( #205937, #159327, #22900, #10924, #76999, #173476, #58632, #155069, #124785, #190745, #158280, #9870, #6658, #28264 ),
 .UNSPECIFIED., .F., .F.,
 ( 4, 2, 2, 2, 2, 2, 4 ),
 ( 0.5000508295171147699, 0.5622958969969490406, 0.6245409644767833113, 0.6556634982167006687, 0.6867860319566181371, 0.7179085656965356055, 0.7490310994364531849 ),
 .UNSPECIFIED. ) ;
#192368 = PRODUCT ( 'sphere', 'sphere', '', ( #202001 ) ) ;
#192369 = ADVANCED_FACE ( 'NONE', ( #148787 ), #201771, .T. ) ;
#192370 = CARTESIAN_POINT ( 'NONE',  ( 7.512626515748113576, 7.937354821227203594, 0.7216878364870267237 ) ) ;
#192371 = CARTESIAN_POINT ( 'NONE',  ( 3.348500752450942031, 4.929670182657964084, 1.443375672974066548 ) ) ;
#192372 = CARTESIAN_POINT ( 'NONE',  ( -6.607619761813764647, 8.802252036906432764, 1.599625672291269396 ) ) ;
#192373 = CARTESIAN_POINT ( 'NONE',  ( 6.052789233858158369, 6.026285292448116948, 0.000000000000000000 ) ) ;
#192374 =( BOUNDED_SURFACE ( )  B_SPLINE_SURFACE ( 3, 3, ( 
 ( #148075, #118818, #147022, #33240, #66768, #31132, #97207, #34301, #99323, #67838, #116681 ),
 ( #80931, #165373, #132909, #14841, #85188, #133984, #131856, #117764, #213045, #51640, #167513 ),
 ( #114567, #115616, #16966, #2844, #100374, #163259, #196811, #48454, #84123, #166444, #19110 ),
 ( #198914, #183754, #35364, #135033, #101439, #18036, #151271, #201046, #83047, #52689, #180559 ),
 ( #32181, #149122, #15905, #214081, #704, #197863, #170706, #72121, #36434, #43671, #186950 ),
 ( #87330, #11127, #137162, #73191, #203186, #138229, #55894, #54832, #56963, #23374, #154472 ),
 ( #185872, #153397, #69977, #60964, #77205, #53765, #3907, #155539, #89484, #71046, #184805 ) ),
 .UNSPECIFIED., .T., .F., .T. ) 
 B_SPLINE_SURFACE_WITH_KNOTS ( ( 4, 3, 4 ),
 ( 4, 1, 1, 1, 1, 1, 1, 1, 4 ),
 ( 0.000000000000000000, 0.5000000000000000000, 1.000000000000000000 ),
 ( 0.000000000000000000, 0.2255619619413396781, 0.3975297875667437308, 0.5250373104567740423, 0.6172314665434700531, 0.6832587661106447330, 0.7322037845459880012, 0.7729093456892226488, 1.000000000000000000 ),
 .UNSPECIFIED. ) 
 GEOMETRIC_REPRESENTATION_ITEM ( )  RATIONAL_B_SPLINE_SURFACE ( (
 ( 1.000000000000000000, 1.000000000000000000, 1.000000000000000444, 0.9999999999999996669, 1.000000000000000222, 0.9999999999999996669, 1.000000000000000444, 1.000000000000000000, 1.000000000000000000, 1.000000000000000000, 1.000000000000000000),
 ( 0.3333333333333333703, 0.3333333333333333703, 0.3333333333333334814, 0.3333333333333332038, 0.3333333333333333703, 0.3333333333333332593, 0.3333333333333334814, 0.3333333333333333703, 0.3333333333333334814, 0.3333333333333333703, 0.3333333333333333703),
 ( 0.3333333333333333703, 0.3333333333333333703, 0.3333333333333334814, 0.3333333333333332038, 0.3333333333333333703, 0.3333333333333332593, 0.3333333333333334814, 0.3333333333333333703, 0.3333333333333334814, 0.3333333333333333703, 0.3333333333333333703),
 ( 1.000000000000000000, 1.000000000000000000, 1.000000000000000444, 0.9999999999999996669, 1.000000000000000222, 0.9999999999999996669, 1.000000000000000444, 1.000000000000000000, 1.000000000000000000, 1.000000000000000000, 1.000000000000000000),
 ( 0.3333333333333333703, 0.3333333333333333703, 0.3333333333333334814, 0.3333333333333332038, 0.3333333333333333703, 0.3333333333333332593, 0.3333333333333334814, 0.3333333333333333703, 0.3333333333333334814, 0.3333333333333333703, 0.3333333333333333703),
 ( 0.3333333333333333703, 0.3333333333333333703, 0.3333333333333334814, 0.3333333333333332038, 0.3333333333333333703, 0.3333333333333332593, 0.3333333333333334814, 0.3333333333333333703, 0.3333333333333334814, 0.3333333333333333703, 0.3333333333333333703),
 ( 1.000000000000000000, 1.000000000000000000, 1.000000000000000444, 0.9999999999999996669, 1.000000000000000222, 0.9999999999999996669, 1.000000000000000444, 1.000000000000000000, 1.000000000000000000, 1.000000000000000000, 1.000000000000000000) ) ) 
 REPRESENTATION_ITEM ( '' )  SURFACE ( )  );
#192375 = ORIENTED_EDGE ( 'NONE', *, *, #179088, .T. ) ;
#192377 = CARTESIAN_POINT ( 'NONE',  ( 5.115494517658178530, 1.648350763777502559, 1.155591226287083328 ) ) ;
#192376 = CARTESIAN_POINT ( 'NONE',  ( 3.175182228840720988, 1.170341537027960843, 1.421418621496411516 ) ) ;
#192378 = CARTESIAN_POINT ( 'NONE',  ( 0.9490539546192258147, 1.544862702020805223, 1.701928257493188434 ) ) ;
#192379 = CARTESIAN_POINT ( 'NONE',  ( 5.647302737930705696, 1.731814717071546772, -0.9215059220915235993 ) ) ;
#192380 = CARTESIAN_POINT ( 'NONE',  ( -6.338600509588822263, 7.353787668397130162, -1.199719254218446718 ) ) ;
#192381 = CARTESIAN_POINT ( 'NONE',  ( 10.66594405399933976, -7.024005795609692626, -0.4637852190794419793 ) ) ;
#192382 = PRESENTATION_LAYER_ASSIGNMENT (  '', '', ( #119793 ) ) ;
#192383 = CARTESIAN_POINT ( 'NONE',  ( -4.322352044658376968, 3.937165561723182883, 0.7998128361456341429 ) ) ;
#192384 = CARTESIAN_POINT ( 'NONE',  ( 0.5552397518338060278, 1.722184604005328357, -1.148819969904082861 ) ) ;
#192385 = CARTESIAN_POINT ( 'NONE',  ( -5.646044625448194410, 5.551749915969804938, 0.000000000000000000 ) ) ;
#192387 = CARTESIAN_POINT ( 'NONE',  ( 0.2505829665140328899, -1.505242420826727656, 1.110479572284161831 ) ) ;
#192386 = CARTESIAN_POINT ( 'NONE',  ( 1.153981415136243527, 0.8505622500237058903, 1.910110313709513674 ) ) ;
#192388 = CARTESIAN_POINT ( 'NONE',  ( 0.1501718367240000573, 8.265200931437560072, -1.995665264648831316 ) ) ;
#192389 = CARTESIAN_POINT ( 'NONE',  ( -0.1104750535120268551, 0.2303756098476944791, -2.137063993957021513 ) ) ;
#192390 = CARTESIAN_POINT ( 'NONE',  ( 1.962089020239773163, -1.591546648218734816, -0.7047476087739585893 ) ) ;
#192391 = CARTESIAN_POINT ( 'NONE',  ( 6.647575389402066826, 6.649926130590872120, 1.040834085586084257E-14 ) ) ;
#192393 = CARTESIAN_POINT ( 'NONE',  ( 1.567404983201064139, 8.684828555514158666, 2.500997594616644726 ) ) ;
#192392 = DIRECTION ( 'NONE',  ( -1.224646799147353207E-16, 1.000000000000000000, 0.000000000000000000 ) ) ;
#192394 = CARTESIAN_POINT ( 'NONE',  ( 2.982692045960423588, -0.1271664282922572997, -1.720251185527998272 ) ) ;
#192395 = CARTESIAN_POINT ( 'NONE',  ( 2.296645709751913955, 1.758124065145909798, -1.308193547052277861 ) ) ;
#192396 = CARTESIAN_POINT ( 'NONE',  ( 5.373716497573798101, 2.127666891504222058, -0.5857064233696291922 ) ) ;
#192397 = CARTESIAN_POINT ( 'NONE',  ( -9.409940793360268785, 3.999985931113709814, -6.919963696468023784 ) ) ;
#192398 = CARTESIAN_POINT ( 'NONE',  ( 3.045941508711128787, 1.532170317875800603, 1.538426465386952380 ) ) ;
#192399 = CARTESIAN_POINT ( 'NONE',  ( 0.6447967512687136082, -1.567379569643694515, 0.9359695128687425258 ) ) ;
#192400 = CARTESIAN_POINT ( 'NONE',  ( 3.063770578283632862, 1.346675374253442969, 1.633852266970806211 ) ) ;
#192401 = CARTESIAN_POINT ( 'NONE',  ( 6.539320575229250032, 3.707580029678263944, 2.311356139567366963 ) ) ;
#192402 = EDGE_CURVE ( 'NONE', #3975, #11745, #112731, .T. ) ;
#192403 = ORIENTED_EDGE ( 'NONE', *, *, #176945, .F. ) ;
#192405 = CARTESIAN_POINT ( 'NONE',  ( -1.364683531250000748, 1.071875000341421247, 0.000000000000000000 ) ) ;
#192404 = CARTESIAN_POINT ( 'NONE',  ( 3.456809812625420975, -2.022294432149398080, -1.079448172897869540 ) ) ;
#192406 = CARTESIAN_POINT ( 'NONE',  ( 0.6124999999999914957, 2.583333333333347248, 1.060881119635894487 ) ) ;
#192407 = CARTESIAN_POINT ( 'NONE',  ( 3.948449050077836642, 5.629609863222681199, 1.599625672291267398 ) ) ;
#192408 = CARTESIAN_POINT ( 'NONE',  ( 6.410783699188008278, -0.5891560598917375824, -2.141663135048486044 ) ) ;
#192409 = CARTESIAN_POINT ( 'NONE',  ( -5.572037945536512105, 9.444535336527177805, 0.000000000000000000 ) ) ;
#192410 = CIRCLE ( 'NONE', #92117, 0.7500000000000011102 ) ;
#192411 = CARTESIAN_POINT ( 'NONE',  ( 3.050221373394638835, 6.502416002361635528, 0.000000000000000000 ) ) ;
#192412 = CARTESIAN_POINT ( 'NONE',  ( -6.521108698048779573, 8.631046119188804155, -1.443375672974058777 ) ) ;
#192413 = CARTESIAN_POINT ( 'NONE',  ( 3.445180431648323882, 6.073108699348104267, 1.082531754730549078 ) ) ;
#192414 = ORIENTED_EDGE ( 'NONE', *, *, #118482, .T. ) ;
#192415 = CARTESIAN_POINT ( 'NONE',  ( 4.166638809851969327, 1.319227567334404494, 1.525044649537968589 ) ) ;
#192417 = CARTESIAN_POINT ( 'NONE',  ( 1.674751860914457824, 1.388166878297650397, -1.525640323027994683 ) ) ;
#192416 = CARTESIAN_POINT ( 'NONE',  ( 4.625302960556422427, 8.547937220624488575, 1.040834085586084257E-14 ) ) ;
#192418 = CARTESIAN_POINT ( 'NONE',  ( 0.07538891330674882263, -7.154544010627095219, -9.499700864329891914 ) ) ;
#192419 = EDGE_CURVE ( 'NONE', #7565, #123335, #195696, .T. ) ;
#192420 = CARTESIAN_POINT ( 'NONE',  ( 6.556249800660121529, 9.806652646482286073, 1.199719254218452047 ) ) ;
#192421 = CARTESIAN_POINT ( 'NONE',  ( 1.642778471875001811, -3.142708332855375986, 2.845375778867859751 ) ) ;
#192422 = CARTESIAN_POINT ( 'NONE',  ( 0.6823417656249917140, 4.592708333674755394, 1.181850606188765695 ) ) ;
#192423 = CARTESIAN_POINT ( 'NONE',  ( 4.804715953495782621, 1.905792977913090214, 1.081705336968781239 ) ) ;
#192424 = CARTESIAN_POINT ( 'NONE',  ( 2.637342451166882373, 0.6819965276749391236, 1.897697610567940174 ) ) ;
#192425 = CARTESIAN_POINT ( 'NONE',  ( 2.278628554356322500, 1.682734121078124812, -0.7478279864501293783 ) ) ;
#192426 = CARTESIAN_POINT ( 'NONE',  ( 5.784525094524856748, 9.900363043587685041, 1.040834085586084257E-14 ) ) ;
#192427 = CARTESIAN_POINT ( 'NONE',  ( 5.948246703923279810, 1.823645139926059144, 0.08696428134234018836 ) ) ;
#192428 = CARTESIAN_POINT ( 'NONE',  ( -6.307567778855718288, 8.381915046796901692, -1.599625672291263179 ) ) ;
#192430 = CARTESIAN_POINT ( 'NONE',  ( -4.899292406491858820, 6.809203455697518947, -1.599625672291271394 ) ) ;
#192429 = CARTESIAN_POINT ( 'NONE',  ( 6.262609139476608355, -1.605266756365858027, 1.594658822776671592 ) ) ;
#192431 = CARTESIAN_POINT ( 'NONE',  ( 1.858176280533967661, 2.100347624109857758, -0.1560452747076390423 ) ) ;
#192432 = CARTESIAN_POINT ( 'NONE',  ( -4.613517410400161722, 8.604463755433990002, -0.7998128361456362523 ) ) ;
#192433 = CARTESIAN_POINT ( 'NONE',  ( 9.074484886248265880, 9.481320543578137361, 0.7998128361456462443 ) ) ;
#192434 = CARTESIAN_POINT ( 'NONE',  ( 6.143253000323500856, 10.18122924377050609, -0.7216878364870458196 ) ) ;
#192435 = CARTESIAN_POINT ( 'NONE',  ( 8.360351495551780587, 25.13067396371874196, 15.76748856390591058 ) ) ;
#192436 = CARTESIAN_POINT ( 'NONE',  ( -6.028571859570855729, 10.18508426947466816, 0.000000000000000000 ) ) ;
#192437 = UNCERTAINTY_MEASURE_WITH_UNIT (LENGTH_MEASURE( 1.000000000000000082E-05 ), #50885, 'distance_accuracy_value', 'NONE');
#192438 = CARTESIAN_POINT ( 'NONE',  ( 2.998324526916512411, 6.649795714711241423, 0.000000000000000000 ) ) ;
#192439 = CARTESIAN_POINT ( 'NONE',  ( 8.093854517234030155, 8.545177812968924869, -0.7216878364870267237 ) ) ;
#192440 = CARTESIAN_POINT ( 'NONE',  ( 4.221210552267129046, 7.311159377000789661, -0.8807526815687096722 ) ) ;
#192441 = CARTESIAN_POINT ( 'NONE',  ( -8.188761592974033832, 12.49737959187099179, -0.7216878364870267237 ) ) ;
#192443 = CARTESIAN_POINT ( 'NONE',  ( 2.900855728284880808, -2.189247779298031826, -0.3757519495388698672 ) ) ;
#192442 = CARTESIAN_POINT ( 'NONE',  ( 1.424255164902767934, -2.103954720533041556, 0.2648648325892372646 ) ) ;
#192444 = CARTESIAN_POINT ( 'NONE',  ( 0.6455096168876961471, -1.890800792967793686, 1.137844069391671820 ) ) ;
#192445 = CARTESIAN_POINT ( 'NONE',  ( -4.990283058281743678, 7.979691447040783814, -1.199719254218453823 ) ) ;
#192446 = CARTESIAN_POINT ( 'NONE',  ( 4.904298879841284098, 6.744767997946721216, 1.599625672291267398 ) ) ;
#192447 = CARTESIAN_POINT ( 'NONE',  ( 4.668382477721988444, -0.8370036265390871089, -1.774476930476886594 ) ) ;
#192448 = CARTESIAN_POINT ( 'NONE',  ( 9.402743226277308963, 10.92862083786708816, -1.199719254218446718 ) ) ;
#192449 = CARTESIAN_POINT ( 'NONE',  ( -5.108350220830032207, 6.531958715577594887, 1.215759808322430136 ) ) ;
#192450 = CARTESIAN_POINT ( 'NONE',  ( 3.277320446201373638, 4.846626492033466072, 1.599625672291267398 ) ) ;
#192451 = CARTESIAN_POINT ( 'NONE',  ( 1.364683531249986537, 0.9052083336747533959, -0.7879004041258239610 ) ) ;
#192452 = CARTESIAN_POINT ( 'NONE',  ( -6.143253000767895600, 6.339752387083549934, 0.000000000000000000 ) ) ;
#192454 = CARTESIAN_POINT ( 'NONE',  ( -6.060131475628484310, 10.01397778830115470, 0.000000000000000000 ) ) ;
#192453 = AXIS2_PLACEMENT_3D ( 'NONE', #44511, #110628, #176629 ) ;
#192455 = CARTESIAN_POINT ( 'NONE',  ( 3.586284538990120119, 1.181046903802231984, 1.761068336431830472 ) ) ;
#192456 = CARTESIAN_POINT ( 'NONE',  ( -6.147696309153835692, 6.137010213626392208, 0.7998128361456281477 ) ) ;
#192457 = CARTESIAN_POINT ( 'NONE',  ( 4.540002997438313592, 0.9271085556134452954, -1.952944755896801610 ) ) ;
#192458 = CARTESIAN_POINT ( 'NONE',  ( 4.212339636135824961, 1.685202893791247769, 0.7422218904534692019 ) ) ;
#192459 = CARTESIAN_POINT ( 'NONE',  ( -4.552667031389123764, 6.999162803142576550, 1.172958579310765970 ) ) ;
#192460 = CARTESIAN_POINT ( 'NONE',  ( -1.364683531250014514, 0.3427083336747508424, 0.7879004041258379498 ) ) ;
#192461 = B_SPLINE_CURVE_WITH_KNOTS ( 'NONE', 3,
 ( #148118, #181652, #20217, #136136, #151317, #202152, #67879, #50598 ),
 .UNSPECIFIED., .F., .F.,
 ( 4, 2, 2, 4 ),
 ( 5.963111948670136683E-19, 0.0002224730689913816681, 0.0004449461379827627399, 0.0008898922759655248293 ),
 .UNSPECIFIED. ) ;
#192462 = CARTESIAN_POINT ( 'NONE',  ( 5.648340061037051107, -1.368025295233719074, 1.075653158840290891 ) ) ;
#192463 = CARTESIAN_POINT ( 'NONE',  ( 0.02684197942426417779, 14.48154074394417812, 12.00000000000000178 ) ) ;
#192464 = CARTESIAN_POINT ( 'NONE',  ( 3.633221978782282147, 5.261844946711204507, -1.443375672974057666 ) ) ;
#192465 = CARTESIAN_POINT ( 'NONE',  ( -1.115562610750309283E-14, 11.81249999999999822, 1.500000000000001554 ) ) ;
#192466 = AXIS2_PLACEMENT_3D ( 'NONE', #121216, #6286, #73434 ) ;
#192467 = CARTESIAN_POINT ( 'NONE',  ( 2.940462584922590938, 2.145230175562794717, 0.2658940370997217584 ) ) ;
#192468 = CARTESIAN_POINT ( 'NONE',  ( 5.993517489292202960, 1.942244631591660164, 0.5404061186519912852 ) ) ;
#192469 = CARTESIAN_POINT ( 'NONE',  ( -6.683806541412756985, 10.74159869838281622, -0.7216878364870267237 ) ) ;
#192470 = CARTESIAN_POINT ( 'NONE',  ( 2.290102563249151402, -0.9248296759884739870, 1.954025333243500917 ) ) ;
#192471 = CARTESIAN_POINT ( 'NONE',  ( 4.288322324034578692, -1.949444798393678013, -0.2924651067536877536 ) ) ;
#192472 = CARTESIAN_POINT ( 'NONE',  ( 0.02921319935947005314, -2.001080581411585513, 0.8940957790435491992 ) ) ;
#192473 = CARTESIAN_POINT ( 'NONE',  ( 0.08353690965077953390, -0.1615750995121113531, -2.271551823106517709 ) ) ;
#192474 = CARTESIAN_POINT ( 'NONE',  ( 4.388185931656235717, -0.4287674410733510744, -1.893983405979382306 ) ) ;
#192476 = ORIENTED_EDGE ( 'NONE', *, *, #145827, .F. ) ;
#192475 = CARTESIAN_POINT ( 'NONE',  ( -9.937763408692600109, 10.69640485300394417, -0.7216878364870267237 ) ) ;
#192477 = AXIS2_PLACEMENT_3D ( 'NONE', #11545, #147962, #212932 ) ;
#192478 = CARTESIAN_POINT ( 'NONE',  ( -5.447343857640614573, 9.577261277214532242, -0.7998128361456362523 ) ) ;
#192479 = CARTESIAN_POINT ( 'NONE',  ( 11.91826849282518275, 10.19999999999998153, 1.399999999999998579 ) ) ;
#192481 = VERTEX_POINT ( 'NONE', #20883 ) ;
#192480 = CARTESIAN_POINT ( 'NONE',  ( -4.573896719763875574, 6.429575154514868274, -1.599625672291271394 ) ) ;
#192482 = CARTESIAN_POINT ( 'NONE',  ( -7.985389288324692636, 11.29974268881207067, -1.082531754730543083 ) ) ;
#192483 = CARTESIAN_POINT ( 'NONE',  ( 2.643839551151895506, -1.634601560588926361, -1.482707865360691990 ) ) ;
#192484 = CARTESIAN_POINT ( 'NONE',  ( -3.285556943749998737, -2.530208332855374831, 1.896917185911908499 ) ) ;
#192485 = CARTESIAN_POINT ( 'NONE',  ( 6.473494419632052299, -0.2434444386649399217, 1.946554233954982172 ) ) ;
#192486 = CARTESIAN_POINT ( 'NONE',  ( -1.201851678989727383E-14, 5.759375000341417028, -1.575800808251660801 ) ) ;
#192487 = CARTESIAN_POINT ( 'NONE',  ( 1.499999999999987121, 3.827083334016153415, -0.8660254037844323793 ) ) ;
#192488 = CARTESIAN_POINT ( 'NONE',  ( 4.860569815253008130, 6.917139861862701800, -1.418536646215622365 ) ) ;
#192490 = CARTESIAN_POINT ( 'NONE',  ( 0.000000000000000000, 0.7999999999999951594, -11.50000000000000000 ) ) ;
#192489 = FACE_OUTER_BOUND ( 'NONE', #190624, .T. ) ;
#192491 = CARTESIAN_POINT ( 'NONE',  ( 5.701068745948241201, -0.4431999317857804876, 1.786873912291174538 ) ) ;
#192492 = ORIENTED_EDGE ( 'NONE', *, *, #122876, .F. ) ;
#192493 = CARTESIAN_POINT ( 'NONE',  ( -1.360316468750034868, -0.3385416663252556191, 0.7853790794158601596 ) ) ;
#192494 = CARTESIAN_POINT ( 'NONE',  ( -7.588813295347149435, 9.876701482703580837, -1.599625672291263179 ) ) ;
#192495 = CARTESIAN_POINT ( 'NONE',  ( -1.192422653747474470, -9.167912422188539046E-15, 0.4243420385968842967 ) ) ;
#192497 = ADVANCED_FACE ( 'NONE', ( #38236 ), #60858, .T. ) ;
#192496 = CARTESIAN_POINT ( 'NONE',  ( 5.976833544478475702, -1.498421880457675215, 1.500811427713820478 ) ) ;
#192498 = CARTESIAN_POINT ( 'NONE',  ( -2.609770642201835855, -0.3830433331901521576, -0.1872689674646474400 ) ) ;
#192499 = CARTESIAN_POINT ( 'NONE',  ( 5.660692828905515839, 6.562895374266609849, -1.199719254218445830 ) ) ;
#192500 = CARTESIAN_POINT ( 'NONE',  ( 6.626252497008212394, 1.190392663088507552, -1.681986249806742384 ) ) ;
#192503 = CARTESIAN_POINT ( 'NONE',  ( 4.388128076750056117, -0.4078595375654435751, -1.795341762384855544 ) ) ;
#192502 = CARTESIAN_POINT ( 'NONE',  ( 2.435812105726247623, 1.142245297582837882, 1.469210208790121763 ) ) ;
#192501 = DIRECTION ( 'NONE',  ( 8.638326563840814399E-31, 0.000000000000000000, 1.000000000000000000 ) ) ;
#192504 = CARTESIAN_POINT ( 'NONE',  ( 6.272618624616828953, 10.46980549536166016, 1.040834085586084257E-14 ) ) ;
#192505 = CARTESIAN_POINT ( 'NONE',  ( -9.367496997601861608, 14.53091781611221833, -7.499999999994731326 ) ) ;
#192506 = CARTESIAN_POINT ( 'NONE',  ( -7.930593509350902792, 8.217056947189661287, -0.7998128361456362523 ) ) ;
#192508 = ORIENTED_EDGE ( 'NONE', *, *, #87121, .T. ) ;
#192507 = CARTESIAN_POINT ( 'NONE',  ( 3.621833129746810265, 4.096114899008192367, 2.500000000000023093 ) ) ;
#192509 = CARTESIAN_POINT ( 'NONE',  ( 4.108205984530819421, -2.201057848371779535, 0.1611738814469021175 ) ) ;
#192510 = CARTESIAN_POINT ( 'NONE',  ( 5.641944544108610238, 0.9243782401199867049, -2.065144452299176425 ) ) ;
#192511 = CARTESIAN_POINT ( 'NONE',  ( -4.934804725694212912, 8.701096580044490381, -0.7216878364870207285 ) ) ;
#192512 = CARTESIAN_POINT ( 'NONE',  ( 6.205303291940151844, 1.571521137685438108, -0.9011181087926769528 ) ) ;
#192513 = CARTESIAN_POINT ( 'NONE',  ( -0.04763828917917976857, -1.313539345393003321, 1.530161206715647149 ) ) ;
#192514 = FACE_OUTER_BOUND ( 'NONE', #97530, .T. ) ;
#192515 = CARTESIAN_POINT ( 'NONE',  ( 8.731294531955244409, 14.92342541429118263, -8.233198443303315628 ) ) ;
#192516 = CARTESIAN_POINT ( 'NONE',  ( 6.024064539286675846, -1.897261554996135802, 0.2387622092476364699 ) ) ;
#192517 = CARTESIAN_POINT ( 'NONE',  ( 4.030162213014739869, 7.767662802593035209, -0.3896624696924297360 ) ) ;
#192518 = CARTESIAN_POINT ( 'NONE',  ( 1.199835987674138460, -1.870836310881810682, -0.003643258294119822160 ) ) ;
#192519 = CARTESIAN_POINT ( 'NONE',  ( 0.8664231474371618669, -1.968446048378743152, -0.4370742218882398000 ) ) ;
#192521 = CARTESIAN_POINT ( 'NONE',  ( 3.492891347888595455, -0.4109570828031941514, -2.065403110348571492 ) ) ;
#192520 = CARTESIAN_POINT ( 'NONE',  ( -10.34217224912604571, 10.96028913360221502, 0.7998128361456462443 ) ) ;
#192522 = CARTESIAN_POINT ( 'NONE',  ( 9.921869487102386032, 10.46993591124128997, 0.000000000000000000 ) ) ;
#192524 = CARTESIAN_POINT ( 'NONE',  ( -8.015895134177625891, 10.37496362800581018, 1.599625672291295375 ) ) ;
#192523 = CARTESIAN_POINT ( 'NONE',  ( -0.7500000000000249800, -0.8083333333333136972, 1.299038105676659116 ) ) ;
#192525 = CARTESIAN_POINT ( 'NONE',  ( 11.52483635780546045, 9.720000086424631647, 3.345866325258041840 ) ) ;
#192526 = CARTESIAN_POINT ( 'NONE',  ( 2.847920605731304011, -1.359688658692468355, -1.493726022120341224 ) ) ;
#192527 = CARTESIAN_POINT ( 'NONE',  ( -1.364683531250012516, 3.988541667008088876, -0.7879004041258300672 ) ) ;
#192528 = CARTESIAN_POINT ( 'NONE',  ( 2.361091307074211887, 5.906356958228550447, 0.7998128361456462443 ) ) ;
#192529 = CARTESIAN_POINT ( 'NONE',  ( 4.604844690042746436, 1.674155836469687575, -1.367402732809947397 ) ) ;
#192530 = CARTESIAN_POINT ( 'NONE',  ( -0.9311234436981480345, -1.778119629485602537, -3.475000000000001421 ) ) ;
#192531 = CARTESIAN_POINT ( 'NONE',  ( -0.7499999999999972244, 5.108333333333353821, -1.299038105676652011 ) ) ;
#192533 = CARTESIAN_POINT ( 'NONE',  ( -9.603221262331047114, -9.439766061754902182, 0.1988025308400011015 ) ) ;
#192532 = CARTESIAN_POINT ( 'NONE',  ( 7.018280793729500644, 8.217024343219755167, -1.199719254218452047 ) ) ;
#192534 = CARTESIAN_POINT ( 'NONE',  ( 8.880227426826641235, 10.42298208846167284, 1.082531754730549967 ) ) ;
#192536 = CARTESIAN_POINT ( 'NONE',  ( 8.674533818622323977, 14.86056906971758096, -8.228093639940686543 ) ) ;
#192535 = CARTESIAN_POINT ( 'NONE',  ( 1.381551413260760031, -0.05389312200515179035, 2.170675147484208534 ) ) ;
#192538 = CARTESIAN_POINT ( 'NONE',  ( 0.4328342922346357646, -1.301571265828086688, -1.302605208699902928 ) ) ;
#192537 = CARTESIAN_POINT ( 'NONE',  ( -6.900736999675794792, 7.153207375817628666, 1.040834085586084257E-14 ) ) ;
#192539 = CARTESIAN_POINT ( 'NONE',  ( 1.364683531249986537, 1.905208333674750287, -0.7879004041258239610 ) ) ;
#192541 = CARTESIAN_POINT ( 'NONE',  ( 1.839652601550560096, 0.8350199954420146620, -2.026445374841173930 ) ) ;
#192540 = B_SPLINE_CURVE_WITH_KNOTS ( 'NONE', 3,
 ( #107735, #25337, #9094, #75170, #141280, #207288, #132488, #146597, #67409, #196388 ),
 .UNSPECIFIED., .F., .F.,
 ( 4, 3, 3, 4 ),
 ( 0.000000000000000000, 4.502046072369090049E-05, 9.004093402560593489E-05, 0.0001800865003196811486 ),
 .UNSPECIFIED. ) ;
#192542 = CARTESIAN_POINT ( 'NONE',  ( 6.517945676554362855, 6.748686274690250286, -0.003863832781672048907 ) ) ;
#192543 = CARTESIAN_POINT ( 'NONE',  ( 2.659333574217698004, -1.968172486592324244, -1.115815620033432154 ) ) ;
#192544 = CARTESIAN_POINT ( 'NONE',  ( -5.520141099058386125, 9.591915048876776595, 0.000000000000000000 ) ) ;
#192545 = CARTESIAN_POINT ( 'NONE',  ( 1.364683531249990311, 4.446875000341417028, 1.214306433183764966E-14 ) ) ;
#192546 = CARTESIAN_POINT ( 'NONE',  ( 5.176795123377851304, 7.746134302493202561, 1.185296789734613387 ) ) ;
#192547 = CARTESIAN_POINT ( 'NONE',  ( 1.500000000000001332, 11.87499999999999645, 0.000000000000000000 ) ) ;
#192548 = CARTESIAN_POINT ( 'NONE',  ( 6.156811154381533591, 9.236677875870187293, -1.082531754730548412 ) ) ;
#192549 = CARTESIAN_POINT ( 'NONE',  ( 4.059615542810626643, 1.756569389245852042, -0.2146349482602862846 ) ) ;
#192550 = CARTESIAN_POINT ( 'NONE',  ( 7.411503528164766763, 11.79850454950093841, 1.040834085586084257E-14 ) ) ;
#192551 = CARTESIAN_POINT ( 'NONE',  ( 1.272647984039422697, -1.336331724779236119, 1.627640044824183674 ) ) ;
#192553 = CARTESIAN_POINT ( 'NONE',  ( 1.499999999999989120, 0.7750000000000187850, 0.000000000000000000 ) ) ;
#192552 = CARTESIAN_POINT ( 'NONE',  ( 1.364683531250000303, 10.00520833367473017, -0.7879004041258355073 ) ) ;
#192554 = CARTESIAN_POINT ( 'NONE',  ( -5.581116510680924847, 6.540332679663050541, -1.199719254218453823 ) ) ;
#192555 = CARTESIAN_POINT ( 'NONE',  ( 6.134388704033759687, 0.6352148712998658686, 1.913799669303432927 ) ) ;
#192556 = VERTEX_POINT ( 'NONE', #69639 ) ;
#192557 = ADVANCED_FACE ( 'NONE', ( #202839 ), #182333, .F. ) ;
#192558 = CARTESIAN_POINT ( 'NONE',  ( 7.899597058256738968, 12.36794700127490820, 1.040834085586084257E-14 ) ) ;
#192560 = CARTESIAN_POINT ( 'NONE',  ( 4.047608660086319254, 0.6306619223146043840, -1.761260876548931709 ) ) ;
#192559 = AXIS2_PLACEMENT_3D ( 'NONE', #75519, #123302, #23545 ) ;
#192561 = CARTESIAN_POINT ( 'NONE',  ( 4.961816271168415504, -0.5573412460852051886, 1.993729458732765858 ) ) ;
#192562 = CARTESIAN_POINT ( 'NONE',  ( -4.950135482320914271, 8.789258806100786359, -0.7216878364870338292 ) ) ;
#192563 = VECTOR ( 'NONE', #19487, 1000.000000000000000 ) ;
#192564 = CARTESIAN_POINT ( 'NONE',  ( -9.480175724453545172, 12.08329098332774265, 1.599625672291281386 ) ) ;
#192565 = CARTESIAN_POINT ( 'NONE',  ( 5.643937085038755797, 9.806620042512378177, -0.7998128361456481317 ) ) ;
#192567 = CARTESIAN_POINT ( 'NONE',  ( -5.683421429784462298, 6.045756166660654074, -0.6295853902834018800 ) ) ;
#192566 = B_SPLINE_CURVE_WITH_KNOTS ( 'NONE', 3,
 ( #146314, #162551, #181963, #61838, #97557, #95438, #66060, #29343 ),
 .UNSPECIFIED., .F., .F.,
 ( 4, 2, 2, 4 ),
 ( 0.000000000000000000, 0.0006610868961727778791, 0.0009916303442591663849, 0.001322173792345555108 ),
 .UNSPECIFIED. ) ;
#192568 = CARTESIAN_POINT ( 'NONE',  ( -1.364683531250010295, 5.801041667008088432, -0.7879004041258300672 ) ) ;
#192569 = CARTESIAN_POINT ( 'NONE',  ( 4.457442142980160504, 1.574409630067734156, 1.170308293268598421 ) ) ;
#192570 = CARTESIAN_POINT ( 'NONE',  ( 0.7200771085676247463, -1.701685607325746252, -1.080902626906909747 ) ) ;
#192571 = CARTESIAN_POINT ( 'NONE',  ( -2.972980823146582186, 6.690504403638126263, 0.000000000000000000 ) ) ;
#192573 = FILL_AREA_STYLE_COLOUR ( '', #50250 ) ;
#192572 = CARTESIAN_POINT ( 'NONE',  ( 8.284195553149872993, 9.623648552551724578, -1.199719254218445830 ) ) ;
#192574 = CARTESIAN_POINT ( 'NONE',  ( 1.440467042440606749, 0.3595057747620767907, 1.835501880432292010 ) ) ;
#192575 = CARTESIAN_POINT ( 'NONE',  ( 0.6823417656249899377, 3.926041667008085767, -1.181850606188754593 ) ) ;
#192576 = CARTESIAN_POINT ( 'NONE',  ( 3.146742683403806140, 1.965092980649842502, 0.4368759242464967940 ) ) ;
#192578 = CARTESIAN_POINT ( 'NONE',  ( 3.585668865097063840, -0.6122912394212923770, 2.026781372153120930 ) ) ;
#192577 = CARTESIAN_POINT ( 'NONE',  ( -5.422898255786186006, 9.270539031818461950, -0.7216878364870207285 ) ) ;
#192579 = DIRECTION ( 'NONE',  ( 0.000000000000000000, 1.000000000000000000, 0.000000000000000000 ) ) ;
#192580 = CARTESIAN_POINT ( 'NONE',  ( 4.844224204019831781, -0.9789346907586125024, 1.824324395707350943 ) ) ;
#192581 = CARTESIAN_POINT ( 'NONE',  ( 4.085803189671889157, 5.860132702740892263, -1.599625672291273171 ) ) ;
#192583 = CARTESIAN_POINT ( 'NONE',  ( 11.92619526913700057, 13.39999999999998259, 1.328859060402682868 ) ) ;
#192582 = CARTESIAN_POINT ( 'NONE',  ( 6.527293198192279711, -1.364605693714017187, -1.583936087800744907 ) ) ;
#192585 = ORIENTED_EDGE ( 'NONE', *, *, #98066, .F. ) ;
#192584 = CARTESIAN_POINT ( 'NONE',  ( 5.262654937129007671, -1.321179299781930938, 1.260103332352560779 ) ) ;
#192586 = CARTESIAN_POINT ( 'NONE',  ( 7.889955328148847258, 11.29236608522730911, -1.199719254218446718 ) ) ;
#192587 = CARTESIAN_POINT ( 'NONE',  ( -5.398914348987512213, 6.259949555863199677, 2.420000000000001261 ) ) ;
#192588 = CARTESIAN_POINT ( 'NONE',  ( 9.809883170912574002, 12.88719579058855125, -8.001885615786651584 ) ) ;
#192589 = CARTESIAN_POINT ( 'NONE',  ( 6.053802686139254874, 0.6462426183462595120, -2.110027337871730690 ) ) ;
#192590 = CARTESIAN_POINT ( 'NONE',  ( 1.364683531249996529, 11.52604166700806410, 0.7879004041258403923 ) ) ;
#192591 = CARTESIAN_POINT ( 'NONE',  ( 5.619756671179353624, -0.4603523440993940175, 1.855926886426212175 ) ) ;
#192593 = CARTESIAN_POINT ( 'NONE',  ( -7.635213062790267458, 12.05949900656400686, 0.000000000000000000 ) ) ;
#192592 = AXIS2_PLACEMENT_3D ( 'NONE', #40798, #20235, #22361 ) ;
#192594 = CARTESIAN_POINT ( 'NONE',  ( 4.821896187954575197, 8.777295985922343391, 0.7998128361456462443 ) ) ;
#192595 = CARTESIAN_POINT ( 'NONE',  ( -11.09999999999960174, -3.430288072414404179E-15, 0.2598076211376223466 ) ) ;
#192596 = CARTESIAN_POINT ( 'NONE',  ( 2.697709378994964879, 6.091152008895348580, 0.7216878364870338292 ) ) ;
#192597 = FILL_AREA_STYLE ('',( #161188 ) ) ;
#192598 = EDGE_CURVE ( 'NONE', #7182, #117810, #161199, .T. ) ;
#192599 = CARTESIAN_POINT ( 'NONE',  ( 5.196852952739813070, 4.957416621151553571, -0.7998128361456221525 ) ) ;
#192600 = ORIENTED_EDGE ( 'NONE', *, *, #47209, .F. ) ;
#192601 = CIRCLE ( 'NONE', #144291, 0.4000000000000001332 ) ;
#192602 = DIRECTION ( 'NONE',  ( 1.000000000000000000, -7.771561172376097755E-16, -4.440892098500627148E-16 ) ) ;
#192603 = CARTESIAN_POINT ( 'NONE',  ( 0.07700591528353968596, 0.003617085621422307627, -1.910863332519038282 ) ) ;
#192604 = CARTESIAN_POINT ( 'NONE',  ( 7.666209513884374438, 7.908608952478760834, 0.7998128361456281477 ) ) ;
#192605 = CARTESIAN_POINT ( 'NONE',  ( 1.419999999999990603, 8.627523663848661428, 2.580000000000000515 ) ) ;
#192606 = CARTESIAN_POINT ( 'NONE',  ( -0.1405533004718494683, 0.2440837993472090295, -1.754028569132993542 ) ) ;
#192607 = CARTESIAN_POINT ( 'NONE',  ( -5.531363484695544841, 8.436712584578003771, 1.082531754730548412 ) ) ;
#192608 = CARTESIAN_POINT ( 'NONE',  ( 5.169736645512481132, 4.925780929386339935, 0.7998128361456341429 ) ) ;
#192609 = CARTESIAN_POINT ( 'NONE',  ( 2.518351277774394159, 0.8375136450692384216, 1.782609909039992946 ) ) ;
#192610 = CARTESIAN_POINT ( 'NONE',  ( 3.198842376697589085, 1.824128004127192337, 0.8596145101084637918 ) ) ;
#192611 = CARTESIAN_POINT ( 'NONE',  ( -8.342344591110322227, 8.627156865917170236, -0.7998128361456291469 ) ) ;
#192612 = CARTESIAN_POINT ( 'NONE',  ( 5.499767588998890844, 6.445425604367387429, 1.199719254218451159 ) ) ;
#192613 = CARTESIAN_POINT ( 'NONE',  ( 6.827182134110192813, 3.687242579989722824, 2.603029107617850002 ) ) ;
#192614 = AXIS2_PLACEMENT_3D ( 'NONE', #77358, #112071, #70403 ) ;
#192615 = CARTESIAN_POINT ( 'NONE',  ( 3.679775893577118318, -1.080384588543949809, 1.906543112819548913 ) ) ;
#192616 = DIRECTION ( 'NONE',  ( 0.000000000000000000, 0.000000000000000000, -1.000000000000000000 ) ) ;
#192617 = CARTESIAN_POINT ( 'NONE',  ( 2.151277967514260592, -1.545957563563664650, -1.149148694925563596 ) ) ;
#192618 = CARTESIAN_POINT ( 'NONE',  ( -7.472515219426274946, 11.86968485597268064, 0.000000000000000000 ) ) ;
#192619 = FACE_OUTER_BOUND ( 'NONE', #164036, .T. ) ;
#192620 = CARTESIAN_POINT ( 'NONE',  ( 0.1329588055935760349, 7.629137130509077380, -2.445925914280167923 ) ) ;
#192621 = EDGE_CURVE ( 'NONE', #96990, #34591, #12451, .T. ) ;
#192622 = CARTESIAN_POINT ( 'NONE',  ( -9.917242840447775265, 4.174869238508773783, -6.172972641688763140 ) ) ;
#192623 = CARTESIAN_POINT ( 'NONE',  ( 8.796542737168120851, 9.157054702984622097, -0.7998128361456211532 ) ) ;
#192624 = CARTESIAN_POINT ( 'NONE',  ( -6.773846765316610785, -7.473374494057217987, 6.773846765316634766 ) ) ;
#192625 = CARTESIAN_POINT ( 'NONE',  ( 6.699137298928158124, 6.988284068270579574, 0.7216878364870328300 ) ) ;
#192626 = EDGE_LOOP ( 'NONE', ( #162221, #196773, #59955, #83014 ) ) ;
#192628 = CARTESIAN_POINT ( 'NONE',  ( 2.947904902976675068, -1.353543519239216897, -1.490266562291961749 ) ) ;
#192627 = CARTESIAN_POINT ( 'NONE',  ( 6.040549724581927293, -1.551790349881351450, 0.9907606852931831742 ) ) ;
#192629 = CARTESIAN_POINT ( 'NONE',  ( 4.095287530520356434, 1.233756528997317137, -1.939045446859017030 ) ) ;
#192631 = CARTESIAN_POINT ( 'NONE',  ( 2.430303444995636664, -1.149418499707482999, 1.463420418157684422 ) ) ;
#192630 = CARTESIAN_POINT ( 'NONE',  ( -0.1290005225502676156, 1.324981729379502537, -2.425680704180297464 ) ) ;
#192632 = CARTESIAN_POINT ( 'NONE',  ( 1.642778471875001811, -1.392708332855374653, 2.845375778867859751 ) ) ;
#192633 = LINE ( 'NONE', #56261, #50110 ) ;
#192634 = CARTESIAN_POINT ( 'NONE',  ( -8.694856585065634746, 9.038420858865048757, 0.7998128361456462443 ) ) ;
#192635 = CARTESIAN_POINT ( 'NONE',  ( -4.828112100242283766, 7.686528979374367410, -1.082531754730549967 ) ) ;
#192637 = CARTESIAN_POINT ( 'NONE',  ( 3.854256360616271415, 0.6726810918341770140, 1.745705178215435582 ) ) ;
#192636 = CARTESIAN_POINT ( 'NONE',  ( 4.511325128988150190, -2.050071535818901225, 0.4094859698564096706 ) ) ;
#192638 = CARTESIAN_POINT ( 'NONE',  ( 7.483737605063422116, 7.833374748769873719, -0.7216878364870257245 ) ) ;
#192639 = EDGE_LOOP ( 'NONE', ( #191937, #80639 ) ) ;
#192640 = DIRECTION ( 'NONE',  ( -0.6507913734559652719, 0.7592566023652995710, -0.000000000000000000 ) ) ;
#192641 = CARTESIAN_POINT ( 'NONE',  ( 0.000000000000000000, 5.000000000000000888, 10.25000000000000000 ) ) ;
#192642 = CARTESIAN_POINT ( 'NONE',  ( 5.690025311828595278, -0.7696446287084879323, 1.543740960907719950 ) ) ;
#192643 = CARTESIAN_POINT ( 'NONE',  ( -6.925517538482230506, 6.974191971184389160, 0.7998128361456341429 ) ) ;
#192644 = CARTESIAN_POINT ( 'NONE',  ( 1.916292283401900720, -1.133531090463487212, -1.312443884513394554 ) ) ;
#192645 = CARTESIAN_POINT ( 'NONE',  ( 0.3870735955438693310, 1.000000000000000888, -11.88799243440807274 ) ) ;
#192646 = CARTESIAN_POINT ( 'NONE',  ( -2.428612866367529932E-14, 2.999999999999999112, 7.500000000000000000 ) ) ;
#192647 =( LENGTH_UNIT ( ) NAMED_UNIT ( * ) SI_UNIT ( .MILLI., .METRE. ) );
#192648 = CARTESIAN_POINT ( 'NONE',  ( 5.348546061712845301, -2.153812021095147688, -0.2729773376510102323 ) ) ;
#192649 = CARTESIAN_POINT ( 'NONE',  ( 4.389149243953620605, 1.629682310347341456, -0.8231139397327084106 ) ) ;
#192650 = CARTESIAN_POINT ( 'NONE',  ( 2.043732491806522056, 1.349072470436333715, 1.424505092005624807 ) ) ;
#192651 = CARTESIAN_POINT ( 'NONE',  ( 6.333232048763643540, -1.701881231816049000, -1.259509043995930222 ) ) ;
#192652 = CARTESIAN_POINT ( 'NONE',  ( 9.333041836227053523, 4.446947634372834912, 7.472413793103392265 ) ) ;
#192653 = CARTESIAN_POINT ( 'NONE',  ( -9.992522908471816123, 11.61669713376064372, 1.199719254218462483 ) ) ;
#192654 = CARTESIAN_POINT ( 'NONE',  ( 8.535021395002688749, 9.916278701380017324, 1.199719254218462483 ) ) ;
#192655 = CARTESIAN_POINT ( 'NONE',  ( 2.455864667332839257, -1.573010975769023601, -1.422207447652395373 ) ) ;
#192656 = CARTESIAN_POINT ( 'NONE',  ( -5.346851039111045978, 6.199209027673974859, 1.173132900504408438 ) ) ;
#192657 = CARTESIAN_POINT ( 'NONE',  ( -4.837732268475038566, 6.745175811576873848, -1.249133900884531467 ) ) ;
#192658 = CARTESIAN_POINT ( 'NONE',  ( 0.8661811918178536907, -2.060611401584189650, 0.1992402130865863485 ) ) ;
#192660 = CARTESIAN_POINT ( 'NONE',  ( -1.500000000000008216, 13.78125000068279604, 3.469446951953614189E-15 ) ) ;
#192659 = CARTESIAN_POINT ( 'NONE',  ( -11.09544190643409678, 2.974000657017215055, 3.605127613804370412 ) ) ;
#192662 = VERTEX_POINT ( 'NONE', #12905 ) ;
#192661 = CARTESIAN_POINT ( 'NONE',  ( 3.035994277891720827, -2.140246456218936721, 0.5942984311890684435 ) ) ;
#192663 = CARTESIAN_POINT ( 'NONE',  ( 0.6866852740153045476, 1.883736933065732533, 1.317207514508748734 ) ) ;
#192665 = CARTESIAN_POINT ( 'NONE',  ( 5.401261053844283566, -1.771754184838408630, 1.055722541708886020 ) ) ;
#192664 = CARTESIAN_POINT ( 'NONE',  ( 9.571693261567954636, 12.19006144329456731, 1.443375672974076540 ) ) ;
#192667 = CARTESIAN_POINT ( 'NONE',  ( 1.737499999999999378, -2.216666666666665453, -3.009438278150925683 ) ) ;
#192666 = CARTESIAN_POINT ( 'NONE',  ( 4.041212305325117882, 6.872442235258051646, -1.199719254218448494 ) ) ;
#192668 = EDGE_CURVE ( 'NONE', #12234, #136464, #209576, .T. ) ;
#192669 = CARTESIAN_POINT ( 'NONE',  ( 0.2333540202161610289, 0.003568502611739353923, -2.045944795905803471 ) ) ;
#192670 = CARTESIAN_POINT ( 'NONE',  ( 5.513187957602974976, -1.795010045117376496, 0.4093405989887277663 ) ) ;
#192671 = EDGE_CURVE ( 'NONE', #195556, #166249, #155193, .T. ) ;
#192672 = CARTESIAN_POINT ( 'NONE',  ( -0.1106727585416227011, 0.2327126083698972114, -2.036986407471320426 ) ) ;
#192673 = CARTESIAN_POINT ( 'NONE',  ( 2.590480338954644246, -0.2921314510030656453, -1.699667543312991747 ) ) ;
#192674 = CARTESIAN_POINT ( 'NONE',  ( 1.253139057289072822, 0.1435168058863903751, -2.011451928166609893 ) ) ;
#192675 = CARTESIAN_POINT ( 'NONE',  ( 3.112262249421397620, 0.05891664663748399922, 2.298092032709637689 ) ) ;
#192676 = CARTESIAN_POINT ( 'NONE',  ( 2.108995328314038353, 1.677457623459570168, -1.518302342262042304 ) ) ;
#192677 = CARTESIAN_POINT ( 'NONE',  ( 5.654936504234950867, -1.661008888676926309, 1.294703585725354156 ) ) ;
#192678 = CARTESIAN_POINT ( 'NONE',  ( -7.282137904315833410, 7.668451441222825515, 0.000000000000000000 ) ) ;
#192679 = CARTESIAN_POINT ( 'NONE',  ( 3.919032125857401905, -0.1322120426517567060, 1.764875357724977167 ) ) ;
#192680 = PRESENTATION_LAYER_ASSIGNMENT (  '', '', ( #71617 ) ) ;
#192682 = CARTESIAN_POINT ( 'NONE',  ( 6.075753635015332499, -1.229876075327457130, 1.934346496684937966 ) ) ;
#192681 = CARTESIAN_POINT ( 'NONE',  ( 4.136646265500957043, 5.919449624541475607, -1.443375672974068769 ) ) ;
#192683 = CARTESIAN_POINT ( 'NONE',  ( 4.786955173189685553, 1.366302399619228947, 1.234289508136581892 ) ) ;
#192684 = CARTESIAN_POINT ( 'NONE',  ( -5.087333953625788219, 6.958308917361963886, 1.599625672291267398 ) ) ;
#192685 = CARTESIAN_POINT ( 'NONE',  ( 5.843201017365476702, 6.879784610756938257, -1.082531754730543083 ) ) ;
#192686 = CARTESIAN_POINT ( 'NONE',  ( -0.7499999999999972244, 3.358333333333359150, -1.299038105676652011 ) ) ;
#192687 = CARTESIAN_POINT ( 'NONE',  ( 4.523480939507462217, -1.347072049868164978, -1.728447516733351952 ) ) ;
#192688 = CARTESIAN_POINT ( 'NONE',  ( -4.460796234096120472, 5.163016013655583158, 1.199719254218462483 ) ) ;
#192689 = CARTESIAN_POINT ( 'NONE',  ( -0.08000000000000714873, -6.134628647623513231, 10.91970695577494865 ) ) ;
#192690 = CARTESIAN_POINT ( 'NONE',  ( 4.861816338261779613, -0.5554421346023461492, 1.994381909410049669 ) ) ;
#192691 = CARTESIAN_POINT ( 'NONE',  ( 0.3039231887648624619, -1.082844287645868375, -1.700959134490941160 ) ) ;
#192692 = CARTESIAN_POINT ( 'NONE',  ( -1.364683531250012516, 4.488541667008090208, -0.7879004041258300672 ) ) ;
#192693 = CARTESIAN_POINT ( 'NONE',  ( 3.721244860960619683, -0.1409348896288381003, 1.921400582950444580 ) ) ;
#192694 = CARTESIAN_POINT ( 'NONE',  ( 1.364683531249997417, 8.734375000341396245, 2.602085213965210642E-15 ) ) ;
#192695 = CARTESIAN_POINT ( 'NONE',  ( 0.000000000000000000, -8.233137084989836652, 0.000000000000000000 ) ) ;
#192696 = CARTESIAN_POINT ( 'NONE',  ( 0.1939906290522614152, 2.069702213058471241, -0.8072921158600793179 ) ) ;
#192697 = ORIENTED_EDGE ( 'NONE', *, *, #123827, .T. ) ;
#192699 = PLANE ( 'NONE',  #132935 ) ;
#192698 = CARTESIAN_POINT ( 'NONE',  ( -4.719646871332968452, 5.639247783710797712, 1.082531754730549078 ) ) ;
#192700 = CARTESIAN_POINT ( 'NONE',  ( 3.867100128395839942, 5.534702787927018974, -1.599625672291255185 ) ) ;
#192701 = CARTESIAN_POINT ( 'NONE',  ( 8.064677165291193717, -5.223431457505076203, -7.446209719563348983 ) ) ;
#192702 = CARTESIAN_POINT ( 'NONE',  ( 0.2524733864175063847, 6.376792883867242523, -3.135723845156253020 ) ) ;
#192703 = CARTESIAN_POINT ( 'NONE',  ( 6.776370306708061619, -7.161464053357560644, 6.781144757626056396 ) ) ;
#192704 = CARTESIAN_POINT ( 'NONE',  ( 1.662477996687723669, -0.7030478115006146833, -1.831755296705489977 ) ) ;
#192705 = CARTESIAN_POINT ( 'NONE',  ( 1.364683531249988535, 1.926041667008086211, 0.7879004041258500513 ) ) ;
#192706 = CARTESIAN_POINT ( 'NONE',  ( 6.596550757224428629, -0.5713381284546023009, -2.084776384472402100 ) ) ;
#192707 = CARTESIAN_POINT ( 'NONE',  ( 5.476992472119650124, 1.812042599547862176, 0.7524171098330989516 ) ) ;
#192708 = CARTESIAN_POINT ( 'NONE',  ( -9.378489572351046633, 11.96465713920816043, -1.599625672291263179 ) ) ;
#192709 = CARTESIAN_POINT ( 'NONE',  ( -6.033015167956818026, 6.140865238812146742, -0.7216878364870267237 ) ) ;
#192710 = PRESENTATION_LAYER_ASSIGNMENT (  '', '', ( #89015 ) ) ;
#192711 = CARTESIAN_POINT ( 'NONE',  ( 6.016527291255574283, 1.455332790597754000, -1.598591904487467463 ) ) ;
#192713 = ORIENTED_EDGE ( 'NONE', *, *, #71694, .T. ) ;
#192712 = CARTESIAN_POINT ( 'NONE',  ( -0.2106725631050176961, 2.017899180269961956, -2.418275446281520136 ) ) ;
#192714 = CARTESIAN_POINT ( 'NONE',  ( 0.6823417656249899377, 3.926041667008085767, -1.181850606188754593 ) ) ;
#192716 = CARTESIAN_POINT ( 'NONE',  ( 6.766873944267649321, -1.801439555086775002, -0.8010921537245048185 ) ) ;
#192715 = B_SPLINE_CURVE_WITH_KNOTS ( 'NONE', 3,
 ( #81922, #144846, #164248, #44116, #214020, #79789 ),
 .UNSPECIFIED., .F., .F.,
 ( 4, 2, 4 ),
 ( 0.000000000000000000, 0.0003844267940947831432, 0.0007688535881895662864 ),
 .UNSPECIFIED. ) ;
#192717 = CARTESIAN_POINT ( 'NONE',  ( 6.239525021605913047, -1.647457779603450634, -0.5405594386218066649 ) ) ;
#192719 = CARTESIAN_POINT ( 'NONE',  ( 2.577880719133851084, -1.123996537731044354, 1.881222605751430521 ) ) ;
#192718 = CARTESIAN_POINT ( 'NONE',  ( -1.360316468750030650, 0.8697916670080861890, -0.7853790794159041244 ) ) ;
#192720 = CARTESIAN_POINT ( 'NONE',  ( 4.717980713983113361, -2.264103904663441913, 0.4450920570577068247 ) ) ;
#192721 = CARTESIAN_POINT ( 'NONE',  ( 6.081337768261708909, 1.905808788339557802, -0.7845383490599889820 ) ) ;
#192722 = CARTESIAN_POINT ( 'NONE',  ( 0.6384921070224542916, -1.665899481912515245, 0.9977595643581302909 ) ) ;
#192723 = CARTESIAN_POINT ( 'NONE',  ( -5.490689023410187275, 8.389259046411751797, 1.082531754730548412 ) ) ;
#192724 = DIRECTION ( 'NONE',  ( 1.000000000000000000, -0.000000000000000000, -0.000000000000000000 ) ) ;
#192725 = CARTESIAN_POINT ( 'NONE',  ( 5.238584497427841491, 1.261362679698872169, -1.704546977916908457 ) ) ;
#192726 = SURFACE_STYLE_FILL_AREA ( #63810 ) ;
#192727 = CARTESIAN_POINT ( 'NONE',  ( 2.707657903872981553, 1.899618770239443366, 0.6767133375917554483 ) ) ;
#192728 = CARTESIAN_POINT ( 'NONE',  ( -5.382223794500835545, 8.262716279350872384, -1.082531754730543971 ) ) ;
#192729 = CARTESIAN_POINT ( 'NONE',  ( 6.053802686139254874, 0.6462426183462595120, -2.110027337871730690 ) ) ;
#192730 = CARTESIAN_POINT ( 'NONE',  ( -6.257970421159510188, 9.458660037064859694, 1.199719254218452047 ) ) ;
#192731 = CARTESIAN_POINT ( 'NONE',  ( -3.024971404778824091, -3.100164103410550709, -1.602261151954494700 ) ) ;
#192732 = CARTESIAN_POINT ( 'NONE',  ( 0.2580658466875830337, 0.6954254843183353962, 1.688255465954719536 ) ) ;
#192733 = DIRECTION ( 'NONE',  ( 0.000000000000000000, 8.546850786086437571E-32, 1.000000000000000000 ) ) ;
#192735 = CARTESIAN_POINT ( 'NONE',  ( -6.303615075710994553, 6.318915441276409695, -0.7998128361456361413 ) ) ;
#192734 = CARTESIAN_POINT ( 'NONE',  ( -5.196461137543813891, 7.842688287721260032, 1.273345793684066862 ) ) ;
#192736 = CARTESIAN_POINT ( 'NONE',  ( -4.727634349329638219, 8.249773960229633829, 0.6920918352846835431 ) ) ;
#192737 = EDGE_LOOP ( 'NONE', ( #25288, #70552, #35851, #25038, #63163, #109084, #212701, #91975 ) ) ;
#192738 = CARTESIAN_POINT ( 'NONE',  ( 5.612203307022772591, -0.9243832361092527705, -1.842014774801424615 ) ) ;
#192739 = CARTESIAN_POINT ( 'NONE',  ( 4.030162213014739869, 7.767662802593035209, -0.3896624696924297360 ) ) ;
#192740 = CARTESIAN_POINT ( 'NONE',  ( -0.2108831679770961920, 2.882544375557041239, -2.385815782126240236 ) ) ;
#192741 = CARTESIAN_POINT ( 'NONE',  ( -3.578462479003122976, 6.262291094557191684, 1.199719254218464037 ) ) ;
#192742 = CARTESIAN_POINT ( 'NONE',  ( 0.000000000000000000, 13.88000000000000078, 0.000000000000000000 ) ) ;
#192743 = CARTESIAN_POINT ( 'NONE',  ( 4.617835026475571425, -0.5366920026289195844, 1.946999912814169287 ) ) ;
#192744 = CARTESIAN_POINT ( 'NONE',  ( 0.7499999999999902300, 1.483333333333357373, 1.299038105676657340 ) ) ;
#192746 = CARTESIAN_POINT ( 'NONE',  ( 9.164948653157988900, 11.71552606681625619, -1.443375672974057666 ) ) ;
#192745 = CARTESIAN_POINT ( 'NONE',  ( -3.955946960137363799, 7.837298230127379917, 0.7998128361456352531 ) ) ;
#192747 = CARTESIAN_POINT ( 'NONE',  ( 5.798083248138522272, 9.916180889470295412, 0.7998128361456462443 ) ) ;
#192748 = CARTESIAN_POINT ( 'NONE',  ( 3.924726224964281140, 1.956320258297845172, 0.6483119717206936583 ) ) ;
#192749 = CARTESIAN_POINT ( 'NONE',  ( 3.199842427594956185, 1.824118962040650604, 0.8596310190432244758 ) ) ;
#192750 = ORIENTED_EDGE ( 'NONE', *, *, #152940, .T. ) ;
#192751 = CARTESIAN_POINT ( 'NONE',  ( 6.727182134110196721, 7.051813866762763006, 2.787205683092201181 ) ) ;
#192752 = CARTESIAN_POINT ( 'NONE',  ( 5.515469562660962666, 5.329135999392899947, 0.7998128361456341429 ) ) ;
#192753 = CIRCLE ( 'NONE', #9398, 0.08000000000000020983 ) ;
#192755 = EDGE_LOOP ( 'NONE', ( #191760, #169200, #58901, #76046, #3022 ) ) ;
#192754 = CARTESIAN_POINT ( 'NONE',  ( -0.5015801190230781970, 7.801378974689814783, -1.936921611551790212 ) ) ;
#192756 = CARTESIAN_POINT ( 'NONE',  ( 3.057970071934034362, 1.730601471501746147, -1.034006501934421784 ) ) ;
#192757 = CARTESIAN_POINT ( 'NONE',  ( 2.308333576337255000, 1.644441489820291924, 0.8281405146027611686 ) ) ;
#192758 = CARTESIAN_POINT ( 'NONE',  ( 1.190513350481865240, -1.033627929232444620, 2.063343651489284003 ) ) ;
#192759 = CARTESIAN_POINT ( 'NONE',  ( 5.194709132691408549, 6.089524072008651423, 1.199719254218452935 ) ) ;
#192760 = CARTESIAN_POINT ( 'NONE',  ( 3.058072297120766336, 2.151488047868503894, -0.2085137855245971505 ) ) ;
#192761 = CARTESIAN_POINT ( 'NONE',  ( -7.223796917982883592, 7.322184580601816428, -0.7998128361456291469 ) ) ;
#192762 = COLOUR_RGB ( '', 0.08235294, 0.09019608, 0.10196078) ;
#192763 = ORIENTED_EDGE ( 'NONE', *, *, #87277, .T. ) ;
#192764 = CARTESIAN_POINT ( 'NONE',  ( 0.7427767429722329506, -1.606530860214189893, 0.9580933318182258684 ) ) ;
#192765 = ORIENTED_EDGE ( 'NONE', *, *, #81270, .T. ) ;
#192766 = CARTESIAN_POINT ( 'NONE',  ( 5.295764336479223289, -0.7102129355434207980, 1.839261741220117097 ) ) ;
#192768 = CARTESIAN_POINT ( 'NONE',  ( 7.890482213029013536, 12.14938698193514277, 1.040834085586084257E-14 ) ) ;
#192767 = CARTESIAN_POINT ( 'NONE',  ( 1.364683531249988535, 3.613541667008086211, 0.7879004041258500513 ) ) ;
#192770 = CARTESIAN_POINT ( 'NONE',  ( 0.1181803206181560040, -2.163391993613572151, 0.4351206515559591370 ) ) ;
#192769 = CARTESIAN_POINT ( 'NONE',  ( -6.093499974338126179, 9.196501505781426999, -1.199719254218440723 ) ) ;
#192771 = CARTESIAN_POINT ( 'NONE',  ( 5.078784331656527762, 4.889946239879535028, -0.1287282925451668503 ) ) ;
#192772 = CARTESIAN_POINT ( 'NONE',  ( 6.681470773436232413, 6.689470745297396270, -0.7998128361456281477 ) ) ;
#192773 = CARTESIAN_POINT ( 'NONE',  ( -5.738125327081750271, 7.717565519727259904, 1.599625672291269396 ) ) ;
#192774 = VECTOR ( 'NONE', #139703, 1000.000000000000000 ) ;
#192775 = CARTESIAN_POINT ( 'NONE',  ( 6.539320575229239374, 3.684509595994990061, 2.717302710099603225 ) ) ;
#192776 = CARTESIAN_POINT ( 'NONE',  ( 4.856303703212550893, 0.7536814072931929953, 1.821903339724652460 ) ) ;
#192777 = CARTESIAN_POINT ( 'NONE',  ( 6.170177014438331220, 2.014108787598484440, -0.1525786406279260876 ) ) ;
#192778 = CARTESIAN_POINT ( 'NONE',  ( -1.500000000000015099, 0.1604166673494879791, -0.8660254037844383745 ) ) ;
#192779 = CARTESIAN_POINT ( 'NONE',  ( 5.004635055918612352, -0.7736033420917761694, -2.174287598079288841 ) ) ;
#192780 = CARTESIAN_POINT ( 'NONE',  ( 1.727463565662648026, 0.1559948080240464718, -2.056756566214789306 ) ) ;
#192781 = CARTESIAN_POINT ( 'NONE',  ( 6.914295153289432783, 10.05013286460426691, -1.082531754730537976 ) ) ;
#192782 = CARTESIAN_POINT ( 'NONE',  ( 3.867818961648523235, 7.734482231890414283, 1.040834085586084257E-14 ) ) ;
#192783 = CARTESIAN_POINT ( 'NONE',  ( 5.747730777550676073, 5.670383760089384495, 0.000000000000000000 ) ) ;
#192784 = CARTESIAN_POINT ( 'NONE',  ( -1.402160292154681736E-14, 2.509375000341417028, -1.575800808251660134 ) ) ;
#192785 = CARTESIAN_POINT ( 'NONE',  ( 4.390861645979372341, 6.216034235099629157, -1.599625672291269396 ) ) ;
#192786 = CARTESIAN_POINT ( 'NONE',  ( 6.304178240230120522, 6.457222156464352381, -0.7216878364870257245 ) ) ;
#192788 = CARTESIAN_POINT ( 'NONE',  ( 3.010954138651841916, 0.05432569772663429358, 2.015980714967258614 ) ) ;
#192787 = CARTESIAN_POINT ( 'NONE',  ( 5.020078820186387070, 2.148262114505914866, -0.3138009609788168230 ) ) ;
#192790 = CARTESIAN_POINT ( 'NONE',  ( 4.528748383445759806, -1.681502307688139908, 0.7506017836093890061 ) ) ;
#192789 = CARTESIAN_POINT ( 'NONE',  ( -5.097502569058225852, 5.049433873430440478, -0.7216878364870207285 ) ) ;
#192792 = CARTESIAN_POINT ( 'NONE',  ( -0.07933194154488912297, -7.473374494045017968, 9.499668754385634628 ) ) ;
#192791 = DIRECTION ( 'NONE',  ( 0.000000000000000000, 0.000000000000000000, -1.000000000000000000 ) ) ;
#192793 = CARTESIAN_POINT ( 'NONE',  ( 5.056268342064010213, -1.587557771011731678, 1.511049258477934032 ) ) ;
#192794 = DIRECTION ( 'NONE',  ( -0.000000000000000000, -1.000000000000000000, -0.000000000000000000 ) ) ;
#192795 = CARTESIAN_POINT ( 'NONE',  ( 5.629810878523249684, -1.430378642458853378, -1.753011776973804725 ) ) ;
#192796 = CARTESIAN_POINT ( 'NONE',  ( -4.014602626671047503, 7.795841479962435372, -0.4363419845254731255 ) ) ;
#192797 = CARTESIAN_POINT ( 'NONE',  ( -2.974698719455045381, 6.690899969729074748, -0.05384663926280564006 ) ) ;
#192798 = CARTESIAN_POINT ( 'NONE',  ( 4.797842130449009090, 8.250315290282747682, 0.8618622828703215166 ) ) ;
#192799 = CARTESIAN_POINT ( 'NONE',  ( -3.648552735408985725, 7.270745601370182776, -0.7216878364870458196 ) ) ;
#192800 = CARTESIAN_POINT ( 'NONE',  ( 3.933273961740298752, 5.682181936820735579, 1.443375672974058777 ) ) ;
#192801 =( BOUNDED_SURFACE ( )  B_SPLINE_SURFACE ( 3, 3, ( 
 ( #188251, #60390, #138462, #204482, #39892, #106002, #78770, #97190, #144893, #79842, #65692, #176297, #209828, #47375, #178430, #13766, #129754, #95056, #160036, #161106, #143832, #30038, #32166, #11639, #179494, #110288, #113487, #14826, #210901, #61464, #48437, #147007, #98244, #77711, #96124, #64659, #12694, #177358, #127630, #162179, #112417, #145951, #130803, #15887, #31117, #211961, #197848, #62528, #28972, #128689, #194658, #46302, #93995, #63600, #193596, #195739, #196795, #163243, #80917, #213025, #114552, #180543, #164298, #81971, #148058, #214064, #131840, #45237, #111353, #27900, #102492, #150192, #49480, #181595, #2825, #36413, #86241, #71026, #84105, #198895, #103564, #19091, #168556, #149105, #21207, #169624, #1761, #51621, #20155, #18016, #152312, #67819, #85171, #4949, #115600, #684, #201029, #117746, #167495, #68895, #34282, #99307, #100356, #83030, #183737, #185855, #165354, #118801, #33223, #153378, #16949, #133966, #184787, #66751, #132892, #199973, #151255, #35344, #3888, #137141, #50542, #101423, #135015, #52671, #69958, #136070, #202084, #116664, #182662, #53743, #119877, #37487, #87309, #166425, #42856, #40710, #108963, #39623, #25501, #186933, #173928, #120961, #171758, #73170, #56945, #174983, #140362, #26567, #9258, #156591, #72100, #154452, #92672, #55875, #207451, #122032, #106814, #187998, #138210, #158716, #141445, #105728, #91609, #23353, #172844, #123117, #157660, #10313, #76388, #89463, #75328, #24416, #155516, #90529, #7098, #59070, #8185, #125231, #191189, #203168, #54813, #38565, #104640, #6031, #189077, #170687, #22274, #74270, #205308, #206381, #190133, #139276, #58007, #204223, #124171, #88383, #41789, #107902, #29788, #177099, #95873, #178172, #209565, #80667, #61211, #162991, #77455, #146758, #145710, #14572, #96940, #127368, #212776, #193339, #78520, #161928, #159776, #11375, #142496, #60138, #126295, #13518, #79590, #30863, #44984, #111093, #208503, #211708, #28714, #63344, #192254, #143573, #94800, #43917, #113235, #110032, #160849, #12441, #144637, #128440, #210652, #62279, #129503, #194406, #195484, #47117, #46048, #176044, #179239, #27636, #93737, #112169, #117998, #102755, #167748, #5210, #136331, #186117, #87571, #52927, #183988, #119061, #101679, #202350, #204487, #35602, #137398, #68080, #172025, #134216, #86497, #203416, #19348, #200225, #152562, #169872, #54001, #104902, #155776, #85427, #70220, #103824, #69151, #51876, #151513, #3081, #121221, #55072, #56137, #185043, #36667, #23619, #71286, #135271, #187191, #201286, #168811, #20415, #72364, #170943, #138465, #4149, #120139, #37750, #21462, #153641, #38819, #22542, #88649, #154708, #6290, #122298, #188255, #39895, #106005, #89728, #125490, #92931, #26827, #9517, #109232, #192518, #140628, #75590, #95061, #73438, #110291, #28975, #8438, #44171, #76646, #160039, #143835, #127633, #176300, #94000, #158975, #74526, #207713, #27903, #206640, #77714, #11643, #7361, #141702, #91868, #58274, #209831, #124430, #59336, #190388, #90789, #61467, #193598, #42046, #45240, #108157, #191452, #43117, #111357, #177362, #139541, #174184, #205568, #175242, #25756, #10572, #157924, #57206, #142761, #123366, #189332, #40972, #107083, #173105, #24685, #156853, #208766, #60394, #126557, #130807, #163247, #80920, #148061, #211964, #63603, #178434 ),
 ( #34287, #129758, #13769, #195742, #47379, #113490, #144895, #179498, #112421, #31120, #33227, #32169, #98246, #147009, #196798, #210903, #688, #213030, #66754, #97194, #197852, #62530, #131842, #78772, #14829, #64662, #48440, #132895, #164302, #198899, #181599, #114555, #30041, #96128, #50545, #79845, #15891, #65695, #180548, #194660, #99310, #49483, #83034, #128692, #81975, #115603, #214069, #145954, #162183, #165358, #16953, #149108, #116667, #182665, #161109, #12696, #46305, #71835, #170420, #154188, #137944, #5756, #84107, #55612, #54547, #187736, #189877, #6836, #203966, #39364, #123910, #121767, #57750, #22008, #105460, #171495, #88118, #186669, #136876, #74000, #156329, #23086, #100359, #18020, #56686, #90261, #140093, #124968, #89201, #38296, #157399, #72914, #7912, #202902, #75067, #8992, #155254, #139019, #206120, #205042, #41520, #122852, #107632, #150195, #188814, #120694, #40448, #106550, #172577, #24158, #173664, #1765, #25238, #104374, #91340, #141180, #67822, #207189, #166429, #58815, #190930, #60948, #177909, #158454, #174728, #127105, #144382, #28449, #79331, #130297, #10053, #44721, #78258, #193070, #210382, #13259, #110830, #76130, #92414, #12186, #77187, #94541, #27374, #211446, #62023, #46856, #195220, #42594, #64154, #63080, #112970, #208245, #176835, #142233, #80399, #128179, #160580, #194140, #29522, #93475, #159513, #59878, #11112, #26300, #109773, #175782, #95615, #45789, #111908, #161665, #143309, #212513, #209300, #146495, #145449, #108699, #129248, #126028, #162732, #178982, #191990, #30596, #96683, #14304, #43656, #197336, #69449, #114045, #180039, #34825, #183219, #184275, #32709, #181092, #85719, #199454, #48977, #51096, #196285, #147544, #81467, #200517, #84657, #52162, #115095, #164845, #98790, #198389, #66239, #213565, #100899, #65187, #166988, #99851, #148603, #47932, #18579, #168044, #118289, #165913, #67307, #1247, #50030, #83585, #150745, #16437, #116154, #31660, #97738, #2307, #3380, #82516, #68383, #117222, #134513, #35900, #101976, #19646, #151807, #133448, #172, #182141, #163796, #132388, #15373, #131341, #33771, #17498, #149667, #136622, #139835, #54298, #187483, #120435, #4437, #189618, #73738, #202648, #106296, #170165, #39113, #55358, #90011, #91081, #24978, #186410, #156066, #152859, #38047, #119356, #104117, #21753, #56430, #5501, #204776, #138758, #87861, #157141, #153933, #173396, #71582, #8734, #172316, #135555, #41265, #137690, #201579, #203711, #105196, #122589, #70507, #121510, #53225, #185343, #36966, #188551, #40182, #123656, #171233, #22828, #103047, #23907, #88943, #7654, #169102, #86791, #20699, #205863, #57496, #107374, #154996, #6582, #72661, #76924, #159250, #92155, #61758, #26042, #127927, #192802, #27110, #140915, #193879, #46588, #79062, #44460, #160325, #94285, #143050, #176579, #45526, #207993, #209045, #162468, #206928, #177654, #96417, #75872, #111642, #144124, #12988, #211186, #194952, #29262, #161404, #11929, #141979, #60681, #95354, #59620, #145181, #62811, #74814, #126843, #10850, #125776, #128973, #191737, #110577, #43393, #158208, #112707, #178717, #109514, #30333, #175522, #28188, #78001, #58558, #124711, #190670, #93219, #42331, #210118, #108446, #174466, #9797, #182958, #49766, #18313, #166721, #14042, #35635, #34573, #84397, #179778, #82254 ),
 ( #100645, #131088, #150484, #81203, #197078, #180827, #213313, #97471, #47665, #199185, #67048, #114828, #80128, #146233, #181877, #983, #50832, #101714, #48715, #163528, #68114, #198135, #133185, #113776, #200257, #134251, #32453, #16169, #116960, #98522, #2044, #132125, #51909, #63884, #164584, #31397, #165650, #148345, #115892, #33513, #64938, #130038, #214346, #15114, #65976, #118032, #196029, #83314, #212250, #184018, #147282, #99586, #149400, #17239, #85461, #37785, #55105, #153676, #204521, #41006, #69185, #169909, #203451, #103859, #121254, #138499, #21496, #135306, #3114, #38853, #104937, #87606, #187225, #151547, #7395, #5244, #73474, #4183, #56169, #201319, #122332, #52959, #136367, #71321, #137434, #139575, #170978, #205602, #188289, #22577, #36703, #119097, #57240, #20449, #88683, #72399, #202387, #185078, #106038, #39929, #89763, #102788, #154742, #172060, #70254, #86532, #168846, #6326, #23654, #155811, #123400, #189364, #167785, #19381, #152597, #54038, #120174, #186152, #141733, #9548, #90822, #59366, #58305, #191483, #193627, #127665, #60428, #190419, #124460, #210932, #174216, #110323, #11672, #207741, #140659, #45269, #143868, #29006, #156885, #92962, #61498, #75624, #25790, #42078, #159008, #109264, #175272, #111390, #12729, #27936, #26857, #194694, #125523, #91900, #157956, #43151, #10602, #8472, #76678, #108190, #142792, #177392, #208799, #126588, #192549, #95093, #44202, #161142, #176329, #94030, #160068, #77747, #209861, #206673, #78802, #144926, #62558, #107115, #24720, #128722, #173139, #74558, #67856, #80947, #195770, #100392, #15922, #99340, #145983, #18055, #166462, #147039, #48470, #165389, #14857, #33256, #164333, #132925, #96163, #213061, #211994, #197882, #114585, #82005, #65726, #31149, #162214, #97223, #79873, #180576, #182697, #13799, #115632, #46335, #150228, #112450, #64691, #181627, #63635, #178463, #130836, #148093, #32198, #83063, #134005, #129789, #98274, #214098, #196829, #131873, #16984, #49512, #47409, #113522, #149141, #721, #66785, #198930, #30073, #84140, #50576, #1799, #163276, #116698, #179531, #34316, #117782, #168590, #69996, #53783, #171798, #137180, #105772, #38600, #186968, #188034, #36453, #184824, #89504, #203204, #201065, #54851, #200010, #151291, #85207, #204262, #88425, #55913, #52707, #20190, #118838, #202124, #136108, #2862, #104678, #68932, #170726, #103602, #152348, #51660, #22312, #23392, #122071, #169659, #71064, #4988, #119916, #87351, #154491, #102528, #185892, #73210, #183774, #6070, #7138, #86278, #72141, #121001, #138248, #39664, #155558, #35384, #101459, #167530, #3926, #37526, #19128, #21244, #135052, #153417, #139317, #207489, #9296, #140402, #143611, #58045, #191230, #124211, #8221, #193378, #77492, #206421, #110068, #173965, #42893, #59108, #93773, #94837, #28753, #190173, #159813, #109002, #25538, #175019, #41827, #11417, #26606, #209604, #61248, #205346, #160888, #127405, #45022, #90571, #125268, #189114, #177136, #92707, #141482, #158754, #126333, #107940, #91646, #156632, #157699, #123157, #75369, #10348, #60176, #76422, #208540, #142533, #192292, #12483, #43952, #56983, #176080, #27678, #111132, #40748, #106854, #172883, #24457, #74306, #163027, #165144, #196584, #179279, #14610, #99092, #195521, #80707, #146797, #16735, #469, #78557, #213862 ),
 ( #48227, #30903, #212813, #82821, #47158, #33013, #145746, #113274, #96979, #63385, #161965, #112205, #49276, #131632, #64450, #144675, #210689, #31957, #65483, #115397, #100141, #130595, #13556, #132680, #114339, #197631, #178212, #50331, #198686, #180334, #98041, #181390, #164094, #148897, #15675, #66539, #128476, #81762, #29828, #147843, #116449, #182443, #34070, #129540, #194444, #166205, #95912, #62317, #46086, #79627, #211747, #17794, #121812, #83882, #36194, #153160, #133750, #149972, #102270, #119657, #3671, #54594, #105505, #199758, #19940, #53523, #168345, #185642, #202950, #86026, #51403, #67604, #103344, #169408, #152100, #37274, #1542, #71881, #69747, #137990, #68681, #120741, #117523, #186715, #183517, #200811, #135853, #201875, #204008, #20994, #55656, #38343, #87090, #101197, #35125, #187780, #84954, #4735, #136923, #52461, #167285, #170467, #104419, #154232, #18870, #70810, #22053, #134805, #151043, #2612, #88163, #118587, #39410, #5804, #184574, #56730, #143354, #11158, #57794, #173710, #10100, #140140, #158501, #75115, #43702, #6881, #206166, #122898, #108748, #25286, #141227, #190973, #156374, #72960, #7958, #205089, #91387, #93519, #139061, #26349, #171537, #60997, #23129, #189923, #92462, #188857, #89247, #41568, #58860, #157447, #208290, #47702, #40493, #9041, #207236, #107682, #125017, #142280, #42640, #106598, #172625, #174773, #76174, #59923, #126078, #155298, #77236, #192039, #209349, #74050, #109819, #24202, #175829, #90305, #123954, #27421, #159562, #127150, #193123, #19418, #134288, #67084, #197113, #64971, #3150, #180866, #116993, #18353, #148383, #147321, #51945, #150520, #35673, #163570, #99621, #68154, #16207, #32487, #131124, #165687, #115928, #181916, #200293, #101751, #113816, #34610, #69220, #82290, #98561, #164622, #214384, #66014, #97513, #132163, #48752, #198169, #118068, #17276, #49802, #33548, #184054, #83352, #167818, #149437, #1019, #133218, #199224, #114865, #213348, #84431, #166757, #50871, #179816, #31435, #182993, #100679, #2081, #135339, #85496, #151583, #15153, #201353, #81239, #21526, #120208, #103893, #87637, #169941, #36736, #5277, #4217, #137470, #139610, #171011, #153708, #203484, #73507, #71354, #7426, #186183, #55137, #121282, #37816, #136402, #86568, #23685, #106069, #187258, #52994, #185110, #6359, #39961, #89795, #74587, #38885, #202418, #107146, #22608, #172093, #152630, #24751, #173172, #104970, #88716, #155841, #154775, #205632, #72428, #57270, #102822, #138530, #70286, #204553, #56202, #122365, #188321, #123432, #168877, #189394, #54073, #41036, #90853, #20481, #156917, #119130, #8506, #140690, #10625, #127690, #108219, #124489, #76700, #94054, #192574, #29034, #79895, #174244, #208824, #27961, #142817, #160095, #177416, #60454, #25816, #42106, #77772, #143892, #126611, #11698, #190448, #46355, #44229, #112475, #43175, #95117, #91926, #161166, #157986, #175298, #110350, #176353, #178484, #209886, #30094, #12752, #61524, #75651, #9574, #96184, #59393, #193650, #111412, #26884, #141758, #144947, #78826, #128742, #207766, #45292, #210953, #109288, #125549, #191510, #62580, #194716, #162235, #13821, #206706, #58333, #92987, #159032, #34343, #15943, #115659, #66810, #64713, #167555, #182724, #183797, #51685, #196852, #35407, #32224, #197904, #132953, #80970, #147062 ),
 ( #198956, #98296, #146004, #63658, #99364, #50599, #100416, #19156, #180599, #213082, #200033, #181653, #116724, #31170, #117807, #101485, #164359, #148120, #166487, #114608, #18078, #49533, #84166, #195793, #82027, #97243, #83088, #214121, #33279, #165416, #130856, #47431, #48490, #179549, #65750, #67880, #113546, #744, #212014, #129812, #163297, #131896, #150254, #14878, #17012, #149167, #1822, #134026, #122098, #172912, #201091, #87379, #121031, #21273, #38629, #55945, #153447, #52732, #135078, #170755, #22343, #5020, #186998, #68957, #139345, #137211, #205375, #136137, #188062, #118866, #39691, #2886, #53813, #169685, #71094, #57011, #88456, #123182, #105802, #104705, #168616, #36480, #189142, #152375, #154516, #204288, #119942, #184852, #23420, #171826, #7168, #102555, #203233, #89531, #202153, #3954, #86305, #155583, #6097, #73238, #40780, #106886, #85229, #151318, #72166, #70021, #54877, #20218, #185918, #37553, #103633, #138274, #92737, #109031, #25566, #28784, #157730, #76455, #9325, #107966, #78586, #177167, #91677, #209638, #59139, #142563, #158782, #193410, #194475, #128507, #75399, #45054, #208569, #125298, #60203, #141512, #111166, #126364, #94867, #160921, #24486, #46118, #12515, #144708, #190198, #10379, #74334, #62347, #192323, #26636, #43981, #11449, #207520, #191256, #41857, #42921, #8250, #175050, #110100, #159846, #176111, #93806, #27711, #127440, #77523, #143644, #61278, #210720, #112235, #90598, #156658, #140436, #206448, #58076, #124238, #173994, #165170, #113304, #179311, #51430, #95940, #161996, #16764, #82848, #166235, #14642, #163061, #67631, #181415, #30932, #33042, #178244, #129567, #63415, #182470, #66565, #34099, #97008, #146824, #80735, #180363, #48253, #195554, #148924, #47191, #497, #81791, #130622, #29859, #132707, #149999, #100170, #147874, #49307, #197661, #31988, #65512, #198713, #212844, #98067, #13586, #79659, #50359, #199784, #114368, #131658, #116480, #164122, #145776, #211777, #115423, #99120, #15705, #213890, #64481, #17825, #83908, #1569, #196614, #133777, #101228, #88191, #35151, #86052, #201900, #185670, #89276, #54619, #23161, #138018, #70836, #200834, #68708, #6908, #184602, #120767, #22079, #152128, #151073, #55682, #154264, #39436, #167310, #103373, #71909, #19968, #36219, #134831, #169435, #119684, #37299, #204033, #105529, #117550, #38368, #72985, #3697, #102298, #168372, #69773, #135881, #18897, #53552, #52485, #21019, #121838, #87116, #153187, #4760, #187810, #136953, #171563, #202978, #186746, #104448, #170496, #118615, #2636, #5838, #155324, #139089, #183544, #84981, #205116, #10127, #59953, #61025, #107710, #74078, #159591, #125047, #76202, #90332, #77270, #11190, #173736, #9071, #142312, #41599, #208322, #58893, #43733, #40522, #25314, #24230, #26379, #75145, #191002, #108777, #57820, #106626, #123982, #156401, #141255, #93547, #172655, #92492, #56759, #209381, #122923, #157476, #126108, #7989, #140170, #207263, #174803, #42669, #192068, #188881, #91415, #158530, #109847, #175861, #143382, #27449, #127186, #189950, #206192, #187451, #170135, #71552, #19615, #89979, #87831, #156029, #86759, #72628, #85687, #6550, #168010, #4406, #120402, #104086, #7619, #39079, #73705, #56396, #203681, #119324, #201547, #139801, #103015, #105164, #154965, #70477, #69416, #188518 ),
 ( #122557, #172285, #35870, #171203, #205830, #136592, #169070, #152828, #202615, #54266, #151775, #186378, #53193, #38014, #40149, #153902, #21720, #5471, #106263, #137660, #204745, #20669, #55329, #121480, #22795, #185309, #135523, #138727, #88911, #23873, #101945, #3347, #57461, #123622, #36931, #211151, #9765, #124679, #29227, #159218, #28154, #74780, #161368, #95320, #75839, #191701, #94250, #158173, #176543, #93185, #61723, #24943, #141946, #140880, #126810, #43361, #10818, #209010, #174433, #91047, #26010, #8697, #109482, #111608, #157107, #44425, #189586, #79029, #41232, #207958, #110542, #206893, #107339, #59584, #76892, #175491, #11891, #62775, #58524, #27078, #143016, #125741, #12951, #60647, #160289, #190637, #145145, #173361, #192766, #77966, #144087, #210084, #127891, #193842, #45491, #42297, #177619, #108411, #92120, #197043, #32420, #148312, #113741, #178681, #179745, #162432, #48680, #50796, #30295, #198101, #128937, #18277, #194915, #147248, #49730, #96380, #46552, #213279, #16135, #114796, #165617, #2012, #14008, #131055, #164550, #64906, #82221, #99552, #180795, #80094, #146198, #214311, #65943, #98486, #132092, #112672, #182924, #115858, #34540, #31363, #17205, #212212, #83281, #63848, #97439, #181843, #33479, #100610, #149366, #166686, #948, #67014, #130005, #195995, #84360, #47630, #133149, #199152, #163495, #15078, #116924, #150450, #81167, #86196, #150145, #82987, #166379, #17971, #20110, #183692, #168510, #102442, #202036, #35299, #68852, #152268, #84059, #120911, #136024, #137093, #4903, #1717, #203120, #199930, #151211, #3840, #34240, #100312, #186884, #16907, #149062, #69913, #53698, #87264, #67773, #133923, #54762, #119829, #51576, #185808, #99264, #50502, #198855, #103519, #37441, #169577, #117701, #101376, #167450, #19045, #36367, #85124, #134972, #639, #153330, #2781, #70981, #200980, #21160, #66703, #165312, #132850, #52627, #118755, #184739, #116624, #182618, #158674, #59028, #206336, #121984, #204171, #142454, #105680, #41743, #157617, #73125, #72052, #191147, #141399, #154402, #39577, #9214, #207409, #155465, #171708, #55828, #24370, #40668, #106771, #125186, #174943, #38516, #173880, #208462, #7049, #23306, #89417, #139226, #205257, #22224, #56898, #187950, #123073, #42814, #156547, #189027, #172799, #108920, #90482, #26524, #8141, #74223, #140319, #57963, #124128, #138163, #75285, #91563, #190090, #104594, #170640, #107854, #25455, #92633, #60096, #10271, #76347, #126254, #88338, #5981, #77414, #164015, #31881, #78478, #194365, #30820, #160808, #179197, #95829, #64370, #27595, #12399, #143529, #129461, #46007, #161886, #211665, #177057, #93694, #28674, #11334, #112127, #114260, #159736, #47074, #192213, #81676, #43876, #210612, #113191, #209525, #109991, #62239, #79550, #178130, #14528, #65402, #61166, #29746, #13473, #128398, #145668, #162950, #63301, #127329, #193298, #195444, #180257, #94760, #144597, #147762, #96899, #44943, #80625, #176003, #111051, #146716, #196505, #212732, #48147, #130516, #97958, #15589, #213779, #1460, #148814, #118509, #82741, #184492, #35042, #83800, #197551, #36111, #103266, #135774, #101113, #2525, #150961, #133669, #18788, #102194, #50249, #199672, #4655, #49194, #19861, #153078, #132599, #168261, #200730, #69667, #53438, #37189, #85947, #3590, #68601 ),
 ( #84872, #152022, #51316, #99007, #181305, #134724, #52381, #117443, #167200, #115315, #185561, #183438, #169327, #182359, #201797, #32932, #119575, #165062, #100063, #67525, #20912, #87007, #131549, #16655, #386, #66458, #198604, #116371, #33988, #166126, #17712, #149893, #105423, #104339, #8955, #173629, #186636, #71798, #41487, #25200, #187700, #137911, #21971, #56652, #72876, #138984, #91305, #207155, #70726, #206081, #174691, #39328, #203931, #121734, #171460, #23049, #54512, #89165, #88080, #155219, #157363, #188772, #6800, #205005, #75031, #122814, #141143, #57715, #5721, #55579, #158417, #202865, #120657, #123873, #189839, #58779, #40412, #106514, #26265, #73965, #172541, #140059, #136839, #154153, #170383, #124932, #190895, #42559, #24126, #90228, #156292, #7877, #107598, #108662, #92383, #38262, #211416, #128145, #176799, #76094, #129213, #196254, #14271, #194106, #95582, #29490, #12154, #111873, #195189, #143277, #78226, #97704, #142197, #112938, #31628, #11078, #46824, #79299, #162699, #146462, #130264, #178951, #96644, #161631, #77155, #210349, #13224, #110796, #145415, #27338, #10019, #144348, #94509, #209267, #80366, #60913, #61989, #127071, #93440, #64122, #212478, #193032, #30564, #44688, #45754, #177878, #47899, #180006, #114011, #28416, #208212, #63046, #160547, #59843, #125995, #191953, #43621, #109737, #175745, #159479, #185307, #118258, #168009, #115062, #17466, #213532, #201544, #133414, #165879, #83550, #52131, #199421, #53192, #150712, #140, #147512, #16404, #82482, #84621, #33736, #18545, #166954, #184242, #99814, #51064, #2273, #148571, #36930, #200485, #119322, #69415, #66205, #163763, #49996, #1213, #35868, #68349, #67276, #15341, #65154, #149631, #117187, #183188, #34793, #134481, #100868, #131312, #197303, #101944, #19614, #85686, #151774, #48943, #3346, #135522, #81431, #132351, #181059, #32677, #98755, #164812, #198356, #116118, #182107, #74779, #40148, #8696, #123621, #56394, #186376, #54265, #206892, #170134, #106261, #7618, #137659, #136591, #41230, #205829, #4404, #104085, #73703, #57460, #5469, #21718, #120401, #88910, #105163, #171202, #189583, #24942, #103013, #23871, #58522, #71551, #87830, #153900, #203679, #55328, #86758, #121479, #38013, #187450, #107338, #6548, #39078, #22793, #173360, #154964, #91046, #72627, #138726, #204743, #122556, #188517, #202614, #139800, #156028, #172284, #169068, #20667, #89978, #157105, #140879, #124678, #190636, #152827, #70475, #11890, #95319, #141944, #14007, #96379, #143014, #44424, #161367, #10816, #29226, #160287, #128935, #92119, #76891, #207957, #193841, #110541, #77965, #61722, #27077, #158172, #93183, #75838, #176541, #178680, #9764, #111606, #42296, #146197, #108409, #60646, #177616, #59583, #174430, #112671, #144086, #26008, #162431, #94247, #80093, #159216, #79028, #125739, #12950, #191700, #209009, #126808, #28153, #212211, #45490, #63847, #62773, #210083, #43360, #109481, #130003, #175490, #145144, #211150, #192764, #127890, #194913, #46550, #30294, #197042, #166684, #150449, #98484, #48678, #147247, #181841, #198099, #49727, #2011, #117994, #195994, #116922, #85425, #164549, #114795, #32418, #16134, #82219, #179744, #148311, #213277, #65940, #68079, #99550, #214310, #132090, #134214, #115856, #200223, #180794, #33477, #165614, #17203, #64905 ) ),
 .UNSPECIFIED., .T., .F., .F. ) 
 B_SPLINE_SURFACE_WITH_KNOTS ( ( 4, 3, 4 ),
 ( 4, 1, 1, 1, 1, 1, 1, 1, 1, 1, 1, 1, 1, 1, 1, 1, 1, 1, 1, 1, 1, 1, 1, 1, 1, 1, 1, 1, 1, 1, 1, 1, 1, 1, 1, 1, 1, 1, 1, 1, 1, 1, 1, 1, 1, 1, 1, 1, 1, 1, 1, 1, 1, 1, 1, 1, 1, 1, 1, 1, 1, 1, 1, 1, 1, 1, 1, 1, 1, 1, 1, 1, 1, 1, 1, 1, 1, 1, 1, 1, 1, 1, 1, 1, 1, 1, 1, 1, 1, 1, 1, 1, 1, 1, 1, 1, 1, 1, 1, 1, 1, 1, 1, 1, 1, 1, 1, 1, 1, 1, 1, 1, 1, 1, 1, 1, 1, 1, 1, 1, 1, 1, 1, 1, 1, 1, 1, 1, 1, 1, 1, 1, 1, 1, 1, 1, 1, 1, 1, 1, 1, 1, 1, 1, 1, 1, 1, 1, 1, 1, 1, 1, 1, 1, 1, 1, 1, 1, 1, 1, 1, 1, 1, 1, 1, 1, 1, 1, 1, 1, 1, 1, 1, 1, 1, 1, 1, 1, 1, 1, 1, 1, 1, 1, 1, 1, 1, 1, 1, 1, 1, 1, 1, 1, 1, 1, 1, 1, 1, 1, 1, 1, 1, 1, 1, 1, 1, 1, 1, 1, 1, 1, 1, 1, 1, 1, 1, 1, 1, 1, 1, 1, 1, 1, 1, 1, 1, 1, 1, 1, 1, 1, 1, 1, 1, 1, 1, 1, 1, 1, 1, 1, 1, 1, 1, 1, 1, 1, 1, 1, 1, 1, 1, 1, 1, 1, 1, 1, 1, 1, 1, 1, 1, 1, 1, 1, 1, 1, 1, 1, 1, 1, 1, 1, 1, 1, 1, 1, 1, 1, 1, 1, 1, 1, 1, 1, 1, 1, 1, 1, 1, 1, 1, 1, 1, 1, 1, 1, 1, 1, 1, 1, 1, 1, 1, 1, 1, 1, 1, 1, 1, 1, 1, 1, 1, 1, 1, 1, 1, 1, 1, 1, 1, 1, 1, 1, 1, 1, 1, 1, 1, 1, 1, 1, 1, 1, 1, 1, 1, 1, 1, 1, 1, 1, 1, 1, 1, 1, 1, 1, 1, 1, 1, 1, 1, 1, 1, 1, 1, 1, 1, 1, 1, 1, 1, 1, 1, 1, 1, 1, 1, 1, 1, 1, 1, 1, 1, 1, 1, 1, 1, 1, 1, 1, 4 ),
 ( 0.000000000000000000, 0.5000000000000000000, 1.000000000000000000 ),
 ( 0.000000000000000000, 0.002600154539856827565, 0.005208839490340733125, 0.007813275572638063438, 0.01041576435696154809, 0.01302135854728175661, 0.01562456786780599440, 0.01822932761385693060, 0.02083324874646079461, 0.02343713590986815087, 0.02604192363554110393, 0.02864519953128016536, 0.03125045858075606309, 0.03385359029894085409, 0.03645870005206112291, 0.03906221013386886737, 0.04166657361863843057, 0.04427092160485841116, 0.04687444683368256759, 0.04947954930481244379, 0.05208268618576387260, 0.05468794662449812799, 0.05729120536831356497, 0.05989601299138836571, 0.06249988999545372931, 0.06510378435733490954, 0.06770858081828938502, 0.07031184975024351580, 0.07291710771924506118, 0.07552024060328325905, 0.07812534933470290099, 0.08072885870519988516, 0.08333322157114708695, 0.08593756915452624434, 0.08854109358761537429, 0.09114619558392741960, 0.09374933183658358538, 0.09635459170495851156, 0.09895784999447977681, 0.1015626569530685003, 0.1041665336043751944, 0.1067704272253022224, 0.1093752232910748662, 0.1119784915631429623, 0.1145837490571069844, 0.1171868814509031548, 0.1197919896162490533, 0.1223954986480551566, 0.1249998608471283579, 0.1276042081199000311, 0.1302077318846941445, 0.1328128334964322199, 0.1354159692195129883, 0.1380212286176593917, 0.1406244865514671982, 0.1432292929439143159, 0.1458331693420142072, 0.1484370623210626572, 0.1510418580899855479, 0.1536451258019158050, 0.1562503829188521542, 0.1588535149221727560, 0.1614586226195926788, 0.1640621314121666618, 0.1666664930431534797, 0.1692708401040713406, 0.1718743633000545112, 0.1744794646253388370, 0.1770825999186152189, 0.1796878589445308205, 0.1822911166222762891, 0.1848959225469683498, 0.1874997987909985397, 0.1901036912273387502, 0.1927084867977703619, 0.1953117540492253223, 0.1979170108871138589, 0.2005201425997050479, 0.2031252499273119572, 0.2057287585800815777, 0.2083331197417381819, 0.2109374666895270922, 0.2135409894161511279, 0.2161460905530729892, 0.2187492255162853672, 0.2213544842679382729, 0.2239577417892439637, 0.2265625473445374016, 0.2291664235336075273, 0.2317703155263790282, 0.2343751109966507595, 0.2369783778872631419, 0.2395836345440564008, 0.2421867660656364940, 0.2447918731215153465, 0.2473953817338825356, 0.2499997425249363969, 0.2526040894582959329, 0.2552076118149841921, 0.2578127128616094499, 0.2604158475944712281, 0.2630211061698037311, 0.2656243636342671688, 0.2682291689184919115, 0.2708330451516883230, 0.2734369368000036937, 0.2760417322684234342, 0.2786449988978000336, 0.2812502554714267355, 0.2838533869016899303, 0.2864584937839013135, 0.2890620024552456591, 0.2916663629743991848, 0.2942707099920074398, 0.2968742320781582733, 0.2994793331325310004, 0.3020824677347322962, 0.3046877262316646240, 0.3072909837388622112, 0.3098957888503254821, 0.3124996652267145181, 0.3151035566296633839, 0.3177083521945192612, 0.3203116186622446127, 0.3229168752506134110, 0.3255200066892336430, 0.3281251134958176330, 0.3307286223255002655, 0.3333329826714347410, 0.3359373298719517953, 0.3385408517869427647, 0.3411459529470890484, 0.3437490875183005223, 0.3463543460347343617, 0.3489576036842249041, 0.3515624087212146920, 0.3541662853398466204, 0.3567701765964986227, 0.3593749723560626386, 0.3619782387617029862, 0.3645834954627060198, 0.3671866270093405715, 0.3697917338383204244, 0.3723952429256875973, 0.3749996031970665444, 0.3776039506791386557, 0.3802074725223298923, 0.3828125738862612759, 0.3854157085261381011, 0.3880209671599602617, 0.3906242250512887426, 0.3932290301120778819, 0.3958329070719905363, 0.3984367982813996067, 0.4010415943339316058, 0.4036448607770379837, 0.4062501176885546794, 0.4088532494428480657, 0.4114583563922335485, 0.4140618658366201910, 0.4166662261320933647, 0.4192705739943561327, 0.4218740958650940009, 0.4244791975308115917, 0.4270823323389966175, 0.4296875911880828069, 0.4322908494207843844, 0.4348956546036337745, 0.4374995320038561619, 0.4401034232650644085, 0.4427082197088152427, 0.4453114862889279713, 0.4479167435088288185, 0.4505198755704162283, 0.4531249827382076711, 0.4557284926389418844, 0.4583328530571487147, 0.4609372013982309668, 0.4635407233958523388, 0.4661458254613498609, 0.4687489605374778323, 0.4713542196996960976, 0.4739574783732994345, 0.4765622837764619812, 0.4791661617160185016, 0.4817700531280592058, 0.4843748500612748420, 0.4869781168779269698, 0.4895833745040767959, 0.4921865069725880892, 0.4947916144567798824, 0.4973951249131855490, 0.4999994855527590265, 0.5026038344712867589, 0.5052073566951218453, 0.5078124592583899144, 0.5104155947020908579, 0.5130208542753056378, 0.5156241134893367883, 0.5182289192110610676, 0.5208327977889742888, 0.5234366894508762913, 0.5260414869718011976, 0.5286447541245218318, 0.5312500122547839654, 0.5338531452298473923, 0.5364582531284315392, 0.5390617642398328746, 0.5416661251994032700, 0.5442704747940029231, 0.5468739973433798252, 0.5494791005024090014, 0.5520822364133124438, 0.5546874964953879550, 0.5572907563493740835, 0.5598955624879079496, 0.5624994418032033261, 0.5651033338139942463, 0.5677081320208752224, 0.5703113996091939697, 0.5729166583414331271, 0.5755197919226788805, 0.5781249003336490500, 0.5807284121993739889, 0.5833327735775721834, 0.5859371239468746939, 0.5885406469211225122, 0.5911457507739076300, 0.5937488872516457628, 0.5963541479404496082, 0.5989574085339228748, 0.6015622151875171797, 0.6041660953392257172, 0.6067699877979360057, 0.6093747867890261238, 0.6119780549124759217, 0.6145833143445629254, 0.6171864486316270826, 0.6197915576529816617, 0.6223950703723655220, 0.6249994322678273928, 0.6276037835104713025, 0.6302073070089242446, 0.6328124116534677990, 0.6354155487976793637, 0.6380208101910863627, 0.6406240716235875876, 0.6432288788904997334, 0.6458327599776627626, 0.6484366529833293091, 0.6510414528568908565, 0.6536447216150126360, 0.6562499818448275235, 0.6588531169373553764, 0.6614582266671018562, 0.6640617403394915019, 0.6666661028508605868, 0.6692704550654967610, 0.6718739791874978051, 0.6744790847218130603, 0.6770822226321474568, 0.6796874848280434200, 0.6822907471991253026, 0.6848955551776233497, 0.6874994372992955238, 0.6901033309509650993, 0.6927081318052739078, 0.6953114012976200353, 0.6979166624230551674, 0.7005197984207056638, 0.7031249089568636368, 0.7057284236816204759, 0.7083327869075525252, 0.7109371401928469281, 0.7135406650377511539, 0.7161457715598668061, 0.7187489103359874232, 0.7213541734322722609, 0.7239574368415039318, 0.7265622456298695964, 0.7291661288851226663, 0.7317700232818561412, 0.7343748252152053624, 0.7369780955413426371, 0.7395833576603073611, 0.7421864946627563242, 0.7447916061033615920, 0.7473951219798656842, 0.7499994860190324353, 0.7526038404736700160, 0.7552073661408488237, 0.7578124737488122209, 0.7604156134903999886, 0.7630208775849919300, 0.7656241421319622820, 0.7682289518284949326, 0.7708328363164217434, 0.7734367315572975299, 0.7760415346680002990, 0.7786448059275148381, 0.7812500691379388185, 0.7838532072448821664, 0.7864583196879902927, 0.7890618368156444573, 0.7916662017667361884, 0.7942705574894247667, 0.7968740840782696511, 0.7994791928701499018, 0.8020823336769073997, 0.8046875988677468783, 0.8072908646520678966, 0.8098956753550886623, 0.8124995611748068169, 0.8151034573589240884, 0.8177082617453185209, 0.8203115340378186460, 0.8229167984376549727, 0.8255199377488137147, 0.8281250512925039109, 0.8307285697707365024, 0.8333329357324672504, 0.8359372928219411802, 0.8385408204318668401, 0.8411459305057594760, 0.8437490724774151518, 0.8463543388624672481, 0.8489576059837783406, 0.8515624177916331083, 0.8541663050422881875, 0.8567702022687715413, 0.8593750080292236193, 0.8619782814543437421, 0.8645835471415733720, 0.8671866877566964948, 0.8697918024990743957, 0.8723953224273439666, 0.8749996894984543028, 0.8776040480534781363, 0.8802075767839265819, 0.8828126882379567775, 0.8854158314742670566, 0.8880210991515266050, 0.8906243677094983768, 0.8932291807205616774, 0.8958330695013316802, 0.8984369678693342465, 0.9010417751022415933, 0.9036450497596462128, 0.9062503168322812996, 0.9088534588511494317, 0.9114585748903522022, 0.9140620963681507227, 0.9166664646474114164, 0.9192708247667824573, 0.9218743547172278952, 0.9244794676495572405, 0.9270826122503010858, 0.9296878813177945622, 0.9322911514121841048, 0.9348959657248061550, 0.9374998561347748227, 0.9401037557438677306, 0.9427085645475906661, 0.9453118405358371668, 0.9479171090940153865, 0.9505202526155902554, 0.9531253700418979014, 0.9557288931959170286, 0.9583332627756006028, 0.9609376244112938226, 0.9635411559431285022, 0.9661462708106475228, 0.9687494151757961580, 0.9713546862302190332, 0.9739579640138142924, 0.9765627705390533819, 0.9791666547386930208, 0.9817705986233274951, 0.9843753609709087193, 0.9869785915570626900, 0.9895841932699848131, 0.9921866851465583892, 0.9947911401134668097, 0.9973998225951543617, 1.000000000000000000 ),
 .UNSPECIFIED. ) 
 GEOMETRIC_REPRESENTATION_ITEM ( )  RATIONAL_B_SPLINE_SURFACE ( (
 ( 1.000000000000000000, 1.000000000000000000, 1.000000000000000222, 1.000000000000000000, 0.9999999999999996669, 1.000000000000000444, 0.9999999999999997780, 1.000000000000000000, 1.000000000000000222, 0.9999999999999996669, 1.000000000000000222, 0.9999999999999996669, 1.000000000000000000, 0.9999999999999997780, 1.000000000000000222, 0.9999999999999997780, 1.000000000000000222, 1.000000000000000222, 0.9999999999999997780, 1.000000000000000222, 1.000000000000000222, 0.9999999999999996669, 1.000000000000000444, 0.9999999999999997780, 1.000000000000000000, 1.000000000000000222, 1.000000000000000000, 1.000000000000000000, 1.000000000000000000, 1.000000000000000000, 1.000000000000000222, 1.000000000000000000, 1.000000000000000000, 0.9999999999999997780, 1.000000000000000000, 1.000000000000000000, 1.000000000000000000, 1.000000000000000000, 0.9999999999999997780, 1.000000000000000222, 1.000000000000000000, 1.000000000000000000, 1.000000000000000444, 0.9999999999999997780, 1.000000000000000222, 0.9999999999999996669, 1.000000000000000444, 0.9999999999999997780, 1.000000000000000000, 0.9999999999999997780, 1.000000000000000000, 1.000000000000000222, 0.9999999999999997780, 1.000000000000000444, 0.9999999999999997780, 1.000000000000000000, 0.9999999999999996669, 1.000000000000000444, 0.9999999999999997780, 1.000000000000000444, 1.000000000000000000, 1.000000000000000444, 0.9999999999999996669, 1.000000000000000000, 0.9999999999999996669, 1.000000000000000444, 0.9999999999999997780, 1.000000000000000000, 1.000000000000000000, 1.000000000000000000, 1.000000000000000000, 0.9999999999999996669, 1.000000000000000000, 1.000000000000000222, 0.9999999999999997780, 1.000000000000000000, 0.9999999999999997780, 0.9999999999999997780, 1.000000000000000000, 1.000000000000000222, 0.9999999999999997780, 1.000000000000000000, 1.000000000000000222, 1.000000000000000222, 1.000000000000000222, 0.9999999999999997780, 1.000000000000000000, 1.000000000000000222, 0.9999999999999997780, 1.000000000000000222, 1.000000000000000222, 0.9999999999999997780, 0.9999999999999997780, 0.9999999999999997780, 1.000000000000000444, 1.000000000000000000, 1.000000000000000000, 1.000000000000000000, 1.000000000000000222, 0.9999999999999997780, 1.000000000000000000, 1.000000000000000444, 0.9999999999999996669, 1.000000000000000444, 1.000000000000000000, 1.000000000000000000, 1.000000000000000222, 0.9999999999999997780, 1.000000000000000444, 0.9999999999999996669, 1.000000000000000444, 1.000000000000000000, 0.9999999999999997780, 1.000000000000000222, 0.9999999999999996669, 1.000000000000000222, 1.000000000000000000, 1.000000000000000222, 0.9999999999999997780, 1.000000000000000222, 0.9999999999999996669, 1.000000000000000222, 1.000000000000000222, 1.000000000000000222, 1.000000000000000000, 0.9999999999999997780, 1.000000000000000000, 0.9999999999999997780, 1.000000000000000000, 0.9999999999999997780, 0.9999999999999997780, 1.000000000000000222, 1.000000000000000222, 1.000000000000000222, 0.9999999999999997780, 0.9999999999999997780, 1.000000000000000444, 0.9999999999999997780, 1.000000000000000000, 0.9999999999999997780, 1.000000000000000000, 0.9999999999999997780, 1.000000000000000222, 1.000000000000000000, 1.000000000000000000, 1.000000000000000222, 1.000000000000000000, 0.9999999999999997780, 1.000000000000000444, 1.000000000000000000, 1.000000000000000000, 1.000000000000000444, 0.9999999999999997780, 1.000000000000000222, 0.9999999999999997780, 1.000000000000000444, 1.000000000000000000, 1.000000000000000222, 0.9999999999999997780, 0.9999999999999997780, 1.000000000000000000, 1.000000000000000444, 0.9999999999999996669, 1.000000000000000000, 1.000000000000000222, 1.000000000000000222, 0.9999999999999997780, 1.000000000000000222, 0.9999999999999997780, 1.000000000000000222, 1.000000000000000000, 1.000000000000000000, 0.9999999999999997780, 1.000000000000000444, 0.9999999999999997780, 1.000000000000000222, 0.9999999999999996669, 1.000000000000000444, 0.9999999999999996669, 1.000000000000000222, 1.000000000000000000, 1.000000000000000000, 1.000000000000000000, 1.000000000000000444, 1.000000000000000222, 0.9999999999999997780, 1.000000000000000444, 0.9999999999999997780, 1.000000000000000000, 0.9999999999999996669, 1.000000000000000000, 0.9999999999999996669, 1.000000000000000000, 1.000000000000000222, 1.000000000000000000, 0.9999999999999997780, 1.000000000000000222, 1.000000000000000000, 1.000000000000000222, 0.9999999999999996669, 1.000000000000000000, 1.000000000000000000, 1.000000000000000000, 0.9999999999999997780, 1.000000000000000000, 1.000000000000000000, 1.000000000000000222, 1.000000000000000000, 1.000000000000000000, 0.9999999999999997780, 1.000000000000000000, 1.000000000000000222, 0.9999999999999997780, 1.000000000000000000, 1.000000000000000222, 1.000000000000000000, 1.000000000000000000, 0.9999999999999997780, 0.9999999999999997780, 1.000000000000000000, 1.000000000000000000, 0.9999999999999997780, 1.000000000000000000, 1.000000000000000000, 1.000000000000000000, 1.000000000000000222, 1.000000000000000000, 1.000000000000000000, 0.9999999999999997780, 1.000000000000000000, 0.9999999999999997780, 1.000000000000000444, 0.9999999999999997780, 1.000000000000000222, 0.9999999999999997780, 1.000000000000000444, 0.9999999999999994449, 1.000000000000000444, 0.9999999999999997780, 1.000000000000000222, 1.000000000000000000, 1.000000000000000000, 0.9999999999999997780, 1.000000000000000000, 1.000000000000000000, 0.9999999999999997780, 1.000000000000000000, 1.000000000000000000, 0.9999999999999997780, 1.000000000000000222, 1.000000000000000000, 1.000000000000000222, 0.9999999999999997780, 1.000000000000000222, 0.9999999999999997780, 1.000000000000000222, 0.9999999999999997780, 1.000000000000000444, 0.9999999999999996669, 1.000000000000000222, 0.9999999999999997780, 1.000000000000000000, 1.000000000000000000, 1.000000000000000000, 1.000000000000000222, 1.000000000000000222, 1.000000000000000000, 1.000000000000000444, 1.000000000000000222, 0.9999999999999997780, 1.000000000000000222, 0.9999999999999996669, 1.000000000000000444, 0.9999999999999997780, 0.9999999999999997780, 1.000000000000000222, 1.000000000000000000, 1.000000000000000222, 1.000000000000000000, 1.000000000000000000, 1.000000000000000222, 1.000000000000000000, 0.9999999999999997780, 1.000000000000000222, 0.9999999999999997780, 1.000000000000000000, 1.000000000000000222, 1.000000000000000000, 0.9999999999999997780, 0.9999999999999997780, 1.000000000000000000, 0.9999999999999997780, 1.000000000000000000, 1.000000000000000000, 1.000000000000000000, 1.000000000000000222, 0.9999999999999997780, 1.000000000000000000, 1.000000000000000222, 1.000000000000000000, 0.9999999999999997780, 1.000000000000000000, 1.000000000000000000, 1.000000000000000222, 0.9999999999999997780, 1.000000000000000222, 1.000000000000000000, 1.000000000000000000, 1.000000000000000222, 1.000000000000000000, 1.000000000000000000, 1.000000000000000222, 1.000000000000000000, 1.000000000000000444, 0.9999999999999996669, 1.000000000000000444, 0.9999999999999997780, 1.000000000000000000, 1.000000000000000222, 0.9999999999999996669, 1.000000000000000444, 1.000000000000000000, 1.000000000000000000, 1.000000000000000222, 1.000000000000000444, 1.000000000000000000, 0.9999999999999996669, 1.000000000000000444, 0.9999999999999997780, 0.9999999999999997780, 0.9999999999999997780, 1.000000000000000222, 1.000000000000000000, 0.9999999999999996669, 1.000000000000000222, 1.000000000000000000, 1.000000000000000444, 0.9999999999999997780, 1.000000000000000000, 1.000000000000000222, 1.000000000000000222, 1.000000000000000222, 1.000000000000000222, 1.000000000000000000, 1.000000000000000000, 1.000000000000000000, 1.000000000000000000, 1.000000000000000000, 1.000000000000000444, 1.000000000000000000, 0.9999999999999997780, 1.000000000000000000, 1.000000000000000222, 1.000000000000000000, 1.000000000000000222, 1.000000000000000222, 1.000000000000000000, 0.9999999999999997780, 0.9999999999999997780, 1.000000000000000222, 0.9999999999999997780, 1.000000000000000000, 1.000000000000000222, 1.000000000000000000, 1.000000000000000222, 1.000000000000000000, 0.9999999999999997780, 1.000000000000000000, 0.9999999999999997780, 1.000000000000000222, 1.000000000000000000, 0.9999999999999997780, 0.9999999999999997780, 1.000000000000000222, 1.000000000000000000, 1.000000000000000222, 0.9999999999999996669, 1.000000000000000000, 1.000000000000000222, 0.9999999999999997780, 1.000000000000000000, 1.000000000000000000, 1.000000000000000222, 1.000000000000000222, 1.000000000000000000, 1.000000000000000222, 1.000000000000000222),
 ( 0.3333333333333333703, 0.3333333333333333703, 0.3333333333333333703, 0.3333333333333333703, 0.3333333333333333148, 0.3333333333333334259, 0.3333333333333333703, 0.3333333333333333148, 0.3333333333333334259, 0.3333333333333333148, 0.3333333333333334259, 0.3333333333333332038, 0.3333333333333333703, 0.3333333333333332593, 0.3333333333333333703, 0.3333333333333332593, 0.3333333333333334814, 0.3333333333333334259, 0.3333333333333333703, 0.3333333333333334259, 0.3333333333333334259, 0.3333333333333332038, 0.3333333333333335369, 0.3333333333333333148, 0.3333333333333333148, 0.3333333333333334259, 0.3333333333333333703, 0.3333333333333333148, 0.3333333333333334259, 0.3333333333333333148, 0.3333333333333335369, 0.3333333333333333148, 0.3333333333333334259, 0.3333333333333333148, 0.3333333333333334259, 0.3333333333333333703, 0.3333333333333333148, 0.3333333333333333703, 0.3333333333333334259, 0.3333333333333333703, 0.3333333333333334259, 0.3333333333333333703, 0.3333333333333334814, 0.3333333333333333148, 0.3333333333333334259, 0.3333333333333332593, 0.3333333333333335369, 0.3333333333333332593, 0.3333333333333334259, 0.3333333333333333148, 0.3333333333333333703, 0.3333333333333334259, 0.3333333333333333148, 0.3333333333333334814, 0.3333333333333332593, 0.3333333333333333703, 0.3333333333333332593, 0.3333333333333335369, 0.3333333333333333148, 0.3333333333333334259, 0.3333333333333334259, 0.3333333333333334259, 0.3333333333333333148, 0.3333333333333333148, 0.3333333333333333703, 0.3333333333333333703, 0.3333333333333333703, 0.3333333333333334259, 0.3333333333333333148, 0.3333333333333333703, 0.3333333333333333703, 0.3333333333333332593, 0.3333333333333334259, 0.3333333333333333703, 0.3333333333333333703, 0.3333333333333333148, 0.3333333333333333148, 0.3333333333333334259, 0.3333333333333333148, 0.3333333333333334259, 0.3333333333333333148, 0.3333333333333334259, 0.3333333333333333703, 0.3333333333333334259, 0.3333333333333333703, 0.3333333333333333703, 0.3333333333333333148, 0.3333333333333335369, 0.3333333333333332593, 0.3333333333333334814, 0.3333333333333333703, 0.3333333333333333703, 0.3333333333333333148, 0.3333333333333333703, 0.3333333333333334259, 0.3333333333333334259, 0.3333333333333333148, 0.3333333333333333703, 0.3333333333333334259, 0.3333333333333333148, 0.3333333333333333703, 0.3333333333333334814, 0.3333333333333332038, 0.3333333333333334814, 0.3333333333333333703, 0.3333333333333333148, 0.3333333333333334259, 0.3333333333333333148, 0.3333333333333334259, 0.3333333333333332593, 0.3333333333333333703, 0.3333333333333334259, 0.3333333333333333148, 0.3333333333333333703, 0.3333333333333333148, 0.3333333333333334259, 0.3333333333333333703, 0.3333333333333333703, 0.3333333333333333703, 0.3333333333333334259, 0.3333333333333332038, 0.3333333333333334259, 0.3333333333333334259, 0.3333333333333333703, 0.3333333333333333703, 0.3333333333333332593, 0.3333333333333333703, 0.3333333333333333148, 0.3333333333333334259, 0.3333333333333332593, 0.3333333333333334259, 0.3333333333333333703, 0.3333333333333334259, 0.3333333333333334259, 0.3333333333333333148, 0.3333333333333334259, 0.3333333333333334259, 0.3333333333333332593, 0.3333333333333334259, 0.3333333333333333703, 0.3333333333333333703, 0.3333333333333333148, 0.3333333333333334259, 0.3333333333333333703, 0.3333333333333334259, 0.3333333333333334259, 0.3333333333333333703, 0.3333333333333333703, 0.3333333333333334814, 0.3333333333333333703, 0.3333333333333333703, 0.3333333333333335369, 0.3333333333333332593, 0.3333333333333334259, 0.3333333333333333148, 0.3333333333333334259, 0.3333333333333334259, 0.3333333333333334259, 0.3333333333333332593, 0.3333333333333333148, 0.3333333333333333703, 0.3333333333333334259, 0.3333333333333333148, 0.3333333333333333703, 0.3333333333333333148, 0.3333333333333334259, 0.3333333333333333148, 0.3333333333333334259, 0.3333333333333333148, 0.3333333333333334259, 0.3333333333333333703, 0.3333333333333334259, 0.3333333333333333703, 0.3333333333333334259, 0.3333333333333333148, 0.3333333333333333703, 0.3333333333333333703, 0.3333333333333334259, 0.3333333333333333703, 0.3333333333333334259, 0.3333333333333333703, 0.3333333333333333703, 0.3333333333333334259, 0.3333333333333334814, 0.3333333333333333703, 0.3333333333333333703, 0.3333333333333334814, 0.3333333333333333148, 0.3333333333333333703, 0.3333333333333333148, 0.3333333333333333703, 0.3333333333333333148, 0.3333333333333334259, 0.3333333333333334259, 0.3333333333333333703, 0.3333333333333333703, 0.3333333333333333703, 0.3333333333333333703, 0.3333333333333334259, 0.3333333333333332593, 0.3333333333333333703, 0.3333333333333333703, 0.3333333333333333703, 0.3333333333333333148, 0.3333333333333333703, 0.3333333333333333148, 0.3333333333333334259, 0.3333333333333333148, 0.3333333333333333703, 0.3333333333333333703, 0.3333333333333334259, 0.3333333333333333703, 0.3333333333333333148, 0.3333333333333333703, 0.3333333333333333703, 0.3333333333333333148, 0.3333333333333333703, 0.3333333333333333148, 0.3333333333333333703, 0.3333333333333333703, 0.3333333333333334814, 0.3333333333333333148, 0.3333333333333334259, 0.3333333333333334259, 0.3333333333333333703, 0.3333333333333334259, 0.3333333333333333703, 0.3333333333333334259, 0.3333333333333332593, 0.3333333333333334259, 0.3333333333333333148, 0.3333333333333334259, 0.3333333333333333148, 0.3333333333333334259, 0.3333333333333332593, 0.3333333333333335369, 0.3333333333333332038, 0.3333333333333334259, 0.3333333333333333703, 0.3333333333333333148, 0.3333333333333334259, 0.3333333333333333148, 0.3333333333333333148, 0.3333333333333333148, 0.3333333333333334814, 0.3333333333333332593, 0.3333333333333334259, 0.3333333333333333148, 0.3333333333333333148, 0.3333333333333334814, 0.3333333333333333703, 0.3333333333333334259, 0.3333333333333333148, 0.3333333333333333703, 0.3333333333333332593, 0.3333333333333334814, 0.3333333333333333148, 0.3333333333333334259, 0.3333333333333333148, 0.3333333333333334259, 0.3333333333333333703, 0.3333333333333333703, 0.3333333333333334259, 0.3333333333333333148, 0.3333333333333334814, 0.3333333333333333703, 0.3333333333333333703, 0.3333333333333334814, 0.3333333333333333703, 0.3333333333333332593, 0.3333333333333334259, 0.3333333333333332593, 0.3333333333333334814, 0.3333333333333333148, 0.3333333333333333703, 0.3333333333333333703, 0.3333333333333334259, 0.3333333333333333703, 0.3333333333333333703, 0.3333333333333333148, 0.3333333333333334259, 0.3333333333333334259, 0.3333333333333333703, 0.3333333333333334259, 0.3333333333333333148, 0.3333333333333333703, 0.3333333333333334259, 0.3333333333333333703, 0.3333333333333333148, 0.3333333333333334259, 0.3333333333333333703, 0.3333333333333333148, 0.3333333333333333148, 0.3333333333333334259, 0.3333333333333333148, 0.3333333333333333703, 0.3333333333333333703, 0.3333333333333333703, 0.3333333333333334259, 0.3333333333333334259, 0.3333333333333333148, 0.3333333333333334259, 0.3333333333333333148, 0.3333333333333334814, 0.3333333333333332593, 0.3333333333333334814, 0.3333333333333333703, 0.3333333333333333703, 0.3333333333333334259, 0.3333333333333333703, 0.3333333333333333703, 0.3333333333333333703, 0.3333333333333333703, 0.3333333333333334814, 0.3333333333333333148, 0.3333333333333334259, 0.3333333333333333148, 0.3333333333333333703, 0.3333333333333333703, 0.3333333333333333703, 0.3333333333333335369, 0.3333333333333333703, 0.3333333333333333148, 0.3333333333333334814, 0.3333333333333334259, 0.3333333333333333148, 0.3333333333333333148, 0.3333333333333335369, 0.3333333333333332593, 0.3333333333333333703, 0.3333333333333333148, 0.3333333333333333703, 0.3333333333333333703, 0.3333333333333332593, 0.3333333333333334259, 0.3333333333333332593, 0.3333333333333335369, 0.3333333333333333148, 0.3333333333333333703, 0.3333333333333334259, 0.3333333333333333703, 0.3333333333333333703, 0.3333333333333334814, 0.3333333333333333148, 0.3333333333333333148, 0.3333333333333334259, 0.3333333333333333148, 0.3333333333333333703, 0.3333333333333334814, 0.3333333333333333703, 0.3333333333333333703, 0.3333333333333333703, 0.3333333333333333703, 0.3333333333333334814, 0.3333333333333333703, 0.3333333333333334814, 0.3333333333333333703, 0.3333333333333333703, 0.3333333333333333148, 0.3333333333333334259, 0.3333333333333333148, 0.3333333333333334259, 0.3333333333333333148, 0.3333333333333333703, 0.3333333333333334814, 0.3333333333333333148, 0.3333333333333333148, 0.3333333333333333703, 0.3333333333333333703, 0.3333333333333333703, 0.3333333333333334259, 0.3333333333333333148, 0.3333333333333333703, 0.3333333333333334259, 0.3333333333333333148, 0.3333333333333333703, 0.3333333333333332593, 0.3333333333333333703, 0.3333333333333334259, 0.3333333333333333703, 0.3333333333333333703, 0.3333333333333333703, 0.3333333333333333703, 0.3333333333333334814, 0.3333333333333333703, 0.3333333333333334259, 0.3333333333333334259),
 ( 0.3333333333333333703, 0.3333333333333333703, 0.3333333333333333703, 0.3333333333333333703, 0.3333333333333333148, 0.3333333333333334259, 0.3333333333333333703, 0.3333333333333333148, 0.3333333333333334259, 0.3333333333333333148, 0.3333333333333334259, 0.3333333333333332038, 0.3333333333333333703, 0.3333333333333332593, 0.3333333333333333703, 0.3333333333333332593, 0.3333333333333334814, 0.3333333333333334259, 0.3333333333333333703, 0.3333333333333334259, 0.3333333333333334259, 0.3333333333333332038, 0.3333333333333335369, 0.3333333333333333148, 0.3333333333333333148, 0.3333333333333334259, 0.3333333333333333703, 0.3333333333333333148, 0.3333333333333334259, 0.3333333333333333148, 0.3333333333333335369, 0.3333333333333333148, 0.3333333333333334259, 0.3333333333333333148, 0.3333333333333334259, 0.3333333333333333703, 0.3333333333333333148, 0.3333333333333333703, 0.3333333333333334259, 0.3333333333333333703, 0.3333333333333334259, 0.3333333333333333703, 0.3333333333333334814, 0.3333333333333333148, 0.3333333333333334259, 0.3333333333333332593, 0.3333333333333335369, 0.3333333333333332593, 0.3333333333333334259, 0.3333333333333333148, 0.3333333333333333703, 0.3333333333333334259, 0.3333333333333333148, 0.3333333333333334814, 0.3333333333333332593, 0.3333333333333333703, 0.3333333333333332593, 0.3333333333333335369, 0.3333333333333333148, 0.3333333333333334259, 0.3333333333333334259, 0.3333333333333334259, 0.3333333333333333148, 0.3333333333333333148, 0.3333333333333333703, 0.3333333333333333703, 0.3333333333333333703, 0.3333333333333334259, 0.3333333333333333148, 0.3333333333333333703, 0.3333333333333333703, 0.3333333333333332593, 0.3333333333333334259, 0.3333333333333333703, 0.3333333333333333703, 0.3333333333333333148, 0.3333333333333333148, 0.3333333333333334259, 0.3333333333333333148, 0.3333333333333334259, 0.3333333333333333148, 0.3333333333333334259, 0.3333333333333333703, 0.3333333333333334259, 0.3333333333333333703, 0.3333333333333333703, 0.3333333333333333148, 0.3333333333333335369, 0.3333333333333332593, 0.3333333333333334814, 0.3333333333333333703, 0.3333333333333333703, 0.3333333333333333148, 0.3333333333333333703, 0.3333333333333334259, 0.3333333333333334259, 0.3333333333333333148, 0.3333333333333333703, 0.3333333333333334259, 0.3333333333333333148, 0.3333333333333333703, 0.3333333333333334814, 0.3333333333333332038, 0.3333333333333334814, 0.3333333333333333703, 0.3333333333333333148, 0.3333333333333334259, 0.3333333333333333148, 0.3333333333333334259, 0.3333333333333332593, 0.3333333333333333703, 0.3333333333333334259, 0.3333333333333333148, 0.3333333333333333703, 0.3333333333333333148, 0.3333333333333334259, 0.3333333333333333703, 0.3333333333333333703, 0.3333333333333333703, 0.3333333333333334259, 0.3333333333333332038, 0.3333333333333334259, 0.3333333333333334259, 0.3333333333333333703, 0.3333333333333333703, 0.3333333333333332593, 0.3333333333333333703, 0.3333333333333333148, 0.3333333333333334259, 0.3333333333333332593, 0.3333333333333334259, 0.3333333333333333703, 0.3333333333333334259, 0.3333333333333334259, 0.3333333333333333148, 0.3333333333333334259, 0.3333333333333334259, 0.3333333333333332593, 0.3333333333333334259, 0.3333333333333333703, 0.3333333333333333703, 0.3333333333333333148, 0.3333333333333334259, 0.3333333333333333703, 0.3333333333333334259, 0.3333333333333334259, 0.3333333333333333703, 0.3333333333333333703, 0.3333333333333334814, 0.3333333333333333703, 0.3333333333333333703, 0.3333333333333335369, 0.3333333333333332593, 0.3333333333333334259, 0.3333333333333333148, 0.3333333333333334259, 0.3333333333333334259, 0.3333333333333334259, 0.3333333333333332593, 0.3333333333333333148, 0.3333333333333333703, 0.3333333333333334259, 0.3333333333333333148, 0.3333333333333333703, 0.3333333333333333148, 0.3333333333333334259, 0.3333333333333333148, 0.3333333333333334259, 0.3333333333333333148, 0.3333333333333334259, 0.3333333333333333703, 0.3333333333333334259, 0.3333333333333333703, 0.3333333333333334259, 0.3333333333333333148, 0.3333333333333333703, 0.3333333333333333703, 0.3333333333333334259, 0.3333333333333333703, 0.3333333333333334259, 0.3333333333333333703, 0.3333333333333333703, 0.3333333333333334259, 0.3333333333333334814, 0.3333333333333333703, 0.3333333333333333703, 0.3333333333333334814, 0.3333333333333333148, 0.3333333333333333703, 0.3333333333333333148, 0.3333333333333333703, 0.3333333333333333148, 0.3333333333333334259, 0.3333333333333334259, 0.3333333333333333703, 0.3333333333333333703, 0.3333333333333333703, 0.3333333333333333703, 0.3333333333333334259, 0.3333333333333332593, 0.3333333333333333703, 0.3333333333333333703, 0.3333333333333333703, 0.3333333333333333148, 0.3333333333333333703, 0.3333333333333333148, 0.3333333333333334259, 0.3333333333333333148, 0.3333333333333333703, 0.3333333333333333703, 0.3333333333333334259, 0.3333333333333333703, 0.3333333333333333148, 0.3333333333333333703, 0.3333333333333333703, 0.3333333333333333148, 0.3333333333333333703, 0.3333333333333333148, 0.3333333333333333703, 0.3333333333333333703, 0.3333333333333334814, 0.3333333333333333148, 0.3333333333333334259, 0.3333333333333334259, 0.3333333333333333703, 0.3333333333333334259, 0.3333333333333333703, 0.3333333333333334259, 0.3333333333333332593, 0.3333333333333334259, 0.3333333333333333148, 0.3333333333333334259, 0.3333333333333333148, 0.3333333333333334259, 0.3333333333333332593, 0.3333333333333335369, 0.3333333333333332038, 0.3333333333333334259, 0.3333333333333333703, 0.3333333333333333148, 0.3333333333333334259, 0.3333333333333333148, 0.3333333333333333148, 0.3333333333333333148, 0.3333333333333334814, 0.3333333333333332593, 0.3333333333333334259, 0.3333333333333333148, 0.3333333333333333148, 0.3333333333333334814, 0.3333333333333333703, 0.3333333333333334259, 0.3333333333333333148, 0.3333333333333333703, 0.3333333333333332593, 0.3333333333333334814, 0.3333333333333333148, 0.3333333333333334259, 0.3333333333333333148, 0.3333333333333334259, 0.3333333333333333703, 0.3333333333333333703, 0.3333333333333334259, 0.3333333333333333148, 0.3333333333333334814, 0.3333333333333333703, 0.3333333333333333703, 0.3333333333333334814, 0.3333333333333333703, 0.3333333333333332593, 0.3333333333333334259, 0.3333333333333332593, 0.3333333333333334814, 0.3333333333333333148, 0.3333333333333333703, 0.3333333333333333703, 0.3333333333333334259, 0.3333333333333333703, 0.3333333333333333703, 0.3333333333333333148, 0.3333333333333334259, 0.3333333333333334259, 0.3333333333333333703, 0.3333333333333334259, 0.3333333333333333148, 0.3333333333333333703, 0.3333333333333334259, 0.3333333333333333703, 0.3333333333333333148, 0.3333333333333334259, 0.3333333333333333703, 0.3333333333333333148, 0.3333333333333333148, 0.3333333333333334259, 0.3333333333333333148, 0.3333333333333333703, 0.3333333333333333703, 0.3333333333333333703, 0.3333333333333334259, 0.3333333333333334259, 0.3333333333333333148, 0.3333333333333334259, 0.3333333333333333148, 0.3333333333333334814, 0.3333333333333332593, 0.3333333333333334814, 0.3333333333333333703, 0.3333333333333333703, 0.3333333333333334259, 0.3333333333333333703, 0.3333333333333333703, 0.3333333333333333703, 0.3333333333333333703, 0.3333333333333334814, 0.3333333333333333148, 0.3333333333333334259, 0.3333333333333333148, 0.3333333333333333703, 0.3333333333333333703, 0.3333333333333333703, 0.3333333333333335369, 0.3333333333333333703, 0.3333333333333333148, 0.3333333333333334814, 0.3333333333333334259, 0.3333333333333333148, 0.3333333333333333148, 0.3333333333333335369, 0.3333333333333332593, 0.3333333333333333703, 0.3333333333333333148, 0.3333333333333333703, 0.3333333333333333703, 0.3333333333333332593, 0.3333333333333334259, 0.3333333333333332593, 0.3333333333333335369, 0.3333333333333333148, 0.3333333333333333703, 0.3333333333333334259, 0.3333333333333333703, 0.3333333333333333703, 0.3333333333333334814, 0.3333333333333333148, 0.3333333333333333148, 0.3333333333333334259, 0.3333333333333333148, 0.3333333333333333703, 0.3333333333333334814, 0.3333333333333333703, 0.3333333333333333703, 0.3333333333333333703, 0.3333333333333333703, 0.3333333333333334814, 0.3333333333333333703, 0.3333333333333334814, 0.3333333333333333703, 0.3333333333333333703, 0.3333333333333333148, 0.3333333333333334259, 0.3333333333333333148, 0.3333333333333334259, 0.3333333333333333148, 0.3333333333333333703, 0.3333333333333334814, 0.3333333333333333148, 0.3333333333333333148, 0.3333333333333333703, 0.3333333333333333703, 0.3333333333333333703, 0.3333333333333334259, 0.3333333333333333148, 0.3333333333333333703, 0.3333333333333334259, 0.3333333333333333148, 0.3333333333333333703, 0.3333333333333332593, 0.3333333333333333703, 0.3333333333333334259, 0.3333333333333333703, 0.3333333333333333703, 0.3333333333333333703, 0.3333333333333333703, 0.3333333333333334814, 0.3333333333333333703, 0.3333333333333334259, 0.3333333333333334259),
 ( 1.000000000000000000, 1.000000000000000000, 1.000000000000000222, 1.000000000000000000, 0.9999999999999996669, 1.000000000000000444, 0.9999999999999997780, 1.000000000000000000, 1.000000000000000222, 0.9999999999999996669, 1.000000000000000222, 0.9999999999999996669, 1.000000000000000000, 0.9999999999999997780, 1.000000000000000222, 0.9999999999999997780, 1.000000000000000222, 1.000000000000000222, 0.9999999999999997780, 1.000000000000000222, 1.000000000000000222, 0.9999999999999996669, 1.000000000000000444, 0.9999999999999997780, 1.000000000000000000, 1.000000000000000222, 1.000000000000000000, 1.000000000000000000, 1.000000000000000000, 1.000000000000000000, 1.000000000000000222, 1.000000000000000000, 1.000000000000000000, 0.9999999999999997780, 1.000000000000000000, 1.000000000000000000, 1.000000000000000000, 1.000000000000000000, 0.9999999999999997780, 1.000000000000000222, 1.000000000000000000, 1.000000000000000000, 1.000000000000000444, 0.9999999999999997780, 1.000000000000000222, 0.9999999999999996669, 1.000000000000000444, 0.9999999999999997780, 1.000000000000000000, 0.9999999999999997780, 1.000000000000000000, 1.000000000000000222, 0.9999999999999997780, 1.000000000000000444, 0.9999999999999997780, 1.000000000000000000, 0.9999999999999996669, 1.000000000000000444, 0.9999999999999997780, 1.000000000000000444, 1.000000000000000000, 1.000000000000000444, 0.9999999999999996669, 1.000000000000000000, 0.9999999999999996669, 1.000000000000000444, 0.9999999999999997780, 1.000000000000000000, 1.000000000000000000, 1.000000000000000000, 1.000000000000000000, 0.9999999999999996669, 1.000000000000000000, 1.000000000000000222, 0.9999999999999997780, 1.000000000000000000, 0.9999999999999997780, 0.9999999999999997780, 1.000000000000000000, 1.000000000000000222, 0.9999999999999997780, 1.000000000000000000, 1.000000000000000222, 1.000000000000000222, 1.000000000000000222, 0.9999999999999997780, 1.000000000000000000, 1.000000000000000222, 0.9999999999999997780, 1.000000000000000222, 1.000000000000000222, 0.9999999999999997780, 0.9999999999999997780, 0.9999999999999997780, 1.000000000000000444, 1.000000000000000000, 1.000000000000000000, 1.000000000000000000, 1.000000000000000222, 0.9999999999999997780, 1.000000000000000000, 1.000000000000000444, 0.9999999999999996669, 1.000000000000000444, 1.000000000000000000, 1.000000000000000000, 1.000000000000000222, 0.9999999999999997780, 1.000000000000000444, 0.9999999999999996669, 1.000000000000000444, 1.000000000000000000, 0.9999999999999997780, 1.000000000000000222, 0.9999999999999996669, 1.000000000000000222, 1.000000000000000000, 1.000000000000000222, 0.9999999999999997780, 1.000000000000000222, 0.9999999999999996669, 1.000000000000000222, 1.000000000000000222, 1.000000000000000222, 1.000000000000000000, 0.9999999999999997780, 1.000000000000000000, 0.9999999999999997780, 1.000000000000000000, 0.9999999999999997780, 0.9999999999999997780, 1.000000000000000222, 1.000000000000000222, 1.000000000000000222, 0.9999999999999997780, 0.9999999999999997780, 1.000000000000000444, 0.9999999999999997780, 1.000000000000000000, 0.9999999999999997780, 1.000000000000000000, 0.9999999999999997780, 1.000000000000000222, 1.000000000000000000, 1.000000000000000000, 1.000000000000000222, 1.000000000000000000, 0.9999999999999997780, 1.000000000000000444, 1.000000000000000000, 1.000000000000000000, 1.000000000000000444, 0.9999999999999997780, 1.000000000000000222, 0.9999999999999997780, 1.000000000000000444, 1.000000000000000000, 1.000000000000000222, 0.9999999999999997780, 0.9999999999999997780, 1.000000000000000000, 1.000000000000000444, 0.9999999999999996669, 1.000000000000000000, 1.000000000000000222, 1.000000000000000222, 0.9999999999999997780, 1.000000000000000222, 0.9999999999999997780, 1.000000000000000222, 1.000000000000000000, 1.000000000000000000, 0.9999999999999997780, 1.000000000000000444, 0.9999999999999997780, 1.000000000000000222, 0.9999999999999996669, 1.000000000000000444, 0.9999999999999996669, 1.000000000000000222, 1.000000000000000000, 1.000000000000000000, 1.000000000000000000, 1.000000000000000444, 1.000000000000000222, 0.9999999999999997780, 1.000000000000000444, 0.9999999999999997780, 1.000000000000000000, 0.9999999999999996669, 1.000000000000000000, 0.9999999999999996669, 1.000000000000000000, 1.000000000000000222, 1.000000000000000000, 0.9999999999999997780, 1.000000000000000222, 1.000000000000000000, 1.000000000000000222, 0.9999999999999996669, 1.000000000000000000, 1.000000000000000000, 1.000000000000000000, 0.9999999999999997780, 1.000000000000000000, 1.000000000000000000, 1.000000000000000222, 1.000000000000000000, 1.000000000000000000, 0.9999999999999997780, 1.000000000000000000, 1.000000000000000222, 0.9999999999999997780, 1.000000000000000000, 1.000000000000000222, 1.000000000000000000, 1.000000000000000000, 0.9999999999999997780, 0.9999999999999997780, 1.000000000000000000, 1.000000000000000000, 0.9999999999999997780, 1.000000000000000000, 1.000000000000000000, 1.000000000000000000, 1.000000000000000222, 1.000000000000000000, 1.000000000000000000, 0.9999999999999997780, 1.000000000000000000, 0.9999999999999997780, 1.000000000000000444, 0.9999999999999997780, 1.000000000000000222, 0.9999999999999997780, 1.000000000000000444, 0.9999999999999994449, 1.000000000000000444, 0.9999999999999997780, 1.000000000000000222, 1.000000000000000000, 1.000000000000000000, 0.9999999999999997780, 1.000000000000000000, 1.000000000000000000, 0.9999999999999997780, 1.000000000000000000, 1.000000000000000000, 0.9999999999999997780, 1.000000000000000222, 1.000000000000000000, 1.000000000000000222, 0.9999999999999997780, 1.000000000000000222, 0.9999999999999997780, 1.000000000000000222, 0.9999999999999997780, 1.000000000000000444, 0.9999999999999996669, 1.000000000000000222, 0.9999999999999997780, 1.000000000000000000, 1.000000000000000000, 1.000000000000000000, 1.000000000000000222, 1.000000000000000222, 1.000000000000000000, 1.000000000000000444, 1.000000000000000222, 0.9999999999999997780, 1.000000000000000222, 0.9999999999999996669, 1.000000000000000444, 0.9999999999999997780, 0.9999999999999997780, 1.000000000000000222, 1.000000000000000000, 1.000000000000000222, 1.000000000000000000, 1.000000000000000000, 1.000000000000000222, 1.000000000000000000, 0.9999999999999997780, 1.000000000000000222, 0.9999999999999997780, 1.000000000000000000, 1.000000000000000222, 1.000000000000000000, 0.9999999999999997780, 0.9999999999999997780, 1.000000000000000000, 0.9999999999999997780, 1.000000000000000000, 1.000000000000000000, 1.000000000000000000, 1.000000000000000222, 0.9999999999999997780, 1.000000000000000000, 1.000000000000000222, 1.000000000000000000, 0.9999999999999997780, 1.000000000000000000, 1.000000000000000000, 1.000000000000000222, 0.9999999999999997780, 1.000000000000000222, 1.000000000000000000, 1.000000000000000000, 1.000000000000000222, 1.000000000000000000, 1.000000000000000000, 1.000000000000000222, 1.000000000000000000, 1.000000000000000444, 0.9999999999999996669, 1.000000000000000444, 0.9999999999999997780, 1.000000000000000000, 1.000000000000000222, 0.9999999999999996669, 1.000000000000000444, 1.000000000000000000, 1.000000000000000000, 1.000000000000000222, 1.000000000000000444, 1.000000000000000000, 0.9999999999999996669, 1.000000000000000444, 0.9999999999999997780, 0.9999999999999997780, 0.9999999999999997780, 1.000000000000000222, 1.000000000000000000, 0.9999999999999996669, 1.000000000000000222, 1.000000000000000000, 1.000000000000000444, 0.9999999999999997780, 1.000000000000000000, 1.000000000000000222, 1.000000000000000222, 1.000000000000000222, 1.000000000000000222, 1.000000000000000000, 1.000000000000000000, 1.000000000000000000, 1.000000000000000000, 1.000000000000000000, 1.000000000000000444, 1.000000000000000000, 0.9999999999999997780, 1.000000000000000000, 1.000000000000000222, 1.000000000000000000, 1.000000000000000222, 1.000000000000000222, 1.000000000000000000, 0.9999999999999997780, 0.9999999999999997780, 1.000000000000000222, 0.9999999999999997780, 1.000000000000000000, 1.000000000000000222, 1.000000000000000000, 1.000000000000000222, 1.000000000000000000, 0.9999999999999997780, 1.000000000000000000, 0.9999999999999997780, 1.000000000000000222, 1.000000000000000000, 0.9999999999999997780, 0.9999999999999997780, 1.000000000000000222, 1.000000000000000000, 1.000000000000000222, 0.9999999999999996669, 1.000000000000000000, 1.000000000000000222, 0.9999999999999997780, 1.000000000000000000, 1.000000000000000000, 1.000000000000000222, 1.000000000000000222, 1.000000000000000000, 1.000000000000000222, 1.000000000000000222),
 ( 0.3333333333333333703, 0.3333333333333333703, 0.3333333333333333703, 0.3333333333333333703, 0.3333333333333333148, 0.3333333333333334259, 0.3333333333333333703, 0.3333333333333333148, 0.3333333333333334259, 0.3333333333333333148, 0.3333333333333334259, 0.3333333333333332038, 0.3333333333333333703, 0.3333333333333332593, 0.3333333333333333703, 0.3333333333333332593, 0.3333333333333334814, 0.3333333333333334259, 0.3333333333333333703, 0.3333333333333334259, 0.3333333333333334259, 0.3333333333333332038, 0.3333333333333335369, 0.3333333333333333148, 0.3333333333333333148, 0.3333333333333334259, 0.3333333333333333703, 0.3333333333333333148, 0.3333333333333334259, 0.3333333333333333148, 0.3333333333333335369, 0.3333333333333333148, 0.3333333333333334259, 0.3333333333333333148, 0.3333333333333334259, 0.3333333333333333703, 0.3333333333333333148, 0.3333333333333333703, 0.3333333333333334259, 0.3333333333333333703, 0.3333333333333334259, 0.3333333333333333703, 0.3333333333333334814, 0.3333333333333333148, 0.3333333333333334259, 0.3333333333333332593, 0.3333333333333335369, 0.3333333333333332593, 0.3333333333333334259, 0.3333333333333333148, 0.3333333333333333703, 0.3333333333333334259, 0.3333333333333333148, 0.3333333333333334814, 0.3333333333333332593, 0.3333333333333333703, 0.3333333333333332593, 0.3333333333333335369, 0.3333333333333333148, 0.3333333333333334259, 0.3333333333333334259, 0.3333333333333334259, 0.3333333333333333148, 0.3333333333333333148, 0.3333333333333333703, 0.3333333333333333703, 0.3333333333333333703, 0.3333333333333334259, 0.3333333333333333148, 0.3333333333333333703, 0.3333333333333333703, 0.3333333333333332593, 0.3333333333333334259, 0.3333333333333333703, 0.3333333333333333703, 0.3333333333333333148, 0.3333333333333333148, 0.3333333333333334259, 0.3333333333333333148, 0.3333333333333334259, 0.3333333333333333148, 0.3333333333333334259, 0.3333333333333333703, 0.3333333333333334259, 0.3333333333333333703, 0.3333333333333333703, 0.3333333333333333148, 0.3333333333333335369, 0.3333333333333332593, 0.3333333333333334814, 0.3333333333333333703, 0.3333333333333333703, 0.3333333333333333148, 0.3333333333333333703, 0.3333333333333334259, 0.3333333333333334259, 0.3333333333333333148, 0.3333333333333333703, 0.3333333333333334259, 0.3333333333333333148, 0.3333333333333333703, 0.3333333333333334814, 0.3333333333333332038, 0.3333333333333334814, 0.3333333333333333703, 0.3333333333333333148, 0.3333333333333334259, 0.3333333333333333148, 0.3333333333333334259, 0.3333333333333332593, 0.3333333333333333703, 0.3333333333333334259, 0.3333333333333333148, 0.3333333333333333703, 0.3333333333333333148, 0.3333333333333334259, 0.3333333333333333703, 0.3333333333333333703, 0.3333333333333333703, 0.3333333333333334259, 0.3333333333333332038, 0.3333333333333334259, 0.3333333333333334259, 0.3333333333333333703, 0.3333333333333333703, 0.3333333333333332593, 0.3333333333333333703, 0.3333333333333333148, 0.3333333333333334259, 0.3333333333333332593, 0.3333333333333334259, 0.3333333333333333703, 0.3333333333333334259, 0.3333333333333334259, 0.3333333333333333148, 0.3333333333333334259, 0.3333333333333334259, 0.3333333333333332593, 0.3333333333333334259, 0.3333333333333333703, 0.3333333333333333703, 0.3333333333333333148, 0.3333333333333334259, 0.3333333333333333703, 0.3333333333333334259, 0.3333333333333334259, 0.3333333333333333703, 0.3333333333333333703, 0.3333333333333334814, 0.3333333333333333703, 0.3333333333333333703, 0.3333333333333335369, 0.3333333333333332593, 0.3333333333333334259, 0.3333333333333333148, 0.3333333333333334259, 0.3333333333333334259, 0.3333333333333334259, 0.3333333333333332593, 0.3333333333333333148, 0.3333333333333333703, 0.3333333333333334259, 0.3333333333333333148, 0.3333333333333333703, 0.3333333333333333148, 0.3333333333333334259, 0.3333333333333333148, 0.3333333333333334259, 0.3333333333333333148, 0.3333333333333334259, 0.3333333333333333703, 0.3333333333333334259, 0.3333333333333333703, 0.3333333333333334259, 0.3333333333333333148, 0.3333333333333333703, 0.3333333333333333703, 0.3333333333333334259, 0.3333333333333333703, 0.3333333333333334259, 0.3333333333333333703, 0.3333333333333333703, 0.3333333333333334259, 0.3333333333333334814, 0.3333333333333333703, 0.3333333333333333703, 0.3333333333333334814, 0.3333333333333333148, 0.3333333333333333703, 0.3333333333333333148, 0.3333333333333333703, 0.3333333333333333148, 0.3333333333333334259, 0.3333333333333334259, 0.3333333333333333703, 0.3333333333333333703, 0.3333333333333333703, 0.3333333333333333703, 0.3333333333333334259, 0.3333333333333332593, 0.3333333333333333703, 0.3333333333333333703, 0.3333333333333333703, 0.3333333333333333148, 0.3333333333333333703, 0.3333333333333333148, 0.3333333333333334259, 0.3333333333333333148, 0.3333333333333333703, 0.3333333333333333703, 0.3333333333333334259, 0.3333333333333333703, 0.3333333333333333148, 0.3333333333333333703, 0.3333333333333333703, 0.3333333333333333148, 0.3333333333333333703, 0.3333333333333333148, 0.3333333333333333703, 0.3333333333333333703, 0.3333333333333334814, 0.3333333333333333148, 0.3333333333333334259, 0.3333333333333334259, 0.3333333333333333703, 0.3333333333333334259, 0.3333333333333333703, 0.3333333333333334259, 0.3333333333333332593, 0.3333333333333334259, 0.3333333333333333148, 0.3333333333333334259, 0.3333333333333333148, 0.3333333333333334259, 0.3333333333333332593, 0.3333333333333335369, 0.3333333333333332038, 0.3333333333333334259, 0.3333333333333333703, 0.3333333333333333148, 0.3333333333333334259, 0.3333333333333333148, 0.3333333333333333148, 0.3333333333333333148, 0.3333333333333334814, 0.3333333333333332593, 0.3333333333333334259, 0.3333333333333333148, 0.3333333333333333148, 0.3333333333333334814, 0.3333333333333333703, 0.3333333333333334259, 0.3333333333333333148, 0.3333333333333333703, 0.3333333333333332593, 0.3333333333333334814, 0.3333333333333333148, 0.3333333333333334259, 0.3333333333333333148, 0.3333333333333334259, 0.3333333333333333703, 0.3333333333333333703, 0.3333333333333334259, 0.3333333333333333148, 0.3333333333333334814, 0.3333333333333333703, 0.3333333333333333703, 0.3333333333333334814, 0.3333333333333333703, 0.3333333333333332593, 0.3333333333333334259, 0.3333333333333332593, 0.3333333333333334814, 0.3333333333333333148, 0.3333333333333333703, 0.3333333333333333703, 0.3333333333333334259, 0.3333333333333333703, 0.3333333333333333703, 0.3333333333333333148, 0.3333333333333334259, 0.3333333333333334259, 0.3333333333333333703, 0.3333333333333334259, 0.3333333333333333148, 0.3333333333333333703, 0.3333333333333334259, 0.3333333333333333703, 0.3333333333333333148, 0.3333333333333334259, 0.3333333333333333703, 0.3333333333333333148, 0.3333333333333333148, 0.3333333333333334259, 0.3333333333333333148, 0.3333333333333333703, 0.3333333333333333703, 0.3333333333333333703, 0.3333333333333334259, 0.3333333333333334259, 0.3333333333333333148, 0.3333333333333334259, 0.3333333333333333148, 0.3333333333333334814, 0.3333333333333332593, 0.3333333333333334814, 0.3333333333333333703, 0.3333333333333333703, 0.3333333333333334259, 0.3333333333333333703, 0.3333333333333333703, 0.3333333333333333703, 0.3333333333333333703, 0.3333333333333334814, 0.3333333333333333148, 0.3333333333333334259, 0.3333333333333333148, 0.3333333333333333703, 0.3333333333333333703, 0.3333333333333333703, 0.3333333333333335369, 0.3333333333333333703, 0.3333333333333333148, 0.3333333333333334814, 0.3333333333333334259, 0.3333333333333333148, 0.3333333333333333148, 0.3333333333333335369, 0.3333333333333332593, 0.3333333333333333703, 0.3333333333333333148, 0.3333333333333333703, 0.3333333333333333703, 0.3333333333333332593, 0.3333333333333334259, 0.3333333333333332593, 0.3333333333333335369, 0.3333333333333333148, 0.3333333333333333703, 0.3333333333333334259, 0.3333333333333333703, 0.3333333333333333703, 0.3333333333333334814, 0.3333333333333333148, 0.3333333333333333148, 0.3333333333333334259, 0.3333333333333333148, 0.3333333333333333703, 0.3333333333333334814, 0.3333333333333333703, 0.3333333333333333703, 0.3333333333333333703, 0.3333333333333333703, 0.3333333333333334814, 0.3333333333333333703, 0.3333333333333334814, 0.3333333333333333703, 0.3333333333333333703, 0.3333333333333333148, 0.3333333333333334259, 0.3333333333333333148, 0.3333333333333334259, 0.3333333333333333148, 0.3333333333333333703, 0.3333333333333334814, 0.3333333333333333148, 0.3333333333333333148, 0.3333333333333333703, 0.3333333333333333703, 0.3333333333333333703, 0.3333333333333334259, 0.3333333333333333148, 0.3333333333333333703, 0.3333333333333334259, 0.3333333333333333148, 0.3333333333333333703, 0.3333333333333332593, 0.3333333333333333703, 0.3333333333333334259, 0.3333333333333333703, 0.3333333333333333703, 0.3333333333333333703, 0.3333333333333333703, 0.3333333333333334814, 0.3333333333333333703, 0.3333333333333334259, 0.3333333333333334259),
 ( 0.3333333333333333703, 0.3333333333333333703, 0.3333333333333333703, 0.3333333333333333703, 0.3333333333333333148, 0.3333333333333334259, 0.3333333333333333703, 0.3333333333333333148, 0.3333333333333334259, 0.3333333333333333148, 0.3333333333333334259, 0.3333333333333332038, 0.3333333333333333703, 0.3333333333333332593, 0.3333333333333333703, 0.3333333333333332593, 0.3333333333333334814, 0.3333333333333334259, 0.3333333333333333703, 0.3333333333333334259, 0.3333333333333334259, 0.3333333333333332038, 0.3333333333333335369, 0.3333333333333333148, 0.3333333333333333148, 0.3333333333333334259, 0.3333333333333333703, 0.3333333333333333148, 0.3333333333333334259, 0.3333333333333333148, 0.3333333333333335369, 0.3333333333333333148, 0.3333333333333334259, 0.3333333333333333148, 0.3333333333333334259, 0.3333333333333333703, 0.3333333333333333148, 0.3333333333333333703, 0.3333333333333334259, 0.3333333333333333703, 0.3333333333333334259, 0.3333333333333333703, 0.3333333333333334814, 0.3333333333333333148, 0.3333333333333334259, 0.3333333333333332593, 0.3333333333333335369, 0.3333333333333332593, 0.3333333333333334259, 0.3333333333333333148, 0.3333333333333333703, 0.3333333333333334259, 0.3333333333333333148, 0.3333333333333334814, 0.3333333333333332593, 0.3333333333333333703, 0.3333333333333332593, 0.3333333333333335369, 0.3333333333333333148, 0.3333333333333334259, 0.3333333333333334259, 0.3333333333333334259, 0.3333333333333333148, 0.3333333333333333148, 0.3333333333333333703, 0.3333333333333333703, 0.3333333333333333703, 0.3333333333333334259, 0.3333333333333333148, 0.3333333333333333703, 0.3333333333333333703, 0.3333333333333332593, 0.3333333333333334259, 0.3333333333333333703, 0.3333333333333333703, 0.3333333333333333148, 0.3333333333333333148, 0.3333333333333334259, 0.3333333333333333148, 0.3333333333333334259, 0.3333333333333333148, 0.3333333333333334259, 0.3333333333333333703, 0.3333333333333334259, 0.3333333333333333703, 0.3333333333333333703, 0.3333333333333333148, 0.3333333333333335369, 0.3333333333333332593, 0.3333333333333334814, 0.3333333333333333703, 0.3333333333333333703, 0.3333333333333333148, 0.3333333333333333703, 0.3333333333333334259, 0.3333333333333334259, 0.3333333333333333148, 0.3333333333333333703, 0.3333333333333334259, 0.3333333333333333148, 0.3333333333333333703, 0.3333333333333334814, 0.3333333333333332038, 0.3333333333333334814, 0.3333333333333333703, 0.3333333333333333148, 0.3333333333333334259, 0.3333333333333333148, 0.3333333333333334259, 0.3333333333333332593, 0.3333333333333333703, 0.3333333333333334259, 0.3333333333333333148, 0.3333333333333333703, 0.3333333333333333148, 0.3333333333333334259, 0.3333333333333333703, 0.3333333333333333703, 0.3333333333333333703, 0.3333333333333334259, 0.3333333333333332038, 0.3333333333333334259, 0.3333333333333334259, 0.3333333333333333703, 0.3333333333333333703, 0.3333333333333332593, 0.3333333333333333703, 0.3333333333333333148, 0.3333333333333334259, 0.3333333333333332593, 0.3333333333333334259, 0.3333333333333333703, 0.3333333333333334259, 0.3333333333333334259, 0.3333333333333333148, 0.3333333333333334259, 0.3333333333333334259, 0.3333333333333332593, 0.3333333333333334259, 0.3333333333333333703, 0.3333333333333333703, 0.3333333333333333148, 0.3333333333333334259, 0.3333333333333333703, 0.3333333333333334259, 0.3333333333333334259, 0.3333333333333333703, 0.3333333333333333703, 0.3333333333333334814, 0.3333333333333333703, 0.3333333333333333703, 0.3333333333333335369, 0.3333333333333332593, 0.3333333333333334259, 0.3333333333333333148, 0.3333333333333334259, 0.3333333333333334259, 0.3333333333333334259, 0.3333333333333332593, 0.3333333333333333148, 0.3333333333333333703, 0.3333333333333334259, 0.3333333333333333148, 0.3333333333333333703, 0.3333333333333333148, 0.3333333333333334259, 0.3333333333333333148, 0.3333333333333334259, 0.3333333333333333148, 0.3333333333333334259, 0.3333333333333333703, 0.3333333333333334259, 0.3333333333333333703, 0.3333333333333334259, 0.3333333333333333148, 0.3333333333333333703, 0.3333333333333333703, 0.3333333333333334259, 0.3333333333333333703, 0.3333333333333334259, 0.3333333333333333703, 0.3333333333333333703, 0.3333333333333334259, 0.3333333333333334814, 0.3333333333333333703, 0.3333333333333333703, 0.3333333333333334814, 0.3333333333333333148, 0.3333333333333333703, 0.3333333333333333148, 0.3333333333333333703, 0.3333333333333333148, 0.3333333333333334259, 0.3333333333333334259, 0.3333333333333333703, 0.3333333333333333703, 0.3333333333333333703, 0.3333333333333333703, 0.3333333333333334259, 0.3333333333333332593, 0.3333333333333333703, 0.3333333333333333703, 0.3333333333333333703, 0.3333333333333333148, 0.3333333333333333703, 0.3333333333333333148, 0.3333333333333334259, 0.3333333333333333148, 0.3333333333333333703, 0.3333333333333333703, 0.3333333333333334259, 0.3333333333333333703, 0.3333333333333333148, 0.3333333333333333703, 0.3333333333333333703, 0.3333333333333333148, 0.3333333333333333703, 0.3333333333333333148, 0.3333333333333333703, 0.3333333333333333703, 0.3333333333333334814, 0.3333333333333333148, 0.3333333333333334259, 0.3333333333333334259, 0.3333333333333333703, 0.3333333333333334259, 0.3333333333333333703, 0.3333333333333334259, 0.3333333333333332593, 0.3333333333333334259, 0.3333333333333333148, 0.3333333333333334259, 0.3333333333333333148, 0.3333333333333334259, 0.3333333333333332593, 0.3333333333333335369, 0.3333333333333332038, 0.3333333333333334259, 0.3333333333333333703, 0.3333333333333333148, 0.3333333333333334259, 0.3333333333333333148, 0.3333333333333333148, 0.3333333333333333148, 0.3333333333333334814, 0.3333333333333332593, 0.3333333333333334259, 0.3333333333333333148, 0.3333333333333333148, 0.3333333333333334814, 0.3333333333333333703, 0.3333333333333334259, 0.3333333333333333148, 0.3333333333333333703, 0.3333333333333332593, 0.3333333333333334814, 0.3333333333333333148, 0.3333333333333334259, 0.3333333333333333148, 0.3333333333333334259, 0.3333333333333333703, 0.3333333333333333703, 0.3333333333333334259, 0.3333333333333333148, 0.3333333333333334814, 0.3333333333333333703, 0.3333333333333333703, 0.3333333333333334814, 0.3333333333333333703, 0.3333333333333332593, 0.3333333333333334259, 0.3333333333333332593, 0.3333333333333334814, 0.3333333333333333148, 0.3333333333333333703, 0.3333333333333333703, 0.3333333333333334259, 0.3333333333333333703, 0.3333333333333333703, 0.3333333333333333148, 0.3333333333333334259, 0.3333333333333334259, 0.3333333333333333703, 0.3333333333333334259, 0.3333333333333333148, 0.3333333333333333703, 0.3333333333333334259, 0.3333333333333333703, 0.3333333333333333148, 0.3333333333333334259, 0.3333333333333333703, 0.3333333333333333148, 0.3333333333333333148, 0.3333333333333334259, 0.3333333333333333148, 0.3333333333333333703, 0.3333333333333333703, 0.3333333333333333703, 0.3333333333333334259, 0.3333333333333334259, 0.3333333333333333148, 0.3333333333333334259, 0.3333333333333333148, 0.3333333333333334814, 0.3333333333333332593, 0.3333333333333334814, 0.3333333333333333703, 0.3333333333333333703, 0.3333333333333334259, 0.3333333333333333703, 0.3333333333333333703, 0.3333333333333333703, 0.3333333333333333703, 0.3333333333333334814, 0.3333333333333333148, 0.3333333333333334259, 0.3333333333333333148, 0.3333333333333333703, 0.3333333333333333703, 0.3333333333333333703, 0.3333333333333335369, 0.3333333333333333703, 0.3333333333333333148, 0.3333333333333334814, 0.3333333333333334259, 0.3333333333333333148, 0.3333333333333333148, 0.3333333333333335369, 0.3333333333333332593, 0.3333333333333333703, 0.3333333333333333148, 0.3333333333333333703, 0.3333333333333333703, 0.3333333333333332593, 0.3333333333333334259, 0.3333333333333332593, 0.3333333333333335369, 0.3333333333333333148, 0.3333333333333333703, 0.3333333333333334259, 0.3333333333333333703, 0.3333333333333333703, 0.3333333333333334814, 0.3333333333333333148, 0.3333333333333333148, 0.3333333333333334259, 0.3333333333333333148, 0.3333333333333333703, 0.3333333333333334814, 0.3333333333333333703, 0.3333333333333333703, 0.3333333333333333703, 0.3333333333333333703, 0.3333333333333334814, 0.3333333333333333703, 0.3333333333333334814, 0.3333333333333333703, 0.3333333333333333703, 0.3333333333333333148, 0.3333333333333334259, 0.3333333333333333148, 0.3333333333333334259, 0.3333333333333333148, 0.3333333333333333703, 0.3333333333333334814, 0.3333333333333333148, 0.3333333333333333148, 0.3333333333333333703, 0.3333333333333333703, 0.3333333333333333703, 0.3333333333333334259, 0.3333333333333333148, 0.3333333333333333703, 0.3333333333333334259, 0.3333333333333333148, 0.3333333333333333703, 0.3333333333333332593, 0.3333333333333333703, 0.3333333333333334259, 0.3333333333333333703, 0.3333333333333333703, 0.3333333333333333703, 0.3333333333333333703, 0.3333333333333334814, 0.3333333333333333703, 0.3333333333333334259, 0.3333333333333334259),
 ( 1.000000000000000000, 1.000000000000000000, 1.000000000000000222, 1.000000000000000000, 0.9999999999999996669, 1.000000000000000444, 0.9999999999999997780, 1.000000000000000000, 1.000000000000000222, 0.9999999999999996669, 1.000000000000000222, 0.9999999999999996669, 1.000000000000000000, 0.9999999999999997780, 1.000000000000000222, 0.9999999999999997780, 1.000000000000000222, 1.000000000000000222, 0.9999999999999997780, 1.000000000000000222, 1.000000000000000222, 0.9999999999999996669, 1.000000000000000444, 0.9999999999999997780, 1.000000000000000000, 1.000000000000000222, 1.000000000000000000, 1.000000000000000000, 1.000000000000000000, 1.000000000000000000, 1.000000000000000222, 1.000000000000000000, 1.000000000000000000, 0.9999999999999997780, 1.000000000000000000, 1.000000000000000000, 1.000000000000000000, 1.000000000000000000, 0.9999999999999997780, 1.000000000000000222, 1.000000000000000000, 1.000000000000000000, 1.000000000000000444, 0.9999999999999997780, 1.000000000000000222, 0.9999999999999996669, 1.000000000000000444, 0.9999999999999997780, 1.000000000000000000, 0.9999999999999997780, 1.000000000000000000, 1.000000000000000222, 0.9999999999999997780, 1.000000000000000444, 0.9999999999999997780, 1.000000000000000000, 0.9999999999999996669, 1.000000000000000444, 0.9999999999999997780, 1.000000000000000444, 1.000000000000000000, 1.000000000000000444, 0.9999999999999996669, 1.000000000000000000, 0.9999999999999996669, 1.000000000000000444, 0.9999999999999997780, 1.000000000000000000, 1.000000000000000000, 1.000000000000000000, 1.000000000000000000, 0.9999999999999996669, 1.000000000000000000, 1.000000000000000222, 0.9999999999999997780, 1.000000000000000000, 0.9999999999999997780, 0.9999999999999997780, 1.000000000000000000, 1.000000000000000222, 0.9999999999999997780, 1.000000000000000000, 1.000000000000000222, 1.000000000000000222, 1.000000000000000222, 0.9999999999999997780, 1.000000000000000000, 1.000000000000000222, 0.9999999999999997780, 1.000000000000000222, 1.000000000000000222, 0.9999999999999997780, 0.9999999999999997780, 0.9999999999999997780, 1.000000000000000444, 1.000000000000000000, 1.000000000000000000, 1.000000000000000000, 1.000000000000000222, 0.9999999999999997780, 1.000000000000000000, 1.000000000000000444, 0.9999999999999996669, 1.000000000000000444, 1.000000000000000000, 1.000000000000000000, 1.000000000000000222, 0.9999999999999997780, 1.000000000000000444, 0.9999999999999996669, 1.000000000000000444, 1.000000000000000000, 0.9999999999999997780, 1.000000000000000222, 0.9999999999999996669, 1.000000000000000222, 1.000000000000000000, 1.000000000000000222, 0.9999999999999997780, 1.000000000000000222, 0.9999999999999996669, 1.000000000000000222, 1.000000000000000222, 1.000000000000000222, 1.000000000000000000, 0.9999999999999997780, 1.000000000000000000, 0.9999999999999997780, 1.000000000000000000, 0.9999999999999997780, 0.9999999999999997780, 1.000000000000000222, 1.000000000000000222, 1.000000000000000222, 0.9999999999999997780, 0.9999999999999997780, 1.000000000000000444, 0.9999999999999997780, 1.000000000000000000, 0.9999999999999997780, 1.000000000000000000, 0.9999999999999997780, 1.000000000000000222, 1.000000000000000000, 1.000000000000000000, 1.000000000000000222, 1.000000000000000000, 0.9999999999999997780, 1.000000000000000444, 1.000000000000000000, 1.000000000000000000, 1.000000000000000444, 0.9999999999999997780, 1.000000000000000222, 0.9999999999999997780, 1.000000000000000444, 1.000000000000000000, 1.000000000000000222, 0.9999999999999997780, 0.9999999999999997780, 1.000000000000000000, 1.000000000000000444, 0.9999999999999996669, 1.000000000000000000, 1.000000000000000222, 1.000000000000000222, 0.9999999999999997780, 1.000000000000000222, 0.9999999999999997780, 1.000000000000000222, 1.000000000000000000, 1.000000000000000000, 0.9999999999999997780, 1.000000000000000444, 0.9999999999999997780, 1.000000000000000222, 0.9999999999999996669, 1.000000000000000444, 0.9999999999999996669, 1.000000000000000222, 1.000000000000000000, 1.000000000000000000, 1.000000000000000000, 1.000000000000000444, 1.000000000000000222, 0.9999999999999997780, 1.000000000000000444, 0.9999999999999997780, 1.000000000000000000, 0.9999999999999996669, 1.000000000000000000, 0.9999999999999996669, 1.000000000000000000, 1.000000000000000222, 1.000000000000000000, 0.9999999999999997780, 1.000000000000000222, 1.000000000000000000, 1.000000000000000222, 0.9999999999999996669, 1.000000000000000000, 1.000000000000000000, 1.000000000000000000, 0.9999999999999997780, 1.000000000000000000, 1.000000000000000000, 1.000000000000000222, 1.000000000000000000, 1.000000000000000000, 0.9999999999999997780, 1.000000000000000000, 1.000000000000000222, 0.9999999999999997780, 1.000000000000000000, 1.000000000000000222, 1.000000000000000000, 1.000000000000000000, 0.9999999999999997780, 0.9999999999999997780, 1.000000000000000000, 1.000000000000000000, 0.9999999999999997780, 1.000000000000000000, 1.000000000000000000, 1.000000000000000000, 1.000000000000000222, 1.000000000000000000, 1.000000000000000000, 0.9999999999999997780, 1.000000000000000000, 0.9999999999999997780, 1.000000000000000444, 0.9999999999999997780, 1.000000000000000222, 0.9999999999999997780, 1.000000000000000444, 0.9999999999999994449, 1.000000000000000444, 0.9999999999999997780, 1.000000000000000222, 1.000000000000000000, 1.000000000000000000, 0.9999999999999997780, 1.000000000000000000, 1.000000000000000000, 0.9999999999999997780, 1.000000000000000000, 1.000000000000000000, 0.9999999999999997780, 1.000000000000000222, 1.000000000000000000, 1.000000000000000222, 0.9999999999999997780, 1.000000000000000222, 0.9999999999999997780, 1.000000000000000222, 0.9999999999999997780, 1.000000000000000444, 0.9999999999999996669, 1.000000000000000222, 0.9999999999999997780, 1.000000000000000000, 1.000000000000000000, 1.000000000000000000, 1.000000000000000222, 1.000000000000000222, 1.000000000000000000, 1.000000000000000444, 1.000000000000000222, 0.9999999999999997780, 1.000000000000000222, 0.9999999999999996669, 1.000000000000000444, 0.9999999999999997780, 0.9999999999999997780, 1.000000000000000222, 1.000000000000000000, 1.000000000000000222, 1.000000000000000000, 1.000000000000000000, 1.000000000000000222, 1.000000000000000000, 0.9999999999999997780, 1.000000000000000222, 0.9999999999999997780, 1.000000000000000000, 1.000000000000000222, 1.000000000000000000, 0.9999999999999997780, 0.9999999999999997780, 1.000000000000000000, 0.9999999999999997780, 1.000000000000000000, 1.000000000000000000, 1.000000000000000000, 1.000000000000000222, 0.9999999999999997780, 1.000000000000000000, 1.000000000000000222, 1.000000000000000000, 0.9999999999999997780, 1.000000000000000000, 1.000000000000000000, 1.000000000000000222, 0.9999999999999997780, 1.000000000000000222, 1.000000000000000000, 1.000000000000000000, 1.000000000000000222, 1.000000000000000000, 1.000000000000000000, 1.000000000000000222, 1.000000000000000000, 1.000000000000000444, 0.9999999999999996669, 1.000000000000000444, 0.9999999999999997780, 1.000000000000000000, 1.000000000000000222, 0.9999999999999996669, 1.000000000000000444, 1.000000000000000000, 1.000000000000000000, 1.000000000000000222, 1.000000000000000444, 1.000000000000000000, 0.9999999999999996669, 1.000000000000000444, 0.9999999999999997780, 0.9999999999999997780, 0.9999999999999997780, 1.000000000000000222, 1.000000000000000000, 0.9999999999999996669, 1.000000000000000222, 1.000000000000000000, 1.000000000000000444, 0.9999999999999997780, 1.000000000000000000, 1.000000000000000222, 1.000000000000000222, 1.000000000000000222, 1.000000000000000222, 1.000000000000000000, 1.000000000000000000, 1.000000000000000000, 1.000000000000000000, 1.000000000000000000, 1.000000000000000444, 1.000000000000000000, 0.9999999999999997780, 1.000000000000000000, 1.000000000000000222, 1.000000000000000000, 1.000000000000000222, 1.000000000000000222, 1.000000000000000000, 0.9999999999999997780, 0.9999999999999997780, 1.000000000000000222, 0.9999999999999997780, 1.000000000000000000, 1.000000000000000222, 1.000000000000000000, 1.000000000000000222, 1.000000000000000000, 0.9999999999999997780, 1.000000000000000000, 0.9999999999999997780, 1.000000000000000222, 1.000000000000000000, 0.9999999999999997780, 0.9999999999999997780, 1.000000000000000222, 1.000000000000000000, 1.000000000000000222, 0.9999999999999996669, 1.000000000000000000, 1.000000000000000222, 0.9999999999999997780, 1.000000000000000000, 1.000000000000000000, 1.000000000000000222, 1.000000000000000222, 1.000000000000000000, 1.000000000000000222, 1.000000000000000222) ) ) 
 REPRESENTATION_ITEM ( '' )  SURFACE ( )  );
#192802 = CARTESIAN_POINT ( 'NONE',  ( 1.234804682044550850, -1.602240143502192238, 0.7520855130052228610 ) ) ;
#192803 = CARTESIAN_POINT ( 'NONE',  ( 5.004545975878083475, -1.998138528169653316, -0.2443019910301855169 ) ) ;
#192804 = CARTESIAN_POINT ( 'NONE',  ( 6.765682348419287173, 7.852049813699357728, 1.199719254218462483 ) ) ;
#192805 = CARTESIAN_POINT ( 'NONE',  ( 3.592891271941214271, -0.4089703316215765883, -2.065685861495478726 ) ) ;
#192806 = CARTESIAN_POINT ( 'NONE',  ( 2.688967962845473458, 1.619712848077807577, 1.022445119732362961 ) ) ;
#192807 = CARTESIAN_POINT ( 'NONE',  ( 3.871016551901614200, 4.474939717762034697, -1.199719254218446718 ) ) ;
#192808 = CARTESIAN_POINT ( 'NONE',  ( 4.264079249230395163, -1.964438661470244263, 0.1424843695872201332 ) ) ;
#192810 = ADVANCED_FACE ( 'NONE', ( #111563 ), #20668, .T. ) ;
#192809 = CARTESIAN_POINT ( 'NONE',  ( 5.607677614632407881, 1.532089292189286356, 1.316289066716142431 ) ) ;
#192811 = CARTESIAN_POINT ( 'NONE',  ( 1.287742131874554552, -0.8442722623961744777, 1.669378388412197767 ) ) ;
#192814 = EDGE_LOOP ( 'NONE', ( #3957, #93935, #139327, #29388 ) ) ;
#192813 = CARTESIAN_POINT ( 'NONE',  ( 1.775505761281343631, 0.3235837346332003372, -1.884644527778083001 ) ) ;
#192812 = CARTESIAN_POINT ( 'NONE',  ( 5.461458274417386072, 0.3306134467882023142, -1.692711794494299538 ) ) ;
#192816 = CARTESIAN_POINT ( 'NONE',  ( 4.528060117284232966, 6.305822774963486310, 1.443375672974062551 ) ) ;
#192815 = CARTESIAN_POINT ( 'NONE',  ( 1.612255294781844706, -2.189918024983358080, 0.2725913246661854084 ) ) ;
#192817 = CARTESIAN_POINT ( 'NONE',  ( -0.6823417656250003738, 1.780208333674752952, -1.181850606188749264 ) ) ;
#192819 = ADVANCED_FACE ( 'NONE', ( #193799 ), #40385, .T. ) ;
#192818 = CARTESIAN_POINT ( 'NONE',  ( 6.968000882419564945, 10.21675256520979858, 1.199719254218460707 ) ) ;
#192820 = CARTESIAN_POINT ( 'NONE',  ( 6.819227946136852125, -0.1326586024288610444, 1.840611662119538749 ) ) ;
#192821 = DIRECTION ( 'NONE',  ( 0.000000000000000000, -1.000000000000000000, 0.000000000000000000 ) ) ;
#192822 = CYLINDRICAL_SURFACE ( 'NONE', #72311, 0.05000000000000002359 ) ;
#192823 = CARTESIAN_POINT ( 'NONE',  ( 7.834948825496932834, -5.907420853759296264, 7.720982897393586342 ) ) ;
#192824 = VERTEX_POINT ( 'NONE', #89139 ) ;
#192825 = CARTESIAN_POINT ( 'NONE',  ( 2.348173244826061268, -0.8873571809006628452, 1.870714752860686447 ) ) ;
#192826 = CARTESIAN_POINT ( 'NONE',  ( 0.7499999999999902300, 3.733333333333352488, 1.299038105676669330 ) ) ;
#192827 = CARTESIAN_POINT ( 'NONE',  ( 6.257251587906815793, 7.258880593101466161, 1.199719254218462483 ) ) ;
#192828 = CARTESIAN_POINT ( 'NONE',  ( -7.365103760721662951, 9.615707025640515937, 1.599625672291295375 ) ) ;
#192829 = CARTESIAN_POINT ( 'NONE',  ( 4.927462483923885195, 4.713404084191450849, -0.7998128361456481317 ) ) ;
#192830 = CARTESIAN_POINT ( 'NONE',  ( 6.533838320793388554, -2.056994387304663885, 0.5145578593022880343 ) ) ;
#192831 = PLANE ( 'NONE',  #205182 ) ;
#192832 = CARTESIAN_POINT ( 'NONE',  ( -0.6823417656250003738, 2.467708333674753618, -1.181850606188749264 ) ) ;
#192834 = CARTESIAN_POINT ( 'NONE',  ( 9.490344339885973923, 12.09515436799890331, -1.443375672974057666 ) ) ;
#192833 = CARTESIAN_POINT ( 'NONE',  ( 1.249000902703297164E-16, 4.400000000000001243, -2.250000000000000000 ) ) ;
#192835 = CARTESIAN_POINT ( 'NONE',  ( 3.972029700707707445, 1.727737986437705819, 1.038833660170018769 ) ) ;
#192836 = CARTESIAN_POINT ( 'NONE',  ( 4.522610612662866458, 0.3335214923718023416, 1.886305606834618231 ) ) ;
#192837 = LINE ( 'NONE', #78035, #172845 ) ;
#192838 = CARTESIAN_POINT ( 'NONE',  ( 2.472451708263478487, -2.098117355222902436, -0.6331711661175795092 ) ) ;
#192839 = CARTESIAN_POINT ( 'NONE',  ( 0.1335669894368343991, 7.629137130509040965, -2.753547149787978654 ) ) ;
#192840 = CARTESIAN_POINT ( 'NONE',  ( -1.402160292154681736E-14, 0.6187500006828180465, -1.732050807568863648 ) ) ;
#192841 = CARTESIAN_POINT ( 'NONE',  ( 5.431894621915298593, -1.963206642400895374, 0.4451836139030879713 ) ) ;
#192842 = CARTESIAN_POINT ( 'NONE',  ( -7.203459687562382641, 7.298457811777897319, -0.7998128361456291469 ) ) ;
#192844 = CARTESIAN_POINT ( 'NONE',  ( 0.1929827526203631294, 1.755782054984224683, 0.9913788669043410717 ) ) ;
#192843 = CARTESIAN_POINT ( 'NONE',  ( -2.982430605326328532, 5.462957558647244305, -1.082531754730543971 ) ) ;
#192845 = CARTESIAN_POINT ( 'NONE',  ( -1.364683531250014514, 9.401041667008062319, -0.7879004041258335089 ) ) ;
#192847 = CARTESIAN_POINT ( 'NONE',  ( -7.442499979258930587, 7.647614495415686164, -0.7998128361456362523 ) ) ;
#192846 = CARTESIAN_POINT ( 'NONE',  ( 3.562131390660903563, -1.402593093800925894, 1.550658987340556294 ) ) ;
#192849 = EDGE_LOOP ( 'NONE', ( #138102, #20133, #83994 ) ) ;
#192848 = CARTESIAN_POINT ( 'NONE',  ( 2.221339967433374252, -1.673790515994465711, 0.4157018595009522310 ) ) ;
#192850 = CARTESIAN_POINT ( 'NONE',  ( 6.135037582782754129, 1.979230198018981701, 0.7618025574447004900 ) ) ;
#192851 = CARTESIAN_POINT ( 'NONE',  ( 6.810273232766058449, 6.839740281182199233, 1.040834085586084257E-14 ) ) ;
#192852 = DIRECTION ( 'NONE',  ( -0.000000000000000000, 1.000000000000000000, -0.000000000000000000 ) ) ;
#192853 = CARTESIAN_POINT ( 'NONE',  ( 6.717278222822382183, 7.849261790823902629, -6.750415307812251520 ) ) ;
#192854 = CARTESIAN_POINT ( 'NONE',  ( 0.000000000000000000, 0.5000000000000000000, 0.000000000000000000 ) ) ;
#192855 = CARTESIAN_POINT ( 'NONE',  ( 5.982172092127724383, 8.002286745614243912, -1.599625672291262513 ) ) ;
#192856 = ORIENTED_EDGE ( 'NONE', *, *, #179088, .F. ) ;
#192857 = DIRECTION ( 'NONE',  ( 1.276756478318932585E-15, -1.000000000000000000, 1.665334536937738262E-16 ) ) ;
#192858 = EDGE_LOOP ( 'NONE', ( #82044, #63669 ) ) ;
#192859 = CARTESIAN_POINT ( 'NONE',  ( 2.332397652471474903, 1.182373381703984094, -1.372477691862858729 ) ) ;
#192860 = CARTESIAN_POINT ( 'NONE',  ( -6.826694039680798021, 7.923230120171105284, -1.199719254218446718 ) ) ;
#192862 = VERTEX_POINT ( 'NONE', #138956 ) ;
#192861 = AXIS2_PLACEMENT_3D ( 'NONE', #164938, #79426, #62117 ) ;
#192863 = CARTESIAN_POINT ( 'NONE',  ( 2.191614386903386613, 5.708633884695917260, -0.7998128361456281477 ) ) ;
#192864 = EDGE_LOOP ( 'NONE', ( #37981, #51956, #193891, #131350 ) ) ;
#192865 = CARTESIAN_POINT ( 'NONE',  ( 3.562760505341037831, 7.378580699531681830, -1.734723475976807094E-15 ) ) ;
#192866 = CARTESIAN_POINT ( 'NONE',  ( 2.859786144356114779, 0.6500800702718724233, -1.690994707955698617 ) ) ;
#192867 = CARTESIAN_POINT ( 'NONE',  ( 6.539320575229254473, 0.5926322452488984593, 1.950287522085321301 ) ) ;
#192868 = CARTESIAN_POINT ( 'NONE',  ( -0.3000000000000068723, 0.6284510210557009424, 1.086836331270357281 ) ) ;
#192869 = CARTESIAN_POINT ( 'NONE',  ( 4.871297188390688149, 6.684807392805372395, 1.249964738027457889 ) ) ;
#192870 = CARTESIAN_POINT ( 'NONE',  ( 3.631172916894987779, 0.04772338994715261129, -1.860622308654858559 ) ) ;
#192871 = CARTESIAN_POINT ( 'NONE',  ( 1.194790368808082759, 1.690169533058868190, 0.9015364962996033071 ) ) ;
#192872 = CARTESIAN_POINT ( 'NONE',  ( 0.6217474354073999621, -0.9722136304874777757, -1.544982199245432897 ) ) ;
#192873 = CARTESIAN_POINT ( 'NONE',  ( -4.858757509019059562, 5.629766575900002401, 2.420000000000000373 ) ) ;
#192874 = CARTESIAN_POINT ( 'NONE',  ( -1.734723475976807094E-15, 2.999999999999988898, -6.938893903907228378E-15 ) ) ;
#192875 = VECTOR ( 'NONE', #84522, 1000.000000000000000 ) ;
#192876 = CARTESIAN_POINT ( 'NONE',  ( 5.960708871395055120, 7.108654626955757116, 1.090683939682752124 ) ) ;
#192877 = CARTESIAN_POINT ( 'NONE',  ( -11.35573736746270335, 9.987295855867214911, 3.554362808847973731 ) ) ;
#192878 = CARTESIAN_POINT ( 'NONE',  ( -3.687454593236990430, 4.364747115940301292, 1.082531754730560403 ) ) ;
#192879 = CARTESIAN_POINT ( 'NONE',  ( 7.131225611108085616, 10.30321839872603462, 1.082531754730558626 ) ) ;
#192880 = CARTESIAN_POINT ( 'NONE',  ( 5.963713532047742127, -0.4821895448718095945, 1.909345749545824367 ) ) ;
#192881 = CARTESIAN_POINT ( 'NONE',  ( -4.874319919312905647, 5.645460313075203018, -1.199719254218446718 ) ) ;
#192882 = CARTESIAN_POINT ( 'NONE',  ( -0.2313892381897282580, 6.510114678062200788, 3.133603478753892446 ) ) ;
#192883 = CARTESIAN_POINT ( 'NONE',  ( 0.1641640845322315523, -1.364019775510204369, 1.584451847793943324 ) ) ;
#192884 = CARTESIAN_POINT ( 'NONE',  ( 6.988338112840064120, 10.24047933403371502, 1.199719254218460707 ) ) ;
#192885 = CARTESIAN_POINT ( 'NONE',  ( 4.946275538936047766, 1.921213873770099445, 0.1421515328255736899 ) ) ;
#192886 = CARTESIAN_POINT ( 'NONE',  ( -6.392833124043511894, 7.417059051927569868, 1.199719254218450271 ) ) ;
#192887 = CARTESIAN_POINT ( 'NONE',  ( 0.9030137451815029026, 1.489685209907613661, 1.054989265776705709 ) ) ;
#192888 = CARTESIAN_POINT ( 'NONE',  ( 2.350463684150871035, 2.206416367115513477, 0.05273732197710182673 ) ) ;
#192889 = ADVANCED_FACE ( 'NONE', ( #204977 ), #175692, .T. ) ;
#192890 = CARTESIAN_POINT ( 'NONE',  ( -6.067740968097372622, 7.047743726685476773, 1.013785590662339642 ) ) ;
#192891 = CARTESIAN_POINT ( 'NONE',  ( 1.423922367354793606, -1.897583212610975734, 0.2371896777705190806 ) ) ;
#192892 = ORIENTED_EDGE ( 'NONE', *, *, #189888, .F. ) ;
#192893 = CARTESIAN_POINT ( 'NONE',  ( 0.7835775553649370062, -1.871284325210004429, 0.6146160330302401498 ) ) ;
#192894 = CARTESIAN_POINT ( 'NONE',  ( 2.436971693805603856, -1.440716923005976646, -1.302479457752574232 ) ) ;
#192895 = CARTESIAN_POINT ( 'NONE',  ( 1.370470000664014254, -0.4925687793003556969, 1.954872606163795989 ) ) ;
#192897 = CARTESIAN_POINT ( 'NONE',  ( 5.453892037968048001, -0.6717839469763884352, 1.735626407379993186 ) ) ;
#192896 = CARTESIAN_POINT ( 'NONE',  ( -4.471156797456668386, 8.438376373666578445, -0.7998128361456362523 ) ) ;
#192898 = CARTESIAN_POINT ( 'NONE',  ( 5.896870467300973750, 5.844380064798101237, 0.7998128361456352531 ) ) ;
#192899 = CARTESIAN_POINT ( 'NONE',  ( -1.040834085586084257E-14, -9.746166700180788567, -9.579665964948867796 ) ) ;
#192900 = CARTESIAN_POINT ( 'NONE',  ( 9.694243528971124846, 11.26870452434320491, 1.199719254218450271 ) ) ;
#192901 = CARTESIAN_POINT ( 'NONE',  ( -4.741601036477307574, 6.554953847355395880, 1.599625672291267398 ) ) ;
#192902 = CARTESIAN_POINT ( 'NONE',  ( -6.831329296439251131, 9.063246493969506545, -1.599625672291271394 ) ) ;
#192903 = CARTESIAN_POINT ( 'NONE',  ( 1.575987392057216940, -1.168677030305173004, 1.853764812240476623 ) ) ;
#192904 = CARTESIAN_POINT ( 'NONE',  ( 2.873965376416980355, 6.296784005887697155, -0.7216878364870267237 ) ) ;
#192905 = CARTESIAN_POINT ( 'NONE',  ( 5.854088466050551887, 10.05179665369283981, 0.7998128361456341429 ) ) ;
#192906 = CARTESIAN_POINT ( 'NONE',  ( 6.141001612134830978, 5.378507234883239896, -2.500000000000000000 ) ) ;
#192908 = ADVANCED_FACE ( 'NONE', ( #4660 ), #35869, .F. ) ;
#192907 = CARTESIAN_POINT ( 'NONE',  ( 2.262075381241589245, 0.7800679334904643270, 1.650788133108482825 ) ) ;
#192909 = CARTESIAN_POINT ( 'NONE',  ( -0.4867935908897400021, 7.427453578138980994, 4.536604770853145396 ) ) ;
#192910 = CARTESIAN_POINT ( 'NONE',  ( -4.223528545856940042, 4.886203710709899006, -1.199719254218446718 ) ) ;
#192911 = AXIS2_PLACEMENT_3D ( 'NONE', #151488, #185019, #203393 ) ;
#192912 = CARTESIAN_POINT ( 'NONE',  ( -5.143355005462953322, 7.892534720870457043, -1.245665949277234841 ) ) ;
#192913 = DIRECTION ( 'NONE',  ( 0.000000000000000000, 1.000000000000000000, 0.000000000000000000 ) ) ;
#192914 = CARTESIAN_POINT ( 'NONE',  ( 9.053093885623066939, 11.58502883802551153, -1.599625672291262513 ) ) ;
#192915 = CARTESIAN_POINT ( 'NONE',  ( 1.400868510093127073, 1.575373640256217733, -1.108617158386180357 ) ) ;
#192916 = CARTESIAN_POINT ( 'NONE',  ( 5.770351633785986145, -0.8788013674413884813, -1.753946858050984048 ) ) ;
#192917 = PRESENTATION_LAYER_ASSIGNMENT (  '', '', ( #165247 ) ) ;
#192918 = CARTESIAN_POINT ( 'NONE',  ( 1.500000000000001332, 15.12500000000000000, 0.000000000000000000 ) ) ;
#192919 = CARTESIAN_POINT ( 'NONE',  ( -6.256197817702116026, 9.386315656372753224, -1.199719254218440723 ) ) ;
#192920 = CARTESIAN_POINT ( 'NONE',  ( 5.392392409933256303, 7.314210449720692786, 1.599625672291267398 ) ) ;
#192921 = CARTESIAN_POINT ( 'NONE',  ( 4.898067072109578035, -0.7382639882421681010, -2.063579870930781546 ) ) ;
#192922 = CARTESIAN_POINT ( 'NONE',  ( 5.009901455449552010, 5.803638771901306725, -1.199719254218452047 ) ) ;
#192923 = CARTESIAN_POINT ( 'NONE',  ( 3.520434184366732389, 0.9265386974339048232, 1.851387837889128640 ) ) ;
#192925 = CARTESIAN_POINT ( 'NONE',  ( 1.364683531249986537, 0.9677083336747538400, -0.7879004041258239610 ) ) ;
#192924 = CARTESIAN_POINT ( 'NONE',  ( -2.290347054751606493, 1.000000000000000888, 11.71088463649534717 ) ) ;
#192926 = ORIENTED_EDGE ( 'NONE', *, *, #206146, .F. ) ;
#192927 = CARTESIAN_POINT ( 'NONE',  ( 3.516502792989243176, -2.123307701433849282, 0.8810689989526691024 ) ) ;
#192929 = ORIENTED_EDGE ( 'NONE', *, *, #104082, .T. ) ;
#192928 = CARTESIAN_POINT ( 'NONE',  ( 6.968527767744093993, 10.11340424813470662, 1.082531754730558626 ) ) ;
#192931 = FACE_OUTER_BOUND ( 'NONE', #106095, .T. ) ;
#192930 = CARTESIAN_POINT ( 'NONE',  ( 3.770576118376296471, 7.413106214832098750, 0.7216878364870257245 ) ) ;
#192933 = EDGE_CURVE ( 'NONE', #62112, #192043, #169971, .T. ) ;
#192932 = CARTESIAN_POINT ( 'NONE',  ( -7.720011280421934963, -5.361065518611648706, -7.836017471263586387 ) ) ;
#192934 = CARTESIAN_POINT ( 'NONE',  ( -0.4500000000000059508, 3.950000000000009059, -0.8338124244295693765 ) ) ;
#192935 = CARTESIAN_POINT ( 'NONE',  ( 3.767467431601259076, 1.079656630588815780, 1.613968600252370322 ) ) ;
#192936 = ORIENTED_EDGE ( 'NONE', *, *, #87194, .T. ) ;
#192937 = CARTESIAN_POINT ( 'NONE',  ( 8.215877899756996783, 12.52901528311778989, 1.040834085586084257E-14 ) ) ;
#192938 = EDGE_CURVE ( 'NONE', #74349, #177991, #133563, .T. ) ;
#192939 = ORIENTED_EDGE ( 'NONE', *, *, #131846, .T. ) ;
#192940 = CARTESIAN_POINT ( 'NONE',  ( 5.642805672956042962, 1.844803604357934779, 0.5037821151940986564 ) ) ;
#192941 = CARTESIAN_POINT ( 'NONE',  ( 6.668995740727024391, -1.579612310505887685, -0.6930582901118372829 ) ) ;
#192942 = CARTESIAN_POINT ( 'NONE',  ( 5.085172837459294826, 1.651341431264556014, 1.157102043685846793 ) ) ;
#192943 = CARTESIAN_POINT ( 'NONE',  ( -1.734723475976807094E-15, 3.481548657788671619, -12.00000000000000178 ) ) ;
#192944 = CARTESIAN_POINT ( 'NONE',  ( 1.331021600797330118, 2.127646391749141941, 0.5858054460900484761 ) ) ;
#192946 = CARTESIAN_POINT ( 'NONE',  ( 10.99970480893080627, -5.907420853759282053, 0.08058608058608522640 ) ) ;
#192945 = CARTESIAN_POINT ( 'NONE',  ( -10.49131193887636826, 11.13428543831092909, 1.040834085586084257E-14 ) ) ;
#192948 = CARTESIAN_POINT ( 'NONE',  ( 6.643818817254954823, 0.6745290893846628277, -1.636350436104140327 ) ) ;
#192947 = CARTESIAN_POINT ( 'NONE',  ( 1.429752723428807215, 1.029013270877369379, -1.819774963352964292 ) ) ;
#192949 = CARTESIAN_POINT ( 'NONE',  ( 5.713517581197447015, 1.944070655204039433, 0.5350908816983344085 ) ) ;
#192951 = CARTESIAN_POINT ( 'NONE',  ( 3.381108394495379699, 2.072348265612040219, -0.9799971971852624586 ) ) ;
#192950 = CARTESIAN_POINT ( 'NONE',  ( 5.747730777550676073, 5.670383760089384495, 0.000000000000000000 ) ) ;
#192952 = CARTESIAN_POINT ( 'NONE',  ( 0.6557207866510657013, -1.263530833501663952, 1.197007909421362370 ) ) ;
#192953 = CARTESIAN_POINT ( 'NONE',  ( 2.584367824843319283, 1.138156186954141003, 1.789115803205274080 ) ) ;
#192954 = DIRECTION ( 'NONE',  ( -0.7592566023653004592, -0.6507913734559639396, 0.000000000000000000 ) ) ;
#192955 = CARTESIAN_POINT ( 'NONE',  ( 1.545803854144804479, 1.604466568860075437, -0.6577250193331334316 ) ) ;
#192956 = CARTESIAN_POINT ( 'NONE',  ( -3.755786496842897795E-14, 1.109375000341423112, -1.570758158831814466 ) ) ;
#192957 = CARTESIAN_POINT ( 'NONE',  ( 1.802945237480069407, -1.574492340324705753, 0.9918895310334940874 ) ) ;
#192958 = CARTESIAN_POINT ( 'NONE',  ( 1.135490968158389791, -0.05309211241652118246, -2.170675730929682246 ) ) ;
#192959 = CARTESIAN_POINT ( 'NONE',  ( 2.905482715143858030, -1.942096844255640109, 0.5424705965835219246 ) ) ;
#192960 = CARTESIAN_POINT ( 'NONE',  ( 5.156250000000004441, -1.895863743163967108, 0.7852924748302536617 ) ) ;
#192961 = CARTESIAN_POINT ( 'NONE',  ( 0.7499999999999902300, 2.014583334016148530, 1.299038105676669330 ) ) ;
#192962 = CARTESIAN_POINT ( 'NONE',  ( 6.410771793481705672, 1.425725087049932505, -1.295833391663123724 ) ) ;
#192963 = CARTESIAN_POINT ( 'NONE',  ( -1.364683531250014514, 13.08854166700806410, -0.7879004041258335089 ) ) ;
#192964 = CARTESIAN_POINT ( 'NONE',  ( 3.410577425615939795, -2.218986280728425076, -0.1058077642441344057 ) ) ;
#192965 = ORIENTED_EDGE ( 'NONE', *, *, #122755, .F. ) ;
#192966 = CARTESIAN_POINT ( 'NONE',  ( 3.853570894305305305, 8.531289074211816370, 2.447542183238072155 ) ) ;
#192967 = CARTESIAN_POINT ( 'NONE',  ( 0.7499999999999885647, -0.7666666666666446250, 1.299038105676657340 ) ) ;
#192968 = CARTESIAN_POINT ( 'NONE',  ( 7.401861798056875053, 10.72292363345333399, -1.199719254218441611 ) ) ;
#192969 =( NAMED_UNIT ( * ) SI_UNIT ( $, .STERADIAN. ) SOLID_ANGLE_UNIT ( ) );
#192970 = VECTOR ( 'NONE', #181082, 1000.000000000000000 ) ;
#192971 = CARTESIAN_POINT ( 'NONE',  ( 0.2746299231596514012, 1.718356743839201561, -0.6618312839273902126 ) ) ;
#192972 = CARTESIAN_POINT ( 'NONE',  ( 4.176187491914356897, -1.006606191838583131, -1.683785057063936552 ) ) ;
#192974 = CARTESIAN_POINT ( 'NONE',  ( -5.910991785878165317, 8.879612269291090598, -1.082531754730538864 ) ) ;
#192973 = CARTESIAN_POINT ( 'NONE',  ( 3.684065054611349144, 5.321161868511784299, -1.599625672291262513 ) ) ;
#192975 = CARTESIAN_POINT ( 'NONE',  ( -1.369796495953883531, 4.288649915869804374, 0.2487645435796815019 ) ) ;
#192976 = CARTESIAN_POINT ( 'NONE',  ( 6.169232171785941965, 0.1756554044750150145, -2.255672955852848993 ) ) ;
#192977 = CARTESIAN_POINT ( 'NONE',  ( 2.084505489600170680, 1.189443612574309084, -1.685003561244757364 ) ) ;
#192978 = CARTESIAN_POINT ( 'NONE',  ( -6.561256274009600986, 9.742217188731485678, -1.199719254218440723 ) ) ;
#192979 = ORIENTED_EDGE ( 'NONE', *, *, #127934, .T. ) ;
#192980 = CARTESIAN_POINT ( 'NONE',  ( 1.499999999999989120, 1.056250000682816603, 0.000000000000000000 ) ) ;
#192981 = CARTESIAN_POINT ( 'NONE',  ( 3.655401173194738007, 0.4573680094964555076, -1.813624142381641491 ) ) ;
#192982 = CARTESIAN_POINT ( 'NONE',  ( 2.795252500310735133, 1.254151915811404061, -1.197898925204267995 ) ) ;
#192983 = CARTESIAN_POINT ( 'NONE',  ( 0.08209332325101456607, -1.073118421065310413, 2.025687816139466246 ) ) ;
#192984 = CARTESIAN_POINT ( 'NONE',  ( 1.237671066534186792, -1.994493743981802680, 0.9446329514863486265 ) ) ;
#192985 = CARTESIAN_POINT ( 'NONE',  ( 3.959979445722985325, 2.145676688911036578, -0.2621329562078680842 ) ) ;
#192986 = CARTESIAN_POINT ( 'NONE',  ( 5.296799794911354553, 1.588725326081788847, 1.116492485978479499 ) ) ;
#192988 = UNCERTAINTY_MEASURE_WITH_UNIT (LENGTH_MEASURE( 1.000000000000000082E-05 ), #110478, 'distance_accuracy_value', 'NONE');
#192987 = CARTESIAN_POINT ( 'NONE',  ( 6.889956934492897034, -0.7990643998789861424, 1.689675875712663755 ) ) ;
#192989 = CARTESIAN_POINT ( 'NONE',  ( 0.4374999999988640753, 1.451031289089056431, -1.451031289061139651 ) ) ;
#192990 = DIRECTION ( 'NONE',  ( -1.000000000000000000, -1.561251128379122346E-12, 0.000000000000000000 ) ) ;
#192991 = CARTESIAN_POINT ( 'NONE',  ( -5.662713974411738960, 5.571197489760607802, -0.2163730220445139740 ) ) ;
#192992 = CARTESIAN_POINT ( 'NONE',  ( 5.854138739207011888, 0.1455364397412381439, -2.011204036175239018 ) ) ;
#192993 = CARTESIAN_POINT ( 'NONE',  ( -7.994504133552415404, 12.47867192245318435, -0.7998128361456281477 ) ) ;
#192994 =( BOUNDED_CURVE ( )  B_SPLINE_CURVE ( 2, ( #132868, #52647, #33200 ),
 .UNSPECIFIED., .F., .T. ) 
 B_SPLINE_CURVE_WITH_KNOTS ( ( 3, 3 ),
 ( 0.1472187422488249464, 0.1500000000000002165 ),
 .UNSPECIFIED. ) 
 CURVE ( )  GEOMETRIC_REPRESENTATION_ITEM ( )  RATIONAL_B_SPLINE_CURVE ( ( 0.9405305184077485947, 0.9105717077955789440, 1.000000000000007105 ) ) 
 REPRESENTATION_ITEM ( '' )  );
#192995 = CARTESIAN_POINT ( 'NONE',  ( 6.109920781252839994, 10.27999134477033216, 1.040834085586084257E-14 ) ) ;
#192996 = DIRECTION ( 'NONE',  ( 1.000000000000000000, 0.000000000000000000, 0.000000000000000000 ) ) ;
#192997 = CARTESIAN_POINT ( 'NONE',  ( 3.316849939159485228, 1.650902842016691130, 0.7798126646740562995 ) ) ;
#192998 = CARTESIAN_POINT ( 'NONE',  ( 1.624349867039249329, -1.226448341774049267, -1.834376716147153363 ) ) ;
#192999 = VERTEX_POINT ( 'NONE', #71805 ) ;
#193000 = CARTESIAN_POINT ( 'NONE',  ( -4.543390873910949423, 6.393985001019784953, 1.443375672974058777 ) ) ;
#193001 = CARTESIAN_POINT ( 'NONE',  ( -1.642778471874998480, -3.288541666188707246, 2.845375778867863303 ) ) ;
#193002 = CARTESIAN_POINT ( 'NONE',  ( -7.588813295347149435, 9.876701482703580837, -1.599625672291263179 ) ) ;
#193003 = CARTESIAN_POINT ( 'NONE',  ( 0.7737015921927943296, 0.3898077916253924746, -1.981631471940727973 ) ) ;
#193004 = CARTESIAN_POINT ( 'NONE',  ( 1.682450335255514240, 1.092831414372618326, 1.817064408815848964 ) ) ;
#193005 = CARTESIAN_POINT ( 'NONE',  ( 11.92046840572485777, 9.947478752057280715, 1.382231356234940867 ) ) ;
#193006 = ORIENTED_EDGE ( 'NONE', *, *, #9864, .F. ) ;
#193007 = CARTESIAN_POINT ( 'NONE',  ( -4.586401103172829785, 8.572828063668767484, 0.7998128361456281477 ) ) ;
#193008 = CARTESIAN_POINT ( 'NONE',  ( 1.533807339325540475, 1.103149047995868104, 1.498595216881804859 ) ) ;
#193009 = CARTESIAN_POINT ( 'NONE',  ( 4.542145155778077203, 5.257923088951247159, -1.199719254218452047 ) ) ;
#193010 = CARTESIAN_POINT ( 'NONE',  ( 0.7960496800812133511, -0.7770375076890515542, 2.017388685454111652 ) ) ;
#193011 = CARTESIAN_POINT ( 'NONE',  ( 5.959611329766301147, -1.915599147091971544, -0.6298778581111733610 ) ) ;
#193012 = ORIENTED_EDGE ( 'NONE', *, *, #120622, .F. ) ;
#193013 = ORIENTED_EDGE ( 'NONE', *, *, #140820, .F. ) ;
#193014 = CARTESIAN_POINT ( 'NONE',  ( 0.000000000000000000, 6.487495393664096888, -3.100011470320000573 ) ) ;
#193016 = EDGE_CURVE ( 'NONE', #48301, #210699, #197804, .T. ) ;
#193015 = CARTESIAN_POINT ( 'NONE',  ( 4.213378774425760476, -0.3099129147984269195, 1.799030153321119263 ) ) ;
#193017 = VECTOR ( 'NONE', #71678, 1000.000000000000000 ) ;
#193020 = ORIENTED_EDGE ( 'NONE', *, *, #90081, .T. ) ;
#193019 = CARTESIAN_POINT ( 'NONE',  ( -4.747088307715054967, 7.009658186011790804, -1.421664413759090806 ) ) ;
#193018 = CARTESIAN_POINT ( 'NONE',  ( -5.061990249855848667, 6.999017606288844284, -1.599625672291271394 ) ) ;
#193021 = CARTESIAN_POINT ( 'NONE',  ( 6.598740849494261873, 6.770918179921630475, -0.1579934589533253664 ) ) ;
#193022 = CARTESIAN_POINT ( 'NONE',  ( 6.362657644764971643, -0.6818896071447739793, 1.897407954007489295 ) ) ;
#193023 = CARTESIAN_POINT ( 'NONE',  ( 6.210883717528068892, -0.2205035313364057392, 1.827825250963102111 ) ) ;
#193024 = CARTESIAN_POINT ( 'NONE',  ( -0.02299388927988389383, 2.039721852852835582, -2.328191723522631928 ) ) ;
#193025 = CARTESIAN_POINT ( 'NONE',  ( 4.916800105644766994, 1.594097815661306816, -1.668853466001555486 ) ) ;
#193026 = CARTESIAN_POINT ( 'NONE',  ( 4.854701522145073334, 7.821512988214679218, -1.199719254218450271 ) ) ;
#193027 = CARTESIAN_POINT ( 'NONE',  ( 5.694645791630270182, -0.5191100231263061637, -2.098234375727751733 ) ) ;
#193028 = CARTESIAN_POINT ( 'NONE',  ( 1.821723684117615427, 1.116499850783551073, -1.588862189236692091 ) ) ;
#193029 = CARTESIAN_POINT ( 'NONE',  ( 4.376513399274863936, -0.3984044028133710835, 2.263477716089700387 ) ) ;
#193030 = FACE_BOUND ( 'NONE', #69600, .T. ) ;
#193031 = CARTESIAN_POINT ( 'NONE',  ( -5.915100157312088491, 10.12297696016459092, -0.7998128361456362523 ) ) ;
#193032 = CARTESIAN_POINT ( 'NONE',  ( 4.364026845288040413, 0.8817440624687390427, 1.649792572839225091 ) ) ;
#193033 = ORIENTED_EDGE ( 'NONE', *, *, #179509, .T. ) ;
#193035 = CIRCLE ( 'NONE', #155018, 6.200000000000000178 ) ;
#193034 = AXIS2_PLACEMENT_3D ( 'NONE', #183086, #100767, #166849 ) ;
#193038 = CARTESIAN_POINT ( 'NONE',  ( -4.288121723672178476, 8.224835454251337552, -0.7998128361456362523 ) ) ;
#193037 = CARTESIAN_POINT ( 'NONE',  ( -1.500000000000015099, -0.08958333265051321437, -0.8660254037844383745 ) ) ;
#193036 = CARTESIAN_POINT ( 'NONE',  ( 2.478646075381494285, -1.315928518397539548, 1.387899491812602859 ) ) ;
#193039 = CARTESIAN_POINT ( 'NONE',  ( 4.494872972331320327, -0.4818267175418550208, -2.153482813429814069 ) ) ;
#193040 = CARTESIAN_POINT ( 'NONE',  ( 6.883263157960364254, 2.447565407927353220, 2.329071302269662080 ) ) ;
#193041 = CARTESIAN_POINT ( 'NONE',  ( -0.2110808730067144090, 0.7535804146166940054, -1.881771259391984197 ) ) ;
#193042 = CARTESIAN_POINT ( 'NONE',  ( 6.509323147892504657, 6.766834225395614411, 0.000000000000000000 ) ) ;
#193043 = CARTESIAN_POINT ( 'NONE',  ( -5.383996397958228819, 8.335060660042973524, 1.082531754730550855 ) ) ;
#193044 = CARTESIAN_POINT ( 'NONE',  ( 1.370321444179344983, -1.253680685346630019, 1.521333489566406127 ) ) ;
#193045 = CARTESIAN_POINT ( 'NONE',  ( 1.255362601414770296, -1.817582055312426004, 1.421667062125511860 ) ) ;
#193046 = CARTESIAN_POINT ( 'NONE',  ( 2.980854556682940526, 1.846358069237159949, 0.6635599008937702603 ) ) ;
#193047 = CARTESIAN_POINT ( 'NONE',  ( 11.55950211276791251, 11.29999999999998295, 3.221476510067111665 ) ) ;
#193048 = CARTESIAN_POINT ( 'NONE',  ( 6.473490848629269045, -0.2583879851764906976, 2.046290913384725130 ) ) ;
#193049 = CARTESIAN_POINT ( 'NONE',  ( 3.660338286009610975, 6.253849852777763729, -1.082531754730543083 ) ) ;
#193050 = CARTESIAN_POINT ( 'NONE',  ( 3.995327539805045181, -0.3399590882401174463, 1.987497567597557468 ) ) ;
#193051 = CARTESIAN_POINT ( 'NONE',  ( 4.258142763143749399, 7.125527769379820242, 1.199719254218451159 ) ) ;
#193052 = VERTEX_POINT ( 'NONE', #69673 ) ;
#193053 = CARTESIAN_POINT ( 'NONE',  ( -10.45741655484220267, 11.09474082360439873, -0.7998128361456221525 ) ) ;
#193054 = CARTESIAN_POINT ( 'NONE',  ( -3.475000000000000533, -1.399999999999998579, 0.000000000000000000 ) ) ;
#193055 = CARTESIAN_POINT ( 'NONE',  ( 8.062294901620731480, 12.55776115186623620, 1.040834085586084257E-14 ) ) ;
#193056 = CARTESIAN_POINT ( 'NONE',  ( 1.727621483090465926, 0.1626789094613217412, -2.165059144495153021 ) ) ;
#193057 = CARTESIAN_POINT ( 'NONE',  ( 6.364626766972446781, 6.390095747748158139, 0.7998128361456350310 ) ) ;
#193058 = B_SPLINE_CURVE_WITH_KNOTS ( 'NONE', 3,
 ( #174320, #141841, #191589, #90931 ),
 .UNSPECIFIED., .F., .F.,
 ( 4, 4 ),
 ( 0.0006294919072214776642, 0.001039439579420692490 ),
 .UNSPECIFIED. ) ;
#193059 = CARTESIAN_POINT ( 'NONE',  ( 11.41381675112459959, 10.90000000000001101, -3.704697986577260682 ) ) ;
#193060 = CARTESIAN_POINT ( 'NONE',  ( -9.604686356149278126, 4.518467169708413778, -7.193747284969076006 ) ) ;
#193061 = CARTESIAN_POINT ( 'NONE',  ( 2.829206387438303327, -1.746784236434803850, 0.6695917499066756928 ) ) ;
#193062 = CARTESIAN_POINT ( 'NONE',  ( 6.591117433763723277, 1.884315261875910474, -1.059023293578951863 ) ) ;
#193063 = EDGE_CURVE ( 'NONE', #79244, #211530, #51065, .T. ) ;
#193065 = CARTESIAN_POINT ( 'NONE',  ( 6.727182134110237577, 2.483225874290733159, 2.096421262816303255 ) ) ;
#193064 = CYLINDRICAL_SURFACE ( 'NONE', #193133, 1.500000000000005107 ) ;
#193066 = CARTESIAN_POINT ( 'NONE',  ( -1.364683531250010295, 5.801041667008088432, -0.7879004041258300672 ) ) ;
#193067 = CARTESIAN_POINT ( 'NONE',  ( -1.492698588115513703, 3.265477196593705056, -0.1666886929329597367 ) ) ;
#193068 = CARTESIAN_POINT ( 'NONE',  ( 2.508343198132975349, -1.907285675847451234, -0.1387974571645037292 ) ) ;
#193069 = CIRCLE ( 'NONE', #206816, 0.08000000000000034861 ) ;
#193070 = CARTESIAN_POINT ( 'NONE',  ( 4.504631171302628800, 1.367295333670435653, -1.123774403194759408 ) ) ;
#193071 = CARTESIAN_POINT ( 'NONE',  ( 1.471198412684338264, -1.640640410176617658, -0.9821394255850326438 ) ) ;
#193072 = CARTESIAN_POINT ( 'NONE',  ( -6.227272627378437342, 6.159572908229946187, -0.7998128361456291469 ) ) ;
#193074 = CARTESIAN_POINT ( 'NONE',  ( 6.292599812010432281, 1.415705964336026357, -1.290654269910092911 ) ) ;
#193073 = DIRECTION ( 'NONE',  ( 0.000000000000000000, -1.000000000000000000, 0.000000000000000000 ) ) ;
#193075 = CARTESIAN_POINT ( 'NONE',  ( -0.7500000000000006661, -0.6416666666666446250, -1.299038105676652011 ) ) ;
#193076 = CARTESIAN_POINT ( 'NONE',  ( 0.5376586404672692998, 1.932363751568724641, -0.7437053376125392079 ) ) ;
#193077 = CARTESIAN_POINT ( 'NONE',  ( -0.6823417656250003738, -0.7197916663252492686, -1.181850606188749264 ) ) ;
#193079 = EDGE_CURVE ( 'NONE', #158402, #102449, #11080, .T. ) ;
#193078 = AXIS2_PLACEMENT_3D ( 'NONE', #92213, #158265, #9854 ) ;
#193080 = CARTESIAN_POINT ( 'NONE',  ( -15.75000000000000000, 13.39999999999998259, 1.399999999999998579 ) ) ;
#193081 = CARTESIAN_POINT ( 'NONE',  ( 5.032044620589739559, 0.9611010790777809731, -1.604743002217932313 ) ) ;
#193082 = CARTESIAN_POINT ( 'NONE',  ( 1.840199252755945425, 1.805614550920462635, 0.2691313018618191055 ) ) ;
#193084 = CARTESIAN_POINT ( 'NONE',  ( 4.624009687016504166, 8.337032093926254106, -0.3390773965592456252 ) ) ;
#193083 = CARTESIAN_POINT ( 'NONE',  ( 5.250674450588199704, 0.6379336648693231249, 2.112661011922472021 ) ) ;
#193085 = CARTESIAN_POINT ( 'NONE',  ( -1.364683531250000748, -0.7406249996585803075, 0.000000000000000000 ) ) ;
#193086 = CARTESIAN_POINT ( 'NONE',  ( 2.787610149020779193, -1.925555389141724527, 0.7399787145165384050 ) ) ;
#193087 = EDGE_CURVE ( 'NONE', #80159, #195702, #123881, .T. ) ;
#193088 = CARTESIAN_POINT ( 'NONE',  ( -8.178592977541617515, 10.56477777859713463, 1.599625672291295375 ) ) ;
#193089 = SURFACE_SIDE_STYLE ('',( #81484 ) ) ;
#193090 = CARTESIAN_POINT ( 'NONE',  ( 8.041957671200231417, 12.53403438304231976, 1.040834085586084257E-14 ) ) ;
#193091 = CARTESIAN_POINT ( 'NONE',  ( 1.378728738066228754, 4.086408449757453099, -0.5908528300941744416 ) ) ;
#193092 =( NAMED_UNIT ( * ) PLANE_ANGLE_UNIT ( ) SI_UNIT ( $, .RADIAN. ) );
#193093 = CARTESIAN_POINT ( 'NONE',  ( 7.367930134383754215, 7.560616343061329125, -0.7998128361456341429 ) ) ;
#193094 = ORIENTED_EDGE ( 'NONE', *, *, #53693, .T. ) ;
#193095 = CARTESIAN_POINT ( 'NONE',  ( 5.336411075974297979, -1.153114810915600641, 1.719314882265559286 ) ) ;
#193096 = CARTESIAN_POINT ( 'NONE',  ( -0.6823417656250003738, -0.4697916663252491021, -1.181850606188749264 ) ) ;
#193097 = CARTESIAN_POINT ( 'NONE',  ( 2.864712396292764751, -1.492883925411474078, 1.563474562115530375 ) ) ;
#193098 = CARTESIAN_POINT ( 'NONE',  ( -4.612386318492403880, 8.373339136000554461, 0.1892495524792922046 ) ) ;
#193099 = CARTESIAN_POINT ( 'NONE',  ( 3.668621814757520916, 0.7290426041848938610, 1.883679974206926122 ) ) ;
#193100 = CARTESIAN_POINT ( 'NONE',  ( 6.720655732516667591, 2.416141799769660370, 2.554522868665403568 ) ) ;
#193101 = ORIENTED_EDGE ( 'NONE', *, *, #133575, .F. ) ;
#193104 = CARTESIAN_POINT ( 'NONE',  ( 6.887178846062110615, 9.058127958537705027, -1.443375672974057666 ) ) ;
#193103 = CARTESIAN_POINT ( 'NONE',  ( -3.475000000000000533, -1.429166666666668251, -2.006292185433948827 ) ) ;
#193102 = SURFACE_SIDE_STYLE ('',( #214365 ) ) ;
#193105 = CARTESIAN_POINT ( 'NONE',  ( -3.811250578772981346, 6.500190537660166079, -1.082531754730546636 ) ) ;
#193106 = CARTESIAN_POINT ( 'NONE',  ( 0.8488426437929346147, -1.825078332268307513, -0.8578388575243289793 ) ) ;
#193107 = B_SPLINE_CURVE_WITH_KNOTS ( 'NONE', 3,
 ( #184922, #88527, #102632, #120015, #52804, #203300 ),
 .UNSPECIFIED., .F., .F.,
 ( 4, 2, 4 ),
 ( 0.000000000000000000, 0.0003157158648874031190, 0.0006314317297748062380 ),
 .UNSPECIFIED. ) ;
#193109 = CARTESIAN_POINT ( 'NONE',  ( 6.093348126157794198, -0.7399906200981147819, 2.062998119606203939 ) ) ;
#193108 = CARTESIAN_POINT ( 'NONE',  ( -6.091691091241777656, 6.001394449403842479, 0.7998128361456341429 ) ) ;
#193110 = CARTESIAN_POINT ( 'NONE',  ( 0.7499999999999920064, 4.514583334016150751, 1.299038105676669330 ) ) ;
#193111 = CARTESIAN_POINT ( 'NONE',  ( 4.588094604188536429, 1.105678411722615051, 1.560157546714964871 ) ) ;
#193112 = CARTESIAN_POINT ( 'NONE',  ( -3.602716132929368875, 5.226254793216122074, 1.599625672291267398 ) ) ;
#193113 = CARTESIAN_POINT ( 'NONE',  ( 7.415946836550727284, 7.754285518838408109, 0.7216878364870317197 ) ) ;
#193115 = CARTESIAN_POINT ( 'NONE',  ( 3.146111402376899235, 0.9091623069825971459, 1.799915193831227889 ) ) ;
#193114 = CARTESIAN_POINT ( 'NONE',  ( -9.612367721964613310, 11.27714576612263997, -1.082531754730537976 ) ) ;
#193116 = CARTESIAN_POINT ( 'NONE',  ( -0.6823417656250003738, 13.71354166700806942, 1.181850606188754593 ) ) ;
#193117 = COLOUR_RGB ( '', 0.40784314, 0.44705882, 0.49803922) ;
#193118 = CARTESIAN_POINT ( 'NONE',  ( -5.113360211009450040, 5.994616996712990975, -1.199719254218453823 ) ) ;
#193119 = CARTESIAN_POINT ( 'NONE',  ( 5.526277428723715524, 1.024295688422135031, -1.387495638070087134 ) ) ;
#193120 = CARTESIAN_POINT ( 'NONE',  ( 6.984385409695311964, 8.177479728513226576, 1.199719254218452935 ) ) ;
#193121 = CARTESIAN_POINT ( 'NONE',  ( 8.432808358020004391, 12.78210081775797669, 0.7216878364870438212 ) ) ;
#193122 = CARTESIAN_POINT ( 'NONE',  ( 6.925078400183575233, 7.629137130509070275, 2.455651831298297338 ) ) ;
#193123 = CARTESIAN_POINT ( 'NONE',  ( 3.813614929637610285, -1.843318686535614148, 0.3169883347873064250 ) ) ;
#193124 =( NAMED_UNIT ( * ) SI_UNIT ( $, .STERADIAN. ) SOLID_ANGLE_UNIT ( ) );
#193125 = CARTESIAN_POINT ( 'NONE',  ( 0.9892257793299992219, 0.1485654903058269416, 2.064951490685583924 ) ) ;
#193126 = DIRECTION ( 'NONE',  ( 0.000000000000000000, 0.000000000000000000, -1.000000000000000000 ) ) ;
#193127 = VERTEX_POINT ( 'NONE', #189846 ) ;
#193128 = CARTESIAN_POINT ( 'NONE',  ( 5.953728957075980155, -1.316865622510310141, -1.244172183657651365 ) ) ;
#193129 = CARTESIAN_POINT ( 'NONE',  ( 3.379725431556547477, 7.165039780116438273, -1.734723475976807094E-15 ) ) ;
#193130 = CARTESIAN_POINT ( 'NONE',  ( 0.000000000000000000, 7.999999999999992895, 7.750000000000000888 ) ) ;
#193131 = CARTESIAN_POINT ( 'NONE',  ( 0.7030050633033817498, 1.597335618216610964, -0.8546489784103310505 ) ) ;
#193132 = CARTESIAN_POINT ( 'NONE',  ( 4.516274566683592617, 8.283087737857252719, -0.7216878364870357165 ) ) ;
#193133 = AXIS2_PLACEMENT_3D ( 'NONE', #208241, #161660, #60943 ) ;
#193134 = CARTESIAN_POINT ( 'NONE',  ( 11.88048553210577296, 7.839794170119552597, 1.743655026309894218 ) ) ;
#193135 = CARTESIAN_POINT ( 'NONE',  ( 3.205210054081304438, -0.4271916898582402422, 2.149238826137919389 ) ) ;
#193136 = ORIENTED_EDGE ( 'NONE', *, *, #74793, .T. ) ;
#193138 = CARTESIAN_POINT ( 'NONE',  ( 9.053093885623066939, 11.58502883802551153, -1.599625672291262513 ) ) ;
#193137 = CARTESIAN_POINT ( 'NONE',  ( 1.082386330805637398, 1.171445227557347923, -1.573568114121715933 ) ) ;
#193139 = CARTESIAN_POINT ( 'NONE',  ( 5.255460224911852052, 1.844849436727209469, -0.5155117042133209315 ) ) ;
#193140 = CARTESIAN_POINT ( 'NONE',  ( -1.436838838544753916, 7.449283400311742298, 4.203727439823590650 ) ) ;
#193141 = CARTESIAN_POINT ( 'NONE',  ( -6.027110718723775129, 7.076430883291389584, 1.047497865993127553 ) ) ;
#193142 = CARTESIAN_POINT ( 'NONE',  ( -0.6823417656250246877, -0.1989583329919109023, 1.181850606188755259 ) ) ;
#193144 = ORIENTED_EDGE ( 'NONE', *, *, #197058, .F. ) ;
#193143 = CARTESIAN_POINT ( 'NONE',  ( 4.677199807034550183, 8.400557508274889784, 1.040834085586084257E-14 ) ) ;
#193145 = CARTESIAN_POINT ( 'NONE',  ( -9.503902493499651882, 10.19023378527882784, 1.040834085586084257E-14 ) ) ;
#193146 = CARTESIAN_POINT ( 'NONE',  ( 1.323354039402934390, -0.05256100377049736927, 2.161234000603563299 ) ) ;
#193147 = CARTESIAN_POINT ( 'NONE',  ( -4.176793841461789114, 7.030620694084159794, -1.199719254218455378 ) ) ;
#193148 = CARTESIAN_POINT ( 'NONE',  ( 7.512626515748109135, 8.897724035528543851, 1.082531754730549967 ) ) ;
#193149 = CARTESIAN_POINT ( 'NONE',  ( 1.588595499965880675, -0.2641367610144580991, -1.806243275932853498 ) ) ;
#193150 = CARTESIAN_POINT ( 'NONE',  ( 0.08834397731360790762, 1.226219587655341448, 1.729930300845914815 ) ) ;
#193151 = CARTESIAN_POINT ( 'NONE',  ( 4.524309061075334704, 1.122661849025725189, -1.439470297551891154 ) ) ;
#193152 = ADVANCED_FACE ( 'NONE', ( #59850 ), #13724, .F. ) ;
#193153 = CARTESIAN_POINT ( 'NONE',  ( 12.19510520210794979, 6.199134917050342253, -2.169279492894659711 ) ) ;
#193154 = CARTESIAN_POINT ( 'NONE',  ( 3.146637304467227558, 1.866760668956708447, 0.4145885930168375921 ) ) ;
#193155 = VERTEX_POINT ( 'NONE', #211422 ) ;
#193156 = CARTESIAN_POINT ( 'NONE',  ( 3.824621415324851892, -1.324631885467566716, 1.457714561274085163 ) ) ;
#193157 = VERTEX_POINT ( 'NONE', #46830 ) ;
#193158 = CARTESIAN_POINT ( 'NONE',  ( 5.460475975554013317, -1.757383149004720924, -0.8268225932778446863 ) ) ;
#193159 = ORIENTED_EDGE ( 'NONE', *, *, #71115, .T. ) ;
#193160 = CARTESIAN_POINT ( 'NONE',  ( -7.110325215724114578, 7.260077271291732082, 0.000000000000000000 ) ) ;
#193162 = CARTESIAN_POINT ( 'NONE',  ( 6.135037582782754129, 1.979230198018981701, 0.7618025574447004900 ) ) ;
#193161 = CARTESIAN_POINT ( 'NONE',  ( -5.285699784481336927, 7.260012063351913625, 1.599625672291263179 ) ) ;
#193163 = CARTESIAN_POINT ( 'NONE',  ( 6.143253000323500856, 10.18122924377050609, -0.7216878364870458196 ) ) ;
#193164 = CARTESIAN_POINT ( 'NONE',  ( 4.072844535355981677, -1.414876986328793329, 1.286614418101794444 ) ) ;
#193165 = CARTESIAN_POINT ( 'NONE',  ( 4.521492410791133842, 7.227233577430748568, -1.288726771885986055 ) ) ;
#193166 = CARTESIAN_POINT ( 'NONE',  ( 0.000000000000000000, -3.042800438942089514, 0.000000000000000000 ) ) ;
#193167 = DIRECTION ( 'NONE',  ( -1.000000000000000000, 7.771561172376097755E-16, 4.440892098500627148E-16 ) ) ;
#193168 = CARTESIAN_POINT ( 'NONE',  ( 4.936577329151614180, 4.931964103531220722, -0.7216878364870458196 ) ) ;
#193169 = CARTESIAN_POINT ( 'NONE',  ( 5.707686766122681554, 1.525977179164988540, 1.313104676043591601 ) ) ;
#193170 = CARTESIAN_POINT ( 'NONE',  ( -1.420000000000021911, 6.280000000000042881, 2.873333333333347728 ) ) ;
#193171 = CARTESIAN_POINT ( 'NONE',  ( 5.637271085457097541, -1.648663388651723460, 0.7845467231081537651 ) ) ;
#193172 = CARTESIAN_POINT ( 'NONE',  ( 2.330607996690749140, -1.275545549462468120, 1.630658604070814199 ) ) ;
#193173 = CARTESIAN_POINT ( 'NONE',  ( -6.887178846062109727, 10.01849717283904262, -1.082531754730537976 ) ) ;
#193174 = AXIS2_PLACEMENT_3D ( 'NONE', #97580, #19482, #135396 ) ;
#193175 = CARTESIAN_POINT ( 'NONE',  ( -5.622963654236769138, 7.379252650573795869, -1.237363127855268141 ) ) ;
#193176 = DIRECTION ( 'NONE',  ( -1.000000000000000000, 0.000000000000000000, 0.000000000000000000 ) ) ;
#193177 = CARTESIAN_POINT ( 'NONE',  ( 3.285556943750000070, -3.084374999522042415, 0.000000000000000000 ) ) ;
#193178 = CARTESIAN_POINT ( 'NONE',  ( 5.601490020740366838, 9.686822124172440596, 1.040834085586084257E-14 ) ) ;
#193179 = DIRECTION ( 'NONE',  ( -0.000000000000000000, 1.000000000000000000, -0.000000000000000000 ) ) ;
#193180 = FACE_OUTER_BOUND ( 'NONE', #158335, .T. ) ;
#193181 = CARTESIAN_POINT ( 'NONE',  ( 1.364683531250000303, 12.31770833367473195, -0.7879004041258355073 ) ) ;
#193182 = CARTESIAN_POINT ( 'NONE',  ( -3.425406365747000859, 7.148057860013469877, 1.040834085586084257E-14 ) ) ;
#193184 = CARTESIAN_POINT ( 'NONE',  ( -7.795011973214244883, 8.058878488363559356, 0.7998128361456341429 ) ) ;
#193183 = CARTESIAN_POINT ( 'NONE',  ( 7.664865541498710577, -5.787795860784239466, -7.047292192037250658 ) ) ;
#193185 = CARTESIAN_POINT ( 'NONE',  ( 3.674194220352343443, 1.259077133501560697, 1.192749331401379731 ) ) ;
#193186 = CARTESIAN_POINT ( 'NONE',  ( -4.822949958159302497, 6.649860922651058992, -1.599625672291256295 ) ) ;
#193187 = VECTOR ( 'NONE', #35368, 1000.000000000000000 ) ;
#193188 = CARTESIAN_POINT ( 'NONE',  ( 1.463825199929311260, -0.5068179562870354093, 2.007114080642191656 ) ) ;
#193189 = CARTESIAN_POINT ( 'NONE',  ( 2.917688350237046979, -1.423917071783699972, -1.567024636986138253 ) ) ;
#193190 = CARTESIAN_POINT ( 'NONE',  ( 4.867540842506059562, 5.637551390133895168, -1.199719254218452047 ) ) ;
#193191 = CARTESIAN_POINT ( 'NONE',  ( 7.995557903757111617, 10.35123685918189729, 1.599625672291281386 ) ) ;
#193192 = CARTESIAN_POINT ( 'NONE',  ( 0.1417672014102085154, 6.428417890535995660, 3.204557187381015915 ) ) ;
#193193 = CARTESIAN_POINT ( 'NONE',  ( 0.6198874644624132735, 1.948816017023939251, -0.2832832528399802374 ) ) ;
#193194 = CARTESIAN_POINT ( 'NONE',  ( 4.279786810092509164, 7.480689796721937235, 1.046525044888670486 ) ) ;
#193195 = CARTESIAN_POINT ( 'NONE',  ( 4.690757960648224589, 6.495636925554817864, 1.443375672974062551 ) ) ;
#193197 = CARTESIAN_POINT ( 'NONE',  ( 0.000000000000000000, 6.999999999999999112, 0.000000000000000000 ) ) ;
#193196 = CARTESIAN_POINT ( 'NONE',  ( 1.737499999999999378, -1.166666666666666519, -3.009438278150925683 ) ) ;
#193198 = CARTESIAN_POINT ( 'NONE',  ( 3.504133162399528434, -0.9285911969159079682, -2.095928835653658062 ) ) ;
#193200 = EDGE_CURVE ( 'NONE', #168104, #97632, #118806, .T. ) ;
#193199 = CARTESIAN_POINT ( 'NONE',  ( 0.1350027811974127134, -1.670744041527939094, 0.7364786222084362954 ) ) ;
#193201 = CARTESIAN_POINT ( 'NONE',  ( 3.515784362865181478, -0.5505564139345071606, 1.831456330389509501 ) ) ;
#193202 = CARTESIAN_POINT ( 'NONE',  ( 7.191674137406095291, 7.354984346587396082, 0.000000000000000000 ) ) ;
#193203 = CARTESIAN_POINT ( 'NONE',  ( 5.775410249297131315, 9.681803024247919609, 1.040834085586084257E-14 ) ) ;
#193204 = CARTESIAN_POINT ( 'NONE',  ( -9.321394304595349567, 10.83371376257142416, 1.199719254218462483 ) ) ;
#193205 = CARTESIAN_POINT ( 'NONE',  ( 1.968995789680173303, -1.553632997376572566, 1.280276984777522165 ) ) ;
#193206 = CARTESIAN_POINT ( 'NONE',  ( 2.307404798597446849, -1.572557994556064154, -1.172606125687980061 ) ) ;
#193207 = CARTESIAN_POINT ( 'NONE',  ( -9.459838494033043332, 12.05956421450382088, 1.599625672291281386 ) ) ;
#193208 = CARTESIAN_POINT ( 'NONE',  ( -5.038826645773246682, 9.030381520044109322, 0.7998128361456481317 ) ) ;
#193210 = ADVANCED_FACE ( 'NONE', ( #178956 ), #140936, .T. ) ;
#193209 = CARTESIAN_POINT ( 'NONE',  ( -1.364683531250000748, 8.421875000341403350, 0.000000000000000000 ) ) ;
#193212 = CARTESIAN_POINT ( 'NONE',  ( 3.801397759637317186, -0.5140543387622575899, 1.693523888807080047 ) ) ;
#193211 = CARTESIAN_POINT ( 'NONE',  ( 4.787105812777236125, 1.548788850919210702, 1.404477511574409920 ) ) ;
#193213 = CARTESIAN_POINT ( 'NONE',  ( 0.3554123170483391991, 14.00000000000058265, 12.67999999502907649 ) ) ;
#193215 = CARTESIAN_POINT ( 'NONE',  ( 5.929661055573363981, 1.134796830042347660, -1.991584109881129327 ) ) ;
#193214 = CARTESIAN_POINT ( 'NONE',  ( -2.788906526875773208E-15, 9.218750000682799595, -1.499999999999998446 ) ) ;
#193216 = CARTESIAN_POINT ( 'NONE',  ( 4.962738864268898098, 0.1657098081031352088, -1.732421123976911836 ) ) ;
#193217 = CARTESIAN_POINT ( 'NONE',  ( 9.752392566931574081, 10.27221283770866300, -0.7998128361456281477 ) ) ;
#193218 = AXIS2_PLACEMENT_3D ( 'NONE', #123, #103809, #99799 ) ;
#193219 = CARTESIAN_POINT ( 'NONE',  ( -1.333449616921166703, 8.249651149236390424, 11.01993490927447539 ) ) ;
#193220 = CARTESIAN_POINT ( 'NONE',  ( 4.569544190834089470, 1.339882265830975694, -1.100422448201631820 ) ) ;
#193221 = CARTESIAN_POINT ( 'NONE',  ( 5.107971825378077924, 0.6857059611327814830, -2.060108355502160649 ) ) ;
#193222 = CARTESIAN_POINT ( 'NONE',  ( 4.207107738942202246, 3.802713871720993399, 1.214306433183764966E-14 ) ) ;
#193223 = CARTESIAN_POINT ( 'NONE',  ( -0.2232446489705899595, -0.4745787333681207865, -2.071451665377940010 ) ) ;
#193224 = CARTESIAN_POINT ( 'NONE',  ( 4.656250000000003553, -1.895863743163975101, 0.7852924748302414493 ) ) ;
#193225 = CARTESIAN_POINT ( 'NONE',  ( 11.04536101718726293, 10.09418840193640499, -1.100000000000000311 ) ) ;
#193226 = CARTESIAN_POINT ( 'NONE',  ( 2.959893420002459585, 1.917249785004307316, -0.1873479421724104088 ) ) ;
#193227 = CARTESIAN_POINT ( 'NONE',  ( 1.499999999999997113, 10.92708333401613530, -0.8660254037844378194 ) ) ;
#193228 = CARTESIAN_POINT ( 'NONE',  ( 0.5752228765869402682, -1.604835199033414872, 1.536031695938171460 ) ) ;
#193229 = ORIENTED_EDGE ( 'NONE', *, *, #154961, .F. ) ;
#193230 = CARTESIAN_POINT ( 'NONE',  ( -0.1408020194050172424, 4.085453189724971956, -2.655103234342595986 ) ) ;
#193231 = CARTESIAN_POINT ( 'NONE',  ( -1.500000000000013101, 2.629166666666687746, -0.8660254037844313801 ) ) ;
#193232 = CARTESIAN_POINT ( 'NONE',  ( 5.341022448779654930, 8.318611059296550536, 1.199719254218462483 ) ) ;
#193233 = CARTESIAN_POINT ( 'NONE',  ( 2.948112417477159575, -1.493347798232132373, -1.644555409524293577 ) ) ;
#193234 = CARTESIAN_POINT ( 'NONE',  ( -0.02900071798685177615, 6.946858727649162901, -2.768864135414349281 ) ) ;
#193235 = CARTESIAN_POINT ( 'NONE',  ( 7.456621297836078632, 8.762108271306003004, 1.082531754730558626 ) ) ;
#193236 = CARTESIAN_POINT ( 'NONE',  ( 0.4019237886466816012, 10.20758545099816850, -1.499999999999998668 ) ) ;
#193237 = EDGE_CURVE ( 'NONE', #48080, #200114, #189488, .T. ) ;
#193238 = CARTESIAN_POINT ( 'NONE',  ( 7.512626515748109135, 8.897724035528543851, 1.082531754730549967 ) ) ;
#193239 = CARTESIAN_POINT ( 'NONE',  ( 1.002577532868035526, -1.966644254196001196, 0.4445047019146358691 ) ) ;
#193241 = CARTESIAN_POINT ( 'NONE',  ( 5.863753151201884783, -0.5045919461894343705, 1.999881752496771359 ) ) ;
#193240 = CARTESIAN_POINT ( 'NONE',  ( 7.391166297744269365, 11.77477778067701664, 1.040834085586084257E-14 ) ) ;
#193242 =( LENGTH_UNIT ( ) NAMED_UNIT ( * ) SI_UNIT ( .MILLI., .METRE. ) );
#193243 = CARTESIAN_POINT ( 'NONE',  ( -5.088387723830502196, 4.830873854090670605, -0.7998128361456221525 ) ) ;
#193244 = CARTESIAN_POINT ( 'NONE',  ( 1.499999999999989120, 5.035416667349487341, 0.8660254037844524744 ) ) ;
#193245 = CARTESIAN_POINT ( 'NONE',  ( 1.364683531249988757, 0.6343750003414208027, 0.000000000000000000 ) ) ;
#193246 = CARTESIAN_POINT ( 'NONE',  ( 0.4734442463095941411, 1.011852719971978232, 1.451749726636430093 ) ) ;
#193247 = CARTESIAN_POINT ( 'NONE',  ( 5.607993946907785521, -0.03366334548273764576, 1.734015701317252134 ) ) ;
#193248 = CARTESIAN_POINT ( 'NONE',  ( 5.495574104867783305, -1.740626723225440209, 0.008114992421901638317 ) ) ;
#193249 = CARTESIAN_POINT ( 'NONE',  ( 2.525266882823226311, -2.137704731703232053, 0.8281840208047249741 ) ) ;
#193250 = CARTESIAN_POINT ( 'NONE',  ( -1.364683531250014514, -0.2197916663252438285, 0.7879004041258379498 ) ) ;
#193251 = CARTESIAN_POINT ( 'NONE',  ( 2.079791654855645877, -1.805462111169679584, -0.3597937517794968509 ) ) ;
#193252 = CARTESIAN_POINT ( 'NONE',  ( 8.211434591371064684, 12.73175745657494851, -0.7998128361456352531 ) ) ;
#193253 = CARTESIAN_POINT ( 'NONE',  ( 2.221465439867484903, -1.771451409125622600, 0.4407646962370226351 ) ) ;
#193254 = CARTESIAN_POINT ( 'NONE',  ( 2.268204128460939550, 1.842446992372799963, -0.8197738674571022344 ) ) ;
#193255 = CARTESIAN_POINT ( 'NONE',  ( -4.134873662043608178, 4.886736029548026217, 1.082531754730558626 ) ) ;
#193256 = LINE ( 'NONE', #208422, #162633 ) ;
#193257 = CARTESIAN_POINT ( 'NONE',  ( 4.524511627872906061, 1.297711147994727865, -1.658517390945497549 ) ) ;
#193258 = CARTESIAN_POINT ( 'NONE',  ( -5.364222332501225488, 9.410009821226765325, 0.7998128361456481317 ) ) ;
#193259 = CARTESIAN_POINT ( 'NONE',  ( 7.922173639401519196, 13.65794249303706920, 8.699232811755850392 ) ) ;
#193260 = CARTESIAN_POINT ( 'NONE',  ( 2.137250951388528275, -0.09934309608320915363, -2.068088366144354318 ) ) ;
#193261 = CARTESIAN_POINT ( 'NONE',  ( 2.706824224222692088, 6.309712028235118453, 0.7998128361456362523 ) ) ;
#193262 = CARTESIAN_POINT ( 'NONE',  ( 1.360316468749971364, 0.04687500034143698979, -3.469446951953614189E-14 ) ) ;
#193263 = CARTESIAN_POINT ( 'NONE',  ( 5.233110275169113201, 1.959380141031796585, 0.8112103084707968925 ) ) ;
#193264 = ITEM_DEFINED_TRANSFORMATION ( 'NONE', 'NONE', #69589,  #200407 ) ;
#193265 = CARTESIAN_POINT ( 'NONE',  ( 0.02974079377688309753, -1.184178705181990532, -1.520296634558585547 ) ) ;
#193266 = VERTEX_POINT ( 'NONE', #3352 ) ;
#193267 = CARTESIAN_POINT ( 'NONE',  ( -4.142898457427624415, 6.991076079377632091, 1.199719254218452935 ) ) ;
#193268 = CARTESIAN_POINT ( 'NONE',  ( 7.899597058256738968, 12.36794700127490820, 1.040834085586084257E-14 ) ) ;
#193269 = CARTESIAN_POINT ( 'NONE',  ( 5.600926855776875435, 7.627776979863398310, -1.443375672974078761 ) ) ;
#193270 = CARTESIAN_POINT ( 'NONE',  ( 3.475000000000000533, -1.531249999044085541, 0.000000000000000000 ) ) ;
#193271 = AXIS2_PLACEMENT_3D ( 'NONE', #91302, #10017, #174687 ) ;
#193272 = CARTESIAN_POINT ( 'NONE',  ( -6.566226467720086113, 6.555019055295208119, 1.040834085586084257E-14 ) ) ;
#193273 = CARTESIAN_POINT ( 'NONE',  ( 6.117454236943913770, 1.763945953808215394, 1.176740244630887222 ) ) ;
#193274 = CARTESIAN_POINT ( 'NONE',  ( 1.571456177274520805, 0.1552745290232947217, -2.100303177343607608 ) ) ;
#193275 = CARTESIAN_POINT ( 'NONE',  ( -4.457598643843001973, 8.422558527783969851, 0.000000000000000000 ) ) ;
#193276 = CARTESIAN_POINT ( 'NONE',  ( 7.889955328148847258, 11.29236608522730911, -1.199719254218446718 ) ) ;
#193277 = CARTESIAN_POINT ( 'NONE',  ( 5.805462856137336480, -1.465901670865896067, -1.146230774367855254 ) ) ;
#193278 = CARTESIAN_POINT ( 'NONE',  ( 6.642605195691581699, 9.837124264027149678, 1.199719254218462483 ) ) ;
#193279 = PLANE ( 'NONE',  #140366 ) ;
#193280 = CARTESIAN_POINT ( 'NONE',  ( -6.563555762791521531, 9.711213252348503744, 1.082531754730549967 ) ) ;
#193281 = CARTESIAN_POINT ( 'NONE',  ( -8.161645285746702783, 12.46574390010577105, 0.7216878364870478180 ) ) ;
#193282 = CARTESIAN_POINT ( 'NONE',  ( -9.541824394042135893, 5.027248526908232762, 6.730710380108894775 ) ) ;
#193283 = SURFACE_STYLE_USAGE ( .BOTH. , #108906 ) ;
#193285 = CARTESIAN_POINT ( 'NONE',  ( 2.558977423257744022, 1.577441344615847951, -1.166261179026031325 ) ) ;
#193284 = CARTESIAN_POINT ( 'NONE',  ( -6.561256274009600986, 9.742217188731485678, -1.199719254218440723 ) ) ;
#193286 = CARTESIAN_POINT ( 'NONE',  ( 1.270647086845246188, -1.370953960119488668, 1.671340013135722558 ) ) ;
#193288 = CARTESIAN_POINT ( 'NONE',  ( -6.110283559904478246, 6.013173453705326743, 0.3066926896367061506 ) ) ;
#193287 = CARTESIAN_POINT ( 'NONE',  ( -6.296835998904160014, 6.311006518335105397, 0.000000000000000000 ) ) ;
#193289 = CARTESIAN_POINT ( 'NONE',  ( 1.364683531249988757, 1.134375000341421247, 0.000000000000000000 ) ) ;
#193290 = CARTESIAN_POINT ( 'NONE',  ( 3.004952549044386245, 1.720378813442688282, 0.2150250689552536121 ) ) ;
#193291 = CARTESIAN_POINT ( 'NONE',  ( 2.220290661370280638, -0.001068742171999540608, 1.740516466435287235 ) ) ;
#193292 =( GEOMETRIC_REPRESENTATION_CONTEXT ( 3 ) GLOBAL_UNCERTAINTY_ASSIGNED_CONTEXT ( ( #131765 ) ) GLOBAL_UNIT_ASSIGNED_CONTEXT ( ( #160410, #80220, #178806 ) ) REPRESENTATION_CONTEXT ( 'NONE', 'WORKASPACE' ) );
#193293 = CARTESIAN_POINT ( 'NONE',  ( 8.120970824905713314, 8.576813505252564696, 1.040834085586084257E-14 ) ) ;
#193294 = CARTESIAN_POINT ( 'NONE',  ( -11.69380381030441107, 8.410673437356566140, -1.083569014401829955 ) ) ;
#193295 = CARTESIAN_POINT ( 'NONE',  ( 2.108749758911751204, 0.7741990562295970602, -1.861730988020185329 ) ) ;
#193296 = CARTESIAN_POINT ( 'NONE',  ( 6.825078400183575589, -0.005632053428735600553, 2.144262460745151255 ) ) ;
#193297 = CARTESIAN_POINT ( 'NONE',  ( -3.959863383643135393, 6.777535159962392086, 1.199719254218452935 ) ) ;
#193298 = CARTESIAN_POINT ( 'NONE',  ( 0.9363264705049412218, 1.941902958617349961, 0.3393069938249710371 ) ) ;
#193300 = CARTESIAN_POINT ( 'NONE',  ( -4.665414256878287702, 8.457084043084382330, -0.7216878364870338292 ) ) ;
#193299 = CARTESIAN_POINT ( 'NONE',  ( 6.275647926998929371, 0.3200337115364471074, -1.885262484646982095 ) ) ;
#193301 = CARTESIAN_POINT ( 'NONE',  ( -6.766928066552171828, 7.067373297165212342, 0.7216878364870317197 ) ) ;
#193302 = CARTESIAN_POINT ( 'NONE',  ( 6.658989722967328717, 7.797851427330578566, 1.199719254218452935 ) ) ;
#193303 = CARTESIAN_POINT ( 'NONE',  ( -5.121948170912633991, 9.197632976031879792, -0.7998128361456362523 ) ) ;
#193304 = CARTESIAN_POINT ( 'NONE',  ( 1.541671952839033688, -1.900923180158103021, 0.6826752959473363358 ) ) ;
#193305 = DIRECTION ( 'NONE',  ( 1.000000000000000000, -0.000000000000000000, -0.000000000000000000 ) ) ;
#193306 = CARTESIAN_POINT ( 'NONE',  ( 4.735574959254028826, -2.111847384580630038, 0.9304801611131856554 ) ) ;
#193307 = CARTESIAN_POINT ( 'NONE',  ( 6.109812101310618360, 0.5708666350849945781, -1.876949146916474298 ) ) ;
#193308 = CARTESIAN_POINT ( 'NONE',  ( 2.834756127989654484, -1.875839772035441388, -0.5741054328185363209 ) ) ;
#193309 = CARTESIAN_POINT ( 'NONE',  ( 9.447334110624092673, 9.916311305349925220, -0.7998128361456281477 ) ) ;
#193310 = CARTESIAN_POINT ( 'NONE',  ( -9.586287156527431463, 14.76664842859987914, 7.218579095329854312 ) ) ;
#193311 = VERTEX_POINT ( 'NONE', #50001 ) ;
#193312 = CARTESIAN_POINT ( 'NONE',  ( 1.077539098219507663, 1.607448503539260054, 1.378281722515703800 ) ) ;
#193314 = CARTESIAN_POINT ( 'NONE',  ( -6.659026002606323047, 10.92061410301605662, 0.000000000000000000 ) ) ;
#193313 = CARTESIAN_POINT ( 'NONE',  ( -5.108724954250998707, 4.854600622914589714, -0.7998128361456221525 ) ) ;
#193315 = CARTESIAN_POINT ( 'NONE',  ( 1.798526679444776954, 1.530131497970032450, 1.023642133485637595 ) ) ;
#193316 = VERTEX_POINT ( 'NONE', #166960 ) ;
#193317 = CARTESIAN_POINT ( 'NONE',  ( 11.87989628165243161, 7.840779707844498958, 1.747908902009029708 ) ) ;
#193318 = CARTESIAN_POINT ( 'NONE',  ( 2.461320219219771843, -1.760565900816572826, 1.181798851529712646 ) ) ;
#193319 = CARTESIAN_POINT ( 'NONE',  ( 1.499999999999989120, 4.535416667349484676, 0.8660254037844524744 ) ) ;
#193320 = CARTESIAN_POINT ( 'NONE',  ( 7.914208982075123799, 10.25632978388623684, -1.599625672291262513 ) ) ;
#193321 = FACE_OUTER_BOUND ( 'NONE', #32954, .T. ) ;
#193322 = CARTESIAN_POINT ( 'NONE',  ( 3.110674321496671446, 1.495003355660160516, -1.418639704521322153 ) ) ;
#193324 = CARTESIAN_POINT ( 'NONE',  ( 0.7492455685023796663, 1.839184785914184994, -0.09005233288367914257 ) ) ;
#193323 = CARTESIAN_POINT ( 'NONE',  ( -6.855619230004478482, 11.14997286831390788, -0.7998128361456291469 ) ) ;
#193325 = CARTESIAN_POINT ( 'NONE',  ( -1.201851678989727383E-14, 2.696875000341417916, -1.575800808251660134 ) ) ;
#193326 = CARTESIAN_POINT ( 'NONE',  ( -0.02224634325196857623, 5.718740092702407907, -2.883150554214870098 ) ) ;
#193327 = CYLINDRICAL_SURFACE ( 'NONE', #35515, 0.07999999999999993228 ) ;
#193328 = CIRCLE ( 'NONE', #99947, 2.000000000000000000 ) ;
#193329 = CARTESIAN_POINT ( 'NONE',  ( -5.572037945092171540, 5.603058478803390585, 0.7216878364870346063 ) ) ;
#193330 = CARTESIAN_POINT ( 'NONE',  ( 2.952682139456219268, 0.7592856210697115360, 2.131335665991466843 ) ) ;
#193331 = CARTESIAN_POINT ( 'NONE',  ( -8.351459436338030784, 11.72682452816096976, -1.082531754730543971 ) ) ;
#193332 = CARTESIAN_POINT ( 'NONE',  ( 2.425776345151516633, -1.791340243523626974, 0.2692766639123735373 ) ) ;
#193333 = CARTESIAN_POINT ( 'NONE',  ( 2.870226655882984090, -1.888176233477338872, -0.3226071530259622677 ) ) ;
#193334 = CARTESIAN_POINT ( 'NONE',  ( 4.615722581382986967, 0.4567890626981512270, -2.019179087418949692 ) ) ;
#193335 = CARTESIAN_POINT ( 'NONE',  ( 0.6823417656249882723, 2.988541667008084879, -1.181850606188754593 ) ) ;
#193336 = EDGE_CURVE ( 'NONE', #121606, #112218, #117194, .T. ) ;
#193337 = CARTESIAN_POINT ( 'NONE',  ( 2.078924955456124657, -0.09500079177627264448, -1.969288250925634642 ) ) ;
#193338 = CARTESIAN_POINT ( 'NONE',  ( 6.287721633157377532, 1.330437191854600076, 1.393544807510539218 ) ) ;
#193339 = CARTESIAN_POINT ( 'NONE',  ( 3.098369316282158614, -0.5415621961667067552, -1.790553177708480215 ) ) ;
#193341 = CARTESIAN_POINT ( 'NONE',  ( 4.597299534708283453, 8.487268731053720927, 0.09294953129799360392 ) ) ;
#193340 = CARTESIAN_POINT ( 'NONE',  ( 2.385774557197326562, 2.109090111016972191, -0.9369807928535575092 ) ) ;
#193342 = CARTESIAN_POINT ( 'NONE',  ( 3.033498015644376267, 1.768043114356824930, -0.5812464218588138110 ) ) ;
#193343 = CARTESIAN_POINT ( 'NONE',  ( 1.364683531249990311, 2.634375000341422801, 1.214306433183764966E-14 ) ) ;
#193344 = CARTESIAN_POINT ( 'NONE',  ( 6.144999177589818729, -0.2990398410713848154, -2.040763669801145319 ) ) ;
#193345 = VECTOR ( 'NONE', #6970, 1000.000000000000227 ) ;
#193346 = CARTESIAN_POINT ( 'NONE',  ( -4.303823697334223652, 7.108545849276850959, -1.199719254218452047 ) ) ;
#193347 = CARTESIAN_POINT ( 'NONE',  ( 5.503720292143644777, 8.508425209887878538, 1.199719254218462483 ) ) ;
#193348 = CARTESIAN_POINT ( 'NONE',  ( -1.493068410184935635, 3.264629715075684668, -0.1642227666888320947 ) ) ;
#193349 = CARTESIAN_POINT ( 'NONE',  ( 6.053767517140953736, 0.6149031373867475114, -2.014179596626505919 ) ) ;
#193350 = CARTESIAN_POINT ( 'NONE',  ( -1.364683531250012516, 4.551041667008082214, -0.7879004041258300672 ) ) ;
#193351 = CARTESIAN_POINT ( 'NONE',  ( 5.782550318682353030, -2.107506929020441788, -0.4798289361013232668 ) ) ;
#193352 = CARTESIAN_POINT ( 'NONE',  ( 6.358070640981934751, 0.7709996861101749976, -1.866924874111668853 ) ) ;
#193353 = CARTESIAN_POINT ( 'NONE',  ( -1.402160292154681736E-14, -0.9281249996585830830, 1.575800808251672791 ) ) ;
#193354 = CARTESIAN_POINT ( 'NONE',  ( -4.039966587192274083, 5.736380323189513852, 1.443375672974064550 ) ) ;
#193355 = EDGE_CURVE ( 'NONE', #46648, #122534, #101638, .T. ) ;
#193358 = CARTESIAN_POINT ( 'NONE',  ( 3.687454593236936251, 7.245854758844324728, -0.7216878364870267237 ) ) ;
#193357 = CARTESIAN_POINT ( 'NONE',  ( 6.825078400183574701, 6.039200712630649726, 2.350557101739355392 ) ) ;
#193356 = CARTESIAN_POINT ( 'NONE',  ( 7.374709211190586089, 7.568525266002632534, 0.000000000000000000 ) ) ;
#193359 = CARTESIAN_POINT ( 'NONE',  ( -3.817502770699643388, 6.611447778194983194, 1.199719254218452935 ) ) ;
#193360 = CARTESIAN_POINT ( 'NONE',  ( 4.259000112335223243, -0.004834882008357410665, -2.016708403958865414 ) ) ;
#193361 = CARTESIAN_POINT ( 'NONE',  ( -7.121056995675673740, 9.330985799753529264, -1.599625672291263179 ) ) ;
#193363 = CARTESIAN_POINT ( 'NONE',  ( -6.089020385868856522, 9.157588645938716354, -1.082531754730549967 ) ) ;
#193362 = CARTESIAN_POINT ( 'NONE',  ( -8.188761592974033832, 12.49737959187099179, -0.7216878364870267237 ) ) ;
#193364 = CARTESIAN_POINT ( 'NONE',  ( -0.5000000000000213163, 3.299999999999983391, -0.4000000000000444311 ) ) ;
#193366 = CARTESIAN_POINT ( 'NONE',  ( 1.364683531249996529, 9.213541667008062319, 0.7879004041258403923 ) ) ;
#193365 = CARTESIAN_POINT ( 'NONE',  ( 6.280167721515548251, -1.160692707240444710, 1.823489969145650313 ) ) ;
#193367 = CARTESIAN_POINT ( 'NONE',  ( 0.000000000000000000, -2.079999999999998295, 0.000000000000000000 ) ) ;
#193368 = CARTESIAN_POINT ( 'NONE',  ( -11.32640490158465774, 6.353037010736665380, 3.968039318877488952 ) ) ;
#193370 = CARTESIAN_POINT ( 'NONE',  ( 0.2279634046833027561, 1.910523547013969869, 0.1400250592105151126 ) ) ;
#193369 = CARTESIAN_POINT ( 'NONE',  ( -6.141480396866151992, 9.148515648777049591, 1.082531754730548412 ) ) ;
#193371 = CARTESIAN_POINT ( 'NONE',  ( -0.6823417656250003738, -0.7197916663252492686, -1.181850606188749264 ) ) ;
#193372 = CARTESIAN_POINT ( 'NONE',  ( 1.772826578343088544, 3.950000000000001954, -0.4500000000000284883 ) ) ;
#193373 = CARTESIAN_POINT ( 'NONE',  ( 2.121340078736310364, -1.673401575455361723, 0.4176718278932553541 ) ) ;
#193374 = CARTESIAN_POINT ( 'NONE',  ( 7.452141709366786770, 8.723195411463290583, 1.199719254218452047 ) ) ;
#193375 = CARTESIAN_POINT ( 'NONE',  ( 5.855142236255289845, 7.924361590421551860, -1.599625672291281386 ) ) ;
#193376 = AXIS2_PLACEMENT_3D ( 'NONE', #202295, #120085, #186060 ) ;
#193377 = CARTESIAN_POINT ( 'NONE',  ( -11.77314774087514238, 8.651273335165431178, 2.095004279193475760 ) ) ;
#193378 = CARTESIAN_POINT ( 'NONE',  ( 1.334804486018669856, -1.602990312956679597, 0.7502176981645010123 ) ) ;
#193379 = CARTESIAN_POINT ( 'NONE',  ( 2.402991782874515092, -0.3463731968284866625, -1.982927098142922784 ) ) ;
#193380 = DIRECTION ( 'NONE',  ( 0.000000000000000000, 0.000000000000000000, -1.000000000000000000 ) ) ;
#193381 = CARTESIAN_POINT ( 'NONE',  ( 4.032405518703926717, 1.182977813604596973, -1.862726815517960821 ) ) ;
#193382 = CARTESIAN_POINT ( 'NONE',  ( 5.541899213757757181, 1.452536422000339611, 1.613792965789240696 ) ) ;
#193383 = ORIENTED_EDGE ( 'NONE', *, *, #84110, .F. ) ;
#193384 = CARTESIAN_POINT ( 'NONE',  ( -1.402160292154681736E-14, -1.037499999999977662, 1.732050807568877637 ) ) ;
#193385 = CARTESIAN_POINT ( 'NONE',  ( 7.063434842595398777, 11.18449838309590483, -0.7216878364870267237 ) ) ;
#193387 = CARTESIAN_POINT ( 'NONE',  ( 2.900017720922347220, -0.9963201819552582883, -1.753021271517739343 ) ) ;
#193386 = CARTESIAN_POINT ( 'NONE',  ( 3.000754678503589012, -2.089479603458433754, -0.3603616953608209661 ) ) ;
#193389 = VERTEX_POINT ( 'NONE', #52135 ) ;
#193388 = CARTESIAN_POINT ( 'NONE',  ( 2.900440330899815233, -1.785477387793675597, -0.3053432404436141057 ) ) ;
#193390 = CARTESIAN_POINT ( 'NONE',  ( 5.040599249230596435, 9.102725900736217568, 0.7998128361456341429 ) ) ;
#193391 = VERTEX_POINT ( 'NONE', #68354 ) ;
#193392 = DIRECTION ( 'NONE',  ( -5.551115123125764829E-17, 0.000000000000000000, 1.000000000000000000 ) ) ;
#193393 = AXIS2_PLACEMENT_3D ( 'NONE', #6035, #207459, #41795 ) ;
#193394 = CARTESIAN_POINT ( 'NONE',  ( 4.527533231959700366, 7.369540306339926516, 1.199719254218462483 ) ) ;
#193395 = CARTESIAN_POINT ( 'NONE',  ( 6.463509179248937642, 0.3066564278407272748, -1.799597105106438777 ) ) ;
#193397 = CARTESIAN_POINT ( 'NONE',  ( 1.920960065284383678, -1.709437138374754639, 0.8649676252809009869 ) ) ;
#193396 = CARTESIAN_POINT ( 'NONE',  ( -3.795392936821753604, 6.515376628678959392, -1.199719254218452047 ) ) ;
#193398 = CARTESIAN_POINT ( 'NONE',  ( -2.632325991586425218, 0.3920720250259056017, -0.1636427795756393855 ) ) ;
#193399 = CARTESIAN_POINT ( 'NONE',  ( -4.848826244296223109, 5.027555131033083491, -0.8732430475888955934 ) ) ;
#193400 =( BOUNDED_CURVE ( )  B_SPLINE_CURVE ( 2, ( #114113, #29592, #212584, #98859, #148673, #177977, #163864, #82586, #241 ),
 .UNSPECIFIED., .F., .T. ) 
 B_SPLINE_CURVE_WITH_KNOTS ( ( 3, 2, 2, 2, 3 ),
 ( 0.4910714285714285476, 0.4940476190476190688, 0.5000000000000000000, 0.5059523809523809312, 0.5089285714285713969 ),
 .UNSPECIFIED. ) 
 CURVE ( )  GEOMETRIC_REPRESENTATION_ITEM ( )  RATIONAL_B_SPLINE_CURVE ( ( 0.9330127018922194093, 0.9330127018922187432, 1.000000000000000000, 0.8660254037844387076, 1.000000000000000000, 0.8660254037844387076, 1.000000000000000000, 0.9330127018922194093, 0.9330127018922194093 ) ) 
 REPRESENTATION_ITEM ( '' )  );
#193401 = CARTESIAN_POINT ( 'NONE',  ( 1.364683531249988535, 2.176041667008087543, 0.7879004041258500513 ) ) ;
#193402 = CARTESIAN_POINT ( 'NONE',  ( -2.862179826260718762, 6.353310540697199471, 0.000000000000000000 ) ) ;
#193403 = CARTESIAN_POINT ( 'NONE',  ( -7.971304249830880373, 11.38727316052296601, 1.199719254218453823 ) ) ;
#193404 = CARTESIAN_POINT ( 'NONE',  ( 5.541917325712655717, 0.8799508658935292216, -1.974686638939105343 ) ) ;
#193405 = CARTESIAN_POINT ( 'NONE',  ( -5.655159470675923394, 5.770309935309573923, 0.000000000000000000 ) ) ;
#193406 = CARTESIAN_POINT ( 'NONE',  ( -5.887983850084758330, 10.09134126839936840, 0.7998128361456291469 ) ) ;
#193407 = CARTESIAN_POINT ( 'NONE',  ( 3.076547362214879566, 0.9570632234598417387, 1.892448740577145738 ) ) ;
#193409 = CARTESIAN_POINT ( 'NONE',  ( -11.87988507903381219, 5.100570458969788668, 4.764376171217361566 ) ) ;
#193408 = CARTESIAN_POINT ( 'NONE',  ( -0.1298852118744256712, 1.416581902219627542, -1.986715197202136185 ) ) ;
#193410 = CARTESIAN_POINT ( 'NONE',  ( 4.710209360279286273, -0.8403073340159574744, -1.783404427212876842 ) ) ;
#193411 =( BOUNDED_CURVE ( )  B_SPLINE_CURVE ( 3, ( #37400, #149024, #119787, #87223 ),
 .UNSPECIFIED., .F., .T. ) 
 B_SPLINE_CURVE_WITH_KNOTS ( ( 4, 4 ),
 ( 4.712388980384718984, 5.718907872238413681 ),
 .UNSPECIFIED. ) 
 CURVE ( )  GEOMETRIC_REPRESENTATION_ITEM ( )  RATIONAL_B_SPLINE_CURVE ( ( 1.000000000000000000, 0.9173434942194829134, 0.9173434942194829134, 1.000000000000000000 ) ) 
 REPRESENTATION_ITEM ( '' )  );
#193412 = CARTESIAN_POINT ( 'NONE',  ( 0.1408853756387764278, 1.927792606564913136, 0.5802787064154624197 ) ) ;
#193413 = VERTEX_POINT ( 'NONE', #85691 ) ;
#193414 = CARTESIAN_POINT ( 'NONE',  ( 5.436746213213202061, -1.667492067756784158, 1.304688015722222039 ) ) ;
#193415 = CARTESIAN_POINT ( 'NONE',  ( 5.736508391913541338, 6.825586224388162648, -1.082531754730548412 ) ) ;
#193416 = CARTESIAN_POINT ( 'NONE',  ( 0.7661813929631040576, -2.060537521029872643, 0.2012509062776293156 ) ) ;
#193417 = CARTESIAN_POINT ( 'NONE',  ( 3.152217820003437421, -1.470166820979129207, 1.268861441860974049 ) ) ;
#193418 = EDGE_LOOP ( 'NONE', ( #37912, #499, #75816, #4909 ) ) ;
#193419 = CARTESIAN_POINT ( 'NONE',  ( -4.403059289062232651, 7.148295125103961034, -1.075145975261635911 ) ) ;
#193420 = CARTESIAN_POINT ( 'NONE',  ( 6.496291879603339758, 7.608037276739255006, 1.199719254218452935 ) ) ;
#193422 = CARTESIAN_POINT ( 'NONE',  ( 4.794779880727245036, 8.745660294157122649, -0.7998128361456281477 ) ) ;
#193421 = CARTESIAN_POINT ( 'NONE',  ( 3.503930302474305591, -0.8474990640115993568, -1.911341529346534118 ) ) ;
#193423 = CARTESIAN_POINT ( 'NONE',  ( 4.895902867866261055, 4.884510565364971413, -0.7216878364870458196 ) ) ;
#193425 = VERTEX_POINT ( 'NONE', #53198 ) ;
#193424 = CARTESIAN_POINT ( 'NONE',  ( 0.04710954650594124937, -1.657193159602200927, 0.7319819781744562048 ) ) ;
#193426 = CARTESIAN_POINT ( 'NONE',  ( 5.004599478379411437, -0.7411955310945413933, -2.078817424605138964 ) ) ;
#193427 = CARTESIAN_POINT ( 'NONE',  ( 3.092648394857516525, 6.449253795920727228, -0.4031905389056261724 ) ) ;
#193428 = CARTESIAN_POINT ( 'NONE',  ( 2.960231987352707428, 2.196266598062237563, -0.2149427413448631863 ) ) ;
#193429 = CARTESIAN_POINT ( 'NONE',  ( 8.259941899223605333, 10.65968485389279508, -1.599625672291268286 ) ) ;
#193431 =( BOUNDED_CURVE ( )  B_SPLINE_CURVE ( 2, ( #181024, #116080, #129178, #164778, #104, #148537, #117154 ),
 .UNSPECIFIED., .F., .T. ) 
 B_SPLINE_CURVE_WITH_KNOTS ( ( 3, 2, 2, 3 ),
 ( 0.08928571428571412116, 0.09523809523809514954, 0.1011904761904762057, 0.1071428571428572341 ),
 .UNSPECIFIED. ) 
 CURVE ( )  GEOMETRIC_REPRESENTATION_ITEM ( )  RATIONAL_B_SPLINE_CURVE ( ( 1.000000000000003775, 0.8660254037844349329, 1.000000000000000000, 0.8660254037844387076, 1.000000000000000000, 0.8660254037844364872, 1.000000000000002220 ) ) 
 REPRESENTATION_ITEM ( '' )  );
#193430 = FACE_OUTER_BOUND ( 'NONE', #172272, .T. ) ;
#193432 = CARTESIAN_POINT ( 'NONE',  ( 1.752457306817490457, 1.891635876823925200, 0.2793096714826873161 ) ) ;
#193433 = CARTESIAN_POINT ( 'NONE',  ( 9.073431116043567002, 11.60875560684942265, -1.599625672291262513 ) ) ;
#193434 = CARTESIAN_POINT ( 'NONE',  ( 5.178213324540339002, -1.104578422852561914, -1.750899486206449973 ) ) ;
#193436 = CARTESIAN_POINT ( 'NONE',  ( 2.940462584922590938, 2.145230175562794717, 0.2658940370997217584 ) ) ;
#193435 = CARTESIAN_POINT ( 'NONE',  ( -4.464712657601869417, 4.103252943490596216, 0.7998128361456341429 ) ) ;
#193437 = CARTESIAN_POINT ( 'NONE',  ( 4.968408144156593487, -2.063508908063705238, -0.7385586828293493333 ) ) ;
#193438 = EDGE_LOOP ( 'NONE', ( #57294, #155087, #132907, #155019, #206577 ) ) ;
#193439 = CARTESIAN_POINT ( 'NONE',  ( 9.049177462117294013, 12.64479190819049670, -1.199719254218446718 ) ) ;
#193440 = CARTESIAN_POINT ( 'NONE',  ( 4.132297641190314508, 7.622816840561035256, -0.7610026044957002300 ) ) ;
#193441 = CARTESIAN_POINT ( 'NONE',  ( -0.2734184563536292134, 7.240553437303447026, 1.983365796752670773 ) ) ;
#193442 = MECHANICAL_DESIGN_GEOMETRIC_PRESENTATION_REPRESENTATION (  '', ( #68940 ), #93120 ) ;
#193443 = CARTESIAN_POINT ( 'NONE',  ( 5.845500506147374153, 6.848780674373954547, 1.199719254218453823 ) ) ;
#193444 = CARTESIAN_POINT ( 'NONE',  ( 3.285556943749998737, -3.142708332855375986, -1.896917185911906722 ) ) ;
#193445 = CARTESIAN_POINT ( 'NONE',  ( 6.827182134110199918, 7.629137130509069387, 2.789055895399249252 ) ) ;
#193446 = CARTESIAN_POINT ( 'NONE',  ( 0.5103889644224939293, -1.913802852362625151, 0.6352017490645140985 ) ) ;
#193447 = CARTESIAN_POINT ( 'NONE',  ( -7.537970219518066450, 11.73812298950569044, -0.7216878364870267237 ) ) ;
#193448 = CARTESIAN_POINT ( 'NONE',  ( 6.008198349511364000, 7.038594824965278995, 1.199719254218453823 ) ) ;
#193449 = CARTESIAN_POINT ( 'NONE',  ( 4.961816271168416392, -0.5573412460852051886, 1.993729458732765858 ) ) ;
#193450 = CARTESIAN_POINT ( 'NONE',  ( 2.982943389344643759, -0.1423259158175680661, -1.921303036959535415 ) ) ;
#193451 = CARTESIAN_POINT ( 'NONE',  ( 0.3336115229473045618, 0.6298545048411038350, -1.915608025624820909 ) ) ;
#193452 = CARTESIAN_POINT ( 'NONE',  ( -9.622536337397040285, 12.24937836509514710, 1.599625672291281386 ) ) ;
#193453 = CARTESIAN_POINT ( 'NONE',  ( 5.148345644887269756, 7.029489223833707001, -1.599625672291256295 ) ) ;
#193454 = CARTESIAN_POINT ( 'NONE',  ( -1.001543065824772872E-14, 5.321875000341422357, 1.575800808251672791 ) ) ;
#193455 = CARTESIAN_POINT ( 'NONE',  ( 4.399236341264299632, -1.715665262265529734, 0.9668539646570695201 ) ) ;
#193456 = CARTESIAN_POINT ( 'NONE',  ( 0.5510472016944796270, -1.853416330350022179, -1.169031858332982177 ) ) ;
#193457 = CARTESIAN_POINT ( 'NONE',  ( 3.703562413045482060, -0.5285312144065814621, 1.747510042522756990 ) ) ;
#193458 = CARTESIAN_POINT ( 'NONE',  ( 6.861835142292135536, 9.098836647464588978, 1.443375672974065660 ) ) ;
#193459 = CARTESIAN_POINT ( 'NONE',  ( 3.890826896997583884, 4.602014803661035103, -1.082531754730543083 ) ) ;
#193460 = CARTESIAN_POINT ( 'NONE',  ( -5.108390017298964914, 9.181815130149269422, 0.000000000000000000 ) ) ;
#193461 = CARTESIAN_POINT ( 'NONE',  ( 4.366607992053101128, 7.252070536440704096, -1.199719254218448494 ) ) ;
#193462 = VERTEX_POINT ( 'NONE', #152835 ) ;
#193464 = CARTESIAN_POINT ( 'NONE',  ( 4.605731108040309607, 1.494732351555028371, 1.348829144277723824 ) ) ;
#193463 = CARTESIAN_POINT ( 'NONE',  ( 1.786409390178132162, 1.601450680722369846, -0.9084932335857234253 ) ) ;
#193465 = CARTESIAN_POINT ( 'NONE',  ( 0.8612291682562907003, -0.8250023432496387255, 2.145356560901264142 ) ) ;
#193466 = CARTESIAN_POINT ( 'NONE',  ( 5.032062496497622384, 1.126290172248314292, 1.606047186625796819 ) ) ;
#193467 = CARTESIAN_POINT ( 'NONE',  ( -5.343885102080728977, 9.386283052402845328, 0.7998128361456481317 ) ) ;
#193468 = DIRECTION ( 'NONE',  ( -0.9885327375000381167, 0.000000000000000000, -0.1510067114093955609 ) ) ;
#193469 = CARTESIAN_POINT ( 'NONE',  ( -2.950870989268691957, 6.594433254122103349, -0.7998128361456281477 ) ) ;
#193470 = EDGE_CURVE ( 'NONE', #179011, #1071, #67774, .T. ) ;
#193471 = CARTESIAN_POINT ( 'NONE',  ( -5.496904935697871863, 5.377753611261092637, 0.7998128361456281477 ) ) ;
#193474 = CARTESIAN_POINT ( 'NONE',  ( 0.3560485870845608858, 0.7116971694140910021, 1.730184004908103867 ) ) ;
#193473 = B_SPLINE_CURVE_WITH_KNOTS ( 'NONE', 3,
 ( #121799, #53511, #86014, #201865, #120728, #7946, #105492, #171524, #6867, #5790 ),
 .UNSPECIFIED., .F., .F.,
 ( 4, 3, 3, 4 ),
 ( 1.311158639597268106E-16, 6.251569610500030906E-05, 0.0001250312426172235419, 0.0002200345428698334245 ),
 .UNSPECIFIED. ) ;
#193472 = CARTESIAN_POINT ( 'NONE',  ( 1.962552558803489555, -1.912825090402545225, -0.8444004386199343015 ) ) ;
#193475 = CARTESIAN_POINT ( 'NONE',  ( -0.1104750535120234134, 0.7027814200676918421, -2.185477693842474256 ) ) ;
#193476 = CARTESIAN_POINT ( 'NONE',  ( 1.821426705348125230, 1.001848811563336605, -1.422965107008233643 ) ) ;
#193477 = CARTESIAN_POINT ( 'NONE',  ( 4.611744806942754238, 8.532119374741881757, -0.7998128361456231517 ) ) ;
#193479 = CARTESIAN_POINT ( 'NONE',  ( 3.646780131951566251, 7.198401220678091406, -0.7216878364870155105 ) ) ;
#193478 = CARTESIAN_POINT ( 'NONE',  ( 0.008622056077349157799, 14.55305231409391808, 11.95585894185517084 ) ) ;
#193480 = CARTESIAN_POINT ( 'NONE',  ( 2.138867256381206783, -1.541494696628985528, 0.7741069473117598854 ) ) ;
#193481 = CARTESIAN_POINT ( 'NONE',  ( 1.575987392057216940, -1.168677030305173004, 1.853764812240476623 ) ) ;
#193482 = CARTESIAN_POINT ( 'NONE',  ( 4.406973378220558679, 1.706932345810768359, -1.398813476408675260 ) ) ;
#193483 = DIRECTION ( 'NONE',  ( 1.224646797963766027E-16, -4.396526966619892032E-05, 0.9999999990335275424 ) ) ;
#193484 =( BOUNDED_SURFACE ( )  B_SPLINE_SURFACE ( 3, 2, ( 
 ( #163302, #164364, #82032 ),
 ( #63663, #214126, #197910 ),
 ( #49538, #144952, #115664 ),
 ( #181658, #33284, #165421 ),
 ( #195799, #193655, #14883 ),
 ( #46360, #17017, #62585 ),
 ( #111417, #210958, #128747 ),
 ( #129817, #169690, #116729 ),
 ( #68963, #1828, #151323 ),
 ( #19161, #150260, #53818 ),
 ( #52737, #152380, #749 ),
 ( #3959, #183803, #185923 ),
 ( #87384, #119948, #70027 ),
 ( #136142, #67887, #37558 ),
 ( #137217, #182729, #100421 ),
 ( #85235, #201096, #167561 ),
 ( #103638, #202160, #21278 ),
 ( #135083, #54882, #5025 ),
 ( #153452, #166492, #168621 ),
 ( #118871, #88461, #121036 ),
 ( #50604, #102561, #184857 ),
 ( #71099, #51691, #187003 ),
 ( #203238, #84171, #38634 ),
 ( #104711, #36484, #170760 ),
 ( #22349, #117813, #2891 ),
 ( #66815, #132958, #86309 ),
 ( #198961, #134032, #101491 ),
 ( #35413, #34348, #18083 ),
 ( #200039, #20223, #75403 ),
 ( #89536, #191260, #55950 ),
 ( #122103, #39697, #139350 ),
 ( #23425, #188067, #205380 ) ),
 .UNSPECIFIED., .F., .F., .F. ) 
 B_SPLINE_SURFACE_WITH_KNOTS ( ( 4, 2, 2, 2, 2, 2, 2, 2, 2, 2, 2, 2, 2, 2, 2, 4 ),
 ( 3, 3 ),
 ( 0.000000000000000000, 0.001493720594899021785, 0.002987441189798043569, 0.005974882379596087138, 0.007468602974495109140, 0.008962323569394130274, 0.009709183866843641708, 0.01045604416429315314, 0.01194976475919217428, 0.01344348535409119541, 0.01493720594899021828, 0.01643092654388923768, 0.01792464713878826055, 0.02091208832858630629, 0.02240580892348532915, 0.02389952951838434855 ),
 ( 0.000000000000000000, 1.000000000000000000 ),
 .UNSPECIFIED. ) 
 GEOMETRIC_REPRESENTATION_ITEM ( )  RATIONAL_B_SPLINE_SURFACE ( (
 ( 1.000000000000000000, 0.8434733505592640901, 1.000000000000000000),
 ( 1.000000000000000000, 0.8431702246155254876, 1.000000000000000000),
 ( 1.000000000000000000, 0.8426367324223418276, 1.000000000000000000),
 ( 1.000000000000000000, 0.8408650922403015926, 1.000000000000000000),
 ( 1.000000000000000000, 0.8396428711856337435, 1.000000000000000000),
 ( 1.000000000000000000, 0.8353280728740983818, 1.000000000000000000),
 ( 1.000000000000000000, 0.8320647679512711559, 1.000000000000000000),
 ( 1.000000000000000000, 0.8235806410807833267, 1.000000000000000000),
 ( 1.000000000000000000, 0.8255774334008273430, 1.000000000000000000),
 ( 1.000000000000000000, 0.8281857448045425452, 1.000000000000000000),
 ( 1.000000000000000000, 0.8295473863155264915, 1.000000000000000000),
 ( 1.000000000000000000, 0.8309453578789692818, 1.000000000000000000),
 ( 1.000000000000000000, 0.8312210268024100568, 1.000000000000000000),
 ( 1.000000000000000000, 0.8317131830652759739, 1.000000000000000000),
 ( 1.000000000000000000, 0.8319338935246425315, 1.000000000000000000),
 ( 1.000000000000000000, 0.8326804068065388753, 1.000000000000000000),
 ( 1.000000000000000000, 0.8334031718083524387, 1.000000000000000000),
 ( 1.000000000000000000, 0.8334179402980076423, 1.000000000000000000),
 ( 1.000000000000000000, 0.8328045324390893622, 1.000000000000000000),
 ( 1.000000000000000000, 0.8317996902536097803, 1.000000000000000000),
 ( 1.000000000000000000, 0.8314091991306797880, 1.000000000000000000),
 ( 1.000000000000000000, 0.8295445083194166180, 1.000000000000000000),
 ( 1.000000000000000000, 0.8285669895138008112, 1.000000000000000000),
 ( 1.000000000000000000, 0.8259632866995387790, 1.000000000000000000),
 ( 1.000000000000000000, 0.8235472590115482383, 1.000000000000000000),
 ( 1.000000000000000000, 0.8321649622163090898, 1.000000000000000000),
 ( 1.000000000000000000, 0.8357012932624516832, 1.000000000000000000),
 ( 1.000000000000000000, 0.8399852490580022035, 1.000000000000000000),
 ( 1.000000000000000000, 0.8411359117240285732, 1.000000000000000000),
 ( 1.000000000000000000, 0.8427639893650330505, 1.000000000000000000),
 ( 1.000000000000000000, 0.8432301679486819967, 1.000000000000000000),
 ( 1.000000000000000000, 0.8435419936913640671, 1.000000000000000000) ) ) 
 REPRESENTATION_ITEM ( '' )  SURFACE ( )  );
#193485 =( GEOMETRIC_REPRESENTATION_CONTEXT ( 3 ) GLOBAL_UNCERTAINTY_ASSIGNED_CONTEXT ( ( #191391 ) ) GLOBAL_UNIT_ASSIGNED_CONTEXT ( ( #163404, #145050, #203331 ) ) REPRESENTATION_CONTEXT ( 'NONE', 'WORKASPACE' ) );
#193486 = CARTESIAN_POINT ( 'NONE',  ( 2.518641040286667465, 0.9249485440519630286, 1.964284900515224530 ) ) ;
#193487 = CARTESIAN_POINT ( 'NONE',  ( 1.049113529465800054, -1.437755431736492673, -1.125068434497819680 ) ) ;
#193488 = CARTESIAN_POINT ( 'NONE',  ( 3.186815374238487930, 1.666415522689016049, -1.306070977860743110 ) ) ;
#193489 = CARTESIAN_POINT ( 'NONE',  ( 6.539320575229287336, 0.6031692783194403384, 1.851139666870088130 ) ) ;
#193490 = VERTEX_POINT ( 'NONE', #153907 ) ;
#193492 = CARTESIAN_POINT ( 'NONE',  ( -0.6823417656250246877, 0.1135416670080893753, 1.181850606188755259 ) ) ;
#193491 = CARTESIAN_POINT ( 'NONE',  ( 3.667766089696015364, 1.274287168460963127, 1.905377313346041435 ) ) ;
#193493 = CARTESIAN_POINT ( 'NONE',  ( 3.358669367883368118, 4.941533567329135401, -1.599625672291262513 ) ) ;
#193494 = CARTESIAN_POINT ( 'NONE',  ( 4.566398809704347528, 4.221886787610169556, -0.7998128361456211532 ) ) ;
#193495 = CARTESIAN_POINT ( 'NONE',  ( 6.182328207180960433, 1.139467527619671294, 1.906663674214443382 ) ) ;
#193496 = CARTESIAN_POINT ( 'NONE',  ( -5.910991785878165317, 8.879612269291090598, -1.082531754730538864 ) ) ;
#193497 = CARTESIAN_POINT ( 'NONE',  ( 5.341549334104200852, 5.334155099317434257, 0.7216878364870317197 ) ) ;
#193498 = CARTESIAN_POINT ( 'NONE',  ( -6.344852701071109102, 10.34615255131755163, 0.000000000000000000 ) ) ;
#193499 = EDGE_CURVE ( 'NONE', #25291, #94694, #20674, .T. ) ;
#193500 = CARTESIAN_POINT ( 'NONE',  ( 5.289089323106923146, 6.303597310780433283, -1.082531754730548412 ) ) ;
#193501 = ORIENTED_EDGE ( 'NONE', *, *, #130401, .T. ) ;
#193502 = CARTESIAN_POINT ( 'NONE',  ( 3.709611425391425854, 1.915599900965975433, 0.6298755557959597740 ) ) ;
#193504 = CARTESIAN_POINT ( 'NONE',  ( 2.342701370759682433, -2.021932799725610241, -0.4066214432158538616 ) ) ;
#193503 = CARTESIAN_POINT ( 'NONE',  ( 6.148786358997489820, 7.132337826040578754, -1.199719254218446718 ) ) ;
#193505 = FACE_OUTER_BOUND ( 'NONE', #194223, .T. ) ;
#193506 = CARTESIAN_POINT ( 'NONE',  ( 4.868786560638889149, 6.773613302202437403, 1.443375672974065660 ) ) ;
#193507 = CARTESIAN_POINT ( 'NONE',  ( -3.285556943750000514, -2.238541666188709200, -1.896917185911906500 ) ) ;
#193508 = CARTESIAN_POINT ( 'NONE',  ( 1.364683531249990311, 5.363541667008086655, 0.7879004041258500513 ) ) ;
#193509 = CARTESIAN_POINT ( 'NONE',  ( 5.226606370275341362, 0.1587857941063846590, 2.185760735149797185 ) ) ;
#193510 = CARTESIAN_POINT ( 'NONE',  ( 2.320935597664942396, 0.9480396085976348086, -1.779626998253575509 ) ) ;
#193511 = CARTESIAN_POINT ( 'NONE',  ( 2.471991059931688106, -1.762569054296094340, -0.5325411743367302053 ) ) ;
#193512 = CARTESIAN_POINT ( 'NONE',  ( 5.635385404774530649, 9.726366738878972740, 0.7998128361456462443 ) ) ;
#193513 = CARTESIAN_POINT ( 'NONE',  ( 6.792070425361753649, -0.7769146798779454910, 1.650438213995283565 ) ) ;
#193514 = CARTESIAN_POINT ( 'NONE',  ( -0.1394461523061351904, -0.009327122704730000241, -2.280146446826665230 ) ) ;
#193515 = CARTESIAN_POINT ( 'NONE',  ( -7.232384877886063990, 10.52520055992070525, -1.199719254218446718 ) ) ;
#193517 = CARTESIAN_POINT ( 'NONE',  ( -4.847922445338252118, 7.813604065273374921, -1.199719254218453823 ) ) ;
#193516 = CARTESIAN_POINT ( 'NONE',  ( 5.366221907327076046, 1.110187712879026956, 1.971344288924305799 ) ) ;
#193518 = CARTESIAN_POINT ( 'NONE',  ( 0.2761803097106649840, 1.214566955493846967, 1.720366990225271842 ) ) ;
#193519 = CARTESIAN_POINT ( 'NONE',  ( -7.045397100956844127, 8.248660034984974132, -1.199719254218452047 ) ) ;
#193520 = CARTESIAN_POINT ( 'NONE',  ( 7.751511138711133064, 10.06651563329490529, -1.599625672291262513 ) ) ;
#193521 = CARTESIAN_POINT ( 'NONE',  ( 5.506019780481205217, 9.437790487287811558, 0.000000000000000000 ) ) ;
#193522 = CARTESIAN_POINT ( 'NONE',  ( 8.378074386686998665, 17.40827580138378394, 11.64151304414228960 ) ) ;
#193523 = CARTESIAN_POINT ( 'NONE',  ( -7.527801604085656351, 9.805521176231838609, 1.599625672291295375 ) ) ;
#193524 = CARTESIAN_POINT ( 'NONE',  ( 2.989990986282343055, 6.640073250638046432, -0.4916062289654400397 ) ) ;
#193525 = CARTESIAN_POINT ( 'NONE',  ( 7.199016378732056687, 10.38230762762066384, -1.082531754730537976 ) ) ;
#193526 = CARTESIAN_POINT ( 'NONE',  ( 4.014041799177766379, 7.808471211821870206, -0.2759448393452879067 ) ) ;
#193527 = CARTESIAN_POINT ( 'NONE',  ( -9.653042183249972652, 10.36423008998754192, -0.7216878364870267237 ) ) ;
#193528 = CARTESIAN_POINT ( 'NONE',  ( 3.340272282456987263, -1.325889367010645969, -1.782164031402436954 ) ) ;
#193529 = CARTESIAN_POINT ( 'NONE',  ( -0.4000000000000447087, 3.964661556059721814, 0.9099571394228918031 ) ) ;
#193531 = AXIS2_PLACEMENT_3D ( 'NONE', #201007, #150173, #117726 ) ;
#193530 = CARTESIAN_POINT ( 'NONE',  ( -5.152980901645737077, 8.169505597632108262, -1.199719254218453823 ) ) ;
#193532 = CARTESIAN_POINT ( 'NONE',  ( 5.178324605415663306, 8.128796908705222535, 1.199719254218462483 ) ) ;
#193533 = CARTESIAN_POINT ( 'NONE',  ( 3.930091730393743710, 1.087902980620155891, 1.632394305395828304 ) ) ;
#193534 = CARTESIAN_POINT ( 'NONE',  ( 8.041957671200231417, 12.53403438304231976, 1.040834085586084257E-14 ) ) ;
#193535 = CARTESIAN_POINT ( 'NONE',  ( -5.296940370067747317, 6.395615756200102808, 1.134431874056667233 ) ) ;
#193536 = CARTESIAN_POINT ( 'NONE',  ( 4.546061579283848353, 4.198160018786257552, -0.7998128361456211532 ) ) ;
#193537 = CARTESIAN_POINT ( 'NONE',  ( -5.207740401424942434, 6.208690235484773723, 1.082531754730549078 ) ) ;
#193539 = ORIENTED_EDGE ( 'NONE', *, *, #164125, .T. ) ;
#193538 = CARTESIAN_POINT ( 'NONE',  ( -8.026063749610063525, 8.466088584074293877, -0.7216878364870278340 ) ) ;
#193540 = CARTESIAN_POINT ( 'NONE',  ( 3.094099843433151253, 1.348383549611749332, 1.636666742212993686 ) ) ;
#193541 = CARTESIAN_POINT ( 'NONE',  ( -4.960304097753355457, 6.880383762169266504, 1.599625672291263179 ) ) ;
#193542 = CARTESIAN_POINT ( 'NONE',  ( 4.206063578812153203, -2.156103337031569200, 0.1562769059922017589 ) ) ;
#193543 = CARTESIAN_POINT ( 'NONE',  ( 4.018977146631536712, -1.760761141180338774, 0.5383908109771737838 ) ) ;
#193544 = CARTESIAN_POINT ( 'NONE',  ( -5.203466197636060997, 6.462176032175228180, 1.180525766716962410 ) ) ;
#193545 = CARTESIAN_POINT ( 'NONE',  ( 1.364683531249986537, -0.3239583329919163424, 0.7879004041258500513 ) ) ;
#193546 = CARTESIAN_POINT ( 'NONE',  ( 6.122986541590657694, -1.636244173936936885, 0.5932577488661006093 ) ) ;
#193547 = CARTESIAN_POINT ( 'NONE',  ( 6.727182134110205602, 7.053355583909074689, 2.409100679957976165 ) ) ;
#193548 = CARTESIAN_POINT ( 'NONE',  ( 3.172244755917638770, 5.684407401003788607, -1.082531754730543083 ) ) ;
#193549 = CARTESIAN_POINT ( 'NONE',  ( -8.736946208889554263E-14, -8.872104535001076542, 9.837524982414052488 ) ) ;
#193550 = CARTESIAN_POINT ( 'NONE',  ( 3.397504326804317909, 1.702965868850464082, 1.331369057855802174 ) ) ;
#193551 = AXIS2_PLACEMENT_3D ( 'NONE', #209599, #61243, #157695 ) ;
#193552 = CARTESIAN_POINT ( 'NONE',  ( 5.290388671387995956, -1.915306256023459053, 0.6297802918850338161 ) ) ;
#193553 = CARTESIAN_POINT ( 'NONE',  ( -7.958272981097355370, 12.22847621134819285, 0.7216878364870458196 ) ) ;
#193554 = CARTESIAN_POINT ( 'NONE',  ( 2.114359756454447847, -1.018641858927371135, -1.906637348776268004 ) ) ;
#193555 = CARTESIAN_POINT ( 'NONE',  ( 3.303940151695891281, -1.969246965329603638, 0.09337747576219912471 ) ) ;
#193556 = PRESENTATION_STYLE_ASSIGNMENT (( #161064 ) ) ;
#193557 = CARTESIAN_POINT ( 'NONE',  ( 3.983879235506204264, -1.921370479222897165, -0.2818874784011967671 ) ) ;
#193559 = ORIENTED_EDGE ( 'NONE', *, *, #131422, .T. ) ;
#193558 = CARTESIAN_POINT ( 'NONE',  ( -7.958272981097355370, 12.22847621134819285, 0.7216878364870458196 ) ) ;
#193560 = CARTESIAN_POINT ( 'NONE',  ( -4.959250327548641479, 9.007818825440551791, -0.7998128361456362523 ) ) ;
#193561 = CARTESIAN_POINT ( 'NONE',  ( 11.92619526913699701, 10.19999999999998153, 1.328859060402682868 ) ) ;
#193563 = ORIENTED_EDGE ( 'NONE', *, *, #136789, .F. ) ;
#193562 = CARTESIAN_POINT ( 'NONE',  ( -3.820365424000704557, 7.679119771301277098, -0.7998128361456481317 ) ) ;
#193564 = CARTESIAN_POINT ( 'NONE',  ( -8.636180661780668899, 10.13826086257468795, -1.082531754730543083 ) ) ;
#193565 = CARTESIAN_POINT ( 'NONE',  ( 2.432911661931828284, 2.140371652790736601, 0.5367425311649312025 ) ) ;
#193566 = CARTESIAN_POINT ( 'NONE',  ( 3.285556943749998737, -1.655208332855374609, -1.896917185911906500 ) ) ;
#193567 = CARTESIAN_POINT ( 'NONE',  ( 6.649272889308863732, 1.708415183241231983, -0.9640671636572254455 ) ) ;
#193568 = CARTESIAN_POINT ( 'NONE',  ( -1.500000000000015099, 8.979166666666666075, -0.8660254037844309360 ) ) ;
#193569 = CARTESIAN_POINT ( 'NONE',  ( 1.499999999999989120, 4.327083334016148086, -0.8660254037844323793 ) ) ;
#193570 = CARTESIAN_POINT ( 'NONE',  ( 5.506841003474272966, 6.417672382999444203, -1.246111810019270738 ) ) ;
#193571 = DIRECTION ( 'NONE',  ( 0.000000000000000000, -1.084202172485501594E-14, -1.000000000000000000 ) ) ;
#193572 = CARTESIAN_POINT ( 'NONE',  ( 4.962772036422566480, 0.1772586797372834311, -1.832584332494808121 ) ) ;
#193573 = ORIENTED_EDGE ( 'NONE', *, *, #36816, .T. ) ;
#193574 = CARTESIAN_POINT ( 'NONE',  ( 4.506943796211477291E-15, 2.625000000682800483, 1.414508159514579644 ) ) ;
#193575 = CARTESIAN_POINT ( 'NONE',  ( -7.100719765255177229, 9.307259030929609267, -1.599625672291263179 ) ) ;
#193576 = LINE ( 'NONE', #28951, #151944 ) ;
#193577 = CARTESIAN_POINT ( 'NONE',  ( 5.906510592826289319, -2.110524776404258507, -0.2060971850248518311 ) ) ;
#193578 = CARTESIAN_POINT ( 'NONE',  ( 11.95123034216491398, 6.644963984119064193, -0.4921840132778478871 ) ) ;
#193579 = CARTESIAN_POINT ( 'NONE',  ( 5.311043488251262268, 7.219303374425030562, -1.599625672291256295 ) ) ;
#193580 = CARTESIAN_POINT ( 'NONE',  ( 6.714142707505978080, -0.9671387161254895171, -1.819716304366093551 ) ) ;
#193582 = CARTESIAN_POINT ( 'NONE',  ( 3.456447201099471123, -1.625387274077850996, -0.8650149607793489182 ) ) ;
#193581 = CARTESIAN_POINT ( 'NONE',  ( 2.154548830654204217, -0.4927303200079625745, -1.794580903941452865 ) ) ;
#193583 = CARTESIAN_POINT ( 'NONE',  ( 8.132193210098487057, 8.381980254736715708, 1.040834085586084257E-14 ) ) ;
#193584 = CARTESIAN_POINT ( 'NONE',  ( -9.386399777248481513, 14.48154088884566804, -7.476390435783241806 ) ) ;
#193585 = CARTESIAN_POINT ( 'NONE',  ( -6.200875153403786477, 8.327716660428123419, -1.599625672291271394 ) ) ;
#193587 = ORIENTED_EDGE ( 'NONE', *, *, #121379, .T. ) ;
#193586 = CARTESIAN_POINT ( 'NONE',  ( -1.500000000000008216, 10.49999999999999467, 3.469446951953614189E-15 ) ) ;
#193588 = CARTESIAN_POINT ( 'NONE',  ( 3.053566222061272040, -1.804402116661915967, -1.270350324234905903 ) ) ;
#193589 = CARTESIAN_POINT ( 'NONE',  ( 6.274757189715042927, -2.145364790639526564, -0.7184590933012062752 ) ) ;
#193590 = CARTESIAN_POINT ( 'NONE',  ( -6.480434237652138663, 8.583592582059388576, 1.443375672974078761 ) ) ;
#193591 = CARTESIAN_POINT ( 'NONE',  ( 6.117428737855862941, 1.511353622793030427, 0.9985130155200862001 ) ) ;
#193592 = CARTESIAN_POINT ( 'NONE',  ( 6.438697963858233564, -1.475898738386885123, 1.221124472464208743 ) ) ;
#193593 = CARTESIAN_POINT ( 'NONE',  ( -4.650083499807267984, 5.295740330745369207, 1.164732466530402855 ) ) ;
#193595 = EDGE_CURVE ( 'NONE', #100909, #33385, #182617, .T. ) ;
#193594 = VECTOR ( 'NONE', #197160, 1000.000000000000000 ) ;
#193596 = CARTESIAN_POINT ( 'NONE',  ( 5.893391625361731556, 1.417579469995243091, 1.220656814419220249 ) ) ;
#193597 = CARTESIAN_POINT ( 'NONE',  ( 5.795548653916324788, 1.765151677092157811, -0.7360495477024899813 ) ) ;
#193598 = CARTESIAN_POINT ( 'NONE',  ( 0.6373110600932235803, -1.319858442276698129, -1.325903642019378381 ) ) ;
#193599 = CARTESIAN_POINT ( 'NONE',  ( 1.323454262349360144, -1.463929862531298198, -1.387097294446784090 ) ) ;
#193601 = CARTESIAN_POINT ( 'NONE',  ( 3.580784747083717523, -2.029690618531124091, -0.5617794247858574064 ) ) ;
#193600 = CARTESIAN_POINT ( 'NONE',  ( -8.317037166979361018, 11.79062823052953668, 1.199719254218453823 ) ) ;
#193602 = CARTESIAN_POINT ( 'NONE',  ( 9.433775957010412938, 9.900493459467314850, 0.000000000000000000 ) ) ;
#193604 = CARTESIAN_POINT ( 'NONE',  ( -8.422639742587602285, 10.84949900448412841, -1.599625672291263179 ) ) ;
#193603 = CARTESIAN_POINT ( 'NONE',  ( -1.402160292154681736E-14, -0.9124999999999769962, -1.732050807568870754 ) ) ;
#193605 = CARTESIAN_POINT ( 'NONE',  ( 11.44800751629993130, 9.799999999999982947, 3.302956944461088451 ) ) ;
#193606 = CARTESIAN_POINT ( 'NONE',  ( 2.742449504557340489, 1.118516972803576870, -1.681586373676981827 ) ) ;
#193607 = CARTESIAN_POINT ( 'NONE',  ( 1.364683531249988535, 2.905208333674754506, -0.7879004041258239610 ) ) ;
#193608 = CARTESIAN_POINT ( 'NONE',  ( 9.951321562750607086, 11.67259191370631477, -1.082531754730537088 ) ) ;
#193609 = CARTESIAN_POINT ( 'NONE',  ( 3.831458500214664387, -1.998831773244442056, 0.8233788064144487162 ) ) ;
#193610 = CARTESIAN_POINT ( 'NONE',  ( 7.095713291905693332, 9.371694488680407886, 1.599625672291268286 ) ) ;
#193611 = CARTESIAN_POINT ( 'NONE',  ( 0.7499999999999920064, 4.733333333333352932, 1.299038105676669330 ) ) ;
#193613 = CARTESIAN_POINT ( 'NONE',  ( 0.000000000000000000, 0.5000000000000004441, 0.000000000000000000 ) ) ;
#193612 = CARTESIAN_POINT ( 'NONE',  ( 7.517069824134078537, 7.734612647770044092, 0.000000000000000000 ) ) ;
#193614 = CARTESIAN_POINT ( 'NONE',  ( 7.578644679914702031, 10.82520731233375955, 1.082531754730558626 ) ) ;
#193616 = CARTESIAN_POINT ( 'NONE',  ( 9.428250952287722697, 13.54490846161957762, -7.423481931054033645 ) ) ;
#193615 = CARTESIAN_POINT ( 'NONE',  ( 0.3796378701454300453, -0.1059898317679157376, 2.168723291021804833 ) ) ;
#193617 = CARTESIAN_POINT ( 'NONE',  ( -6.399085315970142851, 8.488685506763726352, -1.443375672974059665 ) ) ;
#193618 = CARTESIAN_POINT ( 'NONE',  ( -0.6823417656250212460, 2.051041667008083991, 1.181850606188767472 ) ) ;
#193619 = CARTESIAN_POINT ( 'NONE',  ( 2.507599501126521524, -2.167277876680247850, 0.3246147914140809498 ) ) ;
#193620 = CARTESIAN_POINT ( 'NONE',  ( 6.983263157960363010, -0.003310164959547181717, 1.953544951557646403 ) ) ;
#193621 = CARTESIAN_POINT ( 'NONE',  ( 2.061739773175938595, 0.3863463398323406794, -2.229145236428681454 ) ) ;
#193622 = CARTESIAN_POINT ( 'NONE',  ( -7.369020184227459858, 8.555943955475521889, 1.199719254218450271 ) ) ;
#193623 = CARTESIAN_POINT ( 'NONE',  ( -0.6823417656249969321, 5.030208333674755394, -1.181850606188749264 ) ) ;
#193624 = CARTESIAN_POINT ( 'NONE',  ( 5.701630405109389343, 7.302376724489803905, 1.216486997566777584 ) ) ;
#193625 = CARTESIAN_POINT ( 'NONE',  ( 1.499999999999997113, 11.89583333333333570, -0.8660254037844378194 ) ) ;
#193626 = CARTESIAN_POINT ( 'NONE',  ( 7.377044979611483200, 7.779176362401098999, -0.7216878364870317197 ) ) ;
#193627 = CARTESIAN_POINT ( 'NONE',  ( 4.762845401903825326, -1.580659612885275012, -0.7961057336023872333 ) ) ;
#193628 = CARTESIAN_POINT ( 'NONE',  ( 9.043452155515161905, 10.50944792197790889, 1.199719254218453823 ) ) ;
#193629 = CARTESIAN_POINT ( 'NONE',  ( 0.4289210115673793844, 2.015304021226202558, 0.6111801191295732627 ) ) ;
#193630 = CARTESIAN_POINT ( 'NONE',  ( -1.364683531250000748, 9.359375000341396245, 0.000000000000000000 ) ) ;
#193631 = CARTESIAN_POINT ( 'NONE',  ( -5.147255595043616516, 6.034161611419515125, 1.199719254218452935 ) ) ;
#193632 = CARTESIAN_POINT ( 'NONE',  ( 6.538686444676896414, -1.556836737174282836, 1.281159629702780078 ) ) ;
#193633 = ORIENTED_EDGE ( 'NONE', *, *, #120712, .F. ) ;
#193634 = CARTESIAN_POINT ( 'NONE',  ( 10.01963921569910632, 11.64833282552586091, 1.199719254218450271 ) ) ;
#193635 = CARTESIAN_POINT ( 'NONE',  ( 3.467518583331068438, 1.825290416974333807, -0.4087457676540603990 ) ) ;
#193636 = CARTESIAN_POINT ( 'NONE',  ( 3.098552089154332112, 2.054082100768514607, 0.2579794602402472603 ) ) ;
#193637 = CARTESIAN_POINT ( 'NONE',  ( -7.092323753280154186, 7.447001598347859463, 0.7216878364870317197 ) ) ;
#193638 = CARTESIAN_POINT ( 'NONE',  ( -0.6499422464084805284, 3.350075079687096391, -0.06926476342541870723 ) ) ;
#193639 = CARTESIAN_POINT ( 'NONE',  ( 9.077347539549325717, 10.54899253668443393, -1.199719254218446718 ) ) ;
#193640 = CARTESIAN_POINT ( 'NONE',  ( -1.500000000000022204, 8.627523663848661428, 2.580000000000011173 ) ) ;
#193641 = SURFACE_STYLE_USAGE ( .BOTH. , #30086 ) ;
#193642 = EDGE_CURVE ( 'NONE', #71735, #53136, #5470, .T. ) ;
#193643 = DIRECTION ( 'NONE',  ( -1.000000000000000000, 7.109522442527888164E-16, 0.000000000000000000 ) ) ;
#193644 = CARTESIAN_POINT ( 'NONE',  ( -0.6823417656250212460, 5.113541667008086655, 1.181850606188767472 ) ) ;
#193645 = CARTESIAN_POINT ( 'NONE',  ( 3.701569118832209515, -1.483977648892897960, -1.283320388228793130 ) ) ;
#193646 = CARTESIAN_POINT ( 'NONE',  ( 0.4915642615439493879, 1.928455281639355867, 0.5879340682083398217 ) ) ;
#193647 = DIRECTION ( 'NONE',  ( -1.000000000000000000, 7.771561172376097755E-16, 4.440892098500627148E-16 ) ) ;
#193649 = CARTESIAN_POINT ( 'NONE',  ( 0.4465194593917843902, 3.080450244942134486, 0.4155024747329351120 ) ) ;
#193648 = CARTESIAN_POINT ( 'NONE',  ( 7.690499447449630210, 9.995335326823163058, 1.599625672291281386 ) ) ;
#193650 = CARTESIAN_POINT ( 'NONE',  ( 0.7900579835180140398, -1.855660487967484951, -0.2351621623290362506 ) ) ;
#193651 = CARTESIAN_POINT ( 'NONE',  ( 1.364683531249988535, 3.363541667008084879, 0.7879004041258500513 ) ) ;
#193652 = CARTESIAN_POINT ( 'NONE',  ( 2.847905013607958669, -1.355098151751940483, -1.488992504630684000 ) ) ;
#193654 = CARTESIAN_POINT ( 'NONE',  ( 1.933370326505511105, -1.702675829696152388, -1.258230627273223545 ) ) ;
#193653 = CARTESIAN_POINT ( 'NONE',  ( -6.616015773788831211, 7.781401826584148473, 1.082531754730549967 ) ) ;
#193655 = CARTESIAN_POINT ( 'NONE',  ( 9.476699878348894046, 11.04296043381019743, -7.367623491263915803 ) ) ;
#193656 = CARTESIAN_POINT ( 'NONE',  ( 3.648938843998358106, -0.4010542052625790110, -2.030977206718207473 ) ) ;
#193657 = CARTESIAN_POINT ( 'NONE',  ( 7.856023664475727308, 8.130058794835305136, -0.7998128361456341429 ) ) ;
#193659 = CARTESIAN_POINT ( 'NONE',  ( 11.92050416151433012, 13.65205375279633238, 1.381922468431395767 ) ) ;
#193658 = CARTESIAN_POINT ( 'NONE',  ( 0.09931936810910445279, -0.5537021472524807919, 2.016037456109684989 ) ) ;
#193661 = ORIENTED_EDGE ( 'NONE', *, *, #128877, .T. ) ;
#193660 = CARTESIAN_POINT ( 'NONE',  ( 5.192344348049102720, -1.811977082810274808, -0.2219828972063255801 ) ) ;
#193662 = CARTESIAN_POINT ( 'NONE',  ( 7.242026607993941489, 11.60078147596829901, 0.7998128361456462443 ) ) ;
#193663 = CARTESIAN_POINT ( 'NONE',  ( 1.387358672532239989, 7.315968950352816691, -4.254625267139963363 ) ) ;
#193664 = CARTESIAN_POINT ( 'NONE',  ( 10.40290000253160940, 12.22595686778796065, -6.657689775135003707 ) ) ;
#193665 = VECTOR ( 'NONE', #53470, 1000.000000000000114 ) ;
#193666 = CARTESIAN_POINT ( 'NONE',  ( 6.282275147445602670, -1.185768659569720329, 1.860957768143455038 ) ) ;
#193667 = CARTESIAN_POINT ( 'NONE',  ( -1.364683531250000748, 12.17187500034139980, 0.000000000000000000 ) ) ;
#193668 = CARTESIAN_POINT ( 'NONE',  ( 5.602191078447533279, -0.8559053986842229955, 1.710104642658970997 ) ) ;
#193669 = CARTESIAN_POINT ( 'NONE',  ( -9.833741488613570780, 10.36711991300432345, 0.7998128361456462443 ) ) ;
#193670 = CARTESIAN_POINT ( 'NONE',  ( 6.012151052656117933, 9.101594430485762999, 1.199719254218460707 ) ) ;
#193671 = CARTESIAN_POINT ( 'NONE',  ( -3.555477883677943599E-14, 2.484375000341469963, 1.570758158831768281 ) ) ;
#193672 = CARTESIAN_POINT ( 'NONE',  ( 3.023105065722948126, 6.470780310077995701, 0.7216878364870338292 ) ) ;
#193673 = CARTESIAN_POINT ( 'NONE',  ( 9.488641820551089623, -8.233137084989849086, -0.4644097342742991019 ) ) ;
#193674 = CARTESIAN_POINT ( 'NONE',  ( 4.009460741339333723, 5.700790169694431420, -1.599625672291256295 ) ) ;
#193675 = ORIENTED_EDGE ( 'NONE', *, *, #45482, .F. ) ;
#193676 = DIRECTION ( 'NONE',  ( 0.000000000000000000, 0.000000000000000000, -1.000000000000000000 ) ) ;
#193677 = CIRCLE ( 'NONE', #31068, 11.09999999999999964 ) ;
#193678 = CARTESIAN_POINT ( 'NONE',  ( -3.650979853707545075, 7.481503272625923628, -0.4052952642843922204 ) ) ;
#193679 = CARTESIAN_POINT ( 'NONE',  ( 6.638652492546827766, 7.774124658506663010, 1.199719254218452047 ) ) ;
#193680 = SURFACE_STYLE_FILL_AREA ( #61555 ) ;
#193681 = CARTESIAN_POINT ( 'NONE',  ( -6.068414747559345734, 7.047288584480712714, 1.012934185448462143 ) ) ;
#193682 = CARTESIAN_POINT ( 'NONE',  ( -6.290620087060847965, 7.401773525401500464, 1.082531754730549967 ) ) ;
#193683 = CARTESIAN_POINT ( 'NONE',  ( 4.304877467538922531, 4.981110786005563007, 1.199719254218464037 ) ) ;
#193684 = CARTESIAN_POINT ( 'NONE',  ( 2.623828205405827507, 1.932375918485039756, -0.3793698109293401344 ) ) ;
#193685 = CARTESIAN_POINT ( 'NONE',  ( 3.286732619643798703, 1.587825416925658262, -1.242744175535138940 ) ) ;
#193686 = CARTESIAN_POINT ( 'NONE',  ( -6.672584156219988571, 10.93643194889866521, -0.7998128361456291469 ) ) ;
#193687 = CARTESIAN_POINT ( 'NONE',  ( 4.258142763143749399, 7.125527769379820242, 1.199719254218451159 ) ) ;
#193688 = CARTESIAN_POINT ( 'NONE',  ( 6.827182134110222123, 4.687887262399931920, 2.751577338787388083 ) ) ;
#193689 = CARTESIAN_POINT ( 'NONE',  ( 3.504031732436951874, -0.8880451304637152488, -2.003635182500095535 ) ) ;
#193690 = CARTESIAN_POINT ( 'NONE',  ( 0.08058608058607655278, -8.270571484000479145, 10.99970480893082225 ) ) ;
#193691 = CARTESIAN_POINT ( 'NONE',  ( 2.063383741992553144, 0.3316209358346365876, -1.897488084917675843 ) ) ;
#193692 = CARTESIAN_POINT ( 'NONE',  ( -9.215791728987058562, 11.77484298861683598, -1.599625672291263179 ) ) ;
#193693 = CARTESIAN_POINT ( 'NONE',  ( -0.1296875068448125057, 1.390030859318210688, -2.083197486262199138 ) ) ;
#193694 = CARTESIAN_POINT ( 'NONE',  ( 0.2329586101569527945, 7.629137130509077380, -2.445728209250570107 ) ) ;
#193695 = CARTESIAN_POINT ( 'NONE',  ( 4.760321332173959696, 4.726332107057286791, 0.000000000000000000 ) ) ;
#193696 = CARTESIAN_POINT ( 'NONE',  ( 7.934546212495622086, 10.28005655271014795, -1.599625672291262513 ) ) ;
#193697 = CARTESIAN_POINT ( 'NONE',  ( 4.638861114170084399, 8.563755066507100722, 0.7998128361456462443 ) ) ;
#193698 = CARTESIAN_POINT ( 'NONE',  ( 2.218730694130720771, 5.740269576461138890, 0.7998128361456462443 ) ) ;
#193699 = CARTESIAN_POINT ( 'NONE',  ( 4.692530564105613422, 7.528350520548263702, -1.082531754730548412 ) ) ;
#193700 = ORIENTED_EDGE ( 'NONE', *, *, #186547, .F. ) ;
#193702 = CARTESIAN_POINT ( 'NONE',  ( 2.209637070578834628, 1.557646164037255643, 1.275278917823706948 ) ) ;
#193701 = CARTESIAN_POINT ( 'NONE',  ( 5.302248432823610358, 1.390444127666954355, -1.207098008268410183 ) ) ;
#193703 = CARTESIAN_POINT ( 'NONE',  ( 4.007374829128952598, 2.286843722993581185, 0.2302655642077624243 ) ) ;
#193705 = CARTESIAN_POINT ( 'NONE',  ( 2.465471660774602558, -0.4132369024843309258, 1.814301444843221089 ) ) ;
#193704 = CARTESIAN_POINT ( 'NONE',  ( -0.1291982275798625457, 2.008329037175633491, -2.487957029800022202 ) ) ;
#193706 = CARTESIAN_POINT ( 'NONE',  ( -3.285556943749998737, -2.880208332855377584, 1.896917185911908499 ) ) ;
#193707 = CARTESIAN_POINT ( 'NONE',  ( -9.608183788959879124, 14.88164563814821939, -7.189075342400532698 ) ) ;
#193708 = CARTESIAN_POINT ( 'NONE',  ( 5.062724140118719518, 0.5608846916410530348, 1.828269531156314853 ) ) ;
#193709 = CARTESIAN_POINT ( 'NONE',  ( -6.808165692356648258, 11.09461040772476714, 0.7998128361456481317 ) ) ;
#193710 = EDGE_CURVE ( 'NONE', #63797, #82918, #21920, .T. ) ;
#193711 = CARTESIAN_POINT ( 'NONE',  ( -5.099275172515603138, 8.002885897026576600, 1.082531754730549967 ) ) ;
#193713 = CARTESIAN_POINT ( 'NONE',  ( 3.151090109352538082, -1.528452604574185525, -1.078222621661927061 ) ) ;
#193712 = CARTESIAN_POINT ( 'NONE',  ( 4.528904929885309905, -1.910896387970087096, 0.8487916243252179305 ) ) ;
#193714 = CARTESIAN_POINT ( 'NONE',  ( 6.643132081016124069, 7.813037518349371879, 1.082531754730558626 ) ) ;
#193715 = ORIENTED_EDGE ( 'NONE', *, *, #54197, .T. ) ;
#193716 = CARTESIAN_POINT ( 'NONE',  ( -15.75000000000000000, 13.40000000000000036, 1.099999999999996758 ) ) ;
#193717 = CARTESIAN_POINT ( 'NONE',  ( -1.938011383317839176E-15, -8.407420853759283830, -10.91970695577494865 ) ) ;
#193718 = CARTESIAN_POINT ( 'NONE',  ( 5.004412211769132313, -0.5859011197271257743, -1.622467267129880097 ) ) ;
#193719 = CARTESIAN_POINT ( 'NONE',  ( -7.250913225210214641, 7.353820272367037170, 0.7998128361456341429 ) ) ;
#193720 = CARTESIAN_POINT ( 'NONE',  ( 1.775574910200255818, 1.508776774498999718, -0.8547552410581791271 ) ) ;
#193721 = DIRECTION ( 'NONE',  ( -0.000000000000000000, 0.000000000000000000, -1.000000000000000000 ) ) ;
#193722 = DIRECTION ( 'NONE',  ( 0.000000000000000000, 1.000000000000000000, 0.000000000000000000 ) ) ;
#193723 = CARTESIAN_POINT ( 'NONE',  ( 2.679285714285720044, -0.4970443252110337551, -0.5000000000000004441 ) ) ;
#193724 = CARTESIAN_POINT ( 'NONE',  ( 5.911019566678890058, -1.716411647115582140, 1.329421173595428884 ) ) ;
#193725 = CARTESIAN_POINT ( 'NONE',  ( 4.213378774425760476, -0.3099129147984269195, 1.799030153321119263 ) ) ;
#193726 = CARTESIAN_POINT ( 'NONE',  ( 1.815213341579174688, -1.679845371888911698, -1.013028538569618719 ) ) ;
#193727 = CARTESIAN_POINT ( 'NONE',  ( 0.1931602983361295767, 1.844477155017531844, 1.039358475685886907 ) ) ;
#193728 = CARTESIAN_POINT ( 'NONE',  ( 9.601861702642535690, 3.883749503993501051, 7.121442011178659826 ) ) ;
#193729 = CARTESIAN_POINT ( 'NONE',  ( -6.158835246850665095E-15, 0.8125000000000031086, 1.224999999999960565 ) ) ;
#193730 = CARTESIAN_POINT ( 'NONE',  ( 8.762647353133951711, 9.117510088278095282, 1.040834085586084257E-14 ) ) ;
#193731 = CARTESIAN_POINT ( 'NONE',  ( 2.596466591541984226, -1.087938976695131066, 1.819974527870950265 ) ) ;
#193732 = CARTESIAN_POINT ( 'NONE',  ( -2.982430605326321427, 6.423326772948587227, -0.7216878364870267237 ) ) ;
#193733 = CARTESIAN_POINT ( 'NONE',  ( -15.75000000000000000, 11.29999999999999893, 0.6999999999999992895 ) ) ;
#193734 = CARTESIAN_POINT ( 'NONE',  ( -4.447391987980185313, 7.103198448885253313, -1.107391122544647333 ) ) ;
#193735 = CARTESIAN_POINT ( 'NONE',  ( 6.912935025559954205, -1.683935878860399971, 1.369999676949062550 ) ) ;
#193737 = CARTESIAN_POINT ( 'NONE',  ( -1.500000000000001110, 13.30208333401612997, 0.8660254037844419273 ) ) ;
#193736 = CARTESIAN_POINT ( 'NONE',  ( -9.569358774149645086, 3.553052365627043852, 7.167287524840456392 ) ) ;
#193739 = ORIENTED_EDGE ( 'NONE', *, *, #144993, .F. ) ;
#193738 = CARTESIAN_POINT ( 'NONE',  ( 3.580930751873512285, -1.490882799914891033, 1.646821992171596971 ) ) ;
#193740 = CARTESIAN_POINT ( 'NONE',  ( 0.8272591630335036639, 0.9250671760404407529, -2.104501483148725427 ) ) ;
#193742 = CARTESIAN_POINT ( 'NONE',  ( 5.506706524517535506, 0.5933582781832097419, 1.975413352875006856 ) ) ;
#193741 = CARTESIAN_POINT ( 'NONE',  ( 3.602716132929354664, 5.226254793216122074, 1.599625672291267398 ) ) ;
#193744 = CARTESIAN_POINT ( 'NONE',  ( 0.000000000000000000, -1.487500000000001599, -4.012584370867899430 ) ) ;
#193743 = CARTESIAN_POINT ( 'NONE',  ( 4.420840606507738357, 7.315341919971147355, 1.199719254218451159 ) ) ;
#193745 = CARTESIAN_POINT ( 'NONE',  ( 6.110883706712432861, -0.2185277653131960651, 1.828168259763853776 ) ) ;
#193746 = CARTESIAN_POINT ( 'NONE',  ( 3.897079088924235712, 6.634010472798538949, 1.199719254218462483 ) ) ;
#193747 = FILL_AREA_STYLE ('',( #195899 ) ) ;
#193748 = CARTESIAN_POINT ( 'NONE',  ( 3.363966847960923268, 0.7745139696748448710, 1.541148353905038126 ) ) ;
#193749 = CARTESIAN_POINT ( 'NONE',  ( 0.8312679839070148402, -1.592664559859976237, -1.236796411087807801 ) ) ;
#193750 = CARTESIAN_POINT ( 'NONE',  ( 3.200086968229500783, 2.078864265255635946, 0.9811947989078557697 ) ) ;
#193751 = CARTESIAN_POINT ( 'NONE',  ( -1.364683531249997417, 3.571875000341423245, 1.214306433183764966E-14 ) ) ;
#193752 = CARTESIAN_POINT ( 'NONE',  ( 2.794484930487377561, -2.256151742081555334, -0.1692699688307132133 ) ) ;
#193753 = CARTESIAN_POINT ( 'NONE',  ( 4.723321587070372196, -0.1039652108096918437, 2.103624988570974352 ) ) ;
#193754 = CARTESIAN_POINT ( 'NONE',  ( -3.284818356260900796, 7.054314858938165678, 0.7998128361456352531 ) ) ;
#193755 = CARTESIAN_POINT ( 'NONE',  ( 3.127930002535435516, 0.9861435696450934207, -1.469289397387682161 ) ) ;
#193756 = CARTESIAN_POINT ( 'NONE',  ( 6.159481859310094620, 6.080483678816896109, 1.040834085586084257E-14 ) ) ;
#193758 = CARTESIAN_POINT ( 'NONE',  ( 6.146038201015474378, 0.7148980135479511278, 2.178090959246486324 ) ) ;
#193757 = CARTESIAN_POINT ( 'NONE',  ( 4.434925645001613681, 5.307073019657559065, -1.082531754730548412 ) ) ;
#193759 = CARTESIAN_POINT ( 'NONE',  ( 4.294743845541324490, 1.480121740587354573, 1.094796260939827404 ) ) ;
#193760 = CARTESIAN_POINT ( 'NONE',  ( -3.761497552787613330, 6.475832013972435242, 1.199719254218464037 ) ) ;
#193761 = B_SPLINE_CURVE_WITH_KNOTS ( 'NONE', 3,
 ( #84908, #201831, #3626, #67561, #135807, #133704 ),
 .UNSPECIFIED., .F., .F.,
 ( 4, 2, 4 ),
 ( 0.000000000000000000, 0.0003168911866439334617, 0.0006337823732878669234 ),
 .UNSPECIFIED. ) ;
#193762 = CARTESIAN_POINT ( 'NONE',  ( 4.595850884908202261, 7.345281218159464665, -1.082531754730549078 ) ) ;
#193763 = CARTESIAN_POINT ( 'NONE',  ( 1.499999999999989120, 3.025000000000020783, 1.214306433183764966E-14 ) ) ;
#193764 = CARTESIAN_POINT ( 'NONE',  ( 4.330150130892728377, 2.148942519667027984, 0.4286813238914553015 ) ) ;
#193765 = CARTESIAN_POINT ( 'NONE',  ( -5.122283107864663343, 4.870418468797203637, 0.000000000000000000 ) ) ;
#193766 = CARTESIAN_POINT ( 'NONE',  ( 11.89942855770814312, 13.88000000000000078, 0.6999999999999992895 ) ) ;
#193767 = DIRECTION ( 'NONE',  ( -0.6507913734559559460, 0.7592566023653074536, 0.000000000000000000 ) ) ;
#193768 = PRESENTATION_LAYER_ASSIGNMENT (  '', '', ( #159145 ) ) ;
#193769 = CARTESIAN_POINT ( 'NONE',  ( -1.364683531250010295, 4.030208333674751842, 0.7879004041258379498 ) ) ;
#193770 = CARTESIAN_POINT ( 'NONE',  ( 2.895051130818243834, 1.652057846050537515, -0.9908002393040680200 ) ) ;
#193771 = CARTESIAN_POINT ( 'NONE',  ( -1.402160292154681736E-14, 8.671875000341403350, 1.575800808251682339 ) ) ;
#193772 = CARTESIAN_POINT ( 'NONE',  ( -3.619663825168619731, 7.166765529431275539, 1.040834085586084257E-14 ) ) ;
#193773 = CARTESIAN_POINT ( 'NONE',  ( 0.5630927014088433769, 0.6521865704650819939, 2.123503569120980927 ) ) ;
#193774 = EDGE_LOOP ( 'NONE', ( #199763, #46120, #27075, #157153 ) ) ;
#193776 = FILL_AREA_STYLE ('',( #97373 ) ) ;
#193775 = CARTESIAN_POINT ( 'NONE',  ( -3.024877669624710386, 6.543124691288523920, 0.000000000000000000 ) ) ;
#193777 = CARTESIAN_POINT ( 'NONE',  ( 4.976006071415387311, 5.764094157194782575, 1.199719254218462483 ) ) ;
#193778 = PLANE ( 'NONE',  #49322 ) ;
#193779 = DIRECTION ( 'NONE',  ( -8.881784197001252323E-15, 0.000000000000000000, 1.000000000000000000 ) ) ;
#193780 = CARTESIAN_POINT ( 'NONE',  ( 2.770765728838171960, 1.651868531079144553, -0.5482889651245922424 ) ) ;
#193781 = CARTESIAN_POINT ( 'NONE',  ( 6.775478006741583847, -7.217909409563576517, 6.775478006741560755 ) ) ;
#193782 = DIRECTION ( 'NONE',  ( 0.000000000000000000, 1.000000000000000000, 0.000000000000000000 ) ) ;
#193783 = CARTESIAN_POINT ( 'NONE',  ( 0.6823417656249899377, 1.155208333674752286, 1.181850606188755259 ) ) ;
#193784 = DIRECTION ( 'NONE',  ( -0.7592566023653003482, 0.6507913734559641616, 0.000000000000000000 ) ) ;
#193785 = CARTESIAN_POINT ( 'NONE',  ( -10.47097470845587175, 11.11055866948701443, 1.040834085586084257E-14 ) ) ;
#193786 = CARTESIAN_POINT ( 'NONE',  ( -4.216222583725562245, 7.862750747747711877, 0.7216878364870317197 ) ) ;
#193787 = CARTESIAN_POINT ( 'NONE',  ( 6.227428301493934448, -2.037140905555033576, 0.7235935974677574212 ) ) ;
#193789 = ORIENTED_EDGE ( 'NONE', *, *, #91258, .T. ) ;
#193788 = CARTESIAN_POINT ( 'NONE',  ( -8.855744143575682514, 3.691791674785632082, -7.453352967675195728 ) ) ;
#193790 = CARTESIAN_POINT ( 'NONE',  ( -1.364683531250012516, 4.738541667008091096, -0.7879004041258300672 ) ) ;
#193791 = CARTESIAN_POINT ( 'NONE',  ( 0.1923495491853322581, -0.4021996241703913455, -1.833441224692602844 ) ) ;
#193792 = CARTESIAN_POINT ( 'NONE',  ( 5.782511917101329502, -1.690859530023439250, 0.3827970650602616765 ) ) ;
#193794 = CARTESIAN_POINT ( 'NONE',  ( 3.193114300108112147, 1.729001323093733111, 1.346577201094656395 ) ) ;
#193793 = CARTESIAN_POINT ( 'NONE',  ( -0.6801582343750299797, 1.182291667008061875, 1.178068619123820771 ) ) ;
#193795 = CARTESIAN_POINT ( 'NONE',  ( 3.540313787445231508, 1.039887675495542618, -2.060077152250729071 ) ) ;
#193796 = CARTESIAN_POINT ( 'NONE',  ( 5.360643824631334375, -1.495535663558609674, 1.418079957933044755 ) ) ;
#193797 = CARTESIAN_POINT ( 'NONE',  ( 1.201004818612857017, -0.4721336787944198643, 1.883569333377318245 ) ) ;
#193798 = CARTESIAN_POINT ( 'NONE',  ( -4.880572110795192486, 8.637825195995631589, 1.214306433183764966E-14 ) ) ;
#193799 = FACE_OUTER_BOUND ( 'NONE', #12139, .T. ) ;
#193800 = DIRECTION ( 'NONE',  ( -3.330669073875478989E-16, 3.330669073875478989E-16, 1.000000000000000000 ) ) ;
#193801 = CARTESIAN_POINT ( 'NONE',  ( 4.271814301144261528, 0.4616217191124799002, -2.069597271375968273 ) ) ;
#193802 = CARTESIAN_POINT ( 'NONE',  ( 1.846327496167538884, 0.3419342931599393398, -1.987046799686801757 ) ) ;
#193803 = CARTESIAN_POINT ( 'NONE',  ( -5.951666246274811556, 7.966696592119163256, 1.443375672974064550 ) ) ;
#193804 = CARTESIAN_POINT ( 'NONE',  ( 5.807716119225245777, -0.5415507062403871474, 2.139171552897000339 ) ) ;
#193805 = CARTESIAN_POINT ( 'NONE',  ( 1.642778471875000035, -0.6635416661887084677, -2.845375778867859751 ) ) ;
#193806 = CARTESIAN_POINT ( 'NONE',  ( -2.112474647679212225, -3.050145162711633162, 2.777154369939415002 ) ) ;
#193807 = CARTESIAN_POINT ( 'NONE',  ( 0.3811277156573149583, 1.704729334087114578, -0.6539457117896373406 ) ) ;
#193808 = DIRECTION ( 'NONE',  ( 0.000000000000000000, 1.000000000000000000, 0.000000000000000000 ) ) ;
#193810 = CARTESIAN_POINT ( 'NONE',  ( -2.609770642201835855, -0.3830433331901521576, 0.000000000000000000 ) ) ;
#193809 = CARTESIAN_POINT ( 'NONE',  ( -5.094039349513959536, 7.939876775568885492, 1.214520887661042936 ) ) ;
#193811 = CARTESIAN_POINT ( 'NONE',  ( 1.608462485350599769, 8.735270501766756013, -2.463594439587629914 ) ) ;
#193812 = VERTEX_POINT ( 'NONE', #201552 ) ;
#193813 = CARTESIAN_POINT ( 'NONE',  ( 4.469639075930389893, 1.999461767218065678, -0.4989166988303375683 ) ) ;
#193814 = CARTESIAN_POINT ( 'NONE',  ( 0.6801582343749987825, 2.723958333674732391, 1.178068619123836314 ) ) ;
#193815 = CARTESIAN_POINT ( 'NONE',  ( -0.2108831679771203116, 0.7314853703891763814, -1.979988191570913880 ) ) ;
#193816 = CARTESIAN_POINT ( 'NONE',  ( -3.567766978690493307, 7.314145241780881435, 1.040834085586084257E-14 ) ) ;
#193817 = CARTESIAN_POINT ( 'NONE',  ( -4.787964524281469458, 5.614988695530339413, -1.199719254218453823 ) ) ;
#193818 = CARTESIAN_POINT ( 'NONE',  ( 4.828773858256512064, 1.391243881446821762, -1.464325142460545459 ) ) ;
#193819 = CARTESIAN_POINT ( 'NONE',  ( -1.500000000000013101, 0.4208333333333572068, 0.8660254037844403729 ) ) ;
#193821 = CARTESIAN_POINT ( 'NONE',  ( 9.408995418203975447, 10.07950886410055524, 0.7216878364870438212 ) ) ;
#193820 = CARTESIAN_POINT ( 'NONE',  ( -3.820365424000704557, 7.679119771301277098, -0.7998128361456481317 ) ) ;
#193822 = CARTESIAN_POINT ( 'NONE',  ( 7.955937213120826357, 8.176348258262782664, 0.7998128361456481317 ) ) ;
#193823 = CARTESIAN_POINT ( 'NONE',  ( 3.414965445803084254, 1.862500966792278057, 0.8825600945957471355 ) ) ;
#193824 = CARTESIAN_POINT ( 'NONE',  ( 2.865861461037176205, -0.1511401116795624278, -2.010826411938296143 ) ) ;
#193825 = ORIENTED_EDGE ( 'NONE', *, *, #128394, .F. ) ;
#193826 = CARTESIAN_POINT ( 'NONE',  ( 0.000000000000000000, 11.29999999999999893, 0.000000000000000000 ) ) ;
#193827 = CARTESIAN_POINT ( 'NONE',  ( 3.330499290451326200, 7.037332938835193730, -0.7998128361456291469 ) ) ;
#193829 = ORIENTED_EDGE ( 'NONE', *, *, #61547, .T. ) ;
#193828 = CARTESIAN_POINT ( 'NONE',  ( -0.2837385194698915925, 8.150966340525300780, -2.020310785919212648 ) ) ;
#193830 = CARTESIAN_POINT ( 'NONE',  ( 2.934922540206805319, 1.076151813804010926, 1.704677747124828446 ) ) ;
#193831 = CARTESIAN_POINT ( 'NONE',  ( 1.904012794591736668, 1.364881752761820222, -1.235849761865935870 ) ) ;
#193832 = CARTESIAN_POINT ( 'NONE',  ( 0.06561565146986823860, -2.064482179495107150, -1.031447015078267304 ) ) ;
#193833 = CARTESIAN_POINT ( 'NONE',  ( 4.549643065837591038, 7.465611455855944101, -1.199719254218452047 ) ) ;
#193834 = EDGE_CURVE ( 'NONE', #71497, #132514, #88606, .T. ) ;
#193835 = CARTESIAN_POINT ( 'NONE',  ( 2.179201376995115513, -0.1036959380565916911, -2.159207860300814463 ) ) ;
#193836 = CARTESIAN_POINT ( 'NONE',  ( 8.072990401933337168, 11.50590700464255356, -1.199719254218446718 ) ) ;
#193837 = CARTESIAN_POINT ( 'NONE',  ( -5.656776405399756236, 7.622658444431597680, -1.599625672291256295 ) ) ;
#193838 = ADVANCED_FACE ( 'NONE', ( #182112 ), #19246, .T. ) ;
#193839 = ORIENTED_EDGE ( 'NONE', *, *, #192621, .F. ) ;
#193840 = CARTESIAN_POINT ( 'NONE',  ( 0.1949432477380687867, 3.354551554867308827, -2.067633736988962578 ) ) ;
#193841 = CARTESIAN_POINT ( 'NONE',  ( 1.516246529245099284, 1.258767711876613848, -1.383943980506313398 ) ) ;
#193842 = CARTESIAN_POINT ( 'NONE',  ( 5.207875265678946874, -1.962022031532301369, 0.1926216461900862598 ) ) ;
#193844 = CARTESIAN_POINT ( 'NONE',  ( 8.175203438916005538, 11.52119253116861586, -1.082531754730543083 ) ) ;
#193843 = CARTESIAN_POINT ( 'NONE',  ( 1.364683531249990311, 3.134375000341423245, 1.214306433183764966E-14 ) ) ;
#193846 = CARTESIAN_POINT ( 'NONE',  ( 0.08304785351339466493, -2.141800023564765620, -0.5316218738360134477 ) ) ;
#193845 = CARTESIAN_POINT ( 'NONE',  ( -5.930802130974132780, 9.006687355190106103, -1.199719254218440723 ) ) ;
#193847 = CARTESIAN_POINT ( 'NONE',  ( 6.496543107701719499, 2.047251205643263017, 0.3077783505985449142 ) ) ;
#193848 = CARTESIAN_POINT ( 'NONE',  ( 5.198661835836162481, 8.152523677529138979, 1.199719254218462483 ) ) ;
#193849 = CARTESIAN_POINT ( 'NONE',  ( -5.900823170445743671, 7.907379670318584353, 1.599625672291269396 ) ) ;
#193850 = CARTESIAN_POINT ( 'NONE',  ( 6.539320575229258914, 2.958022083381315337, 2.556018433155104574 ) ) ;
#193851 = CARTESIAN_POINT ( 'NONE',  ( 5.137557537983609812, -1.393591726081166771, -1.394729141857486532 ) ) ;
#193852 = CARTESIAN_POINT ( 'NONE',  ( 6.433853624855537134, -1.958103210868083810, 0.4948410764434567066 ) ) ;
#193853 = CARTESIAN_POINT ( 'NONE',  ( -1.402160292154681736E-14, -0.1312499993171854229, -1.732050807568870754 ) ) ;
#193854 = CARTESIAN_POINT ( 'NONE',  ( 4.951972348128318657, 0.7275260799690360658, -2.190091995644850797 ) ) ;
#193855 = EDGE_CURVE ( 'NONE', #116214, #86356, #186780, .T. ) ;
#193856 = CARTESIAN_POINT ( 'NONE',  ( 1.481379835429663228, -0.05473030402166743219, 2.062018025990194126 ) ) ;
#193857 = CARTESIAN_POINT ( 'NONE',  ( 7.537970219518073556, 9.817384560903001045, -1.443375672974057666 ) ) ;
#193858 = CARTESIAN_POINT ( 'NONE',  ( 5.017399365509065845, 8.011327138806002779, -1.199719254218450271 ) ) ;
#193859 = CARTESIAN_POINT ( 'NONE',  ( 4.492547798081839794, 6.334668079219206049, 1.599625672291262513 ) ) ;
#193860 = CARTESIAN_POINT ( 'NONE',  ( -1.364683531250012516, 2.092708333674750953, 0.7879004041258379498 ) ) ;
#193861 = CARTESIAN_POINT ( 'NONE',  ( 4.228163802615382494, 6.026220084508304708, -1.599625672291269396 ) ) ;
#193862 = CARTESIAN_POINT ( 'NONE',  ( 5.843201017365476702, 6.879784610756938257, -1.082531754730543083 ) ) ;
#193863 = CARTESIAN_POINT ( 'NONE',  ( 3.842362351650536301, -1.073271228610745309, 1.887301499758537116 ) ) ;
#193864 = FACE_OUTER_BOUND ( 'NONE', #124539, .T. ) ;
#193866 = CARTESIAN_POINT ( 'NONE',  ( 4.546344060013487898, -1.475942220874026489, 1.100600019281534836 ) ) ;
#193865 = CARTESIAN_POINT ( 'NONE',  ( -3.145128448690317935, 5.652771709238564313, -1.082531754730549967 ) ) ;
#193868 = CARTESIAN_POINT ( 'NONE',  ( 6.720655732516652492, 7.053303974100803231, 2.424416723604695179 ) ) ;
#193867 = LINE ( 'NONE', #109504, #127310 ) ;
#193869 = CARTESIAN_POINT ( 'NONE',  ( 4.985950990042907094, -2.174969566330759996, -0.2684501861200879747 ) ) ;
#193870 = CARTESIAN_POINT ( 'NONE',  ( -11.92619526913700057, 19.00000000000000000, 1.328859060402684644 ) ) ;
#193871 = CARTESIAN_POINT ( 'NONE',  ( 5.577129106639307388, -0.04938619725537891220, -2.262140991306497373 ) ) ;
#193872 = ORIENTED_EDGE ( 'NONE', *, *, #187404, .F. ) ;
#193873 = CARTESIAN_POINT ( 'NONE',  ( -4.550628574872730425, 7.191434026324334816, -1.338276217581878980 ) ) ;
#193874 = CARTESIAN_POINT ( 'NONE',  ( -0.1108833634136781182, 7.629137130509072939, -2.496956624467902675 ) ) ;
#193875 = CARTESIAN_POINT ( 'NONE',  ( 4.895464504754282409, 8.144056917144915531, 1.010406422583273178 ) ) ;
#193876 = AXIS2_PLACEMENT_3D ( 'NONE', #32013, #49333, #27740 ) ;
#193877 = CARTESIAN_POINT ( 'NONE',  ( -6.766928066552171828, 7.067373297165212342, 0.7216878364870317197 ) ) ;
#193878 = CARTESIAN_POINT ( 'NONE',  ( 4.923019175537949543, 4.916146257648610352, 0.000000000000000000 ) ) ;
#193879 = CARTESIAN_POINT ( 'NONE',  ( 1.182078593147641632, -1.725526258793514067, -0.3928099155053321745 ) ) ;
#193880 = CARTESIAN_POINT ( 'NONE',  ( 5.514319586171100518, -2.013265972089046230, 0.002284521408187425995 ) ) ;
#193881 = CARTESIAN_POINT ( 'NONE',  ( 7.494959990256193194, 7.638541498254023843, -0.7998128361456281477 ) ) ;
#193882 = CARTESIAN_POINT ( 'NONE',  ( 4.243269300766455920, -1.833519874744583111, 1.035826785333898270 ) ) ;
#193883 = CARTESIAN_POINT ( 'NONE',  ( 2.073720586576404568, -0.8169873708120840572, 1.732773573125611088 ) ) ;
#193885 = EDGE_CURVE ( 'NONE', #200036, #85668, #27646, .T. ) ;
#193884 = CARTESIAN_POINT ( 'NONE',  ( 2.672928840188529609, 6.270167413528593414, 0.000000000000000000 ) ) ;
#193886 = CARTESIAN_POINT ( 'NONE',  ( 2.787508051956408384, -1.838732291863707236, 0.7063352763673010903 ) ) ;
#193887 = CARTESIAN_POINT ( 'NONE',  ( 5.133071871609922177, 1.867805937340912159, 0.7691607467245373808 ) ) ;
#193888 = CARTESIAN_POINT ( 'NONE',  ( 1.322894217037654085, -0.04941562205608432401, 1.870173573632450958 ) ) ;
#193891 = ORIENTED_EDGE ( 'NONE', *, *, #51475, .F. ) ;
#193890 = CARTESIAN_POINT ( 'NONE',  ( 1.511816067030671729, -0.6413169068853613597, 1.801808535584384252 ) ) ;
#193889 = CARTESIAN_POINT ( 'NONE',  ( 4.934089290906335634, 0.8825209879863432638, -1.481864930267517089 ) ) ;
#193893 = CARTESIAN_POINT ( 'NONE',  ( 4.446711195602238931, 6.210915699667823198, -1.443375672974051449 ) ) ;
#193892 = CARTESIAN_POINT ( 'NONE',  ( 1.629795212970772456, -2.077151576879713080, 0.7458654493318407352 ) ) ;
#193894 = CIRCLE ( 'NONE', #166218, 1.250000000000000222 ) ;
#193895 = CARTESIAN_POINT ( 'NONE',  ( 1.364683531249988757, 1.946875000341415030, 0.000000000000000000 ) ) ;
#193896 = CARTESIAN_POINT ( 'NONE',  ( 9.426996880203592610, 9.892584536526015881, -0.7998128361456281477 ) ) ;
#193897 = CARTESIAN_POINT ( 'NONE',  ( 6.825078400183573812, 0.002648415797040087893, 1.855566311045192540 ) ) ;
#193898 = DIRECTION ( 'NONE',  ( 0.000000000000000000, 1.000000000000000000, 0.000000000000000000 ) ) ;
#193899 = FACE_OUTER_BOUND ( 'NONE', #109610, .T. ) ;
#193900 = DIRECTION ( 'NONE',  ( 0.000000000000000000, 8.546850786086437571E-32, 1.000000000000000000 ) ) ;
#193901 = CARTESIAN_POINT ( 'NONE',  ( 0.9243811426856913815, 1.018911950503737174, 1.802186752163869699 ) ) ;
#193902 = CARTESIAN_POINT ( 'NONE',  ( -1.500000000000013101, 2.379166666666686414, -0.8660254037844313801 ) ) ;
#193903 = CARTESIAN_POINT ( 'NONE',  ( 5.015626762051672571, 7.938982758113895422, 1.199719254218462483 ) ) ;
#193904 = CARTESIAN_POINT ( 'NONE',  ( -6.353967546298838087, 10.56471257065732416, 0.000000000000000000 ) ) ;
#193905 = CARTESIAN_POINT ( 'NONE',  ( 4.740510986633625024, 5.559626234941203116, -1.199719254218450271 ) ) ;
#193907 = EDGE_CURVE ( 'NONE', #30509, #121309, #58529, .T. ) ;
#193906 = CARTESIAN_POINT ( 'NONE',  ( 6.551439628692993900, -1.894445571042557619, 0.9528467149547341641 ) ) ;
#193908 = CARTESIAN_POINT ( 'NONE',  ( 0.7500000000000006661, 10.44791666734946212, -1.299038105676657340 ) ) ;
#193909 = CARTESIAN_POINT ( 'NONE',  ( 1.364683531249988535, 3.155208333674756283, -0.7879004041258239610 ) ) ;
#193910 = EDGE_CURVE ( 'NONE', #90767, #171829, #6555, .T. ) ;
#193912 = CARTESIAN_POINT ( 'NONE',  ( 10.41229878561526512, 11.25002945941372623, -0.7216878364870257245 ) ) ;
#193911 = CARTESIAN_POINT ( 'NONE',  ( -0.4465194593918104249, 3.080450244942120719, -0.4155024747329819634 ) ) ;
#193913 = CARTESIAN_POINT ( 'NONE',  ( 4.411482401463855396, 0.5350073857553553358, 1.943773423102819864 ) ) ;
#193914 = CARTESIAN_POINT ( 'NONE',  ( 5.208173988833650903, 1.135812200204017630, -1.542565181195413526 ) ) ;
#193915 = CARTESIAN_POINT ( 'NONE',  ( 3.228257827484398490, 2.138632370135685523, 0.4780590757816546854 ) ) ;
#193916 = CARTESIAN_POINT ( 'NONE',  ( -1.997523430356386465, 3.481192892629605407, 0.4000000000002922329 ) ) ;
#193917 = CARTESIAN_POINT ( 'NONE',  ( -1.201851678989727383E-14, 0.9937500006828198229, 1.732050807568877637 ) ) ;
#193918 = CARTESIAN_POINT ( 'NONE',  ( 4.922139854824453487, -2.003099925734778797, 0.2017396019941309904 ) ) ;
#193919 = CARTESIAN_POINT ( 'NONE',  ( -6.124532705071231931, 8.168374127381657246, -1.599625672291263179 ) ) ;
#193921 = CARTESIAN_POINT ( 'NONE',  ( 5.941034585168498694, -1.816085283887830082, -1.088097372982429034 ) ) ;
#193920 = CARTESIAN_POINT ( 'NONE',  ( -4.297571505851936813, 4.116180966356429494, 1.214306433183764966E-14 ) ) ;
#193922 = CARTESIAN_POINT ( 'NONE',  ( -8.012344526598182026E-15, 9.109375000341398021, -1.575800808251669460 ) ) ;
#193924 = CARTESIAN_POINT ( 'NONE',  ( -7.228432174741334038, 8.462200954400218578, -1.199719254218452047 ) ) ;
#193923 = CARTESIAN_POINT ( 'NONE',  ( 3.773056988009905410, 1.967892522216899476, -0.7064651350525589235 ) ) ;
#193926 = ORIENTED_EDGE ( 'NONE', *, *, #200741, .T. ) ;
#193925 = CARTESIAN_POINT ( 'NONE',  ( 2.432253191915220825, 1.672178088080849223, 0.4220979471536658867 ) ) ;
#193927 = CARTESIAN_POINT ( 'NONE',  ( 4.816704082729271086, -0.7169179515637627009, -1.995842421597990413 ) ) ;
#193928 = CARTESIAN_POINT ( 'NONE',  ( 6.647575389402066826, 6.649926130590872120, 1.040834085586084257E-14 ) ) ;
#193929 = DIRECTION ( 'NONE',  ( -0.000000000000000000, -1.000000000000000000, -0.000000000000000000 ) ) ;
#193930 = CARTESIAN_POINT ( 'NONE',  ( 7.834948813061768824, -6.306565840633488129, 7.720982910012296863 ) ) ;
#193931 = DIRECTION ( 'NONE',  ( -0.7806247497998005658, 0.000000000000000000, -0.6249999999999988898 ) ) ;
#193932 = CARTESIAN_POINT ( 'NONE',  ( 6.979750152936881058, 7.037463354714830643, 0.7998128361456341429 ) ) ;
#193933 = EDGE_LOOP ( 'NONE', ( #177703, #44482, #163740, #95561 ) ) ;
#193934 = DIRECTION ( 'NONE',  ( 0.000000000000000000, 0.000000000000000000, 1.000000000000000000 ) ) ;
#193936 = CARTESIAN_POINT ( 'NONE',  ( 1.137045503269896285, -0.04498225810314023659, 1.811072777871777006 ) ) ;
#193935 = CARTESIAN_POINT ( 'NONE',  ( 6.150558962454855561, 7.204682206732687000, 1.199719254218452047 ) ) ;
#193937 = CARTESIAN_POINT ( 'NONE',  ( -6.905180308061733996, 6.950465202360470052, 0.7998128361456341429 ) ) ;
#193938 = ORIENTED_EDGE ( 'NONE', *, *, #1100, .T. ) ;
#193939 = CARTESIAN_POINT ( 'NONE',  ( 4.241003122976366058, 3.842258486427521103, -0.7998128361456211532 ) ) ;
#193940 = EDGE_LOOP ( 'NONE', ( #42974, #33722, #117935, #106248 ) ) ;
#193941 = CARTESIAN_POINT ( 'NONE',  ( 4.688087255275310561, 8.691461907788344377, -0.7998128361456381397 ) ) ;
#193942 = CARTESIAN_POINT ( 'NONE',  ( 3.228980503213836339, 1.638859372766150679, 0.7719998214037685491 ) ) ;
#193943 = CARTESIAN_POINT ( 'NONE',  ( 6.639320575229239019, 3.696696400505532942, 2.511109302898812956 ) ) ;
#193944 = CYLINDRICAL_SURFACE ( 'NONE', #429, 1.250000000000000000 ) ;
#193945 = CARTESIAN_POINT ( 'NONE',  ( 4.388421827844267042, 7.126904390760538277, 1.074283327121795528 ) ) ;
#193946 = ORIENTED_EDGE ( 'NONE', *, *, #109273, .T. ) ;
#193947 = CARTESIAN_POINT ( 'NONE',  ( 4.123391753781197266, 0.2291962677869363585, -1.846827494033479455 ) ) ;
#193948 = CARTESIAN_POINT ( 'NONE',  ( 1.388148191917773611, -0.6910900405009687830, -1.786773533054702545 ) ) ;
#193949 = CARTESIAN_POINT ( 'NONE',  ( 6.387721611049761883, 1.328912806184729734, 1.394852177740999233 ) ) ;
#193950 = CARTESIAN_POINT ( 'NONE',  ( 1.499999999999993117, 11.60416666666666607, 0.8660254037844408170 ) ) ;
#193951 = CARTESIAN_POINT ( 'NONE',  ( 4.612778539632031105, 8.351152097327862123, 0.2683542610703564812 ) ) ;
#193952 = CARTESIAN_POINT ( 'NONE',  ( -2.657034918598338180, 6.043698471765932112, -0.7216878364870267237 ) ) ;
#193953 = CARTESIAN_POINT ( 'NONE',  ( 7.998947442382716488, 9.394822106610419610, -1.082531754730543083 ) ) ;
#193954 = CARTESIAN_POINT ( 'NONE',  ( 6.034039001082764919, 1.170257472284089717, 1.583912470002272199 ) ) ;
#193955 = B_SPLINE_CURVE_WITH_KNOTS ( 'NONE', 3,
 ( #95237, #161286, #211073, #12872, #128857, #162357 ),
 .UNSPECIFIED., .F., .F.,
 ( 4, 2, 4 ),
 ( 0.8817142480080221167, 0.9367698396229139357, 0.9918254312378057547 ),
 .UNSPECIFIED. ) ;
#193956 = CARTESIAN_POINT ( 'NONE',  ( -4.066556009095094737, 6.831733546331167695, 1.199719254218464037 ) ) ;
#193957 = CARTESIAN_POINT ( 'NONE',  ( -9.499668754385638181, -7.246166700194470067, -0.07933194154487506478 ) ) ;
#193958 = CARTESIAN_POINT ( 'NONE',  ( 6.714806894218784628, -0.1628439675423892508, 2.155775914164249407 ) ) ;
#193959 = DIRECTION ( 'NONE',  ( 0.000000000000000000, 1.000000000000000000, 0.000000000000000000 ) ) ;
#193960 = CARTESIAN_POINT ( 'NONE',  ( 5.069325366411169931, 0.1891801624123757852, -1.917091172425288370 ) ) ;
#193961 = CARTESIAN_POINT ( 'NONE',  ( -6.856673000209188906, 9.022537805042615489, 1.599625672291283607 ) ) ;
#193962 = CARTESIAN_POINT ( 'NONE',  ( 1.658932825283397250, -1.563847321437005666, -0.9416461389453802955 ) ) ;
#193963 = CARTESIAN_POINT ( 'NONE',  ( 2.631697372267821855, -2.058793095894187353, 0.7952504953367269813 ) ) ;
#193964 = CARTESIAN_POINT ( 'NONE',  ( 0.08795244648929222142, 1.102731429460445334, 1.562230693318837238 ) ) ;
#193965 = ORIENTED_EDGE ( 'NONE', *, *, #182948, .T. ) ;
#193966 = CARTESIAN_POINT ( 'NONE',  ( 0.9417814284814338688, 1.320271805612409421, 1.461702747868667496 ) ) ;
#193967 = CARTESIAN_POINT ( 'NONE',  ( 2.577597507962032353, -0.9963960007246205342, 1.666827093504752222 ) ) ;
#193968 = EDGE_LOOP ( 'NONE', ( #42426, #21812, #138354, #39159 ) ) ;
#193969 = CARTESIAN_POINT ( 'NONE',  ( 1.388045824401448414, -0.05229234656609069859, 2.015604296821980057 ) ) ;
#193971 = CARTESIAN_POINT ( 'NONE',  ( 5.190230013454653069, 0.9586131782086585451, -1.594917819662385883 ) ) ;
#193970 = CARTESIAN_POINT ( 'NONE',  ( -6.493429226302317225, 6.540365283632955773, 0.7998128361456341429 ) ) ;
#193972 = CARTESIAN_POINT ( 'NONE',  ( 6.398522151006641678, 6.429640362454684954, 0.000000000000000000 ) ) ;
#193973 = PLANE ( 'NONE',  #101063 ) ;
#193974 = CARTESIAN_POINT ( 'NONE',  ( 1.426745631513068657, 7.396214564680185788, -4.272608017058045604 ) ) ;
#193975 = CARTESIAN_POINT ( 'NONE',  ( -4.055860508782465068, 7.883587693554856557, 1.040834085586084257E-14 ) ) ;
#193976 = CARTESIAN_POINT ( 'NONE',  ( -5.966470118465691641, 9.118576350588734059, -1.199719254218452047 ) ) ;
#193977 = CARTESIAN_POINT ( 'NONE',  ( 0.9432342461353732110, -1.730868645791438842, -1.344178957308760802 ) ) ;
#193978 = CARTESIAN_POINT ( 'NONE',  ( 2.562127843302666186, 5.932973550587659517, 0.000000000000000000 ) ) ;
#193979 = CARTESIAN_POINT ( 'NONE',  ( -6.966220764712148572, 6.002124920821316323, 2.420000000000000373 ) ) ;
#193980 = LINE ( 'NONE', #213413, #13207 ) ;
#193981 = CARTESIAN_POINT ( 'NONE',  ( 3.193790821891542731, -0.7392406677243367197, 1.669511829839696260 ) ) ;
#193982 = CARTESIAN_POINT ( 'NONE',  ( -2.137381772448751605, 5.645362501165475777, -0.7998128361456281477 ) ) ;
#193983 = CARTESIAN_POINT ( 'NONE',  ( -3.093231602212184850, 6.760520635889515795, -0.7998128361456281477 ) ) ;
#193984 = CARTESIAN_POINT ( 'NONE',  ( -5.946407990378149933, 7.222024315256661886, -1.239984355232233826 ) ) ;
#193985 = CARTESIAN_POINT ( 'NONE',  ( 6.609000000000029296, 3.690475914267136837, 2.614198802211770367 ) ) ;
#193986 = CARTESIAN_POINT ( 'NONE',  ( 9.901532256681887745, 10.44620914241737530, 0.000000000000000000 ) ) ;
#193987 = CARTESIAN_POINT ( 'NONE',  ( 1.436025505276457226, 0.9502256629446425018, -1.675776081635256043 ) ) ;
#193988 = CARTESIAN_POINT ( 'NONE',  ( 5.137533780887935997, 1.831872034461759835, -0.7024582609849658876 ) ) ;
#193989 = CARTESIAN_POINT ( 'NONE',  ( -7.389357414647957256, 8.579670724299436557, 1.199719254218450271 ) ) ;
#193990 = CARTESIAN_POINT ( 'NONE',  ( 4.798696304233017074, 7.685897223992134819, -1.199719254218452047 ) ) ;
#193991 = CARTESIAN_POINT ( 'NONE',  ( 4.687173145698103838, 1.624054394666199830, 1.471728111018810070 ) ) ;
#193992 = VECTOR ( 'NONE', #192954, 1000.000000000000114 ) ;
#193993 = CARTESIAN_POINT ( 'NONE',  ( 3.985207087413062066, 6.736826471035503694, -1.199719254218452047 ) ) ;
#193994 = CARTESIAN_POINT ( 'NONE',  ( 4.170806909802426965, 1.467596682293986765, -1.460439952253207663 ) ) ;
#193996 = CARTESIAN_POINT ( 'NONE',  ( 0.6823417656249899377, 1.155208333674752286, 1.181850606188755259 ) ) ;
#193995 = SPHERICAL_SURFACE ( 'NONE', #68546, 0.08000000000000000167 ) ;
#193997 = EDGE_LOOP ( 'NONE', ( #34692, #161255, #183447, #75015 ) ) ;
#193998 = CARTESIAN_POINT ( 'NONE',  ( 3.973462176510922816, -2.273730406356341049, -0.3370867821424743949 ) ) ;
#194000 = EDGE_LOOP ( 'NONE', ( #139926, #79705, #6536, #158860, #180377 ) ) ;
#193999 = CARTESIAN_POINT ( 'NONE',  ( 8.297226821883377568, 8.782445501726501291, -0.7216878364870267237 ) ) ;
#194002 = CARTESIAN_POINT ( 'NONE',  ( -1.642778471875000035, -0.8677083328553769626, -2.845375778867859751 ) ) ;
#194001 = CARTESIAN_POINT ( 'NONE',  ( 6.563555762791525972, 6.830105609444471426, -0.7216878364870458196 ) ) ;
#194003 = CARTESIAN_POINT ( 'NONE',  ( -7.573156686838094842, -5.230039540835550227, -7.978162878861462914 ) ) ;
#194004 = DIRECTION ( 'NONE',  ( 4.107825191113088666E-15, 4.274358644806862147E-15, 1.000000000000000000 ) ) ;
#194005 = CARTESIAN_POINT ( 'NONE',  ( 3.345582828684705134, 1.942124712213384452, -0.0007862604347076693808 ) ) ;
#194006 = ORIENTED_EDGE ( 'NONE', *, *, #63060, .F. ) ;
#194007 = CARTESIAN_POINT ( 'NONE',  ( 9.151390499099949949, 12.66007743471656788, -1.082531754730543971 ) ) ;
#194008 = ORIENTED_EDGE ( 'NONE', *, *, #35341, .F. ) ;
#194009 = CARTESIAN_POINT ( 'NONE',  ( 5.045129621168108258, 0.1466893748028277877, 1.906852434080000824 ) ) ;
#194010 = CARTESIAN_POINT ( 'NONE',  ( -4.207966135563093957, 7.175396087857926375, 1.072179110320391260 ) ) ;
#194011 = CARTESIAN_POINT ( 'NONE',  ( 6.229511965242640059, -1.622199917339474329, 0.5863599495292673991 ) ) ;
#194012 = CARTESIAN_POINT ( 'NONE',  ( 4.962125165302472496, -1.116212726388360998, 1.679221540125563905 ) ) ;
#194013 = CARTESIAN_POINT ( 'NONE',  ( 1.499999999999996891, 11.14583333333333215, -0.8660254037844378194 ) ) ;
#194014 = CARTESIAN_POINT ( 'NONE',  ( 2.403190426070573871, 1.771669130372434564, -1.315670724662293178 ) ) ;
#194016 = CARTESIAN_POINT ( 'NONE',  ( -5.004368097219957789, 5.011053332944274352, 0.000000000000000000 ) ) ;
#194015 = CARTESIAN_POINT ( 'NONE',  ( -9.938290294017125603, 11.55342575023019691, -1.199719254218441611 ) ) ;
#194018 = CARTESIAN_POINT ( 'NONE',  ( 0.1800360811037614583, -1.714963048871451790, -0.4369287763777151556 ) ) ;
#194017 = CARTESIAN_POINT ( 'NONE',  ( 1.640690513341718670, -1.765443103004183056, 1.119499978516135252 ) ) ;
#194019 = CARTESIAN_POINT ( 'NONE',  ( 5.643203987388664800, 0.8197706014990979728, 1.842448445624145226 ) ) ;
#194021 = CARTESIAN_POINT ( 'NONE',  ( 3.258078344973667662, 1.030780755083884115, 2.047500790377681845 ) ) ;
#194020 = CARTESIAN_POINT ( 'NONE',  ( 6.235824307642648279, 6.239826211863360506, 0.000000000000000000 ) ) ;
#194022 = CARTESIAN_POINT ( 'NONE',  ( 1.200653373194009443, -0.4260525342448440722, 1.687239105062097400 ) ) ;
#194023 = AXIS2_PLACEMENT_3D ( 'NONE', #84155, #2876, #5008 ) ;
#194024 = CARTESIAN_POINT ( 'NONE',  ( 11.91826849282518275, 10.89999999999999858, -1.400000000000001465 ) ) ;
#194025 = CARTESIAN_POINT ( 'NONE',  ( 0.7371068013607602332, -1.629765380930665364, -0.5920680523868580014 ) ) ;
#194026 = CARTESIAN_POINT ( 'NONE',  ( 0.6801582343750056658, 0.5885416670080856338, -1.178068619123862515 ) ) ;
#194027 = CARTESIAN_POINT ( 'NONE',  ( -11.95359438122011042, 13.60421899708702753, -1.059536798430454008 ) ) ;
#194028 = CARTESIAN_POINT ( 'NONE',  ( 1.610090671168771470, 0.6309225058772853778, -2.077463247357013820 ) ) ;
#194029 = CARTESIAN_POINT ( 'NONE',  ( 1.991423064788412800, -0.4370762659771566527, 1.968445590580846893 ) ) ;
#194030 = CARTESIAN_POINT ( 'NONE',  ( 4.375000000000001776, 2.052068128417944504, -2.491713675105573160E-13 ) ) ;
#194031 = CARTESIAN_POINT ( 'NONE',  ( 0.7499999999999902300, 1.514583334016148086, 1.299038105676657340 ) ) ;
#194032 = CARTESIAN_POINT ( 'NONE',  ( 0.4109946218407485308, 1.674316264148696165, 0.9526004100348076653 ) ) ;
#194033 = CARTESIAN_POINT ( 'NONE',  ( 1.364683531249996529, 13.46354166700806765, 0.7879004041258405033 ) ) ;
#194034 = CARTESIAN_POINT ( 'NONE',  ( 2.865722905416301369, -1.818493784693291815, -1.275605581943892730 ) ) ;
#194035 = EDGE_LOOP ( 'NONE', ( #88880, #129331, #115041, #173883 ) ) ;
#194036 = FACE_OUTER_BOUND ( 'NONE', #85917, .T. ) ;
#194037 = CARTESIAN_POINT ( 'NONE',  ( 1.499999999999987121, -0.4958333333333110882, 0.8660254037844524744 ) ) ;
#194038 = CARTESIAN_POINT ( 'NONE',  ( 9.088043039861931405, 9.497138389460751284, 1.040834085586084257E-14 ) ) ;
#194039 = CARTESIAN_POINT ( 'NONE',  ( 5.987833318177087527, -1.732952516383274855, -0.1613439405771869561 ) ) ;
#194041 = CARTESIAN_POINT ( 'NONE',  ( 3.912515228517557286, 0.7039278570535618673, 1.831416474553926310 ) ) ;
#194040 = COLOUR_RGB ( '', 0.66274510, 0.83137255, 0.94901961) ;
#194043 = CARTESIAN_POINT ( 'NONE',  ( -6.290620087060847965, 7.401773525401500464, 1.082531754730549967 ) ) ;
#194042 = CARTESIAN_POINT ( 'NONE',  ( 4.546061579283848353, 4.198160018786257552, -0.7998128361456211532 ) ) ;
#194044 = EDGE_CURVE ( 'NONE', #127188, #62746, #23878, .T. ) ;
#194045 = DIRECTION ( 'NONE',  ( -1.000000000000000000, 0.000000000000000000, 0.000000000000000000 ) ) ;
#194046 = CARTESIAN_POINT ( 'NONE',  ( 4.270984383450874944, -2.108973115933824527, -0.8193970387949424117 ) ) ;
#194047 = CARTESIAN_POINT ( 'NONE',  ( 2.260285141513069362, -2.062262451202213853, 0.04833688706953364472 ) ) ;
#194048 = CARTESIAN_POINT ( 'NONE',  ( -6.880926654135487652, 7.986501503701545879, 1.199719254218450271 ) ) ;
#194049 = EDGE_LOOP ( 'NONE', ( #44407, #70370 ) ) ;
#194050 = CARTESIAN_POINT ( 'NONE',  ( 0.7499999999999885647, 0.7645833340161543035, 1.299038105676657340 ) ) ;
#194051 = CARTESIAN_POINT ( 'NONE',  ( 3.813614929637610285, -1.843318686535614148, 0.3169883347873064250 ) ) ;
#194052 = CARTESIAN_POINT ( 'NONE',  ( 2.883173651945786009, -0.5064310303744267161, -1.658517218374066848 ) ) ;
#194053 = CARTESIAN_POINT ( 'NONE',  ( 6.128506746050899068, 0.2130254606748181456, 2.181202035047181020 ) ) ;
#194054 = CARTESIAN_POINT ( 'NONE',  ( 6.686558038528344738, -2.261219263861591333, -0.4595595737692282912 ) ) ;
#194055 = CARTESIAN_POINT ( 'NONE',  ( 4.118171802502921253, -1.108985364570359566, -1.855417305202881506 ) ) ;
#194056 = CARTESIAN_POINT ( 'NONE',  ( 4.119036135373352003, -1.858019016064060169, 0.5647323716678387395 ) ) ;
#194057 = CARTESIAN_POINT ( 'NONE',  ( -4.758548728272219641, 4.653987725846768342, 0.7216878364870317197 ) ) ;
#194058 = CARTESIAN_POINT ( 'NONE',  ( 6.538356921592370696, 1.850225872366148883, 0.2742375073267953045 ) ) ;
#194059 = SURFACE_STYLE_USAGE ( .BOTH. , #27292 ) ;
#194060 = CARTESIAN_POINT ( 'NONE',  ( 4.352817808933668431, 7.164511876539561896, 1.041257065902738477 ) ) ;
#194061 = DIRECTION ( 'NONE',  ( -0.000000000000000000, -1.000000000000000000, -0.000000000000000000 ) ) ;
#194062 = CARTESIAN_POINT ( 'NONE',  ( 0.1234922912959918878, 1.848187084301698757, 1.039613981531524400 ) ) ;
#194063 = CARTESIAN_POINT ( 'NONE',  ( 1.360316468749985797, 2.036458333674739940, -0.7853790794159022370 ) ) ;
#194064 = CARTESIAN_POINT ( 'NONE',  ( 5.783827325522512552, 1.646840809264274119, -1.163266671679111353 ) ) ;
#194065 = CARTESIAN_POINT ( 'NONE',  ( -3.429849674132948500, 5.024577257953626308, -1.443375672974051449 ) ) ;
#194066 = CARTESIAN_POINT ( 'NONE',  ( 6.771407655021410399, 9.987393799911945536, -1.199719254218441611 ) ) ;
#194067 = PLANE ( 'NONE',  #74188 ) ;
#194068 = CARTESIAN_POINT ( 'NONE',  ( 3.404746562951189937, 1.438594061741470753, -1.123979961188771304 ) ) ;
#194069 = CARTESIAN_POINT ( 'NONE',  ( 2.591098708763440062, -0.3764507303484417311, -2.174265822884546395 ) ) ;
#194070 = ORIENTED_EDGE ( 'NONE', *, *, #67908, .T. ) ;
#194071 = CARTESIAN_POINT ( 'NONE',  ( -4.123088111887291518, 7.824370207261548416, 0.000000000000000000 ) ) ;
#194072 = DIRECTION ( 'NONE',  ( -0.9992060137953822085, -9.538978360076122062E-16, -0.03984146075563014394 ) ) ;
#194073 = CARTESIAN_POINT ( 'NONE',  ( -8.857554428429624593, 9.228235009456373206, 0.7998128361456462443 ) ) ;
#194074 = CARTESIAN_POINT ( 'NONE',  ( 0.7912781446984231692, -0.05379174966265751895, -2.019256707098691095 ) ) ;
#194075 = CARTESIAN_POINT ( 'NONE',  ( 1.594549238318817785, -1.131586138893545979, 1.793127659086241499 ) ) ;
#194076 = EDGE_CURVE ( 'NONE', #24478, #161735, #153438, .T. ) ;
#194077 = ORIENTED_EDGE ( 'NONE', *, *, #165318, .T. ) ;
#194078 = CARTESIAN_POINT ( 'NONE',  ( -6.798487682609798632, 6.896266815991691779, 0.7998128361456341429 ) ) ;
#194079 = CARTESIAN_POINT ( 'NONE',  ( 1.902945097309636013, -1.575467964945817867, 0.9901336090045903537 ) ) ;
#194080 = CARTESIAN_POINT ( 'NONE',  ( 3.520313441042647540, 7.258782781191745137, 0.7998128361456321445 ) ) ;
#194081 = CARTESIAN_POINT ( 'NONE',  ( 5.928604924596339032, 1.985460353506541376, 0.5521678710885301600 ) ) ;
#194082 = CARTESIAN_POINT ( 'NONE',  ( 5.678361341766085424, 1.528739221709461082, 1.314999087022615587 ) ) ;
#194083 = EDGE_LOOP ( 'NONE', ( #93038, #12517, #2055, #37301, #199934, #182007, #28530, #182634, #178935, #22071, #10467, #54240, #197745, #83180, #8914, #184981, #101399, #167607 ) ) ;
#194084 = VERTEX_POINT ( 'NONE', #7624 ) ;
#194085 = ORIENTED_EDGE ( 'NONE', *, *, #94666, .F. ) ;
#194086 =( BOUNDED_CURVE ( )  B_SPLINE_CURVE ( 3, ( #90319, #6896, #59940, #189938 ),
 .UNSPECIFIED., .F., .T. ) 
 B_SPLINE_CURVE_WITH_KNOTS ( ( 4, 4 ),
 ( 0.000000000000000000, 0.4999999999999984457 ),
 .UNSPECIFIED. ) 
 CURVE ( )  GEOMETRIC_REPRESENTATION_ITEM ( )  RATIONAL_B_SPLINE_CURVE ( ( 1.000000000000000000, 0.3333333333333354243, 0.3333333333333333703, 0.9999999999999978906 ) ) 
 REPRESENTATION_ITEM ( '' )  );
#194087 = PRODUCT_DEFINITION_FORMATION_WITH_SPECIFIED_SOURCE ( 'ANY', '', #121435, .NOT_KNOWN. ) ;
#194088 = CARTESIAN_POINT ( 'NONE',  ( 0.04469154961657068048, 6.488258805693589260, -3.101144068366980200 ) ) ;
#194089 = CARTESIAN_POINT ( 'NONE',  ( 3.650846181029033133, -1.491723252493650564, 1.052289205326197852 ) ) ;
#194091 = CARTESIAN_POINT ( 'NONE',  ( -5.657660137730037953, 6.307591819868396676, -1.155748867827746995 ) ) ;
#194090 = CARTESIAN_POINT ( 'NONE',  ( -4.468294144155606773, 7.370704380560280100, 1.199719254218452935 ) ) ;
#194092 = CARTESIAN_POINT ( 'NONE',  ( 5.275877007301786215, 7.772378248882220397, 1.293907329011657614 ) ) ;
#194093 = CARTESIAN_POINT ( 'NONE',  ( 6.239611212763971793, -1.913511330438378177, -0.6350998681113121380 ) ) ;
#194094 = CARTESIAN_POINT ( 'NONE',  ( 5.595603887632320195, -1.841320590885606068, 0.004091980732826016286 ) ) ;
#194095 = CIRCLE ( 'NONE', #166418, 0.08000000000000041800 ) ;
#194096 = CARTESIAN_POINT ( 'NONE',  ( 0.07700591528351108384, 2.887024434135841755, -2.399578936219012082 ) ) ;
#194097 = CARTESIAN_POINT ( 'NONE',  ( 3.967613463194498813, 0.2842429903056520324, -2.290057832888813483 ) ) ;
#194098 = CARTESIAN_POINT ( 'NONE',  ( 5.285699784481295183, 7.260012063351913625, 1.599625672291268286 ) ) ;
#194099 = CARTESIAN_POINT ( 'NONE',  ( 6.239563118392394969, -1.560868990211834895, -1.495623836407403262 ) ) ;
#194100 = CARTESIAN_POINT ( 'NONE',  ( 5.459129407796876166, 9.520734742405036144, 1.040834085586084257E-14 ) ) ;
#194101 = CARTESIAN_POINT ( 'NONE',  ( 0.6439600106935819968, 0.5648315236305987419, 1.858087668232853984 ) ) ;
#194102 = VERTEX_POINT ( 'NONE', #89984 ) ;
#194103 = CARTESIAN_POINT ( 'NONE',  ( 4.323764262282871584, -1.706850429308865547, 1.539420282360188574 ) ) ;
#194104 = PLANE ( 'NONE',  #144922 ) ;
#194105 = CARTESIAN_POINT ( 'NONE',  ( -4.625266680917477835, 5.425174544939014964, -1.199719254218453823 ) ) ;
#194106 = CARTESIAN_POINT ( 'NONE',  ( 5.032044620589739559, 0.9611010790777809731, -1.604743002217932313 ) ) ;
#194109 = CARTESIAN_POINT ( 'NONE',  ( -4.261005416444848315, 8.193199762486115034, 0.7998128361456352531 ) ) ;
#194108 = CARTESIAN_POINT ( 'NONE',  ( -1.402160292154681736E-14, 0.2437500006828163535, 1.732050807568877637 ) ) ;
#194107 = CARTESIAN_POINT ( 'NONE',  ( 1.986440140746603911, -1.173720106059353396, 1.509789020923378189 ) ) ;
#194110 = CARTESIAN_POINT ( 'NONE',  ( 3.387540773601561916, 1.995160029947869340, -0.9435142334218297178 ) ) ;
#194111 = CARTESIAN_POINT ( 'NONE',  ( 6.983263157960402090, 0.5904152146812295943, 1.899285251901380089 ) ) ;
#194112 = CARTESIAN_POINT ( 'NONE',  ( 2.866659414285625651, 5.431854185720147221, -1.199719254218446718 ) ) ;
#194113 = CARTESIAN_POINT ( 'NONE',  ( 5.302647476276220573, 8.240153584747313076, -1.082531754730548412 ) ) ;
#194114 = CARTESIAN_POINT ( 'NONE',  ( -9.429859533504656000, 10.96025652963230534, -1.199719254218441611 ) ) ;
#194115 = CARTESIAN_POINT ( 'NONE',  ( -5.438229012412890917, 8.398332043573416783, -1.082531754730549967 ) ) ;
#194116 = CARTESIAN_POINT ( 'NONE',  ( 1.176956626245349247, -0.04423564266526488348, -1.971012800895243888 ) ) ;
#194117 = CARTESIAN_POINT ( 'NONE',  ( 1.009288123910282442, 1.745381235414251275, -1.509623180311530977 ) ) ;
#194119 = EDGE_CURVE ( 'NONE', #211538, #183045, #57468, .T. ) ;
#194118 = CARTESIAN_POINT ( 'NONE',  ( 2.523818479427087702, 1.924573107942130656, -0.3798230296482503210 ) ) ;
#194120 = CARTESIAN_POINT ( 'NONE',  ( 11.52469724861194678, 11.37999993351184891, 3.346365485506860526 ) ) ;
#194121 = CARTESIAN_POINT ( 'NONE',  ( 4.803617054199708747, -1.591134784341166508, -1.312391874486463550 ) ) ;
#194122 = CARTESIAN_POINT ( 'NONE',  ( 4.039966587192250103, 7.657118751792200584, 0.7216878364870298324 ) ) ;
#194123 = CARTESIAN_POINT ( 'NONE',  ( 4.529305835417093640, 7.441884687032027657, -1.199719254218450271 ) ) ;
#194124 = ORIENTED_EDGE ( 'NONE', *, *, #195348, .T. ) ;
#194125 = FACE_OUTER_BOUND ( 'NONE', #91726, .T. ) ;
#194126 = CARTESIAN_POINT ( 'NONE',  ( 10.91970695577495043, -6.134628647623513231, 5.204170427930421283E-15 ) ) ;
#194127 = CARTESIAN_POINT ( 'NONE',  ( 3.348500752450942031, 4.929670182657964084, 1.443375672974066548 ) ) ;
#194128 = B_SPLINE_CURVE_WITH_KNOTS ( 'NONE', 3,
 ( #174, #134515, #30599, #65189, #146499, #14307, #166990, #133451, #182143, #199456, #80402, #130300, #1250, #117224, #114047, #213567, #97740, #115098, #197338, #196288, #33774, #131343, #212516, #15375, #17500, #66241, #83587, #149669, #48979, #132390, #200519, #64158, #181094, #32711 ),
 .UNSPECIFIED., .F., .F.,
 ( 4, 2, 2, 2, 2, 2, 2, 2, 2, 2, 2, 2, 2, 2, 2, 2, 4 ),
 ( 0.009372056057571971632, 0.009929098612377838459, 0.01048614116718370702, 0.01104318372198957385, 0.01160022627679544241, 0.01215726883160131097, 0.01271431138640717953, 0.01327135394121304636, 0.01382839649601891319, 0.01438543905082478175, 0.01494248160563065031, 0.01549952416043651714, 0.01605656671524238396, 0.01661360927004825253, 0.01717065182485411762, 0.01772769437965998618, 0.01828473693446585127 ),
 .UNSPECIFIED. ) ;
#194129 = CARTESIAN_POINT ( 'NONE',  ( 1.129994725911891207, 2.092989821048664822, -0.5768834896340956364 ) ) ;
#194130 = CARTESIAN_POINT ( 'NONE',  ( 5.716698046817569434, 6.698511138489155137, -1.199719254218452047 ) ) ;
#194131 = DIRECTION ( 'NONE',  ( 0.000000000000000000, 1.000000000000000000, 0.000000000000000000 ) ) ;
#194132 = CARTESIAN_POINT ( 'NONE',  ( -1.833030277982346634, 2.531131934864056632, -2.499999999999998668 ) ) ;
#194133 = CARTESIAN_POINT ( 'NONE',  ( 2.442468673064964957, 0.4055347385497136137, 1.825902681341363021 ) ) ;
#194134 = CARTESIAN_POINT ( 'NONE',  ( 0.1751657365761209451, 0.002452341591326848407, -2.044164811867712483 ) ) ;
#194136 = SURFACE_STYLE_FILL_AREA ( #142228 ) ;
#194135 = CARTESIAN_POINT ( 'NONE',  ( -11.44791656467458552, 13.79999999999999716, -3.303228920649581291 ) ) ;
#194137 = CARTESIAN_POINT ( 'NONE',  ( -1.364683531250000748, -0.4906249996585801409, 0.000000000000000000 ) ) ;
#194138 = EDGE_CURVE ( 'NONE', #102754, #179825, #173366, .T. ) ;
#194139 = CARTESIAN_POINT ( 'NONE',  ( 2.631394046745598736, -0.1854624247320437180, 1.903247139735386284 ) ) ;
#194140 = CARTESIAN_POINT ( 'NONE',  ( 4.082668839255446436, -0.1736907016443404450, -1.761279006307460371 ) ) ;
#194141 = CARTESIAN_POINT ( 'NONE',  ( 2.279812546382542493, 1.875032136476075584, -0.3747091278499328770 ) ) ;
#194142 = CARTESIAN_POINT ( 'NONE',  ( -6.552668314106420588, 6.539201209412602189, -0.7998128361456291469 ) ) ;
#194144 = CARTESIAN_POINT ( 'NONE',  ( 5.835529424904522422, 0.5513129833306378291, -1.834571867064521022 ) ) ;
#194143 = CARTESIAN_POINT ( 'NONE',  ( 1.499999999999959588, 7.000000000000000000, -10.89724735885168805 ) ) ;
#194145 = CARTESIAN_POINT ( 'NONE',  ( -1.402160292154681736E-14, -0.7874999999999764411, 1.732050807568877637 ) ) ;
#194146 = CARTESIAN_POINT ( 'NONE',  ( 6.426221551499647688, 1.011104814135417751, 1.690039303870519705 ) ) ;
#194147 = CARTESIAN_POINT ( 'NONE',  ( 0.6823417656249882723, -0.5947916663252492686, 1.181850606188755259 ) ) ;
#194148 =( LENGTH_UNIT ( ) NAMED_UNIT ( * ) SI_UNIT ( .MILLI., .METRE. ) );
#194149 = CARTESIAN_POINT ( 'NONE',  ( 5.137510444216992767, -1.323429205136433140, -1.322332877454430955 ) ) ;
#194151 = EDGE_LOOP ( 'NONE', ( #33861, #74672, #73935, #108045 ) ) ;
#194150 = CARTESIAN_POINT ( 'NONE',  ( 1.769861954154128725, 0.9373860217288846330, 1.566528536362868707 ) ) ;
#194153 = CARTESIAN_POINT ( 'NONE',  ( 4.666668778386947380, 8.284408874816399759, 0.5204741841226891985 ) ) ;
#194152 = CARTESIAN_POINT ( 'NONE',  ( 4.389439674793148782, 1.972019932058775016, -0.9908447712502415072 ) ) ;
#194154 = CARTESIAN_POINT ( 'NONE',  ( 1.364683531249988757, -0.8656249996585805295, 0.000000000000000000 ) ) ;
#194155 = CARTESIAN_POINT ( 'NONE',  ( 2.277848244636628827, -2.001361501815647870, 0.4987805053587587856 ) ) ;
#194156 = CARTESIAN_POINT ( 'NONE',  ( 6.419949431270806528, 7.448694743692793274, 1.199719254218462483 ) ) ;
#194157 = CARTESIAN_POINT ( 'NONE',  ( -8.528242318195895066, 9.908369778438709474, 1.199719254218462483 ) ) ;
#194158 = SURFACE_STYLE_USAGE ( .BOTH. , #13277 ) ;
#194159 = CARTESIAN_POINT ( 'NONE',  ( 1.355680771150860275, 3.935647470828122607, -0.6419739358886640268 ) ) ;
#194160 = TOROIDAL_SURFACE ( 'NONE', #114745, 6.399999999999999467, 0.2000000000000000111 ) ;
#194161 = FILL_AREA_STYLE_COLOUR ( '', #40925 ) ;
#194162 = CARTESIAN_POINT ( 'NONE',  ( 7.191674137406095291, 7.354984346587396082, 0.000000000000000000 ) ) ;
#194163 = EDGE_LOOP ( 'NONE', ( #13115, #97540, #165897, #168093 ) ) ;
#194164 = CARTESIAN_POINT ( 'NONE',  ( 5.811005889236001032, -1.634438611397070806, 1.270752202701043609 ) ) ;
#194165 = CARTESIAN_POINT ( 'NONE',  ( 1.364683531249988757, -0.8031249996585804185, 0.000000000000000000 ) ) ;
#194166 = CARTESIAN_POINT ( 'NONE',  ( 2.583474834239877449, 1.977432880963815309, -0.8734481387390122809 ) ) ;
#194167 = CARTESIAN_POINT ( 'NONE',  ( -5.050372967203840879, 7.883769262350217133, 1.105620360010154402 ) ) ;
#194169 = EDGE_CURVE ( 'NONE', #28052, #148211, #91957, .T. ) ;
#194168 = CARTESIAN_POINT ( 'NONE',  ( 3.492836188673923647, -1.947007740449010926, -0.5366636104956448161 ) ) ;
#194170 = CARTESIAN_POINT ( 'NONE',  ( 6.620655732516668834, 6.034240673559561507, 2.768629221164942145 ) ) ;
#194171 = PRODUCT_DEFINITION_SHAPE ( 'NONE', 'NONE',  #189422 ) ;
#194172 = ADVANCED_FACE ( 'NONE', ( #40155 ), #6754, .T. ) ;
#194174 = CARTESIAN_POINT ( 'NONE',  ( 7.971831135155394321, 8.402817200543854170, -0.7216878364870267237 ) ) ;
#194173 = CARTESIAN_POINT ( 'NONE',  ( 3.475000000000000533, -0.8750000000000007772, 0.000000000000000000 ) ) ;
#194175 = CARTESIAN_POINT ( 'NONE',  ( -7.095713291905736853, 9.371694488680407886, 1.599625672291269396 ) ) ;
#194176 = CARTESIAN_POINT ( 'NONE',  ( 1.235564962061060257, 0.5807501988173838781, -1.931125984888550473 ) ) ;
#194177 = CARTESIAN_POINT ( 'NONE',  ( 5.601184584505256581, -0.5335315006234629953, 2.125516261704554211 ) ) ;
#194178 = CARTESIAN_POINT ( 'NONE',  ( -0.7499999999999972244, 4.139583334016149863, -1.299038105676652899 ) ) ;
#194179 = CARTESIAN_POINT ( 'NONE',  ( 4.605663860560767375, 1.420894170025093439, 1.280184534114735095 ) ) ;
#194180 = CARTESIAN_POINT ( 'NONE',  ( -2.903417451620861289, 6.539070793532962611, 0.7998128361456341429 ) ) ;
#194181 = CARTESIAN_POINT ( 'NONE',  ( 6.195713011320782115, 8.251417818006149929, -1.443375672974057666 ) ) ;
#194183 = CARTESIAN_POINT ( 'NONE',  ( 3.603138812553498216, -0.1455146663824242736, 2.011206757212272933 ) ) ;
#194182 = CARTESIAN_POINT ( 'NONE',  ( -8.880227426826648340, 11.38335130276301754, 1.443375672974064550 ) ) ;
#194184 = CARTESIAN_POINT ( 'NONE',  ( -1.364683531250010295, 13.19270833367472839, 0.7879004041258445001 ) ) ;
#194185 = B_SPLINE_CURVE_WITH_KNOTS ( 'NONE', 3,
 ( #199236, #201366, #150532, #99633, #117006, #35686, #183005, #151595, #181930, #67096, #18366, #118080, #33561, #133232, #84443, #36749 ),
 .UNSPECIFIED., .F., .F.,
 ( 4, 2, 2, 2, 2, 2, 2, 4 ),
 ( 0.000000000000000000, 0.0005357556996629550235, 0.001071511399325910047, 0.001607267098988864962, 0.002143022798651820094, 0.003214534197977728189, 0.003750289897640680069, 0.004286045597303632382 ),
 .UNSPECIFIED. ) ;
#194186 = CARTESIAN_POINT ( 'NONE',  ( -5.164730172163054966, 4.990216387137135889, -0.7998128361456362523 ) ) ;
#194187 = CARTESIAN_POINT ( 'NONE',  ( 5.192313411850084215, -1.712133481052197093, -0.2078965086465163203 ) ) ;
#194188 = CARTESIAN_POINT ( 'NONE',  ( 3.979481780810941949, 4.601482484822914998, 1.199719254218464037 ) ) ;
#194189 =( GEOMETRIC_REPRESENTATION_CONTEXT ( 3 ) GLOBAL_UNCERTAINTY_ASSIGNED_CONTEXT ( ( #150171 ) ) GLOBAL_UNIT_ASSIGNED_CONTEXT ( ( #7069, #3861, #136046 ) ) REPRESENTATION_CONTEXT ( 'NONE', 'WORKASPACE' ) );
#194190 = CARTESIAN_POINT ( 'NONE',  ( -5.608135385276092677, 5.599224824533729716, 0.4022279080854191391 ) ) ;
#194191 = CARTESIAN_POINT ( 'NONE',  ( 3.408985558832261731, 6.064568021024562938, 1.199719254218462483 ) ) ;
#194192 = DIRECTION ( 'NONE',  ( -0.9829311923673912377, -0.1839735607939864959, 0.000000000000000000 ) ) ;
#194193 = CARTESIAN_POINT ( 'NONE',  ( 0.7782871991188352601, -1.104406889285912907, -1.750870654829151274 ) ) ;
#194194 = CARTESIAN_POINT ( 'NONE',  ( -11.48788097203293823, 12.26956945602307947, 3.469500700354829714 ) ) ;
#194195 = ORIENTED_EDGE ( 'NONE', *, *, #21454, .T. ) ;
#194196 = CARTESIAN_POINT ( 'NONE',  ( 5.391193890671133637, -0.05051413884850668168, -1.810949582550380521 ) ) ;
#194197 = CARTESIAN_POINT ( 'NONE',  ( 4.179656494762836516, 8.098292687190454586, -0.7998128361456362523 ) ) ;
#194198 = DIRECTION ( 'NONE',  ( 0.000000000000000000, 0.000000000000000000, -1.000000000000000000 ) ) ;
#194199 = CARTESIAN_POINT ( 'NONE',  ( 5.900986446306966116, -0.2725449506757338658, -1.790729509878173475 ) ) ;
#194200 = CARTESIAN_POINT ( 'NONE',  ( 6.658462837642799670, 6.940830530104329377, 0.7216878364870328300 ) ) ;
#194201 = CARTESIAN_POINT ( 'NONE',  ( 1.850000000000000089, 4.013456704145457099E-20, 0.5999999999999969802 ) ) ;
#194202 = CARTESIAN_POINT ( 'NONE',  ( 2.537292984272555785, -1.624655320356691801, -1.470880813658273389 ) ) ;
#194203 = ORIENTED_EDGE ( 'NONE', *, *, #71672, .F. ) ;
#194204 =( GEOMETRIC_REPRESENTATION_CONTEXT ( 3 ) GLOBAL_UNCERTAINTY_ASSIGNED_CONTEXT ( ( #202332 ) ) GLOBAL_UNIT_ASSIGNED_CONTEXT ( ( #130101, #197137, #50896 ) ) REPRESENTATION_CONTEXT ( 'NONE', 'WORKASPACE' ) );
#194206 = CARTESIAN_POINT ( 'NONE',  ( 7.703003830858588863, 12.13858823597705872, -0.7998128361456291469 ) ) ;
#194205 = CARTESIAN_POINT ( 'NONE',  ( 0.2034672893990868703, -1.513989045467616146, -1.247398002513319781 ) ) ;
#194207 = CARTESIAN_POINT ( 'NONE',  ( 5.167565342116251514, 1.290006671357433632, 1.416291653197629952 ) ) ;
#194208 = LINE ( 'NONE', #45853, #114686 ) ;
#194209 = CARTESIAN_POINT ( 'NONE',  ( -6.041007162748570636, 7.066593642038220935, 1.036256717389577586 ) ) ;
#194210 = SURFACE_STYLE_USAGE ( .BOTH. , #165980 ) ;
#194211 = CARTESIAN_POINT ( 'NONE',  ( -1.364683531250014514, -0.7197916663252461600, 0.7879004041258379498 ) ) ;
#194213 = VERTEX_POINT ( 'NONE', #157113 ) ;
#194212 = CARTESIAN_POINT ( 'NONE',  ( 4.175548123328908900, 7.815297210618305179, -0.7216878364870197293 ) ) ;
#194214 = CARTESIAN_POINT ( 'NONE',  ( -9.842856333841300653, 10.58567993234409421, 0.7216878364870438212 ) ) ;
#194215 = CARTESIAN_POINT ( 'NONE',  ( 1.727627455807039469, -2.035446057602477321, 0.7283451284763039490 ) ) ;
#194216 = CARTESIAN_POINT ( 'NONE',  ( -3.461074353238556167, 7.259946855412102273, 0.000000000000000000 ) ) ;
#194217 = CARTESIAN_POINT ( 'NONE',  ( 3.932747076415766596, 6.745899468197171345, 1.199719254218451159 ) ) ;
#194218 = CARTESIAN_POINT ( 'NONE',  ( 1.869861807837460921, 0.9356042063937075604, 1.567457579366556386 ) ) ;
#194219 = CARTESIAN_POINT ( 'NONE',  ( -2.415323921528888196, 5.969628341758991930, 0.7998128361456341429 ) ) ;
#194220 = CARTESIAN_POINT ( 'NONE',  ( 5.104447739783800841, -0.6163660037172628003, -1.718524672285254740 ) ) ;
#194221 = CARTESIAN_POINT ( 'NONE',  ( 9.372627106707136946, 12.67835162939719318, 8.896217961834167909 ) ) ;
#194222 = CARTESIAN_POINT ( 'NONE',  ( 2.443496805918866865, -1.782974011999260977, 0.6919810379762069141 ) ) ;
#194223 = EDGE_LOOP ( 'NONE', ( #86288, #4241, #69779 ) ) ;
#194224 = CARTESIAN_POINT ( 'NONE',  ( 3.437912432318380507, 1.247599126489881138, 1.524034350268144156 ) ) ;
#194225 = ORIENTED_EDGE ( 'NONE', *, *, #205728, .F. ) ;
#194226 = CARTESIAN_POINT ( 'NONE',  ( 5.618683182394583753, -0.04358239772479224894, 1.941727988928889204 ) ) ;
#194227 = VERTEX_POINT ( 'NONE', #188524 ) ;
#194228 = CARTESIAN_POINT ( 'NONE',  ( -6.882699257592852504, 8.058845884393651460, -1.199719254218452047 ) ) ;
#194230 = CARTESIAN_POINT ( 'NONE',  ( 5.203433420164765622, 1.869144303625443371, -1.001675624404389620 ) ) ;
#194229 = CARTESIAN_POINT ( 'NONE',  ( 7.340813827156391191, 7.528980651296110160, 0.7998128361456281477 ) ) ;
#194231 = CARTESIAN_POINT ( 'NONE',  ( 6.333067150914805765, 9.442309871825708356, 1.082531754730549967 ) ) ;
#194233 = EDGE_LOOP ( 'NONE', ( #181147, #100153 ) ) ;
#194232 = CARTESIAN_POINT ( 'NONE',  ( 3.949791169003769475, -1.320912084567291034, -1.382976300589415342 ) ) ;
#194234 = CARTESIAN_POINT ( 'NONE',  ( 5.440174215215161979, 6.465126095745926449, -1.288585324421805511 ) ) ;
#194235 = FACE_OUTER_BOUND ( 'NONE', #198573, .T. ) ;
#194236 = CARTESIAN_POINT ( 'NONE',  ( -9.333041836230020039, 14.55305236562984383, 7.472413793098202639 ) ) ;
#194237 = CARTESIAN_POINT ( 'NONE',  ( 4.811194018343159406, 1.672433887399711994, -1.120210643937557871 ) ) ;
#194238 = LINE ( 'NONE', #210479, #75372 ) ;
#194239 = CARTESIAN_POINT ( 'NONE',  ( 6.533835636172961259, -1.196796279342365210, -1.378804128639096849 ) ) ;
#194240 = CARTESIAN_POINT ( 'NONE',  ( 1.275928261265106611, -2.020323679977220621, 0.4517519998969781736 ) ) ;
#194241 = CARTESIAN_POINT ( 'NONE',  ( -7.782016984564068096, 10.10210578678999482, 1.443375672974090751 ) ) ;
#194242 = AXIS2_PLACEMENT_3D ( 'NONE', #105549, #135900, #124000 ) ;
#194243 = CARTESIAN_POINT ( 'NONE',  ( -5.811016664379555330, 7.234075022110222797, -1.179019473189359068 ) ) ;
#194244 = FACE_OUTER_BOUND ( 'NONE', #132143, .T. ) ;
#194245 = CARTESIAN_POINT ( 'NONE',  ( -3.285556943750000514, -2.588541666188707513, -1.896917185911906722 ) ) ;
#194246 = CARTESIAN_POINT ( 'NONE',  ( 5.113396490648394632, 9.117379672398465473, 1.040834085586084257E-14 ) ) ;
#194247 =( LENGTH_UNIT ( ) NAMED_UNIT ( * ) SI_UNIT ( .MILLI., .METRE. ) );
#194248 = CARTESIAN_POINT ( 'NONE',  ( 4.715538499454675403, 4.395883092318884522, 1.214306433183764966E-14 ) ) ;
#194249 = CARTESIAN_POINT ( 'NONE',  ( -0.6823417656250039265, 11.13020833367473017, -1.181850606188755259 ) ) ;
#194250 = CARTESIAN_POINT ( 'NONE',  ( -5.759516327706961647, 5.613857225279885732, -0.7998128361456221525 ) ) ;
#194252 = CARTESIAN_POINT ( 'NONE',  ( -3.146901051703345331, 6.685485303713597283, 0.000000000000000000 ) ) ;
#194251 = CARTESIAN_POINT ( 'NONE',  ( -11.86685672517501899, 11.10918917859810584, -1.056525322636018727 ) ) ;
#194253 = CARTESIAN_POINT ( 'NONE',  ( 3.340171489122942816, 0.4179119503955433523, -1.682892220811042616 ) ) ;
#194254 = CARTESIAN_POINT ( 'NONE',  ( -4.660252114795309097, 6.460046772059735432, -1.599625672291256295 ) ) ;
#194255 = CARTESIAN_POINT ( 'NONE',  ( 1.340777958403309267, -2.018934908790828597, -0.4573474576154838989 ) ) ;
#194256 = CARTESIAN_POINT ( 'NONE',  ( 1.950926998395795753, -1.937146449801559367, -0.8548520037577662656 ) ) ;
#194257 = CARTESIAN_POINT ( 'NONE',  ( 3.683011284406639607, 7.448596931783069586, 0.7998128361456321445 ) ) ;
#194258 = CARTESIAN_POINT ( 'NONE',  ( 8.209625708274705502, 9.536650400197368427, 1.199719254218462483 ) ) ;
#194259 = LINE ( 'NONE', #127223, #70250 ) ;
#194260 = CARTESIAN_POINT ( 'NONE',  ( 1.112081256596690437, 1.967444819121874744, -0.09107992038001262725 ) ) ;
#194261 = CARTESIAN_POINT ( 'NONE',  ( 4.748509658595381211, 7.014904321862622361, 1.395353610025750646 ) ) ;
#194262 = CARTESIAN_POINT ( 'NONE',  ( 4.012850279964918165, 7.625483060026979842, -0.7216878364870197293 ) ) ;
#194264 = DIRECTION ( 'NONE',  ( -1.000000000000000000, -6.873509095275351032E-09, 4.111253358064373089E-11 ) ) ;
#194263 = CARTESIAN_POINT ( 'NONE',  ( -1.737499999999997824, -2.041666666666667407, 3.009438278150925683 ) ) ;
#194265 = CARTESIAN_POINT ( 'NONE',  ( 2.976851957573245944, -0.1693691376928093406, -2.286062073229557345 ) ) ;
#194266 = CARTESIAN_POINT ( 'NONE',  ( 0.8030139110496161692, 1.490934425176414724, 1.053415343471690857 ) ) ;
#194267 = CARTESIAN_POINT ( 'NONE',  ( 2.988426722125224977, -1.135634098421594240, 1.538566774472991616 ) ) ;
#194268 = CARTESIAN_POINT ( 'NONE',  ( 5.155843554946782703, 9.237177590738404831, -0.7998128361456481317 ) ) ;
#194269 = CARTESIAN_POINT ( 'NONE',  ( 8.229436053370683624, 8.703356271795033905, 0.7216878364870458196 ) ) ;
#194270 = CARTESIAN_POINT ( 'NONE',  ( -9.481229494658258261, 9.955855920056455588, -0.7998128361456291469 ) ) ;
#194271 =( BOUNDED_CURVE ( )  B_SPLINE_CURVE ( 2, ( #150850, #118397, #146600, #48034, #184383 ),
 .UNSPECIFIED., .F., .T. ) 
 B_SPLINE_CURVE_WITH_KNOTS ( ( 3, 2, 3 ),
 ( 0.02154092249793660915, 0.02500000000000000139, 0.02797185281523567602 ),
 .UNSPECIFIED. ) 
 CURVE ( )  GEOMETRIC_REPRESENTATION_ITEM ( )  RATIONAL_B_SPLINE_CURVE ( ( 0.9349445691963351734, 0.9443885786059269538, 1.000000000000000000, 0.9522216662880065297, 0.9385209747078349096 ) ) 
 REPRESENTATION_ITEM ( '' )  );
#194272 = CARTESIAN_POINT ( 'NONE',  ( 1.511978199970403836, -0.6742157057700901568, 1.897102442587648374 ) ) ;
#194273 = CARTESIAN_POINT ( 'NONE',  ( 1.639427129605858902, 1.814645582613241714, -0.7458448512465406521 ) ) ;
#194274 = CARTESIAN_POINT ( 'NONE',  ( -9.833741488613570780, 10.36711991300432345, 0.7998128361456462443 ) ) ;
#194275 = CARTESIAN_POINT ( 'NONE',  ( -8.538937818508475885, 8.856515631215026829, 1.040834085586084257E-14 ) ) ;
#194276 = CYLINDRICAL_SURFACE ( 'NONE', #130205, 0.07999999999999993228 ) ;
#194278 = CARTESIAN_POINT ( 'NONE',  ( 3.889309559433737906, 1.281865973830035754, 1.220554204183731173 ) ) ;
#194277 = CARTESIAN_POINT ( 'NONE',  ( 4.804676392994963408, 1.818819718876990565, 1.030695182279812272 ) ) ;
#194279 = CARTESIAN_POINT ( 'NONE',  ( -1.724555757183727112, 15.99999999999692335, 11.68000002332616205 ) ) ;
#194281 = CARTESIAN_POINT ( 'NONE',  ( 0.1819133275808570704, -1.029140439971199417, 1.934768540691175431 ) ) ;
#194280 = DIRECTION ( 'NONE',  ( 0.000000000000000000, 0.000000000000000000, 1.000000000000000000 ) ) ;
#194282 = CARTESIAN_POINT ( 'NONE',  ( 4.663825473582838832, -1.133750416550326046, 1.320446528551111776 ) ) ;
#194283 = EDGE_CURVE ( 'NONE', #83383, #190177, #49784, .T. ) ;
#194284 = CARTESIAN_POINT ( 'NONE',  ( 8.106885785967500979, 11.54545161934907682, 1.199719254218460707 ) ) ;
#194285 = CARTESIAN_POINT ( 'NONE',  ( -11.41381675112453387, 13.39999999999998259, 3.704697986577180746 ) ) ;
#194286 = CARTESIAN_POINT ( 'NONE',  ( 4.235468066436924417, -1.617573843961607416, -0.6246848730444684028 ) ) ;
#194287 = CARTESIAN_POINT ( 'NONE',  ( 4.457605324860562490, 1.741341149747036576, 1.296620029562136400 ) ) ;
#194288 = CARTESIAN_POINT ( 'NONE',  ( 3.063252641683779753, 5.661212951017999373, 1.199719254218450271 ) ) ;
#194289 = CARTESIAN_POINT ( 'NONE',  ( 0.3041147963815365451, -1.138459102943665036, -1.785081232699109233 ) ) ;
#194290 = CARTESIAN_POINT ( 'NONE',  ( 6.468749999177490828, 0.7852924545920478838, -1.895863743164218018 ) ) ;
#194291 = CARTESIAN_POINT ( 'NONE',  ( -3.511198596259319960, 6.271927390929313617, 1.082471891955974153 ) ) ;
#194292 = CARTESIAN_POINT ( 'NONE',  ( 2.801685564775885595, -0.6058112460363762608, 1.828711369353401617 ) ) ;
#194293 = CARTESIAN_POINT ( 'NONE',  ( -1.500000000000001110, 10.30208333401613352, 0.8660254037844419273 ) ) ;
#194294 = CARTESIAN_POINT ( 'NONE',  ( 6.533471383080789785, -0.1550430487086348341, 2.186663148620856756 ) ) ;
#194295 = VERTEX_POINT ( 'NONE', #187457 ) ;
#194296 = CARTESIAN_POINT ( 'NONE',  ( 6.883263157960402445, 0.5924656843266817852, 1.899575500811432338 ) ) ;
#194297 = CARTESIAN_POINT ( 'NONE',  ( 0.7499999999999902300, 3.733333333333352488, 1.299038105676669330 ) ) ;
#194298 = CARTESIAN_POINT ( 'NONE',  ( 4.462605117192430804, 8.358123070033169455, 1.040834085586084257E-14 ) ) ;
#194299 = EDGE_CURVE ( 'NONE', #167565, #138769, #127430, .T. ) ;
#194300 = CARTESIAN_POINT ( 'NONE',  ( 3.053626115265011709, -1.958026000861570415, 1.048987487942198094 ) ) ;
#194301 = CARTESIAN_POINT ( 'NONE',  ( -1.734723475976807094E-14, 4.000000000000003553, -1.734723475976807094E-14 ) ) ;
#194302 = CARTESIAN_POINT ( 'NONE',  ( 5.965224400332808763, 9.903252867122883885, -0.7216878364870267237 ) ) ;
#194303 = ADVANCED_FACE ( 'NONE', ( #158178 ), #105171, .F. ) ;
#194304 = CARTESIAN_POINT ( 'NONE',  ( -10.29027540264791440, 11.10766884595181203, 0.7216878364870438212 ) ) ;
#194305 =( GEOMETRIC_REPRESENTATION_CONTEXT ( 3 ) GLOBAL_UNCERTAINTY_ASSIGNED_CONTEXT ( ( #190556 ) ) GLOBAL_UNIT_ASSIGNED_CONTEXT ( ( #180847, #107662, #158483 ) ) REPRESENTATION_CONTEXT ( 'NONE', 'WORKASPACE' ) );
#194306 = CARTESIAN_POINT ( 'NONE',  ( 7.865138509703455405, 8.348618814175074121, -0.7216878364870317197 ) ) ;
#194307 = CARTESIAN_POINT ( 'NONE',  ( 0.4752326960846975923, -2.001511663014220677, -0.2440270837566413387 ) ) ;
#194309 = CARTESIAN_POINT ( 'NONE',  ( 5.828601243409065269, -1.311231720126609490, 1.592247268936395121 ) ) ;
#194308 = CARTESIAN_POINT ( 'NONE',  ( 9.348510611822643313, 10.86534945433664134, 1.199719254218453823 ) ) ;
#194310 = CARTESIAN_POINT ( 'NONE',  ( 3.625126395730617901, 6.174274991382457500, 1.251677269935605130 ) ) ;
#194311 = CARTESIAN_POINT ( 'NONE',  ( -5.251085567194491155, 5.020688004682002159, -0.7998128361456221525 ) ) ;
#194312 = CARTESIAN_POINT ( 'NONE',  ( 1.499999999999989120, 4.827083334016149863, -0.8660254037844323793 ) ) ;
#194313 = CARTESIAN_POINT ( 'NONE',  ( -1.364683531250012516, 1.280208333674755172, 0.7879004041258379498 ) ) ;
#194314 = CARTESIAN_POINT ( 'NONE',  ( 0.4382651835369972826, 0.2938455168926180638, 1.745004787994571593 ) ) ;
#194315 = CARTESIAN_POINT ( 'NONE',  ( 6.275961099261262000, 1.503942705979001593, -0.8632642021696999013 ) ) ;
#194316 = CARTESIAN_POINT ( 'NONE',  ( 5.706559709869656771, 1.539012945689299139, 0.8127616963746787659 ) ) ;
#194317 = CARTESIAN_POINT ( 'NONE',  ( 2.841680536636710386, 0.8224841172943345713, -2.139919992735066945 ) ) ;
#194318 = CARTESIAN_POINT ( 'NONE',  ( -1.364683531250014514, -0.5114583329919092369, -0.7879004041258359514 ) ) ;
#194319 = CARTESIAN_POINT ( 'NONE',  ( 1.306327274835542784, 1.622920506532832929, 0.8694138843568788300 ) ) ;
#194320 = CARTESIAN_POINT ( 'NONE',  ( 5.858512798400357546, 6.179092012920288646, 0.8810539604525641222 ) ) ;
#194321 = DIRECTION ( 'NONE',  ( 0.000000000000000000, -1.445602896647338917E-16, 1.000000000000000000 ) ) ;
#194322 = CARTESIAN_POINT ( 'NONE',  ( 1.658932825283397250, -1.563847321437005666, -0.9416461389453802955 ) ) ;
#194323 = CARTESIAN_POINT ( 'NONE',  ( 2.672500184003968382, 1.427937546361924381, 1.423961308954827754 ) ) ;
#194324 = CARTESIAN_POINT ( 'NONE',  ( 1.043234067691005684, -1.729537258485488893, -1.345685951901639532 ) ) ;
#194325 = CARTESIAN_POINT ( 'NONE',  ( 8.655013507854587118, 13.90139471787301240, -7.850520059195646105 ) ) ;
#194326 = CARTESIAN_POINT ( 'NONE',  ( 4.137795317726181032, -1.450671198928995098, -1.526879382678330010 ) ) ;
#194327 = CARTESIAN_POINT ( 'NONE',  ( -7.365103760721662951, 9.615707025640515937, 1.599625672291295375 ) ) ;
#194328 = CARTESIAN_POINT ( 'NONE',  ( 9.196684282068718019, 13.24788661686111091, 9.037284322956145033 ) ) ;
#194329 = CARTESIAN_POINT ( 'NONE',  ( 1.381394743813993964, -0.05274132383669553892, 2.069866178704109938 ) ) ;
#194330 = CARTESIAN_POINT ( 'NONE',  ( 4.599240423533799138, 6.388866465587984322, 1.599625672291267398 ) ) ;
#194331 = CARTESIAN_POINT ( 'NONE',  ( -0.6801582343750091075, 2.848958333674732391, -1.178068619123848526 ) ) ;
#194332 = CARTESIAN_POINT ( 'NONE',  ( 4.143311163141575548, 0.1052805922370502884, 2.118007119816091688 ) ) ;
#194333 = CARTESIAN_POINT ( 'NONE',  ( 0.3461526914491962481, 1.921225470409862357, 0.1432632881103387268 ) ) ;
#194334 = ORIENTED_EDGE ( 'NONE', *, *, #53547, .F. ) ;
#194335 = CARTESIAN_POINT ( 'NONE',  ( -4.606738333593328072, 8.596554832492683929, 0.7998128361456281477 ) ) ;
#194336 = CARTESIAN_POINT ( 'NONE',  ( 10.73535870392234237, 11.41900666419791399, 0.000000000000000000 ) ) ;
#194337 = CARTESIAN_POINT ( 'NONE',  ( 5.628043163004202931, 8.619781885929965526, -1.082531754730548412 ) ) ;
#194338 = CARTESIAN_POINT ( 'NONE',  ( 3.475000000000000533, -1.852083332377418401, -2.006292185433951047 ) ) ;
#194339 = CARTESIAN_POINT ( 'NONE',  ( -4.069418662396130593, 7.899405539437467816, -0.7998128361456281477 ) ) ;
#194340 = CARTESIAN_POINT ( 'NONE',  ( -0.03451705771533463557, -1.778989527951052141, 1.330178892887582398 ) ) ;
#194341 = CARTESIAN_POINT ( 'NONE',  ( 1.061710303787483989, 0.4109483673962707750, -2.065292405001526443 ) ) ;
#194343 = CARTESIAN_POINT ( 'NONE',  ( -5.492988512192097161, 6.437516681426083132, 1.199719254218452935 ) ) ;
#194342 = AXIS2_PLACEMENT_3D ( 'NONE', #182304, #33931, #66401 ) ;
#194344 = CARTESIAN_POINT ( 'NONE',  ( 9.565441069641300587, 11.11843498845840905, -1.199719254218440723 ) ) ;
#194345 = CARTESIAN_POINT ( 'NONE',  ( 5.032013264887808646, 1.069401199365666688, 1.522792188549914272 ) ) ;
#194346 = CARTESIAN_POINT ( 'NONE',  ( 7.618792255875527886, 10.97600916757510170, 1.199719254218460707 ) ) ;
#194347 = CARTESIAN_POINT ( 'NONE',  ( 4.175323295466546014, 3.976416389340326596, -0.2919458039207459832 ) ) ;
#194348 = CARTESIAN_POINT ( 'NONE',  ( -3.688700311369816909, 6.461178242310183784, -1.199719254218450271 ) ) ;
#194350 = EDGE_LOOP ( 'NONE', ( #152135, #84711, #49068, #79673 ) ) ;
#194349 = CARTESIAN_POINT ( 'NONE',  ( -9.164948653157990677, 11.71552606681625619, -1.443375672974059665 ) ) ;
#194352 = CARTESIAN_POINT ( 'NONE',  ( 2.365611650783586040, -0.4327418640146083462, 1.913375882425945917 ) ) ;
#194351 = CARTESIAN_POINT ( 'NONE',  ( -5.696397096036042385, 9.797547045350714967, -0.7998128361456231517 ) ) ;
#194353 = CARTESIAN_POINT ( 'NONE',  ( 0.6202742476981680797, -1.157488721396517040, -1.825510493854154426 ) ) ;
#194355 = CARTESIAN_POINT ( 'NONE',  ( -5.775368881829861856, 6.228402001981104164, 1.032258425150527126 ) ) ;
#194354 = CARTESIAN_POINT ( 'NONE',  ( -4.776215253764153346, 8.794277906025310898, -0.7998128361456362523 ) ) ;
#194356 = CARTESIAN_POINT ( 'NONE',  ( -1.402160292154681736E-14, 0.6968750003414164729, -1.575800808251659024 ) ) ;
#194357 = CARTESIAN_POINT ( 'NONE',  ( 2.741176079829604539, -1.657949034129829302, -0.5072451560675111937 ) ) ;
#194358 = CARTESIAN_POINT ( 'NONE',  ( 2.712550014960776856, -0.1704709713557898410, 1.731945008791212270 ) ) ;
#194359 = CARTESIAN_POINT ( 'NONE',  ( 7.646435448427411963, 8.023188899361205273, -0.7216878364870257245 ) ) ;
#194360 = CARTESIAN_POINT ( 'NONE',  ( -11.91006458477769314, 5.204012295529565790, -4.700227299318338936 ) ) ;
#194361 = AXIS2_PLACEMENT_3D ( 'NONE', #32529, #98604, #66057 ) ;
#194362 = CARTESIAN_POINT ( 'NONE',  ( 0.7903884775103054983, -1.915307795730588181, 0.6297756287277083143 ) ) ;
#194363 = CARTESIAN_POINT ( 'NONE',  ( 6.925078400183566352, 7.051505795288234957, 2.842497989238515821 ) ) ;
#194364 = CARTESIAN_POINT ( 'NONE',  ( -5.255720823952942489, 6.160704378480398979, -1.199719254218453823 ) ) ;
#194365 = CARTESIAN_POINT ( 'NONE',  ( 1.657037912627358001, -1.689797944177928279, -1.015304737199155483 ) ) ;
#194367 = CARTESIAN_POINT ( 'NONE',  ( -6.346625304972878467, 7.537389289624049304, 1.082531754730548412 ) ) ;
#194366 = CARTESIAN_POINT ( 'NONE',  ( 5.414289803398987466, -1.912571729023364364, 0.006307610287324683096 ) ) ;
#194368 = CARTESIAN_POINT ( 'NONE',  ( -6.170369307550858551, 8.292126506933035657, 1.443375672974058777 ) ) ;
#194369 = CARTESIAN_POINT ( 'NONE',  ( 7.523848900940885542, 7.742521570711348389, 0.7998128361456291469 ) ) ;
#194370 = CARTESIAN_POINT ( 'NONE',  ( -5.610041701004606196, 9.767075427805856691, -0.7998128361456362523 ) ) ;
#194371 = CARTESIAN_POINT ( 'NONE',  ( 1.629563124460619239, -0.2448459300014929063, 2.004692427041386615 ) ) ;
#194372 = DIRECTION ( 'NONE',  ( 0.000000000000000000, 0.000000000000000000, -1.000000000000000000 ) ) ;
#194373 = CARTESIAN_POINT ( 'NONE',  ( 5.139818204295112380, -1.627507941656263002, -1.636155730761083227 ) ) ;
#194375 = EDGE_CURVE ( 'NONE', #68014, #95583, #15845, .T. ) ;
#194374 = CARTESIAN_POINT ( 'NONE',  ( 6.285602425426498385, -1.847771260692541162, 0.6596951833430019230 ) ) ;
#194376 = CARTESIAN_POINT ( 'NONE',  ( 2.114041031776827673, 1.956853317873577414, -0.1391692324632237410 ) ) ;
#194377 = CARTESIAN_POINT ( 'NONE',  ( 8.886479618753304166, 12.45497775759917758, -1.199719254218446718 ) ) ;
#194378 = CARTESIAN_POINT ( 'NONE',  ( -9.438511317130744871, 15.32520388209415785, 7.309645043510521134 ) ) ;
#194379 = ORIENTED_EDGE ( 'NONE', *, *, #198353, .F. ) ;
#194380 = CARTESIAN_POINT ( 'NONE',  ( 1.727892286414894674, 0.8051050731917328562, -1.958494560251317740 ) ) ;
#194382 = CARTESIAN_POINT ( 'NONE',  ( -8.843996274815957293, 9.212417163573759282, 1.040834085586084257E-14 ) ) ;
#194381 = CARTESIAN_POINT ( 'NONE',  ( -4.786191920824102830, 5.542644314838231168, 1.199719254218462483 ) ) ;
#194383 = CARTESIAN_POINT ( 'NONE',  ( 1.271164299617353333, 1.095269041189731452, 1.479763895647051131 ) ) ;
#194384 = ORIENTED_EDGE ( 'NONE', *, *, #37073, .F. ) ;
#194385 = CARTESIAN_POINT ( 'NONE',  ( 11.75595146754954357, 7.889406149263008317, 2.187765205025514970 ) ) ;
#194386 = CARTESIAN_POINT ( 'NONE',  ( 3.023802379225454473, -0.4096935937694180518, 2.080477853870852378 ) ) ;
#194387 = CARTESIAN_POINT ( 'NONE',  ( 1.499999999999990896, 3.806250000682819046, 1.214306433183764966E-14 ) ) ;
#194388 = CARTESIAN_POINT ( 'NONE',  ( 9.237182729612253951, 9.671134694169463586, 0.7998128361456462443 ) ) ;
#194389 = CARTESIAN_POINT ( 'NONE',  ( -1.225000000000024736, 2.562500000682817358, -1.908195823574487804E-14 ) ) ;
#194390 = CARTESIAN_POINT ( 'NONE',  ( 3.233719155016498092, -1.381502681103630392, -1.529336839808728365 ) ) ;
#194392 = CARTESIAN_POINT ( 'NONE',  ( 0.4504185290156897947, -1.555054577268409899, -0.9855837367087336709 ) ) ;
#194391 = CARTESIAN_POINT ( 'NONE',  ( -8.311311860377216476, 9.655284244316948872, -1.199719254218446718 ) ) ;
#194393 = CARTESIAN_POINT ( 'NONE',  ( 1.364683531249988535, 3.363541667008084879, 0.7879004041258500513 ) ) ;
#194394 = CARTESIAN_POINT ( 'NONE',  ( 0.07775346131144458828, -0.005211914751935413023, -2.288974916015192651 ) ) ;
#194395 = DIRECTION ( 'NONE',  ( -0.000000000000000000, 1.000000000000000000, -0.000000000000000000 ) ) ;
#194396 = CARTESIAN_POINT ( 'NONE',  ( -3.070819976953871766, 2.800000000000024691, -2.497101503370694253 ) ) ;
#194397 = CARTESIAN_POINT ( 'NONE',  ( 2.583610768588519235, 2.069371435550710459, -0.9147937799905188072 ) ) ;
#194398 = VECTOR ( 'NONE', #31701, 1000.000000000000000 ) ;
#194399 = CARTESIAN_POINT ( 'NONE',  ( -8.134528978519403708, 11.47373899403920205, 1.082531754730549967 ) ) ;
#194400 = CARTESIAN_POINT ( 'NONE',  ( 2.197251250676080847, 1.655042475022786785, -0.7371099161151051238 ) ) ;
#194401 = CARTESIAN_POINT ( 'NONE',  ( 2.184663254350202255, 1.535933850207292783, -1.144682215256398239 ) ) ;
#194402 = CARTESIAN_POINT ( 'NONE',  ( 2.682155120989743402, -1.190029146579720587, -1.693995171316540427 ) ) ;
#194403 = CARTESIAN_POINT ( 'NONE',  ( -1.364683531250012516, 3.342708333674756727, 0.7879004041258379498 ) ) ;
#194404 = CARTESIAN_POINT ( 'NONE',  ( 2.166812389411576056, -1.801713905456410858, -0.8007201275355458892 ) ) ;
#194405 = CARTESIAN_POINT ( 'NONE',  ( 6.463506663115213158, 0.3265968279197262181, -1.898468693527188389 ) ) ;
#194406 = CARTESIAN_POINT ( 'NONE',  ( 2.571000202304725590, 0.09389976206976291540, -1.868427151830873267 ) ) ;
#194408 = CARTESIAN_POINT ( 'NONE',  ( 4.754190777897029818, 8.299541367957775861, -0.7767638722561143183 ) ) ;
#194407 = CARTESIAN_POINT ( 'NONE',  ( 0.9269276575891262082, 1.370462819911044239, -1.856556161720348763 ) ) ;
#194409 = CARTESIAN_POINT ( 'NONE',  ( 2.277597300015369086, -1.806044765408962194, 0.4486390909646633118 ) ) ;
#194410 = CARTESIAN_POINT ( 'NONE',  ( 0.6823417656249899377, 3.426041667008085323, -1.181850606188754593 ) ) ;
#194411 = CARTESIAN_POINT ( 'NONE',  ( 5.934046607644717142, 1.225649100846971651, 1.658920436798372311 ) ) ;
#194412 = CARTESIAN_POINT ( 'NONE',  ( -5.925076824372040640, 6.871343368977510302, 1.199719254218450271 ) ) ;
#194413 = CARTESIAN_POINT ( 'NONE',  ( 6.693975156845185737, 8.832723654451292816, 1.599625672291281386 ) ) ;
#194414 = CARTESIAN_POINT ( 'NONE',  ( -1.286813488861816790, 3.652992958535466794, -0.4595522011843584109 ) ) ;
#194415 = CARTESIAN_POINT ( 'NONE',  ( 6.633818197422741925, -1.372689285068533271, -1.597217228543364564 ) ) ;
#194416 = CARTESIAN_POINT ( 'NONE',  ( -1.364683531250012516, 3.551041667008086211, -0.7879004041258300672 ) ) ;
#194417 = CARTESIAN_POINT ( 'NONE',  ( 5.870447946289020003, -1.376328297836002079, 1.666777564274177559 ) ) ;
#194419 = EDGE_CURVE ( 'NONE', #173630, #153847, #28928, .T. ) ;
#194418 = CARTESIAN_POINT ( 'NONE',  ( 6.252604593904901975, 1.998004417694958512, 0.2941112629052196614 ) ) ;
#194420 = CARTESIAN_POINT ( 'NONE',  ( -1.402160292154681736E-14, -1.178124999658576311, 1.575800808251672791 ) ) ;
#194421 = CARTESIAN_POINT ( 'NONE',  ( -3.945059511896602089, 7.546393830613923548, 1.040834085586084257E-14 ) ) ;
#194422 = ADVANCED_FACE ( 'NONE', ( #44430 ), #163050, .T. ) ;
#194425 = CARTESIAN_POINT ( 'NONE',  ( 3.850152436600926542, 7.435668909435648288, -0.7216878364870197293 ) ) ;
#194424 = CARTESIAN_POINT ( 'NONE',  ( 6.825078400183572036, 4.699117039843025090, 2.418333817060664526 ) ) ;
#194423 = CARTESIAN_POINT ( 'NONE',  ( 6.900173834712277632, 7.014900660111269559, -0.7998128361456341429 ) ) ;
#194426 = CARTESIAN_POINT ( 'NONE',  ( -5.842637852846353397, 5.781108681267656202, 0.7998128361456281477 ) ) ;
#194427 = CARTESIAN_POINT ( 'NONE',  ( 4.188685576152741064, 1.555700494002542067, -1.282988152656767911 ) ) ;
#194428 = CARTESIAN_POINT ( 'NONE',  ( -8.202846631467911820, 9.528741477256060577, 1.199719254218462483 ) ) ;
#194430 = CARTESIAN_POINT ( 'NONE',  ( -5.275531169048895741, 9.168887107283438809, -0.7216878364870338292 ) ) ;
#194429 = CARTESIAN_POINT ( 'NONE',  ( -8.026063749610043985, 12.30756544127966912, -0.7216878364870267237 ) ) ;
#194431 = CARTESIAN_POINT ( 'NONE',  ( 1.364683531249990311, 4.613541667008083103, 0.7879004041258500513 ) ) ;
#194433 = CARTESIAN_POINT ( 'NONE',  ( -1.364683531250000748, 9.859375000341398021, 0.000000000000000000 ) ) ;
#194432 = CARTESIAN_POINT ( 'NONE',  ( 6.192270064542984898, -2.150811787302907785, -0.2168040374768212541 ) ) ;
#194434 = LINE ( 'NONE', #46075, #58623 ) ;
#194435 = CARTESIAN_POINT ( 'NONE',  ( -11.99966308016123229, 8.078345815552603781, 0.5440065656137862415 ) ) ;
#194437 = CARTESIAN_POINT ( 'NONE',  ( 0.08730790862205867198, -0.5103928513382477439, 1.846301284274171728 ) ) ;
#194436 = CARTESIAN_POINT ( 'NONE',  ( -6.738039155867462604, 7.923762439009225389, 1.082531754730549967 ) ) ;
#194438 = CARTESIAN_POINT ( 'NONE',  ( -1.364683531250000748, 0.07187500034142035865, 0.000000000000000000 ) ) ;
#194439 = CARTESIAN_POINT ( 'NONE',  ( 6.639320575229294086, 7.051910277135648997, 2.801414343313723965 ) ) ;
#194440 = CARTESIAN_POINT ( 'NONE',  ( 1.752176261082264208, 0.5389683859425442591, 1.638572262730133566 ) ) ;
#194441 = CARTESIAN_POINT ( 'NONE',  ( 7.842465510862060896, 8.114240948952696542, 0.000000000000000000 ) ) ;
#194442 = CARTESIAN_POINT ( 'NONE',  ( 5.505492895601038938, 8.580769590579979678, -1.199719254218452047 ) ) ;
#194443 = CARTESIAN_POINT ( 'NONE',  ( -11.95038703364911470, 8.982067687420316915, -1.244795252127886664 ) ) ;
#194444 = CARTESIAN_POINT ( 'NONE',  ( 6.169203917683822702, 0.1378038699498609632, -1.865550841118966297 ) ) ;
#194445 = CARTESIAN_POINT ( 'NONE',  ( 0.6100213217023927603, -0.7224815109628316412, 1.879156614266486391 ) ) ;
#194446 = LINE ( 'NONE', #195523, #64390 ) ;
#194447 = CARTESIAN_POINT ( 'NONE',  ( 3.100804818134130780, -0.6391501652806098610, -2.112195066926085829 ) ) ;
#194448 = CARTESIAN_POINT ( 'NONE',  ( 5.911019566678890058, -1.716411647115582140, 1.329421173595428884 ) ) ;
#194449 = ORIENTED_EDGE ( 'NONE', *, *, #177319, .T. ) ;
#194450 = CARTESIAN_POINT ( 'NONE',  ( 0.7499999999999885647, -0.7666666666666446250, 1.299038105676657340 ) ) ;
#194452 = CARTESIAN_POINT ( 'NONE',  ( 2.548454031204652637, -1.388473193742698619, 1.462459214312331168 ) ) ;
#194451 = CARTESIAN_POINT ( 'NONE',  ( 2.948016456289838771, -1.425740979638410399, -1.569777838261996017 ) ) ;
#194454 = ORIENTED_EDGE ( 'NONE', *, *, #59652, .T. ) ;
#194453 = CARTESIAN_POINT ( 'NONE',  ( 2.759786284469767814, 0.6482482438519759915, -1.691825979898635035 ) ) ;
#194455 = CARTESIAN_POINT ( 'NONE',  ( 6.282224075085741433, 8.422623735723785643, 1.599625672291268286 ) ) ;
#194456 = ORIENTED_EDGE ( 'NONE', *, *, #105563, .T. ) ;
#194457 = CARTESIAN_POINT ( 'NONE',  ( 0.8658264364783776479, 0.9185255527898968930, 1.629538061279064642 ) ) ;
#194458 = CARTESIAN_POINT ( 'NONE',  ( 6.449928391799196525, 8.548002428564306143, -1.599625672291262513 ) ) ;
#194460 = ADVANCED_FACE ( 'NONE', ( #41912 ), #23484, .F. ) ;
#194459 = AXIS2_PLACEMENT_3D ( 'NONE', #24941, #190635, #125737 ) ;
#194462 = CARTESIAN_POINT ( 'NONE',  ( 1.042033841529757421, 0.7795281806207611242, 1.750150644309953041 ) ) ;
#194461 = CARTESIAN_POINT ( 'NONE',  ( -5.440899717785814715, 5.242137847038546461, 0.7998128361456341429 ) ) ;
#194463 = AXIS2_PLACEMENT_3D ( 'NONE', #16494, #130353, #179035 ) ;
#194464 = CARTESIAN_POINT ( 'NONE',  ( 0.3866937364864087567, 3.956598013261175772, -11.53692321988872926 ) ) ;
#194465 = CARTESIAN_POINT ( 'NONE',  ( -11.97181042169641962, 12.22000000000000597, -0.8318531151397202672 ) ) ;
#194466 = CARTESIAN_POINT ( 'NONE',  ( -1.364683531250012516, 2.301041667008087988, -0.7879004041258289570 ) ) ;
#194467 = DIRECTION ( 'NONE',  ( 0.000000000000000000, 0.000000000000000000, 1.000000000000000000 ) ) ;
#194468 = CARTESIAN_POINT ( 'NONE',  ( -8.784793466650835825, 12.33634391347959713, 1.199719254218462483 ) ) ;
#194469 = CARTESIAN_POINT ( 'NONE',  ( 4.891577088959510711, 1.599438101461609918, 1.454397306527709155 ) ) ;
#194470 = CARTESIAN_POINT ( 'NONE',  ( -4.502716413514301408, 7.306900678191715848, -1.082531754730549967 ) ) ;
#194471 = CARTESIAN_POINT ( 'NONE',  ( -6.994027139803241866, 9.253060644560830994, -1.599625672291271394 ) ) ;
#194472 = CARTESIAN_POINT ( 'NONE',  ( 3.164422831683691761, 2.120778211551369807, -0.003951117757632071313 ) ) ;
#194474 = CARTESIAN_POINT ( 'NONE',  ( -11.31903982423144051, 5.215113036472975416, 5.710294617915439019 ) ) ;
#194473 = CARTESIAN_POINT ( 'NONE',  ( -4.916039773278787273, 4.881957280557857715, 0.5603013081572870702 ) ) ;
#194475 = CARTESIAN_POINT ( 'NONE',  ( 4.692626201678701925, -0.4289087433139714411, -1.923991814828669433 ) ) ;
#194476 = CARTESIAN_POINT ( 'NONE',  ( 5.396708386617175890, -1.867154475869851504, -0.4128305108781898936 ) ) ;
#194477 = ORIENTED_EDGE ( 'NONE', *, *, #163321, .F. ) ;
#194478 = CARTESIAN_POINT ( 'NONE',  ( 1.600055350837883195, -1.204204895297025235, 1.480038727545127220 ) ) ;
#194479 = CARTESIAN_POINT ( 'NONE',  ( 0.5903903138861701372, 1.065687334306382184, -1.774900233272216798 ) ) ;
#194480 = CARTESIAN_POINT ( 'NONE',  ( 2.747912338643729413, 0.6545661140590716132, 1.828431812057261352 ) ) ;
#194481 = ORIENTED_EDGE ( 'NONE', *, *, #29804, .F. ) ;
#194482 = CARTESIAN_POINT ( 'NONE',  ( -4.332027941937599103, 7.225435059248122016, -1.002253350946308075 ) ) ;
#194483 = CARTESIAN_POINT ( 'NONE',  ( 5.515134625708930649, 9.656350506627580543, 0.000000000000000000 ) ) ;
#194485 = CARTESIAN_POINT ( 'NONE',  ( 5.035963992472171746, 7.962709526937818083, 1.199719254218462483 ) ) ;
#194484 = CARTESIAN_POINT ( 'NONE',  ( 2.466838723508807174, 0.1015857406408589014, -2.088290385120465498 ) ) ;
#194486 = CARTESIAN_POINT ( 'NONE',  ( 4.760321331729593375, 5.686701320840210627, -1.082531754730548412 ) ) ;
#194488 = ORIENTED_EDGE ( 'NONE', *, *, #47895, .F. ) ;
#194487 = CARTESIAN_POINT ( 'NONE',  ( 0.4690326002820300877, -1.529415377529659503, -0.9703845247886667691 ) ) ;
#194489 = ADVANCED_FACE ( 'NONE', ( #172970 ), #205435, .F. ) ;
#194490 = CARTESIAN_POINT ( 'NONE',  ( 4.969440760808212509, 0.2186952961555181096, -2.196011921426939129 ) ) ;
#194491 = CARTESIAN_POINT ( 'NONE',  ( 3.540233119088306513, 0.9941544567689840628, -1.970234943098593039 ) ) ;
#194492 = CARTESIAN_POINT ( 'NONE',  ( 8.392660782059197189, 9.750191319612612872, 1.199719254218462483 ) ) ;
#194493 = CARTESIAN_POINT ( 'NONE',  ( -10.97030319645364749, 12.29999999999998295, 1.695206765504801094 ) ) ;
#194494 = CARTESIAN_POINT ( 'NONE',  ( 1.963391044528959295, -1.536740334223782867, -1.137898036029337812 ) ) ;
#194495 = CARTESIAN_POINT ( 'NONE',  ( 10.18233705906309972, 11.83814697611718714, 1.199719254218450271 ) ) ;
#194496 = CARTESIAN_POINT ( 'NONE',  ( 4.246580143467587831, -2.047389768388275577, -0.3068500204662719666 ) ) ;
#194498 = CARTESIAN_POINT ( 'NONE',  ( 2.676834871759771417, -2.068302492614528365, -0.6285112194897370941 ) ) ;
#194497 = CARTESIAN_POINT ( 'NONE',  ( 6.471393748265540147, 5.229711127717882491, 2.500000000000011102 ) ) ;
#194499 = CARTESIAN_POINT ( 'NONE',  ( 4.318054327947466575, 1.347776305887092185, -1.728067674571641898 ) ) ;
#194500 = DIRECTION ( 'NONE',  ( 0.000000000000000000, -1.000000000000000000, -0.000000000000000000 ) ) ;
#194501 = DIRECTION ( 'NONE',  ( 1.000000000000000000, 0.000000000000000000, -3.706092522800016599E-15 ) ) ;
#194502 = FACE_OUTER_BOUND ( 'NONE', #53254, .T. ) ;
#194503 = CARTESIAN_POINT ( 'NONE',  ( 4.603875680292229156, 7.528882839386387360, 1.199719254218452047 ) ) ;
#194504 = CARTESIAN_POINT ( 'NONE',  ( -3.332271893908731464, 7.109677319527304640, -0.7998128361456481317 ) ) ;
#194505 = CARTESIAN_POINT ( 'NONE',  ( 0.4576579978108759050, -1.899619568183811058, -0.6767110947205197125 ) ) ;
#194506 = CARTESIAN_POINT ( 'NONE',  ( -7.809133291791416909, 11.09411069285655493, 1.082531754730549967 ) ) ;
#194507 = CARTESIAN_POINT ( 'NONE',  ( 5.225469540725330653, 0.2083811790645866135, -2.059773418507819365 ) ) ;
#194508 = CARTESIAN_POINT ( 'NONE',  ( 3.439987180796261423, 0.8656686944604700118, -1.721121497068250017 ) ) ;
#194509 = CARTESIAN_POINT ( 'NONE',  ( 5.888306048034124274, -0.7624388358357903073, -1.975341773770035614 ) ) ;
#194510 = CARTESIAN_POINT ( 'NONE',  ( 5.660692828905515839, 6.562895374266609849, -1.199719254218445830 ) ) ;
#194511 = CARTESIAN_POINT ( 'NONE',  ( 9.622290429756469976, 3.756446959784764061, 7.170831222936541849 ) ) ;
#194512 = CARTESIAN_POINT ( 'NONE',  ( 3.766418665963155998, -0.7939890815925625400, -1.802475468321093732 ) ) ;
#194513 = CARTESIAN_POINT ( 'NONE',  ( 6.193372188798685229, -0.7780443601670664622, 2.156323934359334338 ) ) ;
#194514 = CARTESIAN_POINT ( 'NONE',  ( 4.371595934376539816, 1.770262903079304451, -0.4459408992859363319 ) ) ;
#194515 = CARTESIAN_POINT ( 'NONE',  ( 7.024532985656136930, 8.328281583754568729, 1.082531754730549967 ) ) ;
#194516 = CARTESIAN_POINT ( 'NONE',  ( 4.812781342726870193, 4.717259109377208048, 0.7216878364870317197 ) ) ;
#194517 = CARTESIAN_POINT ( 'NONE',  ( -6.957269102468015554, 8.145844036748005834, 1.199719254218452047 ) ) ;
#194518 = CARTESIAN_POINT ( 'NONE',  ( 4.179656494762836516, 8.098292687190454586, -0.7998128361456362523 ) ) ;
#194519 = VERTEX_POINT ( 'NONE', #157786 ) ;
#194521 = CARTESIAN_POINT ( 'NONE',  ( 5.185796262198086204, 1.939088309008336397, -0.5409127675100529054 ) ) ;
#194520 = CARTESIAN_POINT ( 'NONE',  ( 1.135996871135702024, 0.3593859243370273182, 1.805655672011026391 ) ) ;
#194522 = CARTESIAN_POINT ( 'NONE',  ( 0.4042330683431404892, 0.3962127685512468744, 2.263842283499896801 ) ) ;
#194523 = CARTESIAN_POINT ( 'NONE',  ( 5.664887785843471413, 1.487927489739075959, -1.278645765186999128 ) ) ;
#194524 = CARTESIAN_POINT ( 'NONE',  ( -7.230575994789712801, 7.330093503543126054, 0.7998128361456341429 ) ) ;
#194525 = DIRECTION ( 'NONE',  ( -0.000000000000000000, -1.000000000000000000, -0.000000000000000000 ) ) ;
#194526 = CARTESIAN_POINT ( 'NONE',  ( -4.303823697334223652, 7.108545849276850959, -1.199719254218452047 ) ) ;
#194527 = CARTESIAN_POINT ( 'NONE',  ( -4.163763581353360443, 7.871824920094959488, -5.011504818508299590E-05 ) ) ;
#194528 = CARTESIAN_POINT ( 'NONE',  ( -4.447956913735107598, 7.346977611736363656, 1.199719254218452935 ) ) ;
#194530 = CARTESIAN_POINT ( 'NONE',  ( 6.385617153790816403, 1.223975321695195184, 1.278628327690333411 ) ) ;
#194529 = CARTESIAN_POINT ( 'NONE',  ( 1.329752858235648150, 1.027315703197308361, -1.820849364048042318 ) ) ;
#194531 = CARTESIAN_POINT ( 'NONE',  ( -7.720982897393583677, -5.907420853759296264, 7.834948825496934610 ) ) ;
#194532 = CARTESIAN_POINT ( 'NONE',  ( 1.364683531249990311, 3.446875000341416584, 1.214306433183764966E-14 ) ) ;
#194533 = CARTESIAN_POINT ( 'NONE',  ( 0.7490575545651646516, 1.738588327661923394, -0.08332016361957059192 ) ) ;
#194534 = CARTESIAN_POINT ( 'NONE',  ( 7.135668919494039031, 7.219368582364847242, 1.040834085586084257E-14 ) ) ;
#194536 = CARTESIAN_POINT ( 'NONE',  ( 1.548913609767778699, 8.694120146927671655, 2.506286796689261465 ) ) ;
#194535 = CARTESIAN_POINT ( 'NONE',  ( 1.999999999994443289E-05, 14.55305236562340809, 11.95586206896494197 ) ) ;
#194537 = CARTESIAN_POINT ( 'NONE',  ( 2.015808680039221201, -0.8114285025175859145, -1.522100016238505216 ) ) ;
#194538 = CARTESIAN_POINT ( 'NONE',  ( 1.277182604683280598, 2.023070758711601691, -0.8431670391453591762 ) ) ;
#194539 = CARTESIAN_POINT ( 'NONE',  ( 4.530015419921377351, -1.356323209173672106, -1.740806116466916409 ) ) ;
#194540 = CYLINDRICAL_SURFACE ( 'NONE', #5163, 0.08000000000000020983 ) ;
#194541 = CIRCLE ( 'NONE', #156531, 10.99999999999999112 ) ;
#194542 = CARTESIAN_POINT ( 'NONE',  ( 0.8487579731258857452, -2.154475699732544491, -0.2676485622446558299 ) ) ;
#194543 = CARTESIAN_POINT ( 'NONE',  ( 0.1526014871912773629, -1.468541917219987836, 1.084465738218153064 ) ) ;
#194544 = CARTESIAN_POINT ( 'NONE',  ( 3.872345094350841510, -2.094861191690357227, -0.3068023397686749920 ) ) ;
#194545 = STYLED_ITEM ( 'NONE', ( #137734 ), #50792 ) ;
#194546 = CARTESIAN_POINT ( 'NONE',  ( 6.539320575229254473, 0.5926322452488984593, 1.950287522085321301 ) ) ;
#194547 = EDGE_LOOP ( 'NONE', ( #175363, #207853 ) ) ;
#194549 = CARTESIAN_POINT ( 'NONE',  ( 1.364683531249986537, -0.5322916663252452718, -0.7879004041258309554 ) ) ;
#194548 = CARTESIAN_POINT ( 'NONE',  ( 4.001757606804694056, -2.286216240038071668, 0.1689928914557006778 ) ) ;
#194550 = FILL_AREA_STYLE ('',( #129648 ) ) ;
#194551 = CARTESIAN_POINT ( 'NONE',  ( 4.517891501851804215, 6.293959390292322986, -1.599625672291255185 ) ) ;
#194552 = EDGE_CURVE ( 'NONE', #71536, #192349, #40838, .T. ) ;
#194553 = CARTESIAN_POINT ( 'NONE',  ( 6.147183147440572704, 0.2149688563512392736, 2.210895739474004529 ) ) ;
#194554 = CARTESIAN_POINT ( 'NONE',  ( -5.748293942514169252, 9.650167333001109071, -0.7216878364870207285 ) ) ;
#194555 = CARTESIAN_POINT ( 'NONE',  ( 3.538314903486612817, 7.071858454135611538, 1.040834085586084257E-14 ) ) ;
#194556 = CARTESIAN_POINT ( 'NONE',  ( -6.005898860729463884, 9.950706404252290582, 0.7216878364870458196 ) ) ;
#194557 = CARTESIAN_POINT ( 'NONE',  ( 5.451787166470912993, 6.493411461371761284, -1.082531754730548412 ) ) ;
#194558 = VERTEX_POINT ( 'NONE', #33097 ) ;
#194559 = CARTESIAN_POINT ( 'NONE',  ( 3.639296212489909532, 0.7283784247123014088, 1.880435045658496618 ) ) ;
#194561 = CARTESIAN_POINT ( 'NONE',  ( 2.395447240195498484, -1.844268472375994339, 0.9235843863054800096 ) ) ;
#194560 = CARTESIAN_POINT ( 'NONE',  ( 4.937140493670735708, 8.911747675924535983, -0.7998128361456281477 ) ) ;
#194562 = DIRECTION ( 'NONE',  ( 0.000000000000000000, 1.000000000000000000, 0.000000000000000000 ) ) ;
#194563 = CARTESIAN_POINT ( 'NONE',  ( 5.709392084686216506, 5.833581318321598985, -0.7216878364870458196 ) ) ;
#194564 = CARTESIAN_POINT ( 'NONE',  ( -1.420000000000021911, 6.280000000000042881, 2.873333333333347728 ) ) ;
#194565 = CARTESIAN_POINT ( 'NONE',  ( -0.6823417656250212460, 4.801041667008086655, 1.181850606188767472 ) ) ;
#194566 = CARTESIAN_POINT ( 'NONE',  ( 5.244143516318892750, 0.6338322011035132375, 2.097776330851252258 ) ) ;
#194567 = CARTESIAN_POINT ( 'NONE',  ( 2.426407915648312930, -1.496052118593782065, -1.352154011671408362 ) ) ;
#194568 = CARTESIAN_POINT ( 'NONE',  ( 2.612652284633736777, -0.1782932461553646819, 1.832575692395449485 ) ) ;
#194569 = CARTESIAN_POINT ( 'NONE',  ( 6.825640269476072497, 10.05066518344239412, 1.199719254218460707 ) ) ;
#194571 = EDGE_CURVE ( 'NONE', #54861, #115034, #146881, .T. ) ;
#194570 =( LENGTH_UNIT ( ) NAMED_UNIT ( * ) SI_UNIT ( .MILLI., .METRE. ) );
#194572 = CARTESIAN_POINT ( 'NONE',  ( 5.192344348049102720, -1.811977082810274808, -0.2219828972063255801 ) ) ;
#194573 = CARTESIAN_POINT ( 'NONE',  ( 6.574846728087075931, -0.8593996854794653251, 1.822268861383633531 ) ) ;
#194574 = CARTESIAN_POINT ( 'NONE',  ( -8.701635661872465732, 9.046329781806354831, 1.040834085586084257E-14 ) ) ;
#194576 = CARTESIAN_POINT ( 'NONE',  ( -5.631432701629818460, 7.663367133358481631, 1.599625672291263179 ) ) ;
#194575 = CARTESIAN_POINT ( 'NONE',  ( 5.752851848433533810, -1.787673638215280913, 1.386716842396797489 ) ) ;
#194577 = CARTESIAN_POINT ( 'NONE',  ( 0.5222713366250474332, -1.128438999127111098, -1.778050165696586360 ) ) ;
#194578 = CARTESIAN_POINT ( 'NONE',  ( -6.994027139803241866, 9.253060644560830994, -1.599625672291271394 ) ) ;
#194579 = CARTESIAN_POINT ( 'NONE',  ( 7.564559641420864899, 10.91273778404466199, -1.199719254218446718 ) ) ;
#194580 = CARTESIAN_POINT ( 'NONE',  ( -0.6801582343750420812, 2.713541667008087632, 1.178068619123787908 ) ) ;
#194581 = CARTESIAN_POINT ( 'NONE',  ( 8.378074386687012876, 27.10815134976859397, 15.76159487570643059 ) ) ;
#194582 = CARTESIAN_POINT ( 'NONE',  ( -6.042130013184518589, 10.20090211535728031, -0.7998128361456291469 ) ) ;
#194583 = UNCERTAINTY_MEASURE_WITH_UNIT (LENGTH_MEASURE( 1.000000000000000082E-05 ), #156177, 'distance_accuracy_value', 'NONE');
#194584 = CARTESIAN_POINT ( 'NONE',  ( -1.249999999999964695, 8.500000000000000000, -11.02939254900287303 ) ) ;
#194585 = CARTESIAN_POINT ( 'NONE',  ( 5.191320393234815533, 6.438618948542633724, -1.178512179637403623 ) ) ;
#194586 = CARTESIAN_POINT ( 'NONE',  ( -9.842856333841300653, 10.58567993234409421, 0.7216878364870438212 ) ) ;
#194588 = CARTESIAN_POINT ( 'NONE',  ( 3.164521688127000854, 2.221583673635919354, -0.003682443279265367429 ) ) ;
#194587 = CARTESIAN_POINT ( 'NONE',  ( 1.371502371489873751, -1.821557607348308405, -1.085495857948336251 ) ) ;
#194589 = AXIS2_PLACEMENT_3D ( 'NONE', #63696, #50642, #47471 ) ;
#194590 = CARTESIAN_POINT ( 'NONE',  ( 3.277927966699532014, 6.407906593915337901, -0.9422035321714219425 ) ) ;
#194591 = CARTESIAN_POINT ( 'NONE',  ( -6.934069218746458318, 7.054445274817795486, -0.7998128361456362523 ) ) ;
#194592 = CARTESIAN_POINT ( 'NONE',  ( 6.124532705071213279, 8.168374127381657246, -1.599625672291262513 ) ) ;
#194593 = CARTESIAN_POINT ( 'NONE',  ( 3.578520225191741844, 1.246510459297203610, -1.514941731618473009 ) ) ;
#194594 = CARTESIAN_POINT ( 'NONE',  ( 4.137209430464448445, 7.978494768850520558, 1.040834085586084257E-14 ) ) ;
#194595 = CARTESIAN_POINT ( 'NONE',  ( -4.016961781477323079, 7.622873323794868483, 0.1115696107641880874 ) ) ;
#194596 = CARTESIAN_POINT ( 'NONE',  ( 2.984766373302843778, 6.633977868828633717, -0.7998128361456291469 ) ) ;
#194597 = CARTESIAN_POINT ( 'NONE',  ( -3.838366886444665393, 7.492195444245147939, 0.000000000000000000 ) ) ;
#194598 = CARTESIAN_POINT ( 'NONE',  ( -5.721177635286839092, 9.618531641235897212, 0.7216878364870458196 ) ) ;
#194599 = CARTESIAN_POINT ( 'NONE',  ( 2.531617689938488791, -0.2033970545941807817, 2.110794199748195599 ) ) ;
#194600 = CARTESIAN_POINT ( 'NONE',  ( -6.445975688654487001, 6.485002823043819475, -0.7998128361456362523 ) ) ;
#194601 = CARTESIAN_POINT ( 'NONE',  ( 4.698204674003193304, -2.161138953124014161, -0.05634304724232848394 ) ) ;
#194602 = CARTESIAN_POINT ( 'NONE',  ( 3.140019216317342376, 0.4501627324021879040, 1.785233193441162713 ) ) ;
#194603 = CARTESIAN_POINT ( 'NONE',  ( -5.312135015290653683, 6.384990658495349081, 1.125702006352300000 ) ) ;
#194604 = CARTESIAN_POINT ( 'NONE',  ( 1.364683531249988757, 0.1968750003414204697, 0.000000000000000000 ) ) ;
#194605 = CARTESIAN_POINT ( 'NONE',  ( 6.035049474595155949, -1.265358352104806183, -1.195092038424966363 ) ) ;
#194606 = CARTESIAN_POINT ( 'NONE',  ( 6.727182134110199385, 3.711531441867378600, 2.225637065106730095 ) ) ;
#194607 = CARTESIAN_POINT ( 'NONE',  ( 4.121315508874254796, 5.831287398485176077, -1.443375672974051449 ) ) ;
#194608 = SURFACE_STYLE_FILL_AREA ( #139489 ) ;
#194609 = CARTESIAN_POINT ( 'NONE',  ( 2.958072429731006370, 2.151414462573512765, -0.2105227563667099733 ) ) ;
#194610 = VECTOR ( 'NONE', #66013, 1000.000000000000114 ) ;
#194611 = CARTESIAN_POINT ( 'NONE',  ( 4.780624950969222020, -1.977747464269607347, 0.3905396900540994420 ) ) ;
#194612 = CARTESIAN_POINT ( 'NONE',  ( -7.985389288324692636, 11.29974268881207067, -1.082531754730543083 ) ) ;
#194614 = AXIS2_PLACEMENT_3D ( 'NONE', #173383, #41252, #88932 ) ;
#194613 = CARTESIAN_POINT ( 'NONE',  ( 2.694378501574711926, -2.155843008138720762, -0.1600555415394027403 ) ) ;
#194615 = CARTESIAN_POINT ( 'NONE',  ( 3.005103179519866607, 1.663439489741199928, 1.057676205593648167 ) ) ;
#194616 = CARTESIAN_POINT ( 'NONE',  ( -6.558215298580997832, 6.787841129500100656, 0.5453671684877616777 ) ) ;
#194617 = CARTESIAN_POINT ( 'NONE',  ( 4.440924170176640651, -1.503556815104054811, -1.229221392163130755 ) ) ;
#194620 = ORIENTED_EDGE ( 'NONE', *, *, #68527, .T. ) ;
#194619 = CARTESIAN_POINT ( 'NONE',  ( 0.000000000000000000, 0.000000000000000000, 0.000000000000000000 ) ) ;
#194618 = CARTESIAN_POINT ( 'NONE',  ( -7.768458830506062007, 11.04665715469030296, 1.082531754730549967 ) ) ;
#194621 = CARTESIAN_POINT ( 'NONE',  ( -3.485854892044998543, 6.120562236477518070, -1.082531754730546636 ) ) ;
#194622 = DIRECTION ( 'NONE',  ( 0.000000000000000000, 0.000000000000000000, 1.000000000000000000 ) ) ;
#194624 = ORIENTED_EDGE ( 'NONE', *, *, #113967, .T. ) ;
#194623 = CARTESIAN_POINT ( 'NONE',  ( -3.481411583659053566, 7.283673624236017830, 0.000000000000000000 ) ) ;
#194625 = CARTESIAN_POINT ( 'NONE',  ( -8.798878505144665851, 9.367705798864669475, -0.7216878364870267237 ) ) ;
#194626 = CARTESIAN_POINT ( 'NONE',  ( 0.7982362974770088604, -0.7925503509537080715, 2.059710425106767939 ) ) ;
#194628 = EDGE_CURVE ( 'NONE', #34146, #159908, #13639, .T. ) ;
#194627 = CARTESIAN_POINT ( 'NONE',  ( 3.285556943750000514, -1.363541666188709423, 1.896917185911906500 ) ) ;
#194629 = AXIS2_PLACEMENT_3D ( 'NONE', #48862, #14192, #160473 ) ;
#194630 = CARTESIAN_POINT ( 'NONE',  ( 5.875826477234550538, -1.914729252524836056, 0.4262945716600323731 ) ) ;
#194631 = CARTESIAN_POINT ( 'NONE',  ( -1.001543065824772872E-14, 5.134375000341421469, 1.575800808251672791 ) ) ;
#194632 = CARTESIAN_POINT ( 'NONE',  ( 0.7499999999999902300, 4.097916667349481123, -1.299038105676658228 ) ) ;
#194633 = CARTESIAN_POINT ( 'NONE',  ( 5.816641468517390834, 6.206546802344954372, -0.9418049055998338748 ) ) ;
#194634 = CARTESIAN_POINT ( 'NONE',  ( 0.07499057489264349119, 0.002531239327734773146, -1.955573237620360505 ) ) ;
#194635 = CARTESIAN_POINT ( 'NONE',  ( 4.540845788227630742, -1.424921066559198257, -1.165926479108070346 ) ) ;
#194636 = VERTEX_POINT ( 'NONE', #15759 ) ;
#194637 = CARTESIAN_POINT ( 'NONE',  ( 0.6801582343749952297, -0.1927083329918907739, -1.178068619123876282 ) ) ;
#194638 = CARTESIAN_POINT ( 'NONE',  ( -8.369460898337653276, 8.658792557682392754, 0.7998128361456462443 ) ) ;
#194639 = FACE_OUTER_BOUND ( 'NONE', #50267, .T. ) ;
#194640 = SURFACE_STYLE_FILL_AREA ( #62508 ) ;
#194641 = CARTESIAN_POINT ( 'NONE',  ( 4.638861114170084399, 8.563755066507100722, 0.7998128361456462443 ) ) ;
#194642 = AXIS2_PLACEMENT_3D ( 'NONE', #103140, #151898, #115187 ) ;
#194643 = EDGE_LOOP ( 'NONE', ( #119306, #104995, #37903, #76111 ) ) ;
#194644 = CARTESIAN_POINT ( 'NONE',  ( 6.591097270071800907, 1.795350502275098403, -1.011519373207786288 ) ) ;
#194647 = CARTESIAN_POINT ( 'NONE',  ( 3.878315922200573862, -0.1843894689829879696, -1.832007427040844183 ) ) ;
#194646 = CARTESIAN_POINT ( 'NONE',  ( 1.521681963465530529, 1.834278628056866367, -0.3135228456460791846 ) ) ;
#194645 = CARTESIAN_POINT ( 'NONE',  ( -9.993490455110626058, 4.532987658119245644, 6.649910637754151921 ) ) ;
#194648 = CARTESIAN_POINT ( 'NONE',  ( 6.584456157731144899, 10.83361595066169514, -0.7998128361456291469 ) ) ;
#194649 = DIRECTION ( 'NONE',  ( 0.000000000000000000, -1.000000000000000000, 0.000000000000000000 ) ) ;
#194650 = CARTESIAN_POINT ( 'NONE',  ( -7.442499979258930587, 7.647614495415686164, -0.7998128361456362523 ) ) ;
#194651 = CARTESIAN_POINT ( 'NONE',  ( 3.929058411375439874, 5.999999999999998224, -0.7500000000000006661 ) ) ;
#194652 = CARTESIAN_POINT ( 'NONE',  ( 3.492985898914053866, -0.4302566696539159574, -2.164365734511737305 ) ) ;
#194653 = CARTESIAN_POINT ( 'NONE',  ( 5.729810862507367375, -1.428767958649424408, -1.754208347296302373 ) ) ;
#194654 = CARTESIAN_POINT ( 'NONE',  ( -7.375272376154101472, 7.706831981708990753, -0.7216878364870278340 ) ) ;
#194655 = CARTESIAN_POINT ( 'NONE',  ( 5.449399174529797385, -1.634242350402253852, 0.7820841365046418137 ) ) ;
#194656 = CARTESIAN_POINT ( 'NONE',  ( 5.928903634556547786, -1.614502157299831042, 1.030912532684091110 ) ) ;
#194657 = CARTESIAN_POINT ( 'NONE',  ( 3.930720324626956863, 8.992102070998166496, 0.7749999999999996891 ) ) ;
#194658 = CARTESIAN_POINT ( 'NONE',  ( 5.963714631206167738, 1.842656449598079060, -0.3214700631931910468 ) ) ;
#194659 = CARTESIAN_POINT ( 'NONE',  ( 0.000000000000000000, -6.893137084989842123, 0.000000000000000000 ) ) ;
#194660 = CARTESIAN_POINT ( 'NONE',  ( 6.157089704101026406, -1.520188931036812185, -0.9060637366671944193 ) ) ;
#194661 = CARTESIAN_POINT ( 'NONE',  ( 0.9543149826918421175, -1.275552737861269437, 1.561884623745241951 ) ) ;
#194663 = CARTESIAN_POINT ( 'NONE',  ( 3.141344390434357869, -1.857286833677756599, 0.9929794709265575836 ) ) ;
#194662 = CARTESIAN_POINT ( 'NONE',  ( -10.31505594189871111, 10.92865344183699428, -0.7998128361456291469 ) ) ;
#194664 = CARTESIAN_POINT ( 'NONE',  ( 9.610031953988080744, 10.10612545594124967, -0.7998128361456281477 ) ) ;
#194666 = CARTESIAN_POINT ( 'NONE',  ( -7.883176251342026042, 11.28445716228600126, -1.199719254218446718 ) ) ;
#194665 = CARTESIAN_POINT ( 'NONE',  ( 0.7499999999999885647, -0.7666666666666446250, 1.299038105676657340 ) ) ;
#194667 = CARTESIAN_POINT ( 'NONE',  ( 11.55950211276791428, 9.719999999999982876, 3.221476510067112109 ) ) ;
#194669 = EDGE_CURVE ( 'NONE', #174410, #36083, #192159, .T. ) ;
#194668 = CARTESIAN_POINT ( 'NONE',  ( 2.619404093423041591, 1.708565301817746018, 1.076861402434741821 ) ) ;
#194670 = CARTESIAN_POINT ( 'NONE',  ( -1.364683531250012516, 3.488541667008085767, -0.7879004041258300672 ) ) ;
#194671 = CARTESIAN_POINT ( 'NONE',  ( 4.383363735919856730, 4.008345868194933104, -0.7998128361456211532 ) ) ;
#194672 = CARTESIAN_POINT ( 'NONE',  ( 3.022914066069124051, 2.034213141994867247, 0.7313807043239917149 ) ) ;
#194673 = CARTESIAN_POINT ( 'NONE',  ( 1.438722645073102990, 7.870286565763570330, -3.684014302713757516 ) ) ;
#194675 = CARTESIAN_POINT ( 'NONE',  ( 4.505997031185814627, 8.479023313017261643, -0.7440749432275711728 ) ) ;
#194674 = CARTESIAN_POINT ( 'NONE',  ( 6.801350335910821165, 7.963938809097990124, 1.199719254218452047 ) ) ;
#194676 = CARTESIAN_POINT ( 'NONE',  ( 10.01911233037458260, 10.79131192829960462, 0.7216878364870438212 ) ) ;
#194678 = CARTESIAN_POINT ( 'NONE',  ( 6.928203230275523872, 15.51845925587262620, -9.797958971132697314 ) ) ;
#194677 = CARTESIAN_POINT ( 'NONE',  ( 0.9948528382496389932, 2.139055259286365640, 0.3712904390174593949 ) ) ;
#194679 =( BOUNDED_CURVE ( )  B_SPLINE_CURVE ( 2, ( #161249, #45378, #17096, #145032, #95198 ),
 .UNSPECIFIED., .F., .T. ) 
 B_SPLINE_CURVE_WITH_KNOTS ( ( 3, 2, 3 ),
 ( 0.2697076323948381371, 0.2750000000000000222, 0.2818589531839510443 ),
 .UNSPECIFIED. ) 
 CURVE ( )  GEOMETRIC_REPRESENTATION_ITEM ( )  RATIONAL_B_SPLINE_CURVE ( ( 0.9379021630552799582, 0.9149148624488946391, 1.000000000000000000, 0.8897289420062464149, 0.9609804498502303449 ) ) 
 REPRESENTATION_ITEM ( '' )  );
#194680 = CARTESIAN_POINT ( 'NONE',  ( -5.585596099150174965, 9.460353182409786399, -0.7216878364870207285 ) ) ;
#194681 = ADVANCED_FACE ( 'NONE', ( #147927 ), #71899, .F. ) ;
#194682 = CARTESIAN_POINT ( 'NONE',  ( -0.6823417656250003738, 0.7177083336747519526, -1.181850606188749264 ) ) ;
#194683 = CARTESIAN_POINT ( 'NONE',  ( 1.962683346935737205, -2.005255389829229351, -0.8846387633431598285 ) ) ;
#194684 = CARTESIAN_POINT ( 'NONE',  ( 0.5015801190230135820, 7.801378974689940904, 1.936921611551724931 ) ) ;
#194685 = CARTESIAN_POINT ( 'NONE',  ( 2.975713975707586556, 2.148818855599075928, -0.7084362298409478953 ) ) ;
#194686 = CARTESIAN_POINT ( 'NONE',  ( -7.670162217029145246, 9.971608557999250166, 1.599625672291295375 ) ) ;
#194687 = CARTESIAN_POINT ( 'NONE',  ( 4.540250091716044878, 0.7762272601403925609, 1.861345588084816871 ) ) ;
#194688 = CARTESIAN_POINT ( 'NONE',  ( -2.941756144040963417, 6.375873234782333476, -0.7216878364870257245 ) ) ;
#194689 = CARTESIAN_POINT ( 'NONE',  ( 1.364683531249988535, 3.426041667008085323, 0.7879004041258500513 ) ) ;
#194690 = CARTESIAN_POINT ( 'NONE',  ( 4.855733865602142707, 8.067643820953190215, 0.9155131637919884380 ) ) ;
#194691 = CARTESIAN_POINT ( 'NONE',  ( -1.500000000000001110, 12.52083333333333037, 0.8660254037844419273 ) ) ;
#194692 = CARTESIAN_POINT ( 'NONE',  ( 5.668717624289557833, 8.667235424096215723, -1.082531754730548412 ) ) ;
#194693 =( BOUNDED_CURVE ( )  B_SPLINE_CURVE ( 2, ( #182854, #86435, #51813 ),
 .UNSPECIFIED., .F., .T. ) 
 B_SPLINE_CURVE_WITH_KNOTS ( ( 3, 3 ),
 ( 0.000000000000000000, 0.0002183499308596753715 ),
 .UNSPECIFIED. ) 
 CURVE ( )  GEOMETRIC_REPRESENTATION_ITEM ( )  RATIONAL_B_SPLINE_CURVE ( ( 1.000000000000000000, 0.9929791974830509682, 0.9866942310032964514 ) ) 
 REPRESENTATION_ITEM ( '' )  );
#194694 = CARTESIAN_POINT ( 'NONE',  ( 4.288192095134175652, -1.750260269857591755, -0.2610086191854649740 ) ) ;
#194695 = CARTESIAN_POINT ( 'NONE',  ( 8.075853055234393452, 12.57357899774884658, 0.7998128361456462443 ) ) ;
#194696 = CARTESIAN_POINT ( 'NONE',  ( 6.335036379411270957, 0.2100110484798515254, 2.196758413611602290 ) ) ;
#194697 = CARTESIAN_POINT ( 'NONE',  ( -8.012344526598182026E-15, 9.546875000341399797, -1.575800808251669460 ) ) ;
#194698 = CARTESIAN_POINT ( 'NONE',  ( -5.808742468812186033, 5.741564066561132940, 0.000000000000000000 ) ) ;
#194699 = CARTESIAN_POINT ( 'NONE',  ( 5.923453886551513392, -1.462456689723025782, -1.388475849216065372 ) ) ;
#194700 = ORIENTED_EDGE ( 'NONE', *, *, #118594, .F. ) ;
#194701 = EDGE_CURVE ( 'NONE', #144017, #76712, #177227, .T. ) ;
#194702 = CARTESIAN_POINT ( 'NONE',  ( 4.135518821028766112, -1.289757458839156934, -1.355179912160727085 ) ) ;
#194703 = CARTESIAN_POINT ( 'NONE',  ( 3.608316154870555792, 2.070434559819031684, 0.004826415812286819103 ) ) ;
#194704 = EDGE_CURVE ( 'NONE', #186393, #15455, #185459, .T. ) ;
#194705 = CARTESIAN_POINT ( 'NONE',  ( -6.902509602688830626, 7.225551755991315162, -0.7216878364870338292 ) ) ;
#194706 = SURFACE_STYLE_FILL_AREA ( #33268 ) ;
#194707 = CARTESIAN_POINT ( 'NONE',  ( -9.541882734523161602, 5.027466607964795386, -6.730450668810338044 ) ) ;
#194708 = CARTESIAN_POINT ( 'NONE',  ( -4.002183151617731305, 7.677155228057962688, 0.1020948806719407381 ) ) ;
#194709 = CARTESIAN_POINT ( 'NONE',  ( 5.875883356151953230, 1.283970044810868849, 1.738936680771227206 ) ) ;
#194710 = CARTESIAN_POINT ( 'NONE',  ( -1.364683531250000748, -0.9906249996585805295, 0.000000000000000000 ) ) ;
#194711 = CARTESIAN_POINT ( 'NONE',  ( 2.400770673373255448, 0.4268909467371252431, 1.914702609522442867 ) ) ;
#194712 = CARTESIAN_POINT ( 'NONE',  ( 0.4564073884281876770, 1.492024165150519055, 1.356095248386236074 ) ) ;
#194713 = CARTESIAN_POINT ( 'NONE',  ( -5.334207092333882017, 5.187939460669764635, 0.7998128361456281477 ) ) ;
#194715 = CARTESIAN_POINT ( 'NONE',  ( -11.94105721237523099, 13.40000000000000036, -1.187919463087249827 ) ) ;
#194714 = CARTESIAN_POINT ( 'NONE',  ( 9.094822116668764167, 9.505047312402055582, 0.7998128361456462443 ) ) ;
#194716 = CARTESIAN_POINT ( 'NONE',  ( 0.5439545674776785633, 1.865077268347898665, 0.1441030193207945287 ) ) ;
#194717 = CARTESIAN_POINT ( 'NONE',  ( -1.364683531249997417, 3.259375000341423245, 1.214306433183764966E-14 ) ) ;
#194718 = CARTESIAN_POINT ( 'NONE',  ( 3.480730050573742851, -1.348849006198136635, 1.494714382889005488 ) ) ;
#194720 = CARTESIAN_POINT ( 'NONE',  ( 1.740021635027885649, 2.111287947816307575, -0.1595968877764943616 ) ) ;
#194719 = CARTESIAN_POINT ( 'NONE',  ( -6.561783159334137139, 8.678499657355050800, -1.443375672974059665 ) ) ;
#194721 = DIRECTION ( 'NONE',  ( 1.000000000000000000, -0.000000000000000000, -0.000000000000000000 ) ) ;
#194722 = CARTESIAN_POINT ( 'NONE',  ( 3.965334771736851671, 1.774175476309115984, 1.066894043611272824 ) ) ;
#194723 = CARTESIAN_POINT ( 'NONE',  ( 3.410758162289653672, 6.136912401716668519, -1.199719254218453823 ) ) ;
#194725 = CARTESIAN_POINT ( 'NONE',  ( 2.367870383881045981, 5.914265881169853856, 0.000000000000000000 ) ) ;
#194724 = CARTESIAN_POINT ( 'NONE',  ( 5.314434061427068201, 1.931386623266003078, 0.8008058956679960927 ) ) ;
#194727 = VERTEX_POINT ( 'NONE', #194527 ) ;
#194726 = CARTESIAN_POINT ( 'NONE',  ( 3.715676801689533626, -1.798647723735953496, 0.3114480851732701061 ) ) ;
#194728 = CARTESIAN_POINT ( 'NONE',  ( 9.901532256681887745, 10.44620914241737530, 0.000000000000000000 ) ) ;
#194729 = CARTESIAN_POINT ( 'NONE',  ( 7.778383330260338013, -6.134628647623489250, -7.778383330260366435 ) ) ;
#194731 = AXIS2_PLACEMENT_3D ( 'NONE', #201866, #119648, #151034 ) ;
#194730 = CARTESIAN_POINT ( 'NONE',  ( 9.741349722503858999, 13.15934765701661391, 8.090281636115273400 ) ) ;
#194732 = CARTESIAN_POINT ( 'NONE',  ( 6.827182134110222123, -0.006956174471953178659, 2.188967759425272330 ) ) ;
#194733 = CARTESIAN_POINT ( 'NONE',  ( -1.364683531250010740, 10.94270833367473372, 0.7879004041258445001 ) ) ;
#194734 = CARTESIAN_POINT ( 'NONE',  ( 5.092401474535850348, -1.059014397921493433, 1.592059587274458510 ) ) ;
#194735 = CARTESIAN_POINT ( 'NONE',  ( -9.459838494033043332, 12.05956421450382088, 1.599625672291281386 ) ) ;
#194736 =( BOUNDED_CURVE ( )  B_SPLINE_CURVE ( 2, ( #77177, #110818, #145438, #211438, #63070, #129238, #176824, #142223, #112961 ),
 .UNSPECIFIED., .F., .T. ) 
 B_SPLINE_CURVE_WITH_KNOTS ( ( 3, 2, 2, 2, 3 ),
 ( 0.4553571428571427937, 0.4583333333333333148, 0.4642857142857143016, 0.4702380952380952328, 0.4732142857142856984 ),
 .UNSPECIFIED. ) 
 CURVE ( )  GEOMETRIC_REPRESENTATION_ITEM ( )  RATIONAL_B_SPLINE_CURVE ( ( 0.9330127018922194093, 0.9330127018922180770, 1.000000000000000000, 0.8660254037844387076, 1.000000000000000000, 0.8660254037844387076, 1.000000000000000000, 0.9330127018922194093, 0.9330127018922194093 ) ) 
 REPRESENTATION_ITEM ( '' )  );
#194737 = CARTESIAN_POINT ( 'NONE',  ( 6.632963465583686435, 8.761543347979550589, -1.599625672291262513 ) ) ;
#194738 = CARTESIAN_POINT ( 'NONE',  ( -1.752700365193352683E-14, 1.609375000341425554, -1.570758158831794260 ) ) ;
#194739 = CARTESIAN_POINT ( 'NONE',  ( 4.161989969270902812, 4.918371721313249623, 1.082531754730560403 ) ) ;
#194740 = CARTESIAN_POINT ( 'NONE',  ( 9.500331257164628340, -7.473374494045002869, -1.537682436621775084E-15 ) ) ;
#194741 = CARTESIAN_POINT ( 'NONE',  ( 4.741601036477289810, 6.554953847355395880, 1.599625672291267398 ) ) ;
#194742 = EDGE_LOOP ( 'NONE', ( #115686, #159375 ) ) ;
#194743 = CARTESIAN_POINT ( 'NONE',  ( -7.425025402139490360, 8.691559719698066289, 1.199719254218452047 ) ) ;
#194744 = CARTESIAN_POINT ( 'NONE',  ( 4.323419078940895943, -1.790677508454678657, 0.5408235849187342792 ) ) ;
#194745 = CARTESIAN_POINT ( 'NONE',  ( 0.07700591528354487625, 0.7269319812311864082, -1.993543990282041767 ) ) ;
#194746 = CARTESIAN_POINT ( 'NONE',  ( 5.332099551924443404, 9.442809587212341427, 0.000000000000000000 ) ) ;
#194747 = FACE_OUTER_BOUND ( 'NONE', #168373, .T. ) ;
#194748 = TOROIDAL_SURFACE ( 'NONE', #187793, 6.500000000000000000, 0.2999999999999999889 ) ;
#194749 = AXIS2_PLACEMENT_3D ( 'NONE', #179096, #130419, #81582 ) ;
#194750 = CARTESIAN_POINT ( 'NONE',  ( -6.394499343358424959, 6.826875778244118287, 0.5478302896938479494 ) ) ;
#194751 = CARTESIAN_POINT ( 'NONE',  ( -7.239690840017442675, 7.548653522882887934, 0.7216878364870317197 ) ) ;
#194752 = CARTESIAN_POINT ( 'NONE',  ( 5.359550796103802028, 5.147230771742885125, -0.7998128361456231517 ) ) ;
#194753 = CARTESIAN_POINT ( 'NONE',  ( 0.8659821450925162534, -1.960479642884611629, 0.1873741036552133976 ) ) ;
#194754 = CARTESIAN_POINT ( 'NONE',  ( 2.900017720922347220, -0.9963201819552582883, -1.753021271517739343 ) ) ;
#194755 = CARTESIAN_POINT ( 'NONE',  ( -7.100719765255177229, 9.307259030929609267, -1.599625672291263179 ) ) ;
#194756 = CARTESIAN_POINT ( 'NONE',  ( 6.215487077222150880, 6.216099443039444949, 0.000000000000000000 ) ) ;
#194757 = SURFACE_STYLE_FILL_AREA ( #197947 ) ;
#194758 = CARTESIAN_POINT ( 'NONE',  ( 3.767680093253112705, 1.217039798425190167, 1.822233383357040104 ) ) ;
#194759 = CARTESIAN_POINT ( 'NONE',  ( 9.406473873361589355, 3.553052728507827052, -7.380697183404369532 ) ) ;
#194760 = CARTESIAN_POINT ( 'NONE',  ( -10.14557902172788495, 10.73093036830436553, 1.040834085586084257E-14 ) ) ;
#194761 = CARTESIAN_POINT ( 'NONE',  ( 6.825078400183590688, 2.971555572656236599, 2.408956600524428282 ) ) ;
#194762 = DIRECTION ( 'NONE',  ( -1.276756478318932585E-15, 1.000000000000000000, -1.665334536937738262E-16 ) ) ;
#194763 = CARTESIAN_POINT ( 'NONE',  ( 4.014622883422321209, 5.777089012116397804, -1.443375672974068769 ) ) ;
#194764 = CARTESIAN_POINT ( 'NONE',  ( 7.853197290813620945, 10.18514947741448573, 1.599625672291281386 ) ) ;
#194765 = CIRCLE ( 'NONE', #25168, 4.583333333333340143 ) ;
#194766 = FACE_OUTER_BOUND ( 'NONE', #166241, .T. ) ;
#194767 = CARTESIAN_POINT ( 'NONE',  ( 5.234856708652222856, 8.161064355852680308, 1.082531754730549078 ) ) ;
#194768 = ORIENTED_EDGE ( 'NONE', *, *, #132492, .T. ) ;
#194770 = CARTESIAN_POINT ( 'NONE',  ( 1.348292448571129842, 0.9904378492491233699, -1.752504823097464692 ) ) ;
#194769 = CARTESIAN_POINT ( 'NONE',  ( 4.669393045487420402, 1.064170941109745305, 1.502380130741477693 ) ) ;
#194771 = CARTESIAN_POINT ( 'NONE',  ( 3.761312542938214598, -2.295521343867617414, -0.1171695491895396041 ) ) ;
#194773 = CARTESIAN_POINT ( 'NONE',  ( 1.779899486625190264, -1.028416011161866983, -1.550745576289275895 ) ) ;
#194772 = CARTESIAN_POINT ( 'NONE',  ( -0.02900071798685524560, 0.6937575422599016051, -2.255700163050919471 ) ) ;
#194774 = CARTESIAN_POINT ( 'NONE',  ( 1.642778471875000035, -2.326041666188709112, -2.845375778867859751 ) ) ;
#194775 = FILL_AREA_STYLE_COLOUR ( '', #18996 ) ;
#194776 = CARTESIAN_POINT ( 'NONE',  ( 5.115449499555525747, 1.566912803841558732, 1.096118974231160781 ) ) ;
#194777 = CARTESIAN_POINT ( 'NONE',  ( -7.694415870955439551, 8.935572256658169010, 1.199719254218462483 ) ) ;
#194778 = CARTESIAN_POINT ( 'NONE',  ( -5.722950238744243023, 7.770137593325314285, 1.443375672974058777 ) ) ;
#194780 = CARTESIAN_POINT ( 'NONE',  ( 2.975316878787794828, 1.776827963633962559, -0.5852370025475408521 ) ) ;
#194779 = CARTESIAN_POINT ( 'NONE',  ( 5.214434122969894503, 1.932256357821033887, 0.7989942847940935122 ) ) ;
#194781 = CARTESIAN_POINT ( 'NONE',  ( 6.860062538834778678, 8.066123052471139587, -1.082531754730543083 ) ) ;
#194782 = CARTESIAN_POINT ( 'NONE',  ( 6.304252605626877504, 1.359535501544101077, -1.241908024382516240 ) ) ;
#194783 = TOROIDAL_SURFACE ( 'NONE', #177482, 10.75000000000000000, 0.5000000000000007772 ) ;
#194784 = CARTESIAN_POINT ( 'NONE',  ( 3.063252641683779753, 5.661212951017999373, 1.199719254218450271 ) ) ;
#194785 = CARTESIAN_POINT ( 'NONE',  ( -0.08058605481485492383, -8.243759731405749136, -10.99970480911961346 ) ) ;
#194786 = CARTESIAN_POINT ( 'NONE',  ( 5.250533987919646428, 0.5060912822462645400, 1.648968847961843620 ) ) ;
#194787 = CARTESIAN_POINT ( 'NONE',  ( -7.061099074618889304, 7.132370430010492868, -0.7998128361456291469 ) ) ;
#194788 = CYLINDRICAL_SURFACE ( 'NONE', #185746, 0.07999999999999993228 ) ;
#194789 = DIRECTION ( 'NONE',  ( -1.000000000000000000, 0.000000000000000000, -5.551115123125765446E-17 ) ) ;
#194790 = CARTESIAN_POINT ( 'NONE',  ( 0.000000000000000000, -8.176568542494919711, 0.000000000000000000 ) ) ;
#194791 = CARTESIAN_POINT ( 'NONE',  ( 5.190355475387732120, 1.122157983508360157, -1.858477351540340328 ) ) ;
#194792 = CARTESIAN_POINT ( 'NONE',  ( 2.789462663364688844, 1.291185895303394116, 1.290987730777813702 ) ) ;
#194793 = CARTESIAN_POINT ( 'NONE',  ( 1.516376426791886445, 0.7900930292849810410, 1.795789229542772647 ) ) ;
#194794 = CARTESIAN_POINT ( 'NONE',  ( 6.262923198102183342, -0.1061305018058098515, -2.114825283700927372 ) ) ;
#194796 = CARTESIAN_POINT ( 'NONE',  ( 1.364683531249988535, 3.676041667008087099, 0.7879004041258500513 ) ) ;
#194795 = CARTESIAN_POINT ( 'NONE',  ( 6.603114554492313104, -0.5110835225830052675, 2.243201349117603716 ) ) ;
#194797 = CARTESIAN_POINT ( 'NONE',  ( 4.004068906699964181, 7.801233831630747240, -0.1746446656625457727 ) ) ;
#194798 = CARTESIAN_POINT ( 'NONE',  ( 8.749089199520284410, 9.101692242395490240, 0.7998128361456481317 ) ) ;
#194799 = ADVANCED_FACE ( 'NONE', ( #64534 ), #54058, .T. ) ;
#194800 = CARTESIAN_POINT ( 'NONE',  ( 2.526173596586390957, -2.097057114080549844, 0.3136139059176298871 ) ) ;
#194801 = CARTESIAN_POINT ( 'NONE',  ( -3.470524135418300737, 6.032400010421219427, -1.082531754730549967 ) ) ;
#194802 = CARTESIAN_POINT ( 'NONE',  ( 5.601295902029185036, 5.735459099175467479, 0.6339577218646634815 ) ) ;
#194803 = CARTESIAN_POINT ( 'NONE',  ( -5.219525951136856357, 6.152163700156858539, -1.082531754730543971 ) ) ;
#194804 = CARTESIAN_POINT ( 'NONE',  ( 0.7958623839904412911, -1.461433461687311253, -1.466603172318406090 ) ) ;
#194806 = CARTESIAN_POINT ( 'NONE',  ( 0.7500000000000006661, 13.69791666734946567, -1.299038105676657340 ) ) ;
#194805 = CARTESIAN_POINT ( 'NONE',  ( 6.883263157960366918, 2.950764357809147143, 2.606098932787728639 ) ) ;
#194808 = ORIENTED_EDGE ( 'NONE', *, *, #15140, .F. ) ;
#194807 = CARTESIAN_POINT ( 'NONE',  ( 2.438390712420679396, -1.281362850324974989, -1.814285216940268342 ) ) ;
#194809 = CARTESIAN_POINT ( 'NONE',  ( 0.8097366424872083357, 1.363176973609769416, -1.850781266144943205 ) ) ;
#194811 = CARTESIAN_POINT ( 'NONE',  ( 5.541865367331380909, 1.381078337155069224, 1.532129260548445782 ) ) ;
#194810 = CARTESIAN_POINT ( 'NONE',  ( 2.686486993802192913, 6.285985259411197568, 0.7998128361456362523 ) ) ;
#194813 = CARTESIAN_POINT ( 'NONE',  ( 3.475000000000000533, -2.624999999999998668, 0.000000000000000000 ) ) ;
#194812 = CARTESIAN_POINT ( 'NONE',  ( 6.391743074199808916, 6.421731439513382433, -0.7998128361456481317 ) ) ;
#194814 = CARTESIAN_POINT ( 'NONE',  ( 5.712781623311797397, 7.758274208654143855, -1.599625672291283607 ) ) ;
#194815 = CARTESIAN_POINT ( 'NONE',  ( 0.2333540202161349941, 2.877056899079268870, -2.534299598574590640 ) ) ;
#194816 = CARTESIAN_POINT ( 'NONE',  ( 5.161589042655139181, 0.9124512986629171873, 1.599201395118980740 ) ) ;
#194817 = CARTESIAN_POINT ( 'NONE',  ( 3.623053363349855172, 5.249981562040033189, 1.599625672291267398 ) ) ;
#194818 = DIRECTION ( 'NONE',  ( 1.000000000000000000, 0.000000000000000000, 0.000000000000000000 ) ) ;
#194819 = CARTESIAN_POINT ( 'NONE',  ( 1.817014216480263622, -0.2154200610367338342, 1.711195096342375210 ) ) ;
#194820 = CARTESIAN_POINT ( 'NONE',  ( 1.534389036647098692, 0.6371565916030232923, 1.913260934284975345 ) ) ;
#194821 = CARTESIAN_POINT ( 'NONE',  ( -1.201851678989727383E-14, 4.134375000341417028, 1.575800808251672791 ) ) ;
#194822 = CARTESIAN_POINT ( 'NONE',  ( 2.196875584952286964, -0.6017768564574823564, -2.180865832541518667 ) ) ;
#194823 = CARTESIAN_POINT ( 'NONE',  ( 3.967482597722607363, 0.2578578757282763978, -2.090148584218749939 ) ) ;
#194824 = CARTESIAN_POINT ( 'NONE',  ( -3.149236820124241110, 6.896136400112061970, -0.7998128361456481317 ) ) ;
#194825 = CARTESIAN_POINT ( 'NONE',  ( 2.512676673363742452, 1.578732364194649573, 0.7999210992828114097 ) ) ;
#194826 = ADVANCED_BREP_SHAPE_REPRESENTATION ( '', ( #13191, #200407 ), #13801 ) ;
#194827 = CARTESIAN_POINT ( 'NONE',  ( 6.647575389402066826, 6.649926130590872120, 1.040834085586084257E-14 ) ) ;
#194829 = CARTESIAN_POINT ( 'NONE',  ( 5.179329019713509119, 1.537796090523161796, 1.700180828611449035 ) ) ;
#194828 = CARTESIAN_POINT ( 'NONE',  ( 5.058600711230250013, 5.074324715956299414, -0.7216878364870458196 ) ) ;
#194830 = B_SPLINE_CURVE_WITH_KNOTS ( 'NONE', 3,
 ( #176424, #28031, #111482, #128807 ),
 .UNSPECIFIED., .F., .F.,
 ( 4, 4 ),
 ( 0.000000000000000000, 0.002003498272494342886 ),
 .UNSPECIFIED. ) ;
#194831 = CARTESIAN_POINT ( 'NONE',  ( 4.118977087773854961, -1.761250088754966692, 0.5364436722887636622 ) ) ;
#194832 = CARTESIAN_POINT ( 'NONE',  ( -4.273844736805832767, 6.009238164405336313, 1.599625672291267398 ) ) ;
#194833 = CARTESIAN_POINT ( 'NONE',  ( 6.114364089638795186, 7.196141528409145671, 1.082531754730558626 ) ) ;
#194834 = CARTESIAN_POINT ( 'NONE',  ( -1.499999999999997780, 2.900000000000020783, 1.214306433183764966E-14 ) ) ;
#194835 = CARTESIAN_POINT ( 'NONE',  ( 4.875033280109006384, 2.045454206080063120, -0.7869404205859964474 ) ) ;
#194836 = CARTESIAN_POINT ( 'NONE',  ( -3.601662362724658895, 7.353689856487406473, -0.7998128361456281477 ) ) ;
#194837 = CARTESIAN_POINT ( 'NONE',  ( 3.834746474454188013E-15, 8.593750000682796042, 1.500000000000001554 ) ) ;
#194838 = CARTESIAN_POINT ( 'NONE',  ( -11.86145016429273014, 12.69999999999999929, -1.180000000000002158 ) ) ;
#194839 = VECTOR ( 'NONE', #193782, 1000.000000000000000 ) ;
#194840 = CARTESIAN_POINT ( 'NONE',  ( -1.364683531250012516, 4.238541667008090208, -0.7879004041258300672 ) ) ;
#194841 = CARTESIAN_POINT ( 'NONE',  ( 2.701685709380332145, -0.6039436678997743835, 1.829457556829715115 ) ) ;
#194842 = CARTESIAN_POINT ( 'NONE',  ( 0.6823417656249934904, 9.192708333674733723, 1.181850606188764807 ) ) ;
#194843 = CARTESIAN_POINT ( 'NONE',  ( -4.799223189557577207, 4.701441264013013210, 0.7216878364870317197 ) ) ;
#194844 = CARTESIAN_POINT ( 'NONE',  ( 5.818629517237746462, -0.7649446623404360102, -1.977987144599784086 ) ) ;
#194845 = CARTESIAN_POINT ( 'NONE',  ( -4.326460416536637155, 8.061637896019123062, 0.000000000000000000 ) ) ;
#194846 = EDGE_LOOP ( 'NONE', ( #148025, #166384, #76619, #198512, #196779, #101579, #4380, #155007 ) ) ;
#194849 = STYLED_ITEM ( 'NONE', ( #112401 ), #55200 ) ;
#194848 = FACE_OUTER_BOUND ( 'NONE', #79057, .T. ) ;
#194847 = CARTESIAN_POINT ( 'NONE',  ( -4.448483799059637533, 7.243629294661272588, 1.082531754730549967 ) ) ;
#194850 = CARTESIAN_POINT ( 'NONE',  ( 4.355193658487811703, 6.104145239700998538, -1.599625672291255185 ) ) ;
#194851 = CARTESIAN_POINT ( 'NONE',  ( 6.163598723784100564, 0.9525508894225949152, 1.575581956637741365 ) ) ;
#194852 = SURFACE_STYLE_USAGE ( .BOTH. , #63783 ) ;
#194853 = FACE_OUTER_BOUND ( 'NONE', #56440, .T. ) ;
#194854 = CARTESIAN_POINT ( 'NONE',  ( 0.6823417656249917140, 4.155208333674755394, 1.181850606188765695 ) ) ;
#194855 = CARTESIAN_POINT ( 'NONE',  ( 1.997219015684068344, -1.740079325084613604, 0.04332556902747128347 ) ) ;
#194856 = CARTESIAN_POINT ( 'NONE',  ( 0.3792546940144908008, -0.1001052471676349837, 1.959448305358338693 ) ) ;
#194857 = CARTESIAN_POINT ( 'NONE',  ( -0.6823417656250003738, 0.5302083336747518416, -1.181850606188749264 ) ) ;
#194858 = CARTESIAN_POINT ( 'NONE',  ( -0.3000000002818342670, 3.198312376128883194, -0.5146719259196198548 ) ) ;
#194859 = CARTESIAN_POINT ( 'NONE',  ( 5.893488898593548520, 1.633865717575968324, 1.415524914074948404 ) ) ;
#194860 = CARTESIAN_POINT ( 'NONE',  ( -8.350932551013499960, 11.83017284523606172, -1.199719254218446718 ) ) ;
#194861 = CARTESIAN_POINT ( 'NONE',  ( -6.195713011320795438, 8.251417818006149929, -1.443375672974058777 ) ) ;
#194862 = CARTESIAN_POINT ( 'NONE',  ( 5.278265135069068137, -1.204163492603943064, 1.795060720813673738 ) ) ;
#194864 = ORIENTED_EDGE ( 'NONE', *, *, #9705, .T. ) ;
#194863 = CARTESIAN_POINT ( 'NONE',  ( -0.4382560683119315903, -5.166862915010159263, -10.99126615174919408 ) ) ;
#194865 = CARTESIAN_POINT ( 'NONE',  ( 0.6823417656249899377, 4.676041667008086655, -1.181850606188754593 ) ) ;
#194866 = CARTESIAN_POINT ( 'NONE',  ( 0.6142526126209290060, 1.294576594435635108, -1.350420462534522859 ) ) ;
#194867 = CARTESIAN_POINT ( 'NONE',  ( 6.046190555029876457, 1.600718489819895174, -0.6667736897630163195 ) ) ;
#194869 = CARTESIAN_POINT ( 'NONE',  ( 2.753686713869853531, 2.180749500395392282, -0.2175628297749406803 ) ) ;
#194868 = CARTESIAN_POINT ( 'NONE',  ( -1.360316468750006669, 1.119791667008071201, -0.7853790794158921340 ) ) ;
#194870 = CARTESIAN_POINT ( 'NONE',  ( 3.048224541365350593, 0.8318171267079670361, -2.152611968481593419 ) ) ;
#194871 = CARTESIAN_POINT ( 'NONE',  ( 5.554002131806472065, 2.058623415865985518, -0.09669752385456369115 ) ) ;
#194872 = CARTESIAN_POINT ( 'NONE',  ( 1.236160255307724665, 0.3784122030587311336, 1.904561997804487428 ) ) ;
#194873 = CARTESIAN_POINT ( 'NONE',  ( -6.195713011320804320, 7.291048603704809672, -1.082531754730543083 ) ) ;
#194874 = CARTESIAN_POINT ( 'NONE',  ( -0.4655551865852132210, -8.176568542494939251, -9.512045263456258226 ) ) ;
#194875 =( NAMED_UNIT ( * ) PLANE_ANGLE_UNIT ( ) SI_UNIT ( $, .RADIAN. ) );
#194876 = CARTESIAN_POINT ( 'NONE',  ( 3.955424862866574021, -1.843446357660895041, 1.048082435718917571 ) ) ;
#194877 = CARTESIAN_POINT ( 'NONE',  ( 2.426407915648312930, -1.496052118593782065, -1.352154011671408362 ) ) ;
#194878 = CARTESIAN_POINT ( 'NONE',  ( -6.371969008298464132, 6.536311385877402458, 1.040834085586084257E-14 ) ) ;
#194879 = CARTESIAN_POINT ( 'NONE',  ( 4.032405518703926717, 1.182977813604596973, -1.862726815517960821 ) ) ;
#194880 = DIRECTION ( 'NONE',  ( -5.551115123125765446E-17, 0.000000000000000000, 1.000000000000000000 ) ) ;
#194881 = CARTESIAN_POINT ( 'NONE',  ( -2.821163330806889746, -3.104354205566886460, -1.931348577005352674 ) ) ;
#194882 = DIRECTION ( 'NONE',  ( 0.000000000000000000, 0.000000000000000000, -1.000000000000000000 ) ) ;
#194883 = CARTESIAN_POINT ( 'NONE',  ( -7.425025402139490360, 8.691559719698066289, 1.199719254218452047 ) ) ;
#194885 = CARTESIAN_POINT ( 'NONE',  ( 6.825078400183545391, 2.405270491081310968, 2.624368679222242484 ) ) ;
#194884 = CARTESIAN_POINT ( 'NONE',  ( -5.321855017605967575, 7.728530711523490027, 1.321107644836617467 ) ) ;
#194886 = CARTESIAN_POINT ( 'NONE',  ( 1.537272393291603700, 8.756440202903029046, -2.479668406359592403 ) ) ;
#194887 = ORIENTED_EDGE ( 'NONE', *, *, #206691, .F. ) ;
#194888 = CARTESIAN_POINT ( 'NONE',  ( 4.047771301309529335, 0.6961604498142616171, -1.939876652229477028 ) ) ;
#194889 = CARTESIAN_POINT ( 'NONE',  ( 1.360316468749973584, 2.786458333674735499, -0.7853790794159101196 ) ) ;
#194890 = CARTESIAN_POINT ( 'NONE',  ( 0.4304858038777367724, 6.930341212760413150, -3.770372082616246789 ) ) ;
#194891 = CARTESIAN_POINT ( 'NONE',  ( -3.554208825076827782, 7.298327395898266623, 0.7998128361456341429 ) ) ;
#194892 = CARTESIAN_POINT ( 'NONE',  ( -4.359828915246279024, 7.244161613499399799, -1.199719254218455378 ) ) ;
#194893 = CARTESIAN_POINT ( 'NONE',  ( 2.895180478094826704, -0.1506588039767979559, -2.014126839200135688 ) ) ;
#194894 = CARTESIAN_POINT ( 'NONE',  ( -1.500000000000013101, 1.170833333333352710, 0.8660254037844403729 ) ) ;
#194896 = CARTESIAN_POINT ( 'NONE',  ( 7.456621297836061757, 11.64321591421002644, 0.7216878364870438212 ) ) ;
#194895 = CARTESIAN_POINT ( 'NONE',  ( -5.666381855868691808, 5.575476684793721383, 0.000000000000000000 ) ) ;
#194897 = CARTESIAN_POINT ( 'NONE',  ( 7.494959990256193194, 7.638541498254023843, -0.7998128361456281477 ) ) ;
#194898 = CARTESIAN_POINT ( 'NONE',  ( 2.799741500914772807, -0.6479443615096942555, 1.956441213939211554 ) ) ;
#194899 = CARTESIAN_POINT ( 'NONE',  ( 2.795546247670523954, 1.458556481301529706, -1.392545902517070111 ) ) ;
#194900 = CARTESIAN_POINT ( 'NONE',  ( 1.893304937267609622, 3.295344712542843446, -0.4038802767148514383 ) ) ;
#194901 = CARTESIAN_POINT ( 'NONE',  ( 5.168682875307768931, 7.053215992657626110, -1.599625672291256295 ) ) ;
#194903 = ORIENTED_EDGE ( 'NONE', *, *, #209369, .F. ) ;
#194902 = CARTESIAN_POINT ( 'NONE',  ( -0.4957404558456298682, 7.798922855753633421, -1.990826765680301591 ) ) ;
#194904 = CARTESIAN_POINT ( 'NONE',  ( 2.794295885581669747, -1.882186412485300719, 0.7230279869864174591 ) ) ;
#194905 = CARTESIAN_POINT ( 'NONE',  ( 1.710644026344819046, -0.2265308078298749472, 1.827073587482845207 ) ) ;
#194906 = CARTESIAN_POINT ( 'NONE',  ( 0.2414294658986924358, 0.4011018576653562207, 2.272434410966933438 ) ) ;
#194907 = CARTESIAN_POINT ( 'NONE',  ( 4.766573523656222555, 7.718696989977711809, 1.199719254218452047 ) ) ;
#194908 = CARTESIAN_POINT ( 'NONE',  ( 2.126461914815626297, 1.246462439515462650, -1.765816729463750123 ) ) ;
#194909 = CARTESIAN_POINT ( 'NONE',  ( -4.338245966692955591, 5.124003718305597310, 1.082531754730560403 ) ) ;
#194910 = CARTESIAN_POINT ( 'NONE',  ( 4.927025384238821637, -1.814351377589568548, 1.091279385997992568 ) ) ;
#194911 = CARTESIAN_POINT ( 'NONE',  ( -1.219999999999996199, 6.400000000000024336, 1.214306433183764966E-14 ) ) ;
#194912 = TOROIDAL_SURFACE ( 'NONE', #56544, 11.92000000000000171, 0.08000000000000000167 ) ;
#194913 = CARTESIAN_POINT ( 'NONE',  ( 0.7076149179639171782, -1.862046558926268913, 0.1791945732521060819 ) ) ;
#194914 = AXIS2_PLACEMENT_3D ( 'NONE', #141045, #139962, #75998 ) ;
#194915 = CARTESIAN_POINT ( 'NONE',  ( 4.873880070992254510, 1.134317645522317175, 1.612277344948910285 ) ) ;
#194917 = CARTESIAN_POINT ( 'NONE',  ( 9.368320956918616105, 10.03205532593431037, 0.7216878364870458196 ) ) ;
#194916 = CARTESIAN_POINT ( 'NONE',  ( 0.6823417656249882723, 2.926041667008084879, -1.181850606188754593 ) ) ;
#194919 = CARTESIAN_POINT ( 'NONE',  ( 6.147117739887063337, -1.780134362386740721, 1.125150951816885403 ) ) ;
#194918 = CARTESIAN_POINT ( 'NONE',  ( -6.795661308947694934, 8.951357498570873261, -1.599625672291263179 ) ) ;
#194920 = CIRCLE ( 'NONE', #25457, 10.99999999999999112 ) ;
#194921 = CARTESIAN_POINT ( 'NONE',  ( 6.637176860265922684, -0.09746846054551477900, -2.068182370504913159 ) ) ;
#194922 = CARTESIAN_POINT ( 'NONE',  ( 6.602984505055297326, 7.662235663108029726, 1.199719254218462483 ) ) ;
#194923 = CARTESIAN_POINT ( 'NONE',  ( -5.215082642750900277, 9.236013516518044142, 0.000000000000000000 ) ) ;
#194924 = CARTESIAN_POINT ( 'NONE',  ( 6.875078400183575411, 7.629137130509070275, 2.455651831298297338 ) ) ;
#194925 = CARTESIAN_POINT ( 'NONE',  ( 4.750830034454851969, -1.584041870840187327, 1.173487520707878096 ) ) ;
#194926 = CARTESIAN_POINT ( 'NONE',  ( 6.099869210120771434, 1.395876734396967356, 1.460039163664628159 ) ) ;
#194927 = CARTESIAN_POINT ( 'NONE',  ( 1.499999999999985123, -0.1729166659838496101, -0.8660254037844323793 ) ) ;
#194928 = CARTESIAN_POINT ( 'NONE',  ( 4.196143101376831552, -0.8852276965729001246, 2.131346054819768909 ) ) ;
#194929 = CARTESIAN_POINT ( 'NONE',  ( 1.639586372526161684, 1.907294469559306815, -0.7855861486642725655 ) ) ;
#194930 = CARTESIAN_POINT ( 'NONE',  ( 7.293923454472087897, 8.572294120714675003, 1.082531754730558626 ) ) ;
#194932 = CARTESIAN_POINT ( 'NONE',  ( 4.908934136599710563, 7.884784371745123366, 1.199719254218451159 ) ) ;
#194931 = CIRCLE ( 'NONE', #101535, 0.08000000000000014044 ) ;
#194933 = CARTESIAN_POINT ( 'NONE',  ( 5.248941747146098180, 6.152795455539095570, -1.199719254218452047 ) ) ;
#194934 = CARTESIAN_POINT ( 'NONE',  ( -0.6823417656250212460, 2.613541667008084879, 1.181850606188767472 ) ) ;
#194935 = CARTESIAN_POINT ( 'NONE',  ( 5.011674058906918638, 5.875983152593414971, 1.199719254218452047 ) ) ;
#194936 = CARTESIAN_POINT ( 'NONE',  ( 6.765155463094761679, 6.995028916473103209, 0.7216878364870317197 ) ) ;
#194937 = CARTESIAN_POINT ( 'NONE',  ( 4.123599099448671090, 0.2696675481538573504, -2.154320840723603414 ) ) ;
#194938 = CARTESIAN_POINT ( 'NONE',  ( -3.160184708874208770, 6.440504254417610319, -0.7564881602227467861 ) ) ;
#194940 = CARTESIAN_POINT ( 'NONE',  ( 4.142028884782995135, 0.4951553702221401232, 1.773339192993342639 ) ) ;
#194939 = CARTESIAN_POINT ( 'NONE',  ( -4.934804725694236893, 4.859619722839116918, -0.7216878364870207285 ) ) ;
#194941 = EDGE_CURVE ( 'NONE', #194213, #202678, #171709, .T. ) ;
#194943 = CARTESIAN_POINT ( 'NONE',  ( 6.620655732516656400, 2.994310854299454316, 2.180639477081049993 ) ) ;
#194942 = CARTESIAN_POINT ( 'NONE',  ( 1.364683531249990311, 4.884375000341417916, 1.214306433183764966E-14 ) ) ;
#194944 = CARTESIAN_POINT ( 'NONE',  ( 5.741772062182810998, 2.188963553168365994, 0.1087695542012837302 ) ) ;
#194945 = LINE ( 'NONE', #45519, #91678 ) ;
#194946 = CARTESIAN_POINT ( 'NONE',  ( 6.121994746204825866, -1.250886037347900270, -1.885104629530814702 ) ) ;
#194947 = ORIENTED_EDGE ( 'NONE', *, *, #22206, .F. ) ;
#194948 = CARTESIAN_POINT ( 'NONE',  ( -5.067137445304809695, 6.740953878067043270, -1.444057985504534125 ) ) ;
#194949 = CARTESIAN_POINT ( 'NONE',  ( 4.614865537624940117, 8.465324746759504748, 0.2878883051726736086 ) ) ;
#194950 = CARTESIAN_POINT ( 'NONE',  ( -6.427974226210522168, 6.671927150099951298, 0.000000000000000000 ) ) ;
#194951 = CARTESIAN_POINT ( 'NONE',  ( -0.000000000000000000, 3.038454817776199413, 12.00000000000000178 ) ) ;
#194952 = CARTESIAN_POINT ( 'NONE',  ( 0.8304726968981954727, 0.1242609525908405232, 1.765545458023538572 ) ) ;
#194953 = CARTESIAN_POINT ( 'NONE',  ( 4.740889518710099004, 1.927123460305087965, 0.5820593317791241672 ) ) ;
#194954 = CARTESIAN_POINT ( 'NONE',  ( 7.091078035147269532, 8.231678114882006625, 1.199719254218462483 ) ) ;
#194955 = CARTESIAN_POINT ( 'NONE',  ( 4.366313571243555458, 0.9904663015308888818, 1.858490915321360237 ) ) ;
#194956 = CARTESIAN_POINT ( 'NONE',  ( 2.302218516519896507, 1.249579790052034456, -1.452036884154449314 ) ) ;
#194957 = CARTESIAN_POINT ( 'NONE',  ( 5.007038802148489509, 4.735966778795008381, 0.7998128361456341429 ) ) ;
#194958 = CARTESIAN_POINT ( 'NONE',  ( 3.385164793666879834, 0.04568167736355076974, 1.969186301724828336 ) ) ;
#194959 = CARTESIAN_POINT ( 'NONE',  ( 5.150651408520660723, 1.990593866887302221, 0.3411176234145337216 ) ) ;
#194960 = CARTESIAN_POINT ( 'NONE',  ( 2.008475284031425723, 1.387998011844304491, -1.254312187223500796 ) ) ;
#194961 = CARTESIAN_POINT ( 'NONE',  ( 1.785527960060459440, -1.848404783191982315, 0.6579185095809261252 ) ) ;
#194964 = ORIENTED_EDGE ( 'NONE', *, *, #99445, .T. ) ;
#194963 = CARTESIAN_POINT ( 'NONE',  ( 0.8789968191965717992, -1.730013457311157188, -0.8152767527440167861 ) ) ;
#194962 = CARTESIAN_POINT ( 'NONE',  ( 4.424228590228207914, 1.058368455644955963, -1.361911123238012111 ) ) ;
#194966 = CARTESIAN_POINT ( 'NONE',  ( 4.039966587192250103, 7.657118751792200584, 0.7216878364870298324 ) ) ;
#194965 = CARTESIAN_POINT ( 'NONE',  ( 1.454063653991678473, 0.6380318336138122159, -2.112638918738508398 ) ) ;
#194967 = CARTESIAN_POINT ( 'NONE',  ( -0.6823417656250212460, 2.113541667008083991, 1.181850606188767472 ) ) ;
#194968 = CARTESIAN_POINT ( 'NONE',  ( 8.320953590485093088, 10.73086516036454618, 1.599625672291281386 ) ) ;
#194969 = CARTESIAN_POINT ( 'NONE',  ( 11.33772463945036790, 12.69999999999999929, -3.600000000000000977 ) ) ;
#194970 = CARTESIAN_POINT ( 'NONE',  ( -5.752737250900127997, 5.605948302338584099, 0.000000000000000000 ) ) ;
#194971 = DIRECTION ( 'NONE',  ( -0.6507913734559627184, -0.7592566023653016805, 0.000000000000000000 ) ) ;
#194972 = ADVANCED_FACE ( 'NONE', ( #34151 ), #37350, .F. ) ;
#194973 = CARTESIAN_POINT ( 'NONE',  ( 0.3794556558127279988, -0.1030994254981997954, 2.067933115924729837 ) ) ;
#194974 = CARTESIAN_POINT ( 'NONE',  ( 1.499999999999987121, 1.545833333333354487, -0.8660254037844253849 ) ) ;
#194975 = CARTESIAN_POINT ( 'NONE',  ( 7.135668919494039031, 7.219368582364847242, 1.040834085586084257E-14 ) ) ;
#194976 = CARTESIAN_POINT ( 'NONE',  ( -7.069687034522070590, 10.33538640932937724, -1.199719254218440723 ) ) ;
#194977 = CARTESIAN_POINT ( 'NONE',  ( 3.718679271898170491, 7.560485927181699317, 0.7998128361456271485 ) ) ;
#194978 = CARTESIAN_POINT ( 'NONE',  ( 5.426475896148662770, -0.9536019125786737716, -1.894055658958586852 ) ) ;
#194979 = CARTESIAN_POINT ( 'NONE',  ( 5.571474780572990504, 5.464751763615448787, 0.7998128361456352531 ) ) ;
#194980 = CARTESIAN_POINT ( 'NONE',  ( -0.6823417656250003738, 2.717708333674753618, -1.181850606188749264 ) ) ;
#194981 = ORIENTED_EDGE ( 'NONE', *, *, #118661, .F. ) ;
#194982 = CARTESIAN_POINT ( 'NONE',  ( -1.201851678989727383E-14, 3.212500000000018119, 1.732050807568877637 ) ) ;
#194984 = CARTESIAN_POINT ( 'NONE',  ( 4.196412238629597447, 4.854568018944682706, -1.199719254218452047 ) ) ;
#194983 = CARTESIAN_POINT ( 'NONE',  ( 6.092239754786219486, 0.9682357284593717806, -1.706234036142616928 ) ) ;
#194985 = CARTESIAN_POINT ( 'NONE',  ( 4.147814418418220406, -0.1948115906579734602, -2.006652602119996853 ) ) ;
#194986 = CARTESIAN_POINT ( 'NONE',  ( 3.256958599878871485, 0.04175330623504669436, -1.915424027289241993 ) ) ;
#194987 =( NAMED_UNIT ( * ) SI_UNIT ( $, .STERADIAN. ) SOLID_ANGLE_UNIT ( ) );
#194988 = CARTESIAN_POINT ( 'NONE',  ( 1.962683346935737205, -2.005255389829229351, -0.8846387633431598285 ) ) ;
#194989 = CARTESIAN_POINT ( 'NONE',  ( -11.04986239659823433, 11.10939231485699175, -1.056426191432995765 ) ) ;
#194990 = CARTESIAN_POINT ( 'NONE',  ( -1.402160292154681736E-14, 0.2437500006828163535, 1.732050807568877637 ) ) ;
#194991 = CARTESIAN_POINT ( 'NONE',  ( 5.361592829351686795, -1.589796019859390563, -1.235070861824426824 ) ) ;
#194992 = CARTESIAN_POINT ( 'NONE',  ( -7.881367368245678406, 8.089350105908421185, 0.7998128361456602331 ) ) ;
#194994 = CARTESIAN_POINT ( 'NONE',  ( 6.081681791882147969, -0.7128978460711818954, 1.993742607474026984 ) ) ;
#194993 = CARTESIAN_POINT ( 'NONE',  ( -3.687454593236990430, 4.364747115940301292, 1.082531754730560403 ) ) ;
#194995 = CARTESIAN_POINT ( 'NONE',  ( -1.364683531250000748, 8.921875000341403350, 0.000000000000000000 ) ) ;
#194997 = CARTESIAN_POINT ( 'NONE',  ( -6.474900878978163021, 9.711745571186627402, -1.199719254218452047 ) ) ;
#194996 = CARTESIAN_POINT ( 'NONE',  ( 2.999644136165266595, -2.088248420355208523, 0.1050208477483879216 ) ) ;
#194999 = VERTEX_POINT ( 'NONE', #70890 ) ;
#194998 = CARTESIAN_POINT ( 'NONE',  ( 1.482971688208828187, 1.595641881047437538, -0.6553127101004208033 ) ) ;
#195000 = CARTESIAN_POINT ( 'NONE',  ( 4.904590598983499028, -2.104870323260544129, -0.2570220051709286579 ) ) ;
#195001 = CARTESIAN_POINT ( 'NONE',  ( 4.774442650306744085, 8.721933525333202653, -0.7998128361456281477 ) ) ;
#195002 =( NAMED_UNIT ( * ) SI_UNIT ( $, .STERADIAN. ) SOLID_ANGLE_UNIT ( ) );
#195003 = FACE_OUTER_BOUND ( 'NONE', #72614, .T. ) ;
#195004 = DIRECTION ( 'NONE',  ( 0.000000000000000000, 0.000000000000000000, -1.000000000000000000 ) ) ;
#195005 = CARTESIAN_POINT ( 'NONE',  ( 5.120175567455225618, 9.125288595339771547, -0.7998128361456281477 ) ) ;
#195006 = ORIENTED_EDGE ( 'NONE', *, *, #107076, .F. ) ;
#195008 = TOROIDAL_SURFACE ( 'NONE', #8222, 6.500000000000000000, 0.2999999999999999889 ) ;
#195007 = CARTESIAN_POINT ( 'NONE',  ( -0.7500000000000006661, 9.458333333333332149, -1.299038105676657340 ) ) ;
#195009 = ORIENTED_EDGE ( 'NONE', *, *, #70737, .T. ) ;
#195011 = CARTESIAN_POINT ( 'NONE',  ( 2.191808917380858812, 1.115356421127197351, 1.427258924012535735 ) ) ;
#195010 = CARTESIAN_POINT ( 'NONE',  ( 6.717138760927786834, 6.801359740696030443, -0.7998128361456481317 ) ) ;
#195012 = CARTESIAN_POINT ( 'NONE',  ( -7.152089726408780379, 8.302858421353754181, -1.199719254218446718 ) ) ;
#195013 = VERTEX_POINT ( 'NONE', #169485 ) ;
#195014 = CARTESIAN_POINT ( 'NONE',  ( 3.083589872104280705, 5.684939719841914929, 1.199719254218450271 ) ) ;
#195015 = CIRCLE ( 'NONE', #142187, 0.08000000000000012657 ) ;
#195016 = VERTEX_POINT ( 'NONE', #103424 ) ;
#195017 = CARTESIAN_POINT ( 'NONE',  ( 4.875038752565570732, 7.845239757038595663, -1.199719254218452047 ) ) ;
#195018 = CARTESIAN_POINT ( 'NONE',  ( 2.209342481274043646, 1.400903122447524796, 1.148441741360214152 ) ) ;
#195019 = CARTESIAN_POINT ( 'NONE',  ( 6.539320575229256249, 4.699150603835311912, 2.459441311396874941 ) ) ;
#195020 = CARTESIAN_POINT ( 'NONE',  ( 1.499999999999996891, 9.145833333333330373, -0.8660254037844378194 ) ) ;
#195021 = CARTESIAN_POINT ( 'NONE',  ( 4.147051400439892177, 7.400425289818373109, 0.7480841269332880739 ) ) ;
#195022 = ORIENTED_EDGE ( 'NONE', *, *, #96265, .T. ) ;
#195023 = CARTESIAN_POINT ( 'NONE',  ( 4.176097997218494839, -0.9553649929725913648, -1.596950837584124816 ) ) ;
#195024 = CARTESIAN_POINT ( 'NONE',  ( 1.493601000189462624, -1.900943851588072997, 0.2360903481228252554 ) ) ;
#195025 = CARTESIAN_POINT ( 'NONE',  ( 0.2701547006425785713, -1.196777392914155635, 1.378664180083796875 ) ) ;
#195026 = CARTESIAN_POINT ( 'NONE',  ( 4.871153761480781164, 8.051123856976298399, 0.9350251597124116243 ) ) ;
#195027 = CARTESIAN_POINT ( 'NONE',  ( 0.000000000000000000, 6.999999999999999112, 0.000000000000000000 ) ) ;
#195028 = CARTESIAN_POINT ( 'NONE',  ( 4.594924845400013780, 8.373833185659544043, 0.04553248676899754321 ) ) ;
#195029 = CARTESIAN_POINT ( 'NONE',  ( -4.460269349215930212, 4.305995116947750390, 1.214306433183764966E-14 ) ) ;
#195030 = CARTESIAN_POINT ( 'NONE',  ( 8.432808358020029260, 8.940623960552603222, 0.7216878364870438212 ) ) ;
#195031 = CARTESIAN_POINT ( 'NONE',  ( 4.821133434317745881, -1.757446901322982979, -0.8890814742016742711 ) ) ;
#195032 = CARTESIAN_POINT ( 'NONE',  ( -3.879604511804807032, 7.677955697080923514, 0.7998128361456341429 ) ) ;
#195033 = CARTESIAN_POINT ( 'NONE',  ( -11.89942855770813956, 12.22000000000000064, 0.6999999999999992895 ) ) ;
#195034 = CARTESIAN_POINT ( 'NONE',  ( 0.05869050280414740001, -1.868530317513932504, -0.9378765995749788198 ) ) ;
#195035 = DIRECTION ( 'NONE',  ( 0.000000000000000000, 0.000000000000000000, 1.000000000000000000 ) ) ;
#195036 = CARTESIAN_POINT ( 'NONE',  ( 5.561526637868618117, 0.3756393653304244129, -1.889249976882242610 ) ) ;
#195037 = CARTESIAN_POINT ( 'NONE',  ( -6.693975156845199059, 8.832723654451292816, 1.599625672291283607 ) ) ;
#195038 = CARTESIAN_POINT ( 'NONE',  ( 1.711645973048509850, -1.812212506298327197, 0.2199163931802459171 ) ) ;
#195039 = CARTESIAN_POINT ( 'NONE',  ( 2.385638622766753425, 2.017150886971270651, -0.8956362484653991318 ) ) ;
#195040 = CARTESIAN_POINT ( 'NONE',  ( -0.1405747822309927342, -1.479430311965252542, -1.211566217618691210 ) ) ;
#195041 = ORIENTED_EDGE ( 'NONE', *, *, #60090, .F. ) ;
#195042 = ORIENTED_EDGE ( 'NONE', *, *, #35345, .T. ) ;
#195043 = CARTESIAN_POINT ( 'NONE',  ( 0.9769314595147912117, 1.818477718279483568, 0.7569839642056105378 ) ) ;
#195044 = CARTESIAN_POINT ( 'NONE',  ( 1.259210993675137225, 1.913035009642606754, -0.3336937221413670551 ) ) ;
#195045 = CARTESIAN_POINT ( 'NONE',  ( 1.071638489536786309, 1.528508772698907059, -1.314793605459969372 ) ) ;
#195047 = CARTESIAN_POINT ( 'NONE',  ( 5.752756584690191133, -0.4505887142414471969, -1.805456089952769183 ) ) ;
#195046 = CARTESIAN_POINT ( 'NONE',  ( -4.145761110728687804, 8.058748072483927771, -0.7998128361456481317 ) ) ;
#195048 = CARTESIAN_POINT ( 'NONE',  ( 6.170896192875352959, 7.228408975556602556, 1.199719254218453823 ) ) ;
#195049 = CARTESIAN_POINT ( 'NONE',  ( -2.277139237642805902, 2.743616490267797747, 2.500000000000000000 ) ) ;
#195050 = CARTESIAN_POINT ( 'NONE',  ( 1.436717746206296997, 7.422220963914728742, -4.237135035835245311 ) ) ;
#195051 = CARTESIAN_POINT ( 'NONE',  ( -3.744022975668147790, 7.519777238254810925, -0.7998128361456281477 ) ) ;
#195052 = CARTESIAN_POINT ( 'NONE',  ( -5.725286006720766707, 9.901527117808042178, 0.7998128361456291469 ) ) ;
#195053 = CARTESIAN_POINT ( 'NONE',  ( 1.611130907606239004, -0.2639259086049255965, 2.175532687872412829 ) ) ;
#195054 = CARTESIAN_POINT ( 'NONE',  ( 3.470524135418292300, 5.072030796119872953, -1.443375672974057666 ) ) ;
#195055 = VERTEX_POINT ( 'NONE', #1624 ) ;
#195056 = CARTESIAN_POINT ( 'NONE',  ( 11.00029612940780410, -6.479296433800342925, 0.04006801626471419991 ) ) ;
#195057 = FACE_OUTER_BOUND ( 'NONE', #77913, .T. ) ;
#195058 = CARTESIAN_POINT ( 'NONE',  ( 1.295219883412350503, 1.381147610352757127, 1.194082977437810333 ) ) ;
#195059 = CARTESIAN_POINT ( 'NONE',  ( 1.387358672525591308, 7.251968950354787502, 4.302625267139676524 ) ) ;
#195060 = CARTESIAN_POINT ( 'NONE',  ( -5.264643720808155791, 5.036505850564608089, 0.000000000000000000 ) ) ;
#195061 = CARTESIAN_POINT ( 'NONE',  ( -0.3970953499397937292, 3.114959765369129219, -1.961950730382394870 ) ) ;
#195062 = CARTESIAN_POINT ( 'NONE',  ( 6.509000000000053632, 2.033894086284238956, 2.405029747421689290 ) ) ;
#195063 = CARTESIAN_POINT ( 'NONE',  ( 9.297140650669039275, 11.86975006391249643, 1.599625672291281386 ) ) ;
#195064 = CARTESIAN_POINT ( 'NONE',  ( 0.7856181369204550125, 1.292946451617222436, 1.428335531958953464 ) ) ;
#195065 = CARTESIAN_POINT ( 'NONE',  ( 4.170719094083116474, 1.390339895272204362, -1.384257141873693087 ) ) ;
#195066 = CARTESIAN_POINT ( 'NONE',  ( -6.991200766141138168, 11.30815132714001159, 0.7998128361456481317 ) ) ;
#195067 = CARTESIAN_POINT ( 'NONE',  ( 6.634017235788401301, 6.634108284708264414, 0.7998128361456341429 ) ) ;
#195068 = ADVANCED_FACE ( 'NONE', ( #117605 ), #201948, .F. ) ;
#195069 = CARTESIAN_POINT ( 'NONE',  ( 4.616832073239669043, -0.1072513232249286408, 2.189039617437993357 ) ) ;
#195070 = CIRCLE ( 'NONE', #126042, 0.09999999999999982514 ) ;
#195071 = CARTESIAN_POINT ( 'NONE',  ( 3.310162060030825248, 7.013606170011281726, -0.7998128361456291469 ) ) ;
#195072 = CARTESIAN_POINT ( 'NONE',  ( 4.434477146351770926, -1.196200190851111733, 1.689492296227593116 ) ) ;
#195074 = CARTESIAN_POINT ( 'NONE',  ( -0.6823417656250212460, 1.613541667008083769, 1.181850606188755259 ) ) ;
#195073 = SURFACE_STYLE_FILL_AREA ( #83442 ) ;
#195075 =( BOUNDED_SURFACE ( )  B_SPLINE_SURFACE ( 1, 2, ( 
 ( #16315, #198272, #83465, #36843, #150627, #68264, #118174, #116035, #99726, #1131, #133330, #50980, #183103, #34713, #24858, #202527, #107258, #171119, #38996, #104002, #154882, #122473, #56312, #190555, #174348, #124597, #106178, #7535, #22713, #73619, #153815, #136507, #204662, #6465, #137576, #88827, #42211, #203594, #187366, #5386, #139718, #25926, #90960, #173278, #72542, #188433, #40068, #92034, #71463, #138640, #74694, #37928, #55246, #170045, #172204, #121393, #157026, #23792, #140798, #8611, #206809, #189503, #89899, #54176, #120316, #155950, #58442, #205742, #108328, #57375, #105081, #123538, #158092, #41148, #9680, #186290, #21631, #87739, #63765, #195911, #159137, #194832, #193760, #162348, #125655, #110459, #46466, #31283, #12866, #13931, #95229, #60564, #191617, #126723, #80011, #10739, #47547, #28072, #144005, #175405, #78940, #145062, #94166, #160206, #11808, #177529, #146116, #112589, #211066, #45407, #163415, #43279, #77883, #111523, #75756, #141866, #62690, #209997, #61639, #128849, #76809, #207876, #127806, #29142, #59498, #129924, #178600, #176460, #212127, #109400, #30209, #113659, #161279, #142929, #96296, #179663, #97358, #26989, #93096, #44337, #208929, #192684, #34463, #151434, #184965, #182845, #167670, #117921, #52853, #134142, #183915, #130974, #16057, #200149, #201213, #19271, #51803, #196964, #866, #3006, #82141, #99476, #85353, #69076, #1940, #64828, #135196, #17128, #35526, #132013, #98406, #50719, #198023, #83204, #100535, #101602, #48602, #166610, #68000, #199072, #49651, #148234, #115774, #114720, #102678, #118987, #164471, #180715, #32338, #18198, #84283, #33397, #165535, #149285, #116844, #36591, #14991, #150370, #133075, #81085, #214236, #66932, #147172, #213199, #65863, #181764, #170871, #22462, #105920, #103750, #168736, #88574, #204408, #152490, #8362, #139459, #203342, #40894, #4073, #123291, #90714, #187110, #37674, #38743, #154631, #140549, #171946, #56060, #137326, #6211, #86425, #188179, #156776, #124348, #122218, #106999, #57125, #206562, #73356, #189255, #70143, #169801, #205491, #58189, #173024, #24604, #136255, #72281, #74445, #21390, #104825, #190305, #41963, #155696, #202275, #20337, #138390, #53926, #71210, #87499, #39814, #54995, #23535, #89644, #120063, #186038, #7279, #153564, #5134, #121147, #109148, #76564, #207627, #195665, #211887, #191368, #141618, #78694, #161028, #208684, #108074, #25676, #61392, #210827, #77634, #62452, #177281, #142674, #192436, #194582, #12622, #13693, #91783, #63527, #60313, #96051, #79762, #43036, #144820, #11564, #46228, #157840, #126473, #128615, #129680, #45164, #112345, #127552, #92849, #9436, #158895, #178357, #175160, #145879, #44091, #176219, #110211, #174104, #26748, #10491, #125403, #193523, #75506, #29964, #162105, #27821, #159959, #93919, #59245, #143756, #209751, #111277, #28897, #94981, #80845, #99230, #32089, #1682, #82955, #51539, #133886, #179420, #84019, #68816, #113414, #167419, #14753, #50467, #147985, #165280, #115526, #131764, #150110, #149028, #85091, #34203, #181521, #183656, #49406, #67736, #35261, #65615, #16874, #116586, #98176, #146935, #101337, #33150, #604, #66669, #132818, #212952, #196721, #19010, #48361, #47299, #151175, #64589, #198821, #114473, #197769, #15812, #2746, #100277, #199893, #182581, #164224, #166343, #134938, #17934, #180473, #117664, #31041, #130729, #81897, #97116, #213994, #163168, #56864, #87229, #171674, #184707, #121948, #204138, #7016, #172764, #8104, #105646, #86162, #52593, #20073, #153292, #205223, #104560, #72016, #5946, #138129, #118720, #55792, #23270, #203082, #74193, #36329, #89382, #102408, #155430, #21123, #103481, #168475, #4869, #186851, #120877, #40633, #24338, #188991, #170604, #187914, #70947, #39545, #3804, #200944, #54727, #137058, #202003, #169544, #106736, #73092, #139192, #22191, #185774, #123039, #90447, #156514, #53661, #152233, #69878, #135988, #119794, #37407, #38483, #88305, #154369, #29447, #113961, #124094, #64071, #146416, #163714, #115012, #164765, #47850, #25421, #206306, #173845, #95538, #147465, #46777, #14221, #162648, #80316, #57930 ),
 ( #212429, #161588, #13175, #79253, #30517, #213487, #179958, #130215, #112891, #16356, #41710, #145371, #178903, #140286, #190058, #196209, #211370, #62995, #31581, #78179, #107820, #129164, #96598, #91527, #197253, #97655, #177830, #15296, #157586, #81381, #65110, #195141, #9181, #131266, #48892, #181009, #32629, #98706, #111828, #144307, #210301, #61941, #128099, #194057, #45709, #20623, #185260, #120357, #201499, #36884, #198308, #83501, #53145, #54219, #86711, #119275, #49948, #68302, #4362, #149583, #166905, #152780, #70431, #69368, #132301, #136547, #84576, #102967, #199372, #165833, #118211, #51018, #150664, #35821, #169025, #116069, #19568, #135477, #2226, #184198, #82435, #170087, #85643, #134435, #200437, #151728, #17417, #148525, #52084, #101897, #66156, #202567, #186334, #117139, #37968, #182059, #104041, #91, #100820, #1167, #18498, #167962, #33690, #3300, #99766, #183142, #67231, #133365, #34747, #158130, #191655, #189540, #174389, #124638, #59536, #140837, #190595, #137617, #22749, #206850, #207915, #25967, #58482, #203633, #7575, #9721, #88867, #106217, #92072, #75797, #8653, #71506, #141905, #23831, #42252, #138682, #105119, #57413, #204701, #89936, #41188, #108365, #55285, #173317, #74732, #205784, #56351, #154922, #122513, #121434, #109438, #125696, #171159, #187403, #43320, #21674, #188474, #87782, #153856, #107295, #5427, #123578, #39035, #91002, #40105, #172243, #6506, #72581, #155987, #73660, #139760, #24896, #157065, #81127, #44377, #80053, #78984, #47588, #10776, #210038, #146156, #131014, #112630, #113702, #194873, #160245, #76850, #11845, #179706, #176499, #31323, #142969, #193798, #161320, #95272, #15035, #213237, #163455, #145103, #46508, #61678, #178640, #192723, #175444, #29183, #27029, #126763, #60604, #97399, #77922, #94205, #147212, #127846, #212172, #159176, #96336, #30252, #195952, #64869, #197006, #63806, #110500, #93137, #208972, #45447, #48641, #211107, #162392, #13969, #129964, #28110, #144041, #111562, #177570, #12904, #62731, #128892, #65907, #181807, #115820, #201249, #82181, #133114, #100574, #34500, #168773, #152527, #102716, #84322, #200186, #906, #51839, #132053, #114759, #182884, #199111, #33440, #66975, #20378, #99517, #165574, #198063, #117957, #4112, #69114, #85390, #149328, #166647, #18238, #70181, #49692, #50756, #52890, #16097, #17169, #148275, #150408, #83243, #135236, #1975, #119025, #185007, #32383, #151474, #136293, #180756, #86463, #214274, #183952, #116885, #68038, #134178, #35562, #3045, #101643, #202314, #167709, #19311, #36631, #98449, #164513, #42006, #72321, #171985, #57164, #104862, #21427, #108114, #39855, #89686, #7320, #73398, #87536, #203381, #190344, #55034, #53963, #174141, #153603, #155735, #121182, #204446, #22499, #25715, #107036, #140588, #23577, #38780, #40932, #157881, #123327, #187151, #189290, #88611, #206600, #37713, #8399, #91824, #138427, #137364, #56100, #122256, #9474, #205529, #139501, #154666, #188215, #186079, #173062, #75547, #141656, #24642, #58228, #156812, #120101, #90752, #74484, #169840, #170906, #124386, #103789, #5175, #71248, #6252, #105961, #129715, #60350, #77671, #145913, #211925, #194618, #43074, #63559, #209787, #96086, #110248, #76602, #28932, #176257, #61425, #161066, #178390, #109187, #144855, #46260, #177317, #27858, #208724, #93955, #92887, #80879, #97151, #142715, #26782, #30001, #112378, #159996, #207668, #125446, #12657, #162140, #95016, #13728, #62488, #11597, #143791, #79801, #195700, #113449, #191407, #163205, #127591, #47334, #179454, #126513, #31077, #111314, #14788, #175199, #193558, #59287, #158932, #210862, #10528, #78730, #192475, #44128, #45201, #128652, #82991, #36370, #51579, #643, #32128, #150150, #1720, #165316, #16911, #149066, #34244, #2784, #183695, #67777, #50505, #20113, #48400, #66708, #182621, #146969, #212985, #133926, #132853, #198858, #84061, #81933, #64624, #116627, #100316, #130763, #200983, #117704, #166382, #52630, #184743, #134975, #17974, #199932, #33186, #35302, #164260, #196759, #101379, #167454, #148019, #99268, #118758, #214029, #197810, #15848, #19049, #102447 ) ),
 .UNSPECIFIED., .F., .F., .F. ) 
 B_SPLINE_SURFACE_WITH_KNOTS ( ( 2, 2 ),
 ( 3, 2, 2, 2, 2, 2, 2, 2, 2, 2, 2, 2, 2, 2, 2, 2, 2, 2, 2, 2, 2, 2, 2, 2, 2, 2, 2, 2, 2, 2, 2, 2, 2, 2, 2, 2, 2, 2, 2, 2, 2, 2, 2, 2, 2, 2, 2, 2, 2, 2, 2, 2, 2, 2, 2, 2, 2, 2, 2, 2, 2, 2, 2, 2, 2, 2, 2, 2, 2, 2, 2, 2, 2, 2, 2, 2, 2, 2, 2, 2, 2, 2, 2, 2, 2, 2, 2, 2, 2, 2, 2, 2, 2, 2, 2, 2, 2, 2, 2, 2, 2, 2, 2, 2, 2, 2, 2, 2, 2, 2, 2, 2, 2, 2, 2, 2, 2, 2, 2, 2, 2, 2, 2, 2, 2, 2, 2, 2, 2, 2, 2, 2, 2, 2, 2, 2, 2, 2, 2, 2, 2, 2, 2, 2, 2, 2, 2, 2, 2, 2, 2, 2, 2, 2, 2, 2, 2, 2, 2, 2, 2, 2, 2, 2, 2, 2, 2, 2, 2, 2, 2, 2, 2, 2, 2, 2, 2, 2, 2, 2, 2, 2, 2, 2, 2, 2, 2, 2, 2, 2, 2, 2, 2, 2, 2, 2, 2, 2, 2, 2, 2, 2, 2, 2, 2, 2, 2, 2, 2, 2, 2, 2, 2, 2, 2, 2, 2, 2, 2, 2, 2, 2, 2, 2, 2, 2, 2, 2, 2, 2, 2, 2, 2, 2, 2, 2, 2, 2, 2, 2, 3 ),
 ( 0.000000000000000000, 1.000000000000000000 ),
 ( 0.000000000000000000, 0.004166666666666666609, 0.008333333333333333218, 0.01250000000000000069, 0.01666666666666666644, 0.02083333333333333218, 0.02500000000000000139, 0.02916666666666666713, 0.03333333333333333287, 0.03749999999999999861, 0.04166666666666666435, 0.04583333333333333010, 0.05000000000000000278, 0.05416666666666666852, 0.05833333333333333426, 0.06250000000000000000, 0.06666666666666666574, 0.07083333333333333148, 0.07499999999999999722, 0.07916666666666666297, 0.08333333333333332871, 0.08749999999999999445, 0.09166666666666666019, 0.09583333333333333981, 0.1000000000000000056, 0.1041666666666666713, 0.1083333333333333370, 0.1125000000000000028, 0.1166666666666666685, 0.1208333333333333343, 0.1250000000000000000, 0.1291666666666666796, 0.1333333333333333315, 0.1375000000000000111, 0.1416666666666666630, 0.1458333333333333426, 0.1499999999999999944, 0.1541666666666666741, 0.1583333333333333259, 0.1625000000000000056, 0.1666666666666666574, 0.1708333333333333370, 0.1749999999999999889, 0.1791666666666666685, 0.1833333333333333204, 0.1875000000000000000, 0.1916666666666666796, 0.1958333333333333315, 0.2000000000000000111, 0.2041666666666666630, 0.2083333333333333426, 0.2124999999999999944, 0.2166666666666666741, 0.2208333333333333259, 0.2250000000000000056, 0.2291666666666666574, 0.2333333333333333370, 0.2374999999999999889, 0.2416666666666666685, 0.2458333333333333204, 0.2500000000000000000, 0.2541666666666666519, 0.2583333333333333592, 0.2625000000000000111, 0.2666666666666666630, 0.2708333333333333148, 0.2750000000000000222, 0.2791666666666666741, 0.2833333333333333259, 0.2874999999999999778, 0.2916666666666666852, 0.2958333333333333370, 0.2999999999999999889, 0.3041666666666666408, 0.3083333333333333481, 0.3125000000000000000, 0.3166666666666666519, 0.3208333333333333592, 0.3250000000000000111, 0.3291666666666666630, 0.3333333333333333148, 0.3375000000000000222, 0.3416666666666666741, 0.3458333333333333259, 0.3499999999999999778, 0.3541666666666666852, 0.3583333333333333370, 0.3624999999999999889, 0.3666666666666666408, 0.3708333333333333481, 0.3750000000000000000, 0.3791666666666666519, 0.3833333333333333592, 0.3875000000000000111, 0.3916666666666666630, 0.3958333333333333148, 0.4000000000000000222, 0.4041666666666666741, 0.4083333333333333259, 0.4124999999999999778, 0.4166666666666666852, 0.4208333333333333370, 0.4249999999999999889, 0.4291666666666666408, 0.4333333333333333481, 0.4375000000000000000, 0.4416666666666666519, 0.4458333333333333592, 0.4500000000000000111, 0.4541666666666666630, 0.4583333333333333148, 0.4625000000000000222, 0.4666666666666666741, 0.4708333333333333259, 0.4749999999999999778, 0.4791666666666666852, 0.4833333333333333370, 0.4874999999999999889, 0.4916666666666666408, 0.4958333333333333481, 0.5000000000000000000, 0.5041666666666666519, 0.5083333333333333037, 0.5124999999999999556, 0.5166666666666667185, 0.5208333333333333703, 0.5250000000000000222, 0.5291666666666666741, 0.5333333333333333259, 0.5374999999999999778, 0.5416666666666666297, 0.5458333333333332815, 0.5500000000000000444, 0.5541666666666666963, 0.5583333333333333481, 0.5625000000000000000, 0.5666666666666666519, 0.5708333333333333037, 0.5749999999999999556, 0.5791666666666667185, 0.5833333333333333703, 0.5875000000000000222, 0.5916666666666666741, 0.5958333333333333259, 0.5999999999999999778, 0.6041666666666666297, 0.6083333333333332815, 0.6125000000000000444, 0.6166666666666666963, 0.6208333333333333481, 0.6250000000000000000, 0.6291666666666666519, 0.6333333333333333037, 0.6374999999999999556, 0.6416666666666667185, 0.6458333333333333703, 0.6500000000000000222, 0.6541666666666666741, 0.6583333333333333259, 0.6624999999999999778, 0.6666666666666666297, 0.6708333333333332815, 0.6750000000000000444, 0.6791666666666666963, 0.6833333333333333481, 0.6875000000000000000, 0.6916666666666666519, 0.6958333333333333037, 0.6999999999999999556, 0.7041666666666667185, 0.7083333333333333703, 0.7125000000000000222, 0.7166666666666666741, 0.7208333333333333259, 0.7249999999999999778, 0.7291666666666666297, 0.7333333333333332815, 0.7375000000000000444, 0.7416666666666666963, 0.7458333333333333481, 0.7500000000000000000, 0.7541666666666666519, 0.7583333333333333037, 0.7624999999999999556, 0.7666666666666667185, 0.7708333333333333703, 0.7750000000000000222, 0.7791666666666666741, 0.7833333333333333259, 0.7874999999999999778, 0.7916666666666666297, 0.7958333333333332815, 0.8000000000000000444, 0.8041666666666666963, 0.8083333333333333481, 0.8125000000000000000, 0.8166666666666666519, 0.8208333333333333037, 0.8249999999999999556, 0.8291666666666667185, 0.8333333333333333703, 0.8375000000000000222, 0.8416666666666666741, 0.8458333333333333259, 0.8499999999999999778, 0.8541666666666666297, 0.8583333333333332815, 0.8625000000000000444, 0.8666666666666666963, 0.8708333333333333481, 0.8750000000000000000, 0.8791666666666666519, 0.8833333333333333037, 0.8874999999999999556, 0.8916666666666667185, 0.8958333333333333703, 0.9000000000000000222, 0.9041666666666666741, 0.9083333333333333259, 0.9124999999999999778, 0.9166666666666666297, 0.9208333333333332815, 0.9250000000000000444, 0.9291666666666666963, 0.9333333333333333481, 0.9375000000000000000, 0.9416666666666666519, 0.9458333333333333037, 0.9499999999999999556, 0.9541666666666667185, 0.9583333333333333703, 0.9625000000000000222, 0.9666666666666666741, 0.9708333333333333259, 0.9749999999999999778, 0.9791666666666666297, 0.9833333333333332815, 0.9875000000000000444, 0.9916666666666666963, 0.9958333333333333481, 1.000000000000000000 ),
 .UNSPECIFIED. ) 
 GEOMETRIC_REPRESENTATION_ITEM ( )  RATIONAL_B_SPLINE_SURFACE ( (
 ( 1.000000000000000000, 0.8660254037844387076, 1.000000000000000000, 0.8660254037844387076, 1.000000000000000000, 0.8660254037844387076, 1.000000000000000000, 0.8660254037844387076, 1.000000000000000000, 0.8660254037844387076, 1.000000000000000000, 0.8660254037844387076, 1.000000000000000000, 0.8660254037844387076, 1.000000000000000000, 0.8660254037844387076, 1.000000000000000000, 0.8660254037844387076, 1.000000000000000000, 0.8660254037844387076, 1.000000000000000000, 0.8660254037844387076, 1.000000000000000000, 0.8660254037844387076, 1.000000000000000000, 0.8660254037844387076, 1.000000000000000000, 0.8660254037844387076, 1.000000000000000000, 0.8660254037844387076, 1.000000000000000000, 0.8660254037844387076, 1.000000000000000000, 0.8660254037844387076, 1.000000000000000000, 0.8660254037844387076, 1.000000000000000000, 0.8660254037844387076, 1.000000000000000000, 0.8660254037844387076, 1.000000000000000000, 0.8660254037844387076, 1.000000000000000000, 0.8660254037844387076, 1.000000000000000000, 0.8660254037844387076, 1.000000000000000000, 0.8660254037844387076, 1.000000000000000000, 0.8660254037844387076, 1.000000000000000000, 0.8660254037844387076, 1.000000000000000000, 0.8660254037844387076, 1.000000000000000000, 0.8660254037844387076, 1.000000000000000000, 0.8660254037844387076, 1.000000000000000000, 0.8660254037844387076, 1.000000000000000000, 0.8660254037844387076, 1.000000000000000000, 0.8660254037844387076, 1.000000000000000000, 0.8660254037844387076, 1.000000000000000000, 0.8660254037844387076, 1.000000000000000000, 0.8660254037844387076, 1.000000000000000000, 0.8660254037844387076, 1.000000000000000000, 0.8660254037844387076, 1.000000000000000000, 0.8660254037844387076, 1.000000000000000000, 0.8660254037844387076, 1.000000000000000000, 0.8660254037844387076, 1.000000000000000000, 0.8660254037844387076, 1.000000000000000000, 0.8660254037844387076, 1.000000000000000000, 0.8660254037844387076, 1.000000000000000000, 0.8660254037844387076, 1.000000000000000000, 0.8660254037844387076, 1.000000000000000000, 0.8660254037844387076, 1.000000000000000000, 0.8660254037844387076, 1.000000000000000000, 0.8660254037844387076, 1.000000000000000000, 0.8660254037844387076, 1.000000000000000000, 0.8660254037844387076, 1.000000000000000000, 0.8660254037844387076, 1.000000000000000000, 0.8660254037844387076, 1.000000000000000000, 0.8660254037844387076, 1.000000000000000000, 0.8660254037844387076, 1.000000000000000000, 0.8660254037844387076, 1.000000000000000000, 0.8660254037844387076, 1.000000000000000000, 0.8660254037844387076, 1.000000000000000000, 0.8660254037844387076, 1.000000000000000000, 0.8660254037844387076, 1.000000000000000000, 0.8660254037844387076, 1.000000000000000000, 0.8660254037844387076, 1.000000000000000000, 0.8660254037844387076, 1.000000000000000000, 0.8660254037844387076, 1.000000000000000000, 0.8660254037844387076, 1.000000000000000000, 0.8660254037844387076, 1.000000000000000000, 0.8660254037844387076, 1.000000000000000000, 0.8660254037844387076, 1.000000000000000000, 0.8660254037844387076, 1.000000000000000000, 0.8660254037844387076, 1.000000000000000000, 0.8660254037844387076, 1.000000000000000000, 0.8660254037844387076, 1.000000000000000000, 0.8660254037844387076, 1.000000000000000000, 0.8660254037844387076, 1.000000000000000000, 0.8660254037844387076, 1.000000000000000000, 0.8660254037844387076, 1.000000000000000000, 0.8660254037844387076, 1.000000000000000000, 0.8660254037844387076, 1.000000000000000000, 0.8660254037844387076, 1.000000000000000000, 0.8660254037844387076, 1.000000000000000000, 0.8660254037844387076, 1.000000000000000000, 0.8660254037844387076, 1.000000000000000000, 0.8660254037844387076, 1.000000000000000000, 0.8660254037844387076, 1.000000000000000000, 0.8660254037844387076, 1.000000000000000000, 0.8660254037844387076, 1.000000000000000000, 0.8660254037844387076, 1.000000000000000000, 0.8660254037844387076, 1.000000000000000000, 0.8660254037844387076, 1.000000000000000000, 0.8660254037844387076, 1.000000000000000000, 0.8660254037844387076, 1.000000000000000000, 0.8660254037844387076, 1.000000000000000000, 0.8660254037844387076, 1.000000000000000000, 0.8660254037844387076, 1.000000000000000000, 0.8660254037844387076, 1.000000000000000000, 0.8660254037844387076, 1.000000000000000000, 0.8660254037844387076, 1.000000000000000000, 0.8660254037844387076, 1.000000000000000000, 0.8660254037844387076, 1.000000000000000000, 0.8660254037844387076, 1.000000000000000000, 0.8660254037844387076, 1.000000000000000000, 0.8660254037844387076, 1.000000000000000000, 0.8660254037844387076, 1.000000000000000000, 0.8660254037844387076, 1.000000000000000000, 0.8660254037844387076, 1.000000000000000000, 0.8660254037844387076, 1.000000000000000000, 0.8660254037844387076, 1.000000000000000000, 0.8660254037844387076, 1.000000000000000000, 0.8660254037844387076, 1.000000000000000000, 0.8660254037844387076, 1.000000000000000000, 0.8660254037844387076, 1.000000000000000000, 0.8660254037844387076, 1.000000000000000000, 0.8660254037844387076, 1.000000000000000000, 0.8660254037844387076, 1.000000000000000000, 0.8660254037844387076, 1.000000000000000000, 0.8660254037844387076, 1.000000000000000000, 0.8660254037844387076, 1.000000000000000000, 0.8660254037844387076, 1.000000000000000000, 0.8660254037844387076, 1.000000000000000000, 0.8660254037844387076, 1.000000000000000000, 0.8660254037844387076, 1.000000000000000000, 0.8660254037844387076, 1.000000000000000000, 0.8660254037844387076, 1.000000000000000000, 0.8660254037844387076, 1.000000000000000000, 0.8660254037844387076, 1.000000000000000000, 0.8660254037844387076, 1.000000000000000000, 0.8660254037844387076, 1.000000000000000000, 0.8660254037844387076, 1.000000000000000000, 0.8660254037844387076, 1.000000000000000000, 0.8660254037844387076, 1.000000000000000000, 0.8660254037844387076, 1.000000000000000000, 0.8660254037844387076, 1.000000000000000000, 0.8660254037844387076, 1.000000000000000000, 0.8660254037844387076, 1.000000000000000000, 0.8660254037844387076, 1.000000000000000000, 0.8660254037844387076, 1.000000000000000000, 0.8660254037844387076, 1.000000000000000000, 0.8660254037844387076, 1.000000000000000000, 0.8660254037844387076, 1.000000000000000000, 0.8660254037844387076, 1.000000000000000000, 0.8660254037844387076, 1.000000000000000000, 0.8660254037844387076, 1.000000000000000000, 0.8660254037844387076, 1.000000000000000000, 0.8660254037844387076, 1.000000000000000000, 0.8660254037844387076, 1.000000000000000000, 0.8660254037844387076, 1.000000000000000000, 0.8660254037844387076, 1.000000000000000000, 0.8660254037844387076, 1.000000000000000000, 0.8660254037844387076, 1.000000000000000000, 0.8660254037844387076, 1.000000000000000000, 0.8660254037844387076, 1.000000000000000000, 0.8660254037844387076, 1.000000000000000000, 0.8660254037844387076, 1.000000000000000000, 0.8660254037844387076, 1.000000000000000000, 0.8660254037844387076, 1.000000000000000000, 0.8660254037844387076, 1.000000000000000000, 0.8660254037844387076, 1.000000000000000000, 0.8660254037844387076, 1.000000000000000000, 0.8660254037844387076, 1.000000000000000000, 0.8660254037844387076, 1.000000000000000000, 0.8660254037844387076, 1.000000000000000000, 0.8660254037844387076, 1.000000000000000000, 0.8660254037844387076, 1.000000000000000000, 0.8660254037844387076, 1.000000000000000000, 0.8660254037844387076, 1.000000000000000000, 0.8660254037844387076, 1.000000000000000000, 0.8660254037844387076, 1.000000000000000000, 0.8660254037844387076, 1.000000000000000000, 0.8660254037844387076, 1.000000000000000000, 0.8660254037844387076, 1.000000000000000000, 0.8660254037844387076, 1.000000000000000000, 0.8660254037844387076, 1.000000000000000000, 0.8660254037844387076, 1.000000000000000000, 0.8660254037844387076, 1.000000000000000000, 0.8660254037844387076, 1.000000000000000000, 0.8660254037844387076, 1.000000000000000000, 0.8660254037844387076, 1.000000000000000000, 0.8660254037844387076, 1.000000000000000000, 0.8660254037844387076, 1.000000000000000000, 0.8660254037844387076, 1.000000000000000000, 0.8660254037844387076, 1.000000000000000000, 0.8660254037844387076, 1.000000000000000000, 0.8660254037844387076, 1.000000000000000000, 0.8660254037844387076, 1.000000000000000000, 0.8660254037844387076, 1.000000000000000000, 0.8660254037844387076, 1.000000000000000000, 0.8660254037844387076, 1.000000000000000000, 0.8660254037844387076, 1.000000000000000000, 0.8660254037844387076, 1.000000000000000000, 0.8660254037844387076, 1.000000000000000000, 0.8660254037844387076, 1.000000000000000000, 0.8660254037844387076, 1.000000000000000000, 0.8660254037844387076, 1.000000000000000000, 0.8660254037844387076, 1.000000000000000000, 0.8660254037844387076, 1.000000000000000000, 0.8660254037844387076, 1.000000000000000000, 0.8660254037844387076, 1.000000000000000000, 0.8660254037844387076, 1.000000000000000000, 0.8660254037844387076, 1.000000000000000000, 0.8660254037844387076, 1.000000000000000000, 0.8660254037844387076, 1.000000000000000000, 0.8660254037844387076, 1.000000000000000000, 0.8660254037844387076, 1.000000000000000000, 0.8660254037844387076, 1.000000000000000000, 0.8660254037844387076, 1.000000000000000000, 0.8660254037844387076, 1.000000000000000000, 0.8660254037844387076, 1.000000000000000000, 0.8660254037844387076, 1.000000000000000000, 0.8660254037844387076, 1.000000000000000000, 0.8660254037844387076, 1.000000000000000000, 0.8660254037844387076, 1.000000000000000000, 0.8660254037844387076, 1.000000000000000000, 0.8660254037844387076, 1.000000000000000000, 0.8660254037844387076, 1.000000000000000000, 0.8660254037844387076, 1.000000000000000000, 0.8660254037844387076, 1.000000000000000000, 0.8660254037844387076, 1.000000000000000000, 0.8660254037844387076, 1.000000000000000000, 0.8660254037844387076, 1.000000000000000000, 0.8660254037844387076, 1.000000000000000000, 0.8660254037844387076, 1.000000000000000000, 0.8660254037844387076, 1.000000000000000000, 0.8660254037844387076, 1.000000000000000000, 0.8660254037844387076, 1.000000000000000000, 0.8660254037844387076, 1.000000000000000000, 0.8660254037844387076, 1.000000000000000000, 0.8660254037844387076, 1.000000000000000000, 0.8660254037844387076, 1.000000000000000000, 0.8660254037844387076, 1.000000000000000000, 0.8660254037844387076, 1.000000000000000000, 0.8660254037844387076, 1.000000000000000000, 0.8660254037844387076, 1.000000000000000000, 0.8660254037844387076, 1.000000000000000000, 0.8660254037844387076, 1.000000000000000000, 0.8660254037844387076, 1.000000000000000000, 0.8660254037844387076, 1.000000000000000000, 0.8660254037844387076, 1.000000000000000000, 0.8660254037844387076, 1.000000000000000000, 0.8660254037844387076, 1.000000000000000000, 0.8660254037844387076, 1.000000000000000000, 0.8660254037844387076, 1.000000000000000000),
 ( 1.000000000000000000, 0.8660254037844387076, 1.000000000000000000, 0.8660254037844387076, 1.000000000000000000, 0.8660254037844387076, 1.000000000000000000, 0.8660254037844387076, 1.000000000000000000, 0.8660254037844387076, 1.000000000000000000, 0.8660254037844387076, 1.000000000000000000, 0.8660254037844387076, 1.000000000000000000, 0.8660254037844387076, 1.000000000000000000, 0.8660254037844387076, 1.000000000000000000, 0.8660254037844387076, 1.000000000000000000, 0.8660254037844387076, 1.000000000000000000, 0.8660254037844387076, 1.000000000000000000, 0.8660254037844387076, 1.000000000000000000, 0.8660254037844387076, 1.000000000000000000, 0.8660254037844387076, 1.000000000000000000, 0.8660254037844387076, 1.000000000000000000, 0.8660254037844387076, 1.000000000000000000, 0.8660254037844387076, 1.000000000000000000, 0.8660254037844387076, 1.000000000000000000, 0.8660254037844387076, 1.000000000000000000, 0.8660254037844387076, 1.000000000000000000, 0.8660254037844387076, 1.000000000000000000, 0.8660254037844387076, 1.000000000000000000, 0.8660254037844387076, 1.000000000000000000, 0.8660254037844387076, 1.000000000000000000, 0.8660254037844387076, 1.000000000000000000, 0.8660254037844387076, 1.000000000000000000, 0.8660254037844387076, 1.000000000000000000, 0.8660254037844387076, 1.000000000000000000, 0.8660254037844387076, 1.000000000000000000, 0.8660254037844387076, 1.000000000000000000, 0.8660254037844387076, 1.000000000000000000, 0.8660254037844387076, 1.000000000000000000, 0.8660254037844387076, 1.000000000000000000, 0.8660254037844387076, 1.000000000000000000, 0.8660254037844387076, 1.000000000000000000, 0.8660254037844387076, 1.000000000000000000, 0.8660254037844387076, 1.000000000000000000, 0.8660254037844387076, 1.000000000000000000, 0.8660254037844387076, 1.000000000000000000, 0.8660254037844387076, 1.000000000000000000, 0.8660254037844387076, 1.000000000000000000, 0.8660254037844387076, 1.000000000000000000, 0.8660254037844387076, 1.000000000000000000, 0.8660254037844387076, 1.000000000000000000, 0.8660254037844387076, 1.000000000000000000, 0.8660254037844387076, 1.000000000000000000, 0.8660254037844387076, 1.000000000000000000, 0.8660254037844387076, 1.000000000000000000, 0.8660254037844387076, 1.000000000000000000, 0.8660254037844387076, 1.000000000000000000, 0.8660254037844387076, 1.000000000000000000, 0.8660254037844387076, 1.000000000000000000, 0.8660254037844387076, 1.000000000000000000, 0.8660254037844387076, 1.000000000000000000, 0.8660254037844387076, 1.000000000000000000, 0.8660254037844387076, 1.000000000000000000, 0.8660254037844387076, 1.000000000000000000, 0.8660254037844387076, 1.000000000000000000, 0.8660254037844387076, 1.000000000000000000, 0.8660254037844387076, 1.000000000000000000, 0.8660254037844387076, 1.000000000000000000, 0.8660254037844387076, 1.000000000000000000, 0.8660254037844387076, 1.000000000000000000, 0.8660254037844387076, 1.000000000000000000, 0.8660254037844387076, 1.000000000000000000, 0.8660254037844387076, 1.000000000000000000, 0.8660254037844387076, 1.000000000000000000, 0.8660254037844387076, 1.000000000000000000, 0.8660254037844387076, 1.000000000000000000, 0.8660254037844387076, 1.000000000000000000, 0.8660254037844387076, 1.000000000000000000, 0.8660254037844387076, 1.000000000000000000, 0.8660254037844387076, 1.000000000000000000, 0.8660254037844387076, 1.000000000000000000, 0.8660254037844387076, 1.000000000000000000, 0.8660254037844387076, 1.000000000000000000, 0.8660254037844387076, 1.000000000000000000, 0.8660254037844387076, 1.000000000000000000, 0.8660254037844387076, 1.000000000000000000, 0.8660254037844387076, 1.000000000000000000, 0.8660254037844387076, 1.000000000000000000, 0.8660254037844387076, 1.000000000000000000, 0.8660254037844387076, 1.000000000000000000, 0.8660254037844387076, 1.000000000000000000, 0.8660254037844387076, 1.000000000000000000, 0.8660254037844387076, 1.000000000000000000, 0.8660254037844387076, 1.000000000000000000, 0.8660254037844387076, 1.000000000000000000, 0.8660254037844387076, 1.000000000000000000, 0.8660254037844387076, 1.000000000000000000, 0.8660254037844387076, 1.000000000000000000, 0.8660254037844387076, 1.000000000000000000, 0.8660254037844387076, 1.000000000000000000, 0.8660254037844387076, 1.000000000000000000, 0.8660254037844387076, 1.000000000000000000, 0.8660254037844387076, 1.000000000000000000, 0.8660254037844387076, 1.000000000000000000, 0.8660254037844387076, 1.000000000000000000, 0.8660254037844387076, 1.000000000000000000, 0.8660254037844387076, 1.000000000000000000, 0.8660254037844387076, 1.000000000000000000, 0.8660254037844387076, 1.000000000000000000, 0.8660254037844387076, 1.000000000000000000, 0.8660254037844387076, 1.000000000000000000, 0.8660254037844387076, 1.000000000000000000, 0.8660254037844387076, 1.000000000000000000, 0.8660254037844387076, 1.000000000000000000, 0.8660254037844387076, 1.000000000000000000, 0.8660254037844387076, 1.000000000000000000, 0.8660254037844387076, 1.000000000000000000, 0.8660254037844387076, 1.000000000000000000, 0.8660254037844387076, 1.000000000000000000, 0.8660254037844387076, 1.000000000000000000, 0.8660254037844387076, 1.000000000000000000, 0.8660254037844387076, 1.000000000000000000, 0.8660254037844387076, 1.000000000000000000, 0.8660254037844387076, 1.000000000000000000, 0.8660254037844387076, 1.000000000000000000, 0.8660254037844387076, 1.000000000000000000, 0.8660254037844387076, 1.000000000000000000, 0.8660254037844387076, 1.000000000000000000, 0.8660254037844387076, 1.000000000000000000, 0.8660254037844387076, 1.000000000000000000, 0.8660254037844387076, 1.000000000000000000, 0.8660254037844387076, 1.000000000000000000, 0.8660254037844387076, 1.000000000000000000, 0.8660254037844387076, 1.000000000000000000, 0.8660254037844387076, 1.000000000000000000, 0.8660254037844387076, 1.000000000000000000, 0.8660254037844387076, 1.000000000000000000, 0.8660254037844387076, 1.000000000000000000, 0.8660254037844387076, 1.000000000000000000, 0.8660254037844387076, 1.000000000000000000, 0.8660254037844387076, 1.000000000000000000, 0.8660254037844387076, 1.000000000000000000, 0.8660254037844387076, 1.000000000000000000, 0.8660254037844387076, 1.000000000000000000, 0.8660254037844387076, 1.000000000000000000, 0.8660254037844387076, 1.000000000000000000, 0.8660254037844387076, 1.000000000000000000, 0.8660254037844387076, 1.000000000000000000, 0.8660254037844387076, 1.000000000000000000, 0.8660254037844387076, 1.000000000000000000, 0.8660254037844387076, 1.000000000000000000, 0.8660254037844387076, 1.000000000000000000, 0.8660254037844387076, 1.000000000000000000, 0.8660254037844387076, 1.000000000000000000, 0.8660254037844387076, 1.000000000000000000, 0.8660254037844387076, 1.000000000000000000, 0.8660254037844387076, 1.000000000000000000, 0.8660254037844387076, 1.000000000000000000, 0.8660254037844387076, 1.000000000000000000, 0.8660254037844387076, 1.000000000000000000, 0.8660254037844387076, 1.000000000000000000, 0.8660254037844387076, 1.000000000000000000, 0.8660254037844387076, 1.000000000000000000, 0.8660254037844387076, 1.000000000000000000, 0.8660254037844387076, 1.000000000000000000, 0.8660254037844387076, 1.000000000000000000, 0.8660254037844387076, 1.000000000000000000, 0.8660254037844387076, 1.000000000000000000, 0.8660254037844387076, 1.000000000000000000, 0.8660254037844387076, 1.000000000000000000, 0.8660254037844387076, 1.000000000000000000, 0.8660254037844387076, 1.000000000000000000, 0.8660254037844387076, 1.000000000000000000, 0.8660254037844387076, 1.000000000000000000, 0.8660254037844387076, 1.000000000000000000, 0.8660254037844387076, 1.000000000000000000, 0.8660254037844387076, 1.000000000000000000, 0.8660254037844387076, 1.000000000000000000, 0.8660254037844387076, 1.000000000000000000, 0.8660254037844387076, 1.000000000000000000, 0.8660254037844387076, 1.000000000000000000, 0.8660254037844387076, 1.000000000000000000, 0.8660254037844387076, 1.000000000000000000, 0.8660254037844387076, 1.000000000000000000, 0.8660254037844387076, 1.000000000000000000, 0.8660254037844387076, 1.000000000000000000, 0.8660254037844387076, 1.000000000000000000, 0.8660254037844387076, 1.000000000000000000, 0.8660254037844387076, 1.000000000000000000, 0.8660254037844387076, 1.000000000000000000, 0.8660254037844387076, 1.000000000000000000, 0.8660254037844387076, 1.000000000000000000, 0.8660254037844387076, 1.000000000000000000, 0.8660254037844387076, 1.000000000000000000, 0.8660254037844387076, 1.000000000000000000, 0.8660254037844387076, 1.000000000000000000, 0.8660254037844387076, 1.000000000000000000, 0.8660254037844387076, 1.000000000000000000, 0.8660254037844387076, 1.000000000000000000, 0.8660254037844387076, 1.000000000000000000, 0.8660254037844387076, 1.000000000000000000, 0.8660254037844387076, 1.000000000000000000, 0.8660254037844387076, 1.000000000000000000, 0.8660254037844387076, 1.000000000000000000, 0.8660254037844387076, 1.000000000000000000, 0.8660254037844387076, 1.000000000000000000, 0.8660254037844387076, 1.000000000000000000, 0.8660254037844387076, 1.000000000000000000, 0.8660254037844387076, 1.000000000000000000, 0.8660254037844387076, 1.000000000000000000, 0.8660254037844387076, 1.000000000000000000, 0.8660254037844387076, 1.000000000000000000, 0.8660254037844387076, 1.000000000000000000, 0.8660254037844387076, 1.000000000000000000, 0.8660254037844387076, 1.000000000000000000, 0.8660254037844387076, 1.000000000000000000, 0.8660254037844387076, 1.000000000000000000, 0.8660254037844387076, 1.000000000000000000, 0.8660254037844387076, 1.000000000000000000, 0.8660254037844387076, 1.000000000000000000, 0.8660254037844387076, 1.000000000000000000, 0.8660254037844387076, 1.000000000000000000, 0.8660254037844387076, 1.000000000000000000, 0.8660254037844387076, 1.000000000000000000, 0.8660254037844387076, 1.000000000000000000, 0.8660254037844387076, 1.000000000000000000, 0.8660254037844387076, 1.000000000000000000, 0.8660254037844387076, 1.000000000000000000, 0.8660254037844387076, 1.000000000000000000, 0.8660254037844387076, 1.000000000000000000, 0.8660254037844387076, 1.000000000000000000, 0.8660254037844387076, 1.000000000000000000, 0.8660254037844387076, 1.000000000000000000, 0.8660254037844387076, 1.000000000000000000, 0.8660254037844387076, 1.000000000000000000, 0.8660254037844387076, 1.000000000000000000, 0.8660254037844387076, 1.000000000000000000, 0.8660254037844387076, 1.000000000000000000, 0.8660254037844387076, 1.000000000000000000, 0.8660254037844387076, 1.000000000000000000, 0.8660254037844387076, 1.000000000000000000, 0.8660254037844387076, 1.000000000000000000, 0.8660254037844387076, 1.000000000000000000, 0.8660254037844387076, 1.000000000000000000, 0.8660254037844387076, 1.000000000000000000, 0.8660254037844387076, 1.000000000000000000) ) ) 
 REPRESENTATION_ITEM ( '' )  SURFACE ( )  );
#195077 = ORIENTED_EDGE ( 'NONE', *, *, #156896, .T. ) ;
#195076 = AXIS2_PLACEMENT_3D ( 'NONE', #44195, #142785, #110315 ) ;
#195078 = CARTESIAN_POINT ( 'NONE',  ( 3.498943719384327355, -2.264459259401516267, 0.3945650996091658591 ) ) ;
#195080 = ORIENTED_EDGE ( 'NONE', *, *, #136902, .T. ) ;
#195079 = CARTESIAN_POINT ( 'NONE',  ( 8.107412671292047790, 8.560995659369956101, 0.7216878364870458196 ) ) ;
#195082 = CARTESIAN_POINT ( 'NONE',  ( 1.642778471875000035, -0.9260416661887073131, -2.845375778867859751 ) ) ;
#195081 = CARTESIAN_POINT ( 'NONE',  ( 5.072158865288222351, 8.931619419562697004, 0.7216878364870317197 ) ) ;
#195083 = DIRECTION ( 'NONE',  ( -0.000000000000000000, 1.000000000000000000, -0.000000000000000000 ) ) ;
#195084 = FACE_OUTER_BOUND ( 'NONE', #154407, .T. ) ;
#195085 = B_SPLINE_CURVE_WITH_KNOTS ( 'NONE', 3,
 ( #9936, #110713, #124843, #45666, #26183, #176713 ),
 .UNSPECIFIED., .F., .F.,
 ( 4, 2, 4 ),
 ( 0.000000000000000000, 0.0003767011250903909100, 0.0007534022501807818200 ),
 .UNSPECIFIED. ) ;
#195086 = CARTESIAN_POINT ( 'NONE',  ( 3.433474178283620670, 0.8725410082476585671, -1.734956227438133158 ) ) ;
#195087 = VERTEX_POINT ( 'NONE', #53604 ) ;
#195089 = ADVANCED_FACE ( 'NONE', ( #87167 ), #94088, .F. ) ;
#195088 = CARTESIAN_POINT ( 'NONE',  ( -6.742488139262638275E-15, -9.746166700180788567, 9.500331257164617682 ) ) ;
#195090 = CARTESIAN_POINT ( 'NONE',  ( 4.834190613173367623, -1.027981871586785889, -1.612434056610718480 ) ) ;
#195091 = LINE ( 'NONE', #30467, #96571 ) ;
#195092 = CARTESIAN_POINT ( 'NONE',  ( -0.01747323780270595983, -0.1290080397739183926, -1.696210917522892325 ) ) ;
#195093 = CARTESIAN_POINT ( 'NONE',  ( 4.083220446344194343, 1.622485107653489633, 1.197306254465977826 ) ) ;
#195094 = CARTESIAN_POINT ( 'NONE',  ( 5.239047776066017903, 2.296150469294107488, -0.1107920306624484569 ) ) ;
#195095 = CARTESIAN_POINT ( 'NONE',  ( -1.598423149420378220, 8.713846000021357341, 2.499999999999998668 ) ) ;
#195096 = CARTESIAN_POINT ( 'NONE',  ( 0.7509353727821498348, 0.6442623716619542140, 2.110749664216593047 ) ) ;
#195098 = CARTESIAN_POINT ( 'NONE',  ( -5.817857314039913241, 5.960124085900898372, 0.000000000000000000 ) ) ;
#195097 = CARTESIAN_POINT ( 'NONE',  ( -3.838774385731502203, 7.492511168737228111, -0.01748052351197342674 ) ) ;
#195100 = CARTESIAN_POINT ( 'NONE',  ( 0.2679308956112765872, -1.161373500300251216, 1.335597826242039154 ) ) ;
#195099 = CARTESIAN_POINT ( 'NONE',  ( 0.02354010051478470922, -1.288079656314411459, -1.647238045112088267 ) ) ;
#195101 = CARTESIAN_POINT ( 'NONE',  ( 5.256482491209823138, 1.942542154241846397, -0.5404887192124520068 ) ) ;
#195103 = CARTESIAN_POINT ( 'NONE',  ( 3.170184779232795957, -1.365206436085873776, 1.841245074435297502 ) ) ;
#195102 = CARTESIAN_POINT ( 'NONE',  ( 4.213551878797002992, 8.137837301896977849, 0.000000000000000000 ) ) ;
#195104 = CARTESIAN_POINT ( 'NONE',  ( 1.218268023815568535, -0.04584277261814385940, 1.739893813429808311 ) ) ;
#195105 = CARTESIAN_POINT ( 'NONE',  ( -2.617062827300063343, -0.3852370113777853766, -0.1797355214283803959 ) ) ;
#195106 = CARTESIAN_POINT ( 'NONE',  ( 1.387607149621207236, -0.04906231267952190778, 1.733339852973712292 ) ) ;
#195107 = CARTESIAN_POINT ( 'NONE',  ( -4.957638175832625493E-14, 0.8593750003414141192, -1.570758158831808249 ) ) ;
#195108 = CARTESIAN_POINT ( 'NONE',  ( -11.97297122925952095, 13.79874920673088567, -0.8121202983519171248 ) ) ;
#195109 = CARTESIAN_POINT ( 'NONE',  ( 1.328853926488116510, -1.377647258212051362, 1.678094904287985800 ) ) ;
#195110 = CARTESIAN_POINT ( 'NONE',  ( 2.026577684455236561, 0.4465047249504557891, 1.966304233017155845 ) ) ;
#195111 = CARTESIAN_POINT ( 'NONE',  ( 5.468750000000003553, 0.7852924748297082091, -1.895863743164194704 ) ) ;
#195112 = CARTESIAN_POINT ( 'NONE',  ( 1.499999999999989120, 1.785416667349487563, 0.8660254037844524744 ) ) ;
#195113 = CARTESIAN_POINT ( 'NONE',  ( 0.3055242992691169501, -0.5169788762636564616, 1.855657374570508278 ) ) ;
#195114 = CARTESIAN_POINT ( 'NONE',  ( 1.364683531249997417, 12.73437500034139980, 2.602085213965210642E-15 ) ) ;
#195115 = CARTESIAN_POINT ( 'NONE',  ( 3.480930870787651621, -1.489476591903232228, 1.648259452209248854 ) ) ;
#195116 = ORIENTED_EDGE ( 'NONE', *, *, #161695, .F. ) ;
#195117 = CARTESIAN_POINT ( 'NONE',  ( 0.000000000000000000, 1.000000000000000888, 0.000000000000000000 ) ) ;
#195119 = EDGE_CURVE ( 'NONE', #103981, #167139, #64421, .T. ) ;
#195118 = CARTESIAN_POINT ( 'NONE',  ( 8.483651433849084711, 10.92067931095586886, 1.599625672291281386 ) ) ;
#195120 = CARTESIAN_POINT ( 'NONE',  ( 7.797347741190739256, 8.269529584243604958, 0.7216878364870267237 ) ) ;
#195121 = CARTESIAN_POINT ( 'NONE',  ( 0.6823417656249864960, -1.073958332991911568, -1.181850606188749264 ) ) ;
#195122 = CARTESIAN_POINT ( 'NONE',  ( 5.829613671240826633, 0.8500414093583901209, -1.518663286469445151 ) ) ;
#195123 = CARTESIAN_POINT ( 'NONE',  ( 3.578520225191741844, 1.246510459297203610, -1.514941731618473009 ) ) ;
#195125 = CARTESIAN_POINT ( 'NONE',  ( -6.887178846062128379, 7.137389529935019183, -0.7216878364870278340 ) ) ;
#195124 = CARTESIAN_POINT ( 'NONE',  ( 2.361091307074211887, 5.906356958228550447, 0.7998128361456462443 ) ) ;
#195126 = CARTESIAN_POINT ( 'NONE',  ( 11.86239285000045740, 13.87999999999998302, 1.812080536912751061 ) ) ;
#195127 = CARTESIAN_POINT ( 'NONE',  ( 4.850980959722003938, -1.821092479232713446, 1.342276170020906711 ) ) ;
#195128 = CARTESIAN_POINT ( 'NONE',  ( 1.627463713854758298, 0.1539993984382737602, -2.057001629134532550 ) ) ;
#195129 = CARTESIAN_POINT ( 'NONE',  ( -5.208303565944065738, 9.228104593576741621, -0.7998128361456231517 ) ) ;
#195130 = CONICAL_SURFACE ( 'NONE', #126097, 11.53746066217573940, 0.1181278931043537039 ) ;
#195131 = CARTESIAN_POINT ( 'NONE',  ( 2.360583983009652442, 0.9673915393220763326, 2.045390427905840358 ) ) ;
#195132 = ORIENTED_EDGE ( 'NONE', *, *, #31157, .T. ) ;
#195134 = ADVANCED_FACE ( 'NONE', ( #5886 ), #173791, .T. ) ;
#195133 = CARTESIAN_POINT ( 'NONE',  ( -1.402160292154681736E-14, 1.118750000682820378, -1.732050807568863648 ) ) ;
#195135 = CARTESIAN_POINT ( 'NONE',  ( 3.198369223161025676, -0.5396142385952484855, -1.791042426047453784 ) ) ;
#195136 = CARTESIAN_POINT ( 'NONE',  ( 2.039351246016813501, -1.339629256360101106, 1.101148611782216014 ) ) ;
#195137 = CARTESIAN_POINT ( 'NONE',  ( 6.233935805145816467, 2.167428969419796125, 0.3234103439683775894 ) ) ;
#195138 = CARTESIAN_POINT ( 'NONE',  ( 6.721674876502457430, -2.240710703332372766, 0.5512419492274822641 ) ) ;
#195139 = CARTESIAN_POINT ( 'NONE',  ( 3.942369626403975147, 2.151062187213080623, 0.2142938780915065733 ) ) ;
#195140 = CARTESIAN_POINT ( 'NONE',  ( 4.699130951095971120, -0.5162677480817599029, 1.872006234571305772 ) ) ;
#195141 = CARTESIAN_POINT ( 'NONE',  ( -4.595850884908229794, 4.464173575255435011, 0.7216878364870317197 ) ) ;
#195142 = EDGE_CURVE ( 'NONE', #213643, #154544, #76259, .T. ) ;
#195144 = UNCERTAINTY_MEASURE_WITH_UNIT (LENGTH_MEASURE( 1.000000000000000082E-05 ), #111671, 'distance_accuracy_value', 'NONE');
#195143 = CARTESIAN_POINT ( 'NONE',  ( 6.802024559211160337, -1.870114703409443857, 0.04643648283486621897 ) ) ;
#195145 =( NAMED_UNIT ( * ) PLANE_ANGLE_UNIT ( ) SI_UNIT ( $, .RADIAN. ) );
#195146 = CARTESIAN_POINT ( 'NONE',  ( 4.815628398899983509, 6.730757278346135131, 1.248813279183153657 ) ) ;
#195147 = CARTESIAN_POINT ( 'NONE',  ( 4.114536431845257525, 3.902640046681976393, 1.214306433183764966E-14 ) ) ;
#195148 = CARTESIAN_POINT ( 'NONE',  ( 4.475600106286968582, 5.354526557823810151, -1.082531754730548412 ) ) ;
#195149 = CARTESIAN_POINT ( 'NONE',  ( -3.505400730386704341E-15, 2.703125000341406903, 1.570758158831794260 ) ) ;
#195150 = CARTESIAN_POINT ( 'NONE',  ( 5.748672702226536479, 1.986101125435947301, -0.3474646712962395911 ) ) ;
#195151 = CARTESIAN_POINT ( 'NONE',  ( -8.455481356417053007, 13.01647868246193518, 0.7998128361456341429 ) ) ;
#195152 = CARTESIAN_POINT ( 'NONE',  ( 8.457588896826466751, 8.761608555919362828, 1.040834085586084257E-14 ) ) ;
#195153 = LINE ( 'NONE', #191922, #8001 ) ;
#195155 = CARTESIAN_POINT ( 'NONE',  ( -1.326716514427061987E-15, 2.999999999999988454, -1.225000000000003864 ) ) ;
#195154 = CARTESIAN_POINT ( 'NONE',  ( 3.773894676421325478, 1.015518775504126614, 1.516979517045339509 ) ) ;
#195156 = CARTESIAN_POINT ( 'NONE',  ( 7.037870247915942734, -8.233137084989836652, -6.381095703207974701 ) ) ;
#195157 = ORIENTED_EDGE ( 'NONE', *, *, #164982, .T. ) ;
#195158 = CARTESIAN_POINT ( 'NONE',  ( -5.112833325684916552, 7.058334528089422300, -1.443375672974066548 ) ) ;
#195159 = CARTESIAN_POINT ( 'NONE',  ( -6.471393748265563239, 5.229711127717889596, 2.499999999999998668 ) ) ;
#195160 = CARTESIAN_POINT ( 'NONE',  ( -7.049349804101573191, 10.31165964050546258, -1.199719254218440723 ) ) ;
#195161 = CARTESIAN_POINT ( 'NONE',  ( 6.551426717330563143, -1.803173079755305608, 0.9099084737219197416 ) ) ;
#195162 = CARTESIAN_POINT ( 'NONE',  ( 1.471502243059899850, -1.820439715282649251, -1.087164402369590555 ) ) ;
#195163 = VERTEX_POINT ( 'NONE', #156456 ) ;
#195164 = CARTESIAN_POINT ( 'NONE',  ( -5.611095471209320174, 7.639640364534566075, 1.599625672291263179 ) ) ;
#195165 = CARTESIAN_POINT ( 'NONE',  ( 1.656853885927531689, 1.525116498273047405, -1.066097284832379755 ) ) ;
#195166 = CARTESIAN_POINT ( 'NONE',  ( 2.855963913973019963, 6.483708332943829866, 0.000000000000000000 ) ) ;
#195167 = CARTESIAN_POINT ( 'NONE',  ( 6.086805585656668960, -0.2997611930264115765, -2.038837977671539736 ) ) ;
#195168 = CARTESIAN_POINT ( 'NONE',  ( 6.469375277500488686, -1.978045142091336306, -0.3906011616893814709 ) ) ;
#195169 = ORIENTED_EDGE ( 'NONE', *, *, #74578, .F. ) ;
#195170 = VERTEX_POINT ( 'NONE', #75199 ) ;
#195171 = CARTESIAN_POINT ( 'NONE',  ( -10.29471871147821282, 10.90492667301307605, -0.7998128361456291469 ) ) ;
#195172 = CARTESIAN_POINT ( 'NONE',  ( 3.949673224339702138, 0.6133576713117370183, -1.719707012317383432 ) ) ;
#195175 = ORIENTED_EDGE ( 'NONE', *, *, #204228, .F. ) ;
#195174 = CARTESIAN_POINT ( 'NONE',  ( -4.868901516392104334, 6.903810023003053686, -1.445308410833840318 ) ) ;
#195173 = CARTESIAN_POINT ( 'NONE',  ( -4.359828915246279024, 7.244161613499399799, -1.199719254218455378 ) ) ;
#195176 = CARTESIAN_POINT ( 'NONE',  ( 6.104935607482663507, 7.108274908414393245, 1.121150977946131722 ) ) ;
#195177 = CARTESIAN_POINT ( 'NONE',  ( 6.573592277014387086, 1.495820547097842068, -1.351949839681469090 ) ) ;
#195178 = CARTESIAN_POINT ( 'NONE',  ( 5.279192629422701621, 1.239228542960477242, 1.361826556748657602 ) ) ;
#195179 = CARTESIAN_POINT ( 'NONE',  ( 2.982514307567902812, 6.468353249220382573, 0.4073410874377252910 ) ) ;
#195180 = CARTESIAN_POINT ( 'NONE',  ( 3.194261032343487461, -0.9352514745577229505, 2.109854200106716426 ) ) ;
#195181 = CARTESIAN_POINT ( 'NONE',  ( 4.857564175446106525, 8.889184981320973122, 0.7998128361456331437 ) ) ;
#195182 = CARTESIAN_POINT ( 'NONE',  ( 5.483715611629243369, 1.447241891022777560, 1.605803905980404123 ) ) ;
#195183 = CARTESIAN_POINT ( 'NONE',  ( 7.096803341749390981, 10.36702210109460154, -1.199719254218441611 ) ) ;
#195184 = CARTESIAN_POINT ( 'NONE',  ( 0.9955321287432462585, -1.942234967994656669, 0.001507142460104027087 ) ) ;
#195185 = CARTESIAN_POINT ( 'NONE',  ( -3.867100128395853709, 5.534702787927018974, -1.599625672291256295 ) ) ;
#195186 = ORIENTED_EDGE ( 'NONE', *, *, #7050, .T. ) ;
#195187 = CARTESIAN_POINT ( 'NONE',  ( -2.428612866367529932E-14, 8.999999999999998224, 0.7749999999999996891 ) ) ;
#195188 = CARTESIAN_POINT ( 'NONE',  ( -4.248501033035892327, 6.049946853332221153, -1.599625672291271394 ) ) ;
#195189 = CARTESIAN_POINT ( 'NONE',  ( 4.944154083221365070, 1.865701114312174225, 0.1370711555178441010 ) ) ;
#195192 = CARTESIAN_POINT ( 'NONE',  ( -3.962726036944197894, 7.845207153068690431, -0.7998128361456481317 ) ) ;
#195191 = CARTESIAN_POINT ( 'NONE',  ( 1.499999999999985123, -0.1729166659838496101, -0.8660254037844323793 ) ) ;
#195190 = CARTESIAN_POINT ( 'NONE',  ( 0.8789968191965717992, -1.730013457311157188, -0.8152767527440167861 ) ) ;
#195193 = CARTESIAN_POINT ( 'NONE',  ( 4.143358556170802842, -1.920740624720223666, 1.086653567583625746 ) ) ;
#195194 = CARTESIAN_POINT ( 'NONE',  ( 2.191614386903386613, 5.708633884695917260, -0.7998128361456281477 ) ) ;
#195195 = CARTESIAN_POINT ( 'NONE',  ( 5.628043163004202931, 8.619781885929965526, -1.082531754730548412 ) ) ;
#195196 = CARTESIAN_POINT ( 'NONE',  ( -4.471491734408701291, 4.111161866431900513, 1.214306433183764966E-14 ) ) ;
#195197 = CARTESIAN_POINT ( 'NONE',  ( -6.089020385868867180, 7.236850217336030511, -1.082531754730549967 ) ) ;
#195198 = CARTESIAN_POINT ( 'NONE',  ( 2.231653169902757750, -1.284661796483690832, -1.495404430405805174 ) ) ;
#195199 = CARTESIAN_POINT ( 'NONE',  ( 1.343279689680024536, 0.4525242940816387449, 2.262625540901804122 ) ) ;
#195200 = CARTESIAN_POINT ( 'NONE',  ( 2.260140581184489239, -1.961506502764579052, 0.04509734162668613960 ) ) ;
#195201 = CARTESIAN_POINT ( 'NONE',  ( 4.979373296276208727, -0.1066085398311214100, 2.059958923327874114 ) ) ;
#195202 = CARTESIAN_POINT ( 'NONE',  ( 3.551873057100274789, 7.087676300018221021, 0.7216878364870298324 ) ) ;
#195203 = CARTESIAN_POINT ( 'NONE',  ( 3.881377115262159894, 7.750300077773022878, 0.7998128361456271485 ) ) ;
#195204 = EDGE_LOOP ( 'NONE', ( #113834, #210241, #100497, #102032, #127974, #115428, #119402, #57551, #52711, #158537, #3239, #192337, #142177, #126891, #190210, #188599, #92816, #167570, #151140, #103070, #108634, #204039, #80602, #168904, #90097 ) ) ;
#195205 = CARTESIAN_POINT ( 'NONE',  ( -9.378489572351046633, 11.96465713920816043, -1.599625672291263179 ) ) ;
#195206 = CARTESIAN_POINT ( 'NONE',  ( -1.559647396048210677, 1.374772708486763806, 1.500000000000001332 ) ) ;
#195207 = CARTESIAN_POINT ( 'NONE',  ( 10.40996301719436090, 11.03937836301526687, 0.000000000000000000 ) ) ;
#195208 = CARTESIAN_POINT ( 'NONE',  ( 1.305810364819631753, -1.710103357748852027, -1.337415221091219353 ) ) ;
#195210 = CARTESIAN_POINT ( 'NONE',  ( 5.817764947765640571, 7.282435344852455472, -1.374816383645981688 ) ) ;
#195209 = CARTESIAN_POINT ( 'NONE',  ( -1.937985808864938540E-15, -9.954378579146972328, -10.91970693179590768 ) ) ;
#195211 = ADVANCED_FACE ( 'NONE', ( #8042 ), #190001, .T. ) ;
#195212 = CARTESIAN_POINT ( 'NONE',  ( 11.48243876534946217, 11.29999999999999893, -3.200000000000001510 ) ) ;
#195213 = CARTESIAN_POINT ( 'NONE',  ( -7.137427359597535492, -7.616807914308467709, 7.137427359599341159 ) ) ;
#195214 = CARTESIAN_POINT ( 'NONE',  ( 2.565516880305099612, 1.835255434019352094, -0.3607447438512822457 ) ) ;
#195215 = CARTESIAN_POINT ( 'NONE',  ( 6.872347393157318685, -1.336039616365672700, 1.699942530728588919 ) ) ;
#195217 = CARTESIAN_POINT ( 'NONE',  ( 6.827182134110196365, 2.083530588508203607, 2.119847806254702594 ) ) ;
#195216 = CARTESIAN_POINT ( 'NONE',  ( 0.07735805125224680390, 0.7159309182679198802, -2.172969595131315934 ) ) ;
#195218 = CARTESIAN_POINT ( 'NONE',  ( -1.402160292154681736E-14, -0.1781249996585796136, 1.575800808251672791 ) ) ;
#195219 = CARTESIAN_POINT ( 'NONE',  ( 2.016128127738999076, -1.911839501640894001, 0.04842977492004740814 ) ) ;
#195220 = CARTESIAN_POINT ( 'NONE',  ( 4.276060399186999206, -1.018433877553532207, 1.447237009025013732 ) ) ;
#195221 = CARTESIAN_POINT ( 'NONE',  ( 1.682132150489405564, 0.9841149911452107268, 1.639481845682550398 ) ) ;
#195222 = CARTESIAN_POINT ( 'NONE',  ( -4.229253852459088137, 7.021547696922494808, 1.199719254218464037 ) ) ;
#195224 = CARTESIAN_POINT ( 'NONE',  ( 5.624599552000627334, 0.3785363404739845450, 1.877648607602548925 ) ) ;
#195223 = CARTESIAN_POINT ( 'NONE',  ( 7.317172100869718143, -6.705807707649934279, -7.317172100869746565 ) ) ;
#195225 = CARTESIAN_POINT ( 'NONE',  ( 0.1509401653462701109, -0.4529219869476922011, -2.027634260368789576 ) ) ;
#195226 = CARTESIAN_POINT ( 'NONE',  ( 1.499999999999990896, 4.525000000000021672, 1.214306433183764966E-14 ) ) ;
#195227 = CARTESIAN_POINT ( 'NONE',  ( 2.074623746436579985, 0.9110886696130392481, 1.915067268644244702 ) ) ;
#195228 = CARTESIAN_POINT ( 'NONE',  ( 4.680451076648031616, -1.814532364864028136, -0.4542276060127621862 ) ) ;
#195230 = EDGE_LOOP ( 'NONE', ( #197644, #136810, #63462, #70761 ) ) ;
#195229 = CARTESIAN_POINT ( 'NONE',  ( 1.787459277025660542, 1.258035843444211155, 1.323286951131589895 ) ) ;
#195232 = CARTESIAN_POINT ( 'NONE',  ( 4.739057715201537846, 8.198473722472776615, 0.7146191656044629248 ) ) ;
#195231 = CARTESIAN_POINT ( 'NONE',  ( 4.600333186373093852, -2.206333364838486411, -0.05604163552313382035 ) ) ;
#195233 = CARTESIAN_POINT ( 'NONE',  ( -1.364683531250000748, -0.9906249996585805295, 0.000000000000000000 ) ) ;
#195234 = CARTESIAN_POINT ( 'NONE',  ( 2.031754214314248408, 1.974575511506712289, -0.5964607296059397656 ) ) ;
#195235 = CARTESIAN_POINT ( 'NONE',  ( 5.262536180398716290, 9.291375977107183104, -0.7998128361456291469 ) ) ;
#195237 = CARTESIAN_POINT ( 'NONE',  ( -9.189729191964438826, 9.615772233580322848, 1.040834085586084257E-14 ) ) ;
#195236 = AXIS2_PLACEMENT_3D ( 'NONE', #56535, #21855, #202750 ) ;
#195238 = DIRECTION ( 'NONE',  ( 0.000000000000000000, -1.000000000000000000, 0.000000000000000000 ) ) ;
#195239 = DIRECTION ( 'NONE',  ( 0.000000000000000000, 0.000000000000000000, 1.000000000000000000 ) ) ;
#195240 = FILL_AREA_STYLE ('',( #194161 ) ) ;
#195241 = CARTESIAN_POINT ( 'NONE',  ( 5.996449078994045223, 10.21788403546024782, 0.7998128361456331437 ) ) ;
#195242 = VERTEX_POINT ( 'NONE', #71959 ) ;
#195243 = CARTESIAN_POINT ( 'NONE',  ( 4.211429588753928144, -1.719575573843846072, -1.152724658989822348 ) ) ;
#195245 = CARTESIAN_POINT ( 'NONE',  ( -1.364683531250014514, -0.9489583329919112353, -0.7879004041258359514 ) ) ;
#195244 = CIRCLE ( 'NONE', #25760, 0.04999999999999991257 ) ;
#195246 = CARTESIAN_POINT ( 'NONE',  ( 2.601032539102793084, 1.737798908178284307, -1.285340053188685383 ) ) ;
#195247 = CARTESIAN_POINT ( 'NONE',  ( -5.005744162364479166, 7.928486884654230238, -1.069363714833789558 ) ) ;
#195248 = CARTESIAN_POINT ( 'NONE',  ( 1.488931934708405569, -1.918476728873222070, -0.6315473366199951810 ) ) ;
#195249 = CARTESIAN_POINT ( 'NONE',  ( -3.284816854459712054, -0.1112512837626866702, -0.08051823526699090905 ) ) ;
#195250 = ORIENTED_EDGE ( 'NONE', *, *, #78041, .T. ) ;
#195251 = EDGE_CURVE ( 'NONE', #47534, #29614, #107765, .T. ) ;
#195253 = CARTESIAN_POINT ( 'NONE',  ( 8.459924665247367415, 8.972259652317825740, -0.7216878364870267237 ) ) ;
#195252 = CARTESIAN_POINT ( 'NONE',  ( -3.475000000000000533, -2.129166666666665542, -2.006292185433948827 ) ) ;
#195254 = CARTESIAN_POINT ( 'NONE',  ( -3.458738584817664385, 7.049295759013638474, 0.7216878364870338292 ) ) ;
#195255 = CARTESIAN_POINT ( 'NONE',  ( 0.02267320670834571672, 0.3494893071277604402, 1.985867805234131644 ) ) ;
#195256 = CARTESIAN_POINT ( 'NONE',  ( 5.495707582769355781, -2.191739722525353429, -0.0009102486706394352645 ) ) ;
#195257 = CIRCLE ( 'NONE', #32746, 11.09999999999999964 ) ;
#195258 = CARTESIAN_POINT ( 'NONE',  ( 0.7499999999999902300, 4.097916667349481123, -1.299038105676658228 ) ) ;
#195259 = CARTESIAN_POINT ( 'NONE',  ( 4.254103502353132171, 0.8128351696983120434, -1.731171583500931366 ) ) ;
#195260 = B_SPLINE_CURVE_WITH_KNOTS ( 'NONE', 3,
 ( #142079, #192906, #40285, #211292, #98629, #61860, #114933, #18 ),
 .UNSPECIFIED., .F., .F.,
 ( 4, 2, 2, 4 ),
 ( 3.127317220692751914E-18, 0.003102675431456557598, 0.004654013147184835747, 0.006205350862913112595 ),
 .UNSPECIFIED. ) ;
#195261 = CARTESIAN_POINT ( 'NONE',  ( -2.578021764892882040, 6.159442492350315490, 0.7998128361456341429 ) ) ;
#195262 = CARTESIAN_POINT ( 'NONE',  ( 6.982085920913413624, 8.208483664896217391, -1.082531754730543971 ) ) ;
#195264 = CARTESIAN_POINT ( 'NONE',  ( 2.478138860811992306, -2.011206848916185397, -0.1455134472309257965 ) ) ;
#195263 = CARTESIAN_POINT ( 'NONE',  ( -9.775065565328603157, 11.46695991671396087, -1.082531754730537976 ) ) ;
#195265 = CARTESIAN_POINT ( 'NONE',  ( -1.364683531250014514, 12.15104166700806765, -0.7879004041258335089 ) ) ;
#195266 = CARTESIAN_POINT ( 'NONE',  ( -3.871735385154307263, 6.674719161725423788, -1.199719254218450271 ) ) ;
#195267 = CARTESIAN_POINT ( 'NONE',  ( 5.737229663476812291, -1.557457729854847983, 0.7413209835094927147 ) ) ;
#195268 = CARTESIAN_POINT ( 'NONE',  ( 0.000000000000000000, 19.00000000000000000, 0.000000000000000000 ) ) ;
#195269 = CARTESIAN_POINT ( 'NONE',  ( 3.277320446201373638, 4.846626492033466072, 1.599625672291267398 ) ) ;
#195270 = CARTESIAN_POINT ( 'NONE',  ( 1.383850883036507884E-15, 0.2000000000000057288, -11.29999999999998828 ) ) ;
#195271 = DIRECTION ( 'NONE',  ( 0.000000000000000000, 1.000000000000000000, 0.000000000000000000 ) ) ;
#195272 = EDGE_LOOP ( 'NONE', ( #204565, #75127, #69775, #77677 ) ) ;
#195273 = CARTESIAN_POINT ( 'NONE',  ( 1.182579820358391931, 1.236233925375467058, -1.660450453320160058 ) ) ;
#195274 = VERTEX_POINT ( 'NONE', #187859 ) ;
#195275 = CARTESIAN_POINT ( 'NONE',  ( 4.564998375345614257, -1.451947166338814377, 1.082946968254307585 ) ) ;
#195276 = CIRCLE ( 'NONE', #185363, 11.09999999999999964 ) ;
#195277 = CARTESIAN_POINT ( 'NONE',  ( 5.041653019435334393, 6.975290837464928728, -1.599625672291269396 ) ) ;
#195278 = CARTESIAN_POINT ( 'NONE',  ( -2.193105066167346795, 5.702484939155337607, 2.500000000000011102 ) ) ;
#195279 = ADVANCED_FACE ( 'NONE', ( #109903 ), #23212, .T. ) ;
#195280 = CARTESIAN_POINT ( 'NONE',  ( 5.953728957075980155, -1.316865622510310141, -1.244172183657651365 ) ) ;
#195281 = CARTESIAN_POINT ( 'NONE',  ( 4.028181036591620412, 7.713645286083276709, -0.7216878364870338292 ) ) ;
#195282 = CARTESIAN_POINT ( 'NONE',  ( 0.9486429539237075659, 3.230410930033764227, -1.028101543438967758 ) ) ;
#195283 = CARTESIAN_POINT ( 'NONE',  ( 3.240350661220792183, 0.5327334615983710941, 2.125583950146384904 ) ) ;
#195284 = ORIENTED_EDGE ( 'NONE', *, *, #151772, .F. ) ;
#195285 = EDGE_CURVE ( 'NONE', #198869, #145411, #39486, .T. ) ;
#195287 = CARTESIAN_POINT ( 'NONE',  ( 7.377608144130607393, 11.75895993479440982, -0.7998128361456291469 ) ) ;
#195286 = CARTESIAN_POINT ( 'NONE',  ( 6.883263157960402445, 0.001763689368145578400, 1.846037217754380011 ) ) ;
#195288 = CARTESIAN_POINT ( 'NONE',  ( 5.343340938886254499, 0.3690371538600076273, -1.879538113519742204 ) ) ;
#195289 = FACE_BOUND ( 'NONE', #125936, .T. ) ;
#195290 =( GEOMETRIC_REPRESENTATION_CONTEXT ( 3 ) GLOBAL_UNCERTAINTY_ASSIGNED_CONTEXT ( ( #212129 ) ) GLOBAL_UNIT_ASSIGNED_CONTEXT ( ( #52892, #134180, #116889 ) ) REPRESENTATION_CONTEXT ( 'NONE', 'WORKASPACE' ) );
#195291 = CARTESIAN_POINT ( 'NONE',  ( -1.402160292154681736E-14, -0.6781249996585819728, 1.575800808251672791 ) ) ;
#195292 = CARTESIAN_POINT ( 'NONE',  ( 6.317736394288147039, 6.473040002865377396, 0.7216878364870317197 ) ) ;
#195293 = B_SPLINE_CURVE_WITH_KNOTS ( 'NONE', 3,
 ( #158281, #106370, #9871, #90084, #156147, #142049 ),
 .UNSPECIFIED., .F., .F.,
 ( 4, 2, 4 ),
 ( 0.000000000000000000, 0.0006264319474642703360, 0.001252863894928540672 ),
 .UNSPECIFIED. ) ;
#195294 = CARTESIAN_POINT ( 'NONE',  ( -7.998947442382709383, 12.27592974951444660, 0.7216878364870478180 ) ) ;
#195295 = CARTESIAN_POINT ( 'NONE',  ( 1.780366757100563913, -1.156431984057613827, 1.826190802295484472 ) ) ;
#195296 = CARTESIAN_POINT ( 'NONE',  ( -5.795184315198522285, 5.725746220678519904, -0.7998128361456362523 ) ) ;
#195297 = AXIS2_PLACEMENT_3D ( 'NONE', #138266, #24477, #110092 ) ;
#195298 = CARTESIAN_POINT ( 'NONE',  ( 4.041212305325117882, 6.872442235258051646, -1.199719254218448494 ) ) ;
#195299 = CARTESIAN_POINT ( 'NONE',  ( 1.447985623159939284, 1.823312892812560593, 0.09356915273009414058 ) ) ;
#195300 = CARTESIAN_POINT ( 'NONE',  ( -2.740719608256871442, 6.349256642941639051, 0.7998128361456341429 ) ) ;
#195301 = CARTESIAN_POINT ( 'NONE',  ( 5.192344348049102720, -1.811977082810274808, -0.2219828972063255801 ) ) ;
#195302 = CARTESIAN_POINT ( 'NONE',  ( 8.639639562656480365, 12.08920847220495887, 8.327081629787771888 ) ) ;
#195303 = ORIENTED_EDGE ( 'NONE', *, *, #15281, .T. ) ;
#195304 = CARTESIAN_POINT ( 'NONE',  ( 4.141030287458704606, -0.1905934838449650226, -1.960285098343496291 ) ) ;
#195305 = ORIENTED_EDGE ( 'NONE', *, *, #149058, .F. ) ;
#195306 = CARTESIAN_POINT ( 'NONE',  ( 5.021012369077997306, -1.842940949158570207, 0.6126725321249880674 ) ) ;
#195307 = ORIENTED_EDGE ( 'NONE', *, *, #23415, .F. ) ;
#195308 = CARTESIAN_POINT ( 'NONE',  ( -7.611976899429754084, 7.845337568948314022, 0.7998128361456341429 ) ) ;
#195310 = CARTESIAN_POINT ( 'NONE',  ( 5.062787373817618786, 0.6179034821891697948, 2.028544477791139222 ) ) ;
#195309 = CARTESIAN_POINT ( 'NONE',  ( 7.028976294042106332, 7.165170195996068969, 0.000000000000000000 ) ) ;
#195311 = CARTESIAN_POINT ( 'NONE',  ( 10.95308175811721085, 9.799999999999982947, 1.799999999999999600 ) ) ;
#195313 = EDGE_LOOP ( 'NONE', ( #169765, #194454, #173490, #34003, #43186, #106866, #145769, #52741, #180368 ) ) ;
#195312 = CARTESIAN_POINT ( 'NONE',  ( 3.246637215680724164, 1.866209232881730573, 0.4165188312477489663 ) ) ;
#195314 = CARTESIAN_POINT ( 'NONE',  ( 4.357662274398333757, 7.395159486995275699, -1.145423081618229144 ) ) ;
#195315 = CARTESIAN_POINT ( 'NONE',  ( -9.499801640457404162, -7.008739397177338404, -0.06269018847474143452 ) ) ;
#195316 = VERTEX_POINT ( 'NONE', #105584 ) ;
#195317 = CARTESIAN_POINT ( 'NONE',  ( 0.000000000000000000, -9.999999999999994671, 0.000000000000000000 ) ) ;
#195318 = CARTESIAN_POINT ( 'NONE',  ( 4.740889518710099004, 1.927123460305087965, 0.5820593317791241672 ) ) ;
#195319 = CARTESIAN_POINT ( 'NONE',  ( -4.038416155542518204, 7.756558617010888668, -0.6477684560860890173 ) ) ;
#195320 = CARTESIAN_POINT ( 'NONE',  ( 5.338443970399977978, 1.799313579390570128, 0.3082849261525285600 ) ) ;
#195321 = CARTESIAN_POINT ( 'NONE',  ( 1.328672132201724532, -1.314895749051579132, 1.599177317581280455 ) ) ;
#195322 = CARTESIAN_POINT ( 'NONE',  ( -6.371969008742801144, 10.37778824360119145, 0.7216878364870458196 ) ) ;
#195323 = CARTESIAN_POINT ( 'NONE',  ( -6.616720264197946122, 6.757059058146986708, -0.05018984082068300712 ) ) ;
#195324 = DIRECTION ( 'NONE',  ( -8.881784197001252323E-16, 0.000000000000000000, 1.000000000000000000 ) ) ;
#195325 = CARTESIAN_POINT ( 'NONE',  ( 5.910993886665249164, 1.650546521282238110, 0.8803886038859505270 ) ) ;
#195326 = CARTESIAN_POINT ( 'NONE',  ( 6.317209508963599340, 9.457495962844502557, 1.199719254218462483 ) ) ;
#195327 = CARTESIAN_POINT ( 'NONE',  ( -3.653032323878261600, 6.349289246911547835, -1.199719254218452047 ) ) ;
#195328 = EDGE_CURVE ( 'NONE', #8666, #175384, #175915, .T. ) ;
#195329 = CARTESIAN_POINT ( 'NONE',  ( 0.6823417656249934904, 9.755208333674728394, 1.181850606188764807 ) ) ;
#195330 = CARTESIAN_POINT ( 'NONE',  ( -6.084912014434944894, 5.993485526462540847, -0.7998128361456291469 ) ) ;
#195332 = CARTESIAN_POINT ( 'NONE',  ( -5.112833325684928987, 5.137596099486740897, -0.7216878364870338292 ) ) ;
#195331 = CARTESIAN_POINT ( 'NONE',  ( 6.549078289569694178, -6.948428148671534466, -6.549078289569718159 ) ) ;
#195333 = CARTESIAN_POINT ( 'NONE',  ( -6.579784621333750749, 6.570836901177822931, 0.7998128361456341429 ) ) ;
#195334 = CARTESIAN_POINT ( 'NONE',  ( 1.604436975501881468, 2.067711310959176707, 0.1055696395834623824 ) ) ;
#195335 = CARTESIAN_POINT ( 'NONE',  ( 2.530995666134610911, -1.758555926239983691, 1.178765877976214016 ) ) ;
#195336 = CARTESIAN_POINT ( 'NONE',  ( 7.727257484784855635, 11.10255193463598111, -1.199719254218446718 ) ) ;
#195337 = LINE ( 'NONE', #12294, #160110 ) ;
#195338 = CARTESIAN_POINT ( 'NONE',  ( 0.7077770966438132749, 0.6232387800201264483, -1.868272854783992187 ) ) ;
#195339 = CARTESIAN_POINT ( 'NONE',  ( 4.048816217420559305, 7.761621341895022397, 0.4883610165275272808 ) ) ;
#195340 = CARTESIAN_POINT ( 'NONE',  ( 5.355107487717867265, 5.349972945200037522, 1.040834085586084257E-14 ) ) ;
#195342 = DIRECTION ( 'NONE',  ( 1.000000000000000000, 0.000000000000000000, 0.000000000000000000 ) ) ;
#195341 = CARTESIAN_POINT ( 'NONE',  ( -3.474999999999998312, -3.120833333333331350, 2.006292185433951047 ) ) ;
#195343 = CARTESIAN_POINT ( 'NONE',  ( 2.431904175345489083, 1.079062523900159221, -2.022394142706671616 ) ) ;
#195344 = CARTESIAN_POINT ( 'NONE',  ( 1.084280211047653264, -1.780658692889337091, -0.4022698149812459212 ) ) ;
#195345 = CARTESIAN_POINT ( 'NONE',  ( 2.162237915172473546, 1.912057200688283665, 0.04323261116381121871 ) ) ;
#195346 = CARTESIAN_POINT ( 'NONE',  ( 7.367930134383754215, 7.560616343061329125, -0.7998128361456341429 ) ) ;
#195348 = EDGE_CURVE ( 'NONE', #122450, #49683, #88702, .T. ) ;
#195347 = CARTESIAN_POINT ( 'NONE',  ( 6.765155463094751909, 8.915767345075790828, 1.443375672974076540 ) ) ;
#195349 = CARTESIAN_POINT ( 'NONE',  ( 1.388932857043408742, -1.913036705441802265, -0.6274143624813811604 ) ) ;
#195350 = CARTESIAN_POINT ( 'NONE',  ( 1.955835763735654487, -0.6658547638305843952, 1.845409454533278648 ) ) ;
#195351 = CARTESIAN_POINT ( 'NONE',  ( -8.123306592882240551, 12.62894145833798376, 0.000000000000000000 ) ) ;
#195352 = CARTESIAN_POINT ( 'NONE',  ( -6.527360889975461156, 9.702672574024962415, 1.199719254218452047 ) ) ;
#195353 = CARTESIAN_POINT ( 'NONE',  ( -7.629869294364566734, -5.350481869465718354, -7.876942567271131068 ) ) ;
#195355 = CARTESIAN_POINT ( 'NONE',  ( 3.432247180620687566, 1.726460203109028591, 0.3886401920838201685 ) ) ;
#195354 = CARTESIAN_POINT ( 'NONE',  ( 4.839831225001551829, 2.085006553764104265, 0.1541250707555453237 ) ) ;
#195356 = CARTESIAN_POINT ( 'NONE',  ( -11.33772463945037146, 13.50911576511424173, 3.599999999999998757 ) ) ;
#195358 = CARTESIAN_POINT ( 'NONE',  ( -0.01142137120296871262, -0.4863542539808898280, -2.144715426241408984 ) ) ;
#195357 = DIRECTION ( 'NONE',  ( -0.000000000000000000, -1.000000000000000000, -0.000000000000000000 ) ) ;
#195359 = CARTESIAN_POINT ( 'NONE',  ( 4.681465254972009049, -0.8165918992961908041, 1.536851246062352905 ) ) ;
#195360 = CARTESIAN_POINT ( 'NONE',  ( 9.413438726589914651, 9.876766690643398405, 0.000000000000000000 ) ) ;
#195361 = CARTESIAN_POINT ( 'NONE',  ( 7.341412881700125403, -6.244189044378190445, -6.724721492623487507 ) ) ;
#195362 = CARTESIAN_POINT ( 'NONE',  ( 4.710095198716817144, -1.340344737836828282, -1.099787012688882015 ) ) ;
#195363 =( BOUNDED_SURFACE ( )  B_SPLINE_SURFACE ( 3, 3, ( 
 ( #20971, #69728, #156354, #5781, #119638, #102251, #121791, #56709, #104397, #55635, #135832 ),
 ( #140118, #103324, #187758, #37254, #120720, #40473, #6859, #186693, #205067, #123936, #105483 ),
 ( #38321, #122877, #189904, #72938, #168325, #172603, #170446, #3650, #22032, #109801, #129276 ),
 ( #95643, #91366, #157426, #77215, #93500, #29551, #193100, #28475, #128208, #192019, #78283 ),
 ( #9017, #27401, #210411, #158481, #108728, #207216, #44749, #11138, #175808, #92441, #211474 ),
 ( #79361, #174754, #63109, #144411, #145479, #161694, #10081, #41546, #142259, #62053, #76155 ),
 ( #173689, #42618, #194170, #13288, #208271, #58840, #124995, #59904, #111936, #143334, #159540 ) ),
 .UNSPECIFIED., .T., .F., .T. ) 
 B_SPLINE_SURFACE_WITH_KNOTS ( ( 4, 3, 4 ),
 ( 4, 1, 1, 1, 1, 1, 1, 1, 4 ),
 ( 0.000000000000000000, 0.5000000000000000000, 1.000000000000000000 ),
 ( 0.000000000000000000, 0.2257091236145174484, 0.3979912149639216468, 0.5260416812932605657, 0.6190739408849097458, 0.6862087210430605211, 0.7361363507675404705, 0.7768852254246026989, 0.9999999999999998890 ),
 .UNSPECIFIED. ) 
 GEOMETRIC_REPRESENTATION_ITEM ( )  RATIONAL_B_SPLINE_SURFACE ( (
 ( 1.000000000000000222, 1.000000000000000222, 1.000000000000000000, 1.000000000000000000, 1.000000000000000222, 1.000000000000000000, 1.000000000000000000, 1.000000000000000000, 1.000000000000000222, 1.000000000000000000, 1.000000000000000000),
 ( 0.3333333333333334259, 0.3333333333333334259, 0.3333333333333333148, 0.3333333333333333703, 0.3333333333333334259, 0.3333333333333333703, 0.3333333333333333703, 0.3333333333333334259, 0.3333333333333333703, 0.3333333333333333703, 0.3333333333333333703),
 ( 0.3333333333333334259, 0.3333333333333334259, 0.3333333333333333148, 0.3333333333333333703, 0.3333333333333334259, 0.3333333333333333703, 0.3333333333333333703, 0.3333333333333334259, 0.3333333333333333703, 0.3333333333333333703, 0.3333333333333333703),
 ( 1.000000000000000222, 1.000000000000000222, 1.000000000000000000, 1.000000000000000000, 1.000000000000000222, 1.000000000000000000, 1.000000000000000000, 1.000000000000000000, 1.000000000000000222, 1.000000000000000000, 1.000000000000000000),
 ( 0.3333333333333334259, 0.3333333333333334259, 0.3333333333333333148, 0.3333333333333333703, 0.3333333333333334259, 0.3333333333333333703, 0.3333333333333333703, 0.3333333333333334259, 0.3333333333333333703, 0.3333333333333333703, 0.3333333333333333703),
 ( 0.3333333333333334259, 0.3333333333333334259, 0.3333333333333333148, 0.3333333333333333703, 0.3333333333333334259, 0.3333333333333333703, 0.3333333333333333703, 0.3333333333333334259, 0.3333333333333333703, 0.3333333333333333703, 0.3333333333333333703),
 ( 1.000000000000000222, 1.000000000000000222, 1.000000000000000000, 1.000000000000000000, 1.000000000000000222, 1.000000000000000000, 1.000000000000000000, 1.000000000000000000, 1.000000000000000222, 1.000000000000000000, 1.000000000000000000) ) ) 
 REPRESENTATION_ITEM ( '' )  SURFACE ( )  );
#195364 = CARTESIAN_POINT ( 'NONE',  ( 4.879425774075326849, -0.1113562312203674326, 2.168454086520410495 ) ) ;
#195365 = CARTESIAN_POINT ( 'NONE',  ( 3.765413976293345844, 5.416068943807445635, 1.599625672291267398 ) ) ;
#195366 = CARTESIAN_POINT ( 'NONE',  ( 6.245327377194020535, 0.3399632236478037917, -1.987496870419297013 ) ) ;
#195367 = CARTESIAN_POINT ( 'NONE',  ( 6.375000000015829116, 2.052068128807268188, -3.630807684676397404E-13 ) ) ;
#195368 = CARTESIAN_POINT ( 'NONE',  ( 0.7499999999999920064, 5.014583334016150751, 1.299038105676669330 ) ) ;
#195369 = CARTESIAN_POINT ( 'NONE',  ( 2.924735480247532937, 1.813364411391896969, 0.6504805730627157834 ) ) ;
#195370 = CARTESIAN_POINT ( 'NONE',  ( -0.7500000000000179856, 9.572916667349467446, 1.299038105676658228 ) ) ;
#195371 = CARTESIAN_POINT ( 'NONE',  ( 6.451452576676337536, -1.984925862664425500, 0.9976300440488919952 ) ) ;
#195372 = VERTEX_POINT ( 'NONE', #139136 ) ;
#195373 = CARTESIAN_POINT ( 'NONE',  ( 6.983263157960407419, 1.286439435963281142, 1.962168536134776931 ) ) ;
#195374 = CARTESIAN_POINT ( 'NONE',  ( -0.7500000000000215383, 3.191666666666689967, 1.299038105676671107 ) ) ;
#195375 = CARTESIAN_POINT ( 'NONE',  ( 6.823831386379729302, 6.855558127064808716, -0.7998128361456281477 ) ) ;
#195376 = CARTESIAN_POINT ( 'NONE',  ( 1.541950133533489975, -2.090104109921666620, 0.7524221467923494222 ) ) ;
#195377 = CARTESIAN_POINT ( 'NONE',  ( 6.865691018405424728, -0.4312029709039078562, 1.920920986087648163 ) ) ;
#195378 = CARTESIAN_POINT ( 'NONE',  ( 6.643132081016105417, 10.69414516125339887, 0.7216878364870438212 ) ) ;
#195379 = CARTESIAN_POINT ( 'NONE',  ( -9.829298179783291900, 11.53023130024440768, 1.082531754730558626 ) ) ;
#195380 = AXIS2_PLACEMENT_3D ( 'NONE', #213155, #194789, #47506 ) ;
#195381 = CARTESIAN_POINT ( 'NONE',  ( 6.373741612200160667, 9.489763409991955001, 1.082531754730549078 ) ) ;
#195382 = CARTESIAN_POINT ( 'NONE',  ( 0.1236729436712938751, 0.3474707636354073537, 1.986100063511665237 ) ) ;
#195384 = CARTESIAN_POINT ( 'NONE',  ( 5.916483495826922123, 0.8326555988564422472, 1.887315221659194631 ) ) ;
#195383 = CARTESIAN_POINT ( 'NONE',  ( 9.541187415715040032, 12.15447128979948310, -1.599625672291262513 ) ) ;
#195385 = CYLINDRICAL_SURFACE ( 'NONE', #26583, 0.07999999999999998779 ) ;
#195386 = CARTESIAN_POINT ( 'NONE',  ( -4.009460741339347045, 5.700790169694431420, -1.599625672291256295 ) ) ;
#195387 = CIRCLE ( 'NONE', #160748, 12.00000000000000178 ) ;
#195389 = EDGE_CURVE ( 'NONE', #85120, #131174, #85125, .T. ) ;
#195388 = CARTESIAN_POINT ( 'NONE',  ( -1.201851678989727383E-14, 4.868750000682822154, -1.732050807568863648 ) ) ;
#195390 = CARTESIAN_POINT ( 'NONE',  ( -1.402160292154681736E-14, 0.5718750003414239114, 1.575800808251672791 ) ) ;
#195391 = CARTESIAN_POINT ( 'NONE',  ( 0.7898890640410756170, -1.755383811729524624, -0.2245491444978504059 ) ) ;
#195392 = CARTESIAN_POINT ( 'NONE',  ( 6.065060216814489813, -0.9193275656586662459, 1.470200510888696632 ) ) ;
#195393 = CARTESIAN_POINT ( 'NONE',  ( 4.177133728293176418, 1.140962030703307928, 1.314357115670391707 ) ) ;
#195394 = CARTESIAN_POINT ( 'NONE',  ( 3.388648328411762556, 6.040841252200647382, 1.199719254218462483 ) ) ;
#195395 = CARTESIAN_POINT ( 'NONE',  ( 3.351411269679291038, 0.5553372447333758677, -2.223988721106509470 ) ) ;
#195396 = CARTESIAN_POINT ( 'NONE',  ( -0.6823417656249969321, 5.780208333674756283, -1.181850606188749264 ) ) ;
#195397 = CARTESIAN_POINT ( 'NONE',  ( 1.271164299617353333, 1.095269041189731452, 1.479763895647051353 ) ) ;
#195398 = EDGE_CURVE ( 'NONE', #125687, #158402, #191765, .T. ) ;
#195399 = FACE_OUTER_BOUND ( 'NONE', #71418, .T. ) ;
#195400 = DIRECTION ( 'NONE',  ( -0.000000000000000000, 1.000000000000000000, 1.804652791718263484E-16 ) ) ;
#195401 = CARTESIAN_POINT ( 'NONE',  ( 1.676486011727536418, -1.732352342712149440, -0.5761224636358779350 ) ) ;
#195402 = CARTESIAN_POINT ( 'NONE',  ( 2.777970385693105726, 1.728001979019553325, -1.038993764437286416 ) ) ;
#195403 = CARTESIAN_POINT ( 'NONE',  ( 1.552940555598739891, -1.880887156831068552, -1.124362282834884263 ) ) ;
#195404 = CARTESIAN_POINT ( 'NONE',  ( 8.233435442164850571, 14.52223435847226618, -8.288968424944320290 ) ) ;
#195405 = CARTESIAN_POINT ( 'NONE',  ( 4.366313571243555458, 0.9904663015308888818, 1.858490915321360237 ) ) ;
#195406 = CARTESIAN_POINT ( 'NONE',  ( -5.852315862593199469, 9.979452273000736895, 0.7998128361456481317 ) ) ;
#195407 = CARTESIAN_POINT ( 'NONE',  ( 8.327294770833812976, 13.18750184243608103, 8.540276611412847885 ) ) ;
#195408 = VECTOR ( 'NONE', #188282, 1000.000000000000000 ) ;
#195409 = CARTESIAN_POINT ( 'NONE',  ( 1.328672132201724532, -1.314895749051579132, 1.599177317581280455 ) ) ;
#195410 = CARTESIAN_POINT ( 'NONE',  ( 6.505214776458575265, 6.483838748823460563, 1.040834085586084257E-14 ) ) ;
#195411 = CARTESIAN_POINT ( 'NONE',  ( -1.360316468750028651, -1.078124999658591765, -4.510281037539698445E-14 ) ) ;
#195412 = CARTESIAN_POINT ( 'NONE',  ( 3.352298257493666167, 0.9517314053594098100, -1.894962337767625904 ) ) ;
#195413 = CARTESIAN_POINT ( 'NONE',  ( 0.1000542341482368452, -1.926035175483146400, -0.04890095678477742597 ) ) ;
#195414 = VERTEX_POINT ( 'NONE', #211576 ) ;
#195415 = CARTESIAN_POINT ( 'NONE',  ( -6.306477729012051725, 7.386587434382707151, 1.199719254218452047 ) ) ;
#195416 = CARTESIAN_POINT ( 'NONE',  ( 8.398386088661320414, 11.88553530582519357, -1.199719254218446718 ) ) ;
#195417 = CARTESIAN_POINT ( 'NONE',  ( 6.821160681006793070, 7.130644680695653825, 0.7216878364870328300 ) ) ;
#195418 = CARTESIAN_POINT ( 'NONE',  ( 1.737500000000001155, -2.639583332377418046, 3.009438278150922130 ) ) ;
#195419 = CARTESIAN_POINT ( 'NONE',  ( -6.389970470742427189, 6.349387058821269747, -0.7998128361456291469 ) ) ;
#195420 = CARTESIAN_POINT ( 'NONE',  ( 6.152600690169603759, 2.097733681304454034, 0.3095894981632040244 ) ) ;
#195421 = CARTESIAN_POINT ( 'NONE',  ( 0.7453164640696362531, -1.806240154289909139, 1.082582905463305378 ) ) ;
#195422 = CARTESIAN_POINT ( 'NONE',  ( -6.005335696210345020, 5.970922831858983315, 0.7998128361456281477 ) ) ;
#195423 = CARTESIAN_POINT ( 'NONE',  ( 8.378048858240820351, 11.86180853700128601, -1.199719254218446718 ) ) ;
#195424 = CARTESIAN_POINT ( 'NONE',  ( 5.664867498354182018, 1.410286671683948168, -1.214315750818369510 ) ) ;
#195425 = CARTESIAN_POINT ( 'NONE',  ( 7.293396569147545527, 10.59638086639245280, 1.199719254218460707 ) ) ;
#195426 = CARTESIAN_POINT ( 'NONE',  ( -0.5727075793229210454, 4.245792387587058236, -0.3118784721225407730 ) ) ;
#195427 = CARTESIAN_POINT ( 'NONE',  ( -3.447516199624892419, 7.244129009529488350, 0.7998128361456352531 ) ) ;
#195428 = CARTESIAN_POINT ( 'NONE',  ( -9.083599731475995753, 11.62061899152058686, 1.443375672974064550 ) ) ;
#195430 = CARTESIAN_POINT ( 'NONE',  ( 1.908577322519442454, 0.6123880975643315461, 1.863924812142327525 ) ) ;
#195429 = CARTESIAN_POINT ( 'NONE',  ( -6.612626235163205024, 8.737816579155630592, -1.599625672291263179 ) ) ;
#195431 = CARTESIAN_POINT ( 'NONE',  ( 1.516726440323381331, 1.451591637995581996, -1.601975981646540426 ) ) ;
#195432 = CIRCLE ( 'NONE', #57038, 1.224999999999996980 ) ;
#195434 = CARTESIAN_POINT ( 'NONE',  ( -5.544970132138452357, 6.385306161890050625, 1.248999107086716798 ) ) ;
#195433 = CARTESIAN_POINT ( 'NONE',  ( -6.947627372360122955, 7.070263120700404968, 0.000000000000000000 ) ) ;
#195435 = CARTESIAN_POINT ( 'NONE',  ( 0.6823417656249899377, 0.5927083336747518416, 1.181850606188755259 ) ) ;
#195436 = CARTESIAN_POINT ( 'NONE',  ( 3.040114402249920911, 1.647253858686392958, -0.5413168154804471888 ) ) ;
#195437 = CARTESIAN_POINT ( 'NONE',  ( 2.905909708737213659, 1.260233761464889302, -1.200475698291984861 ) ) ;
#195438 = CARTESIAN_POINT ( 'NONE',  ( 7.619319141200070256, 8.951922421897323900, 1.082531754730558626 ) ) ;
#195439 = CARTESIAN_POINT ( 'NONE',  ( -11.97594889418004804, 7.449136658168690417, 0.9368335759953716479 ) ) ;
#195440 = CARTESIAN_POINT ( 'NONE',  ( 2.372404410299948196, -1.270453386316850342, 1.622462496149602140 ) ) ;
#195441 = CARTESIAN_POINT ( 'NONE',  ( 0.7552322466577044979, -2.000550463317086525, -0.2495714061315074117 ) ) ;
#195442 = CARTESIAN_POINT ( 'NONE',  ( 6.925078400183575233, 4.688909937558557672, 2.706876980850602354 ) ) ;
#195443 = CARTESIAN_POINT ( 'NONE',  ( -5.147255595043616516, 6.034161611419515125, 1.199719254218452935 ) ) ;
#195444 = CARTESIAN_POINT ( 'NONE',  ( 0.9187500235564357576, 1.820693165844145867, 0.7566030219750378150 ) ) ;
#195445 = COLOUR_RGB ( '', 0.40784314, 0.44705882, 0.49803922) ;
#195447 = CARTESIAN_POINT ( 'NONE',  ( -4.489158259900630554, 8.251452046610447510, 0.000000000000000000 ) ) ;
#195446 = CARTESIAN_POINT ( 'NONE',  ( 5.326388512780113160, -0.8654452107222168067, -1.705464787417856787 ) ) ;
#195448 = CARTESIAN_POINT ( 'NONE',  ( -5.411112705185557203, 9.327065566109540740, 0.7216878364870267237 ) ) ;
#195449 = CARTESIAN_POINT ( 'NONE',  ( 6.770317605177710085, 8.992066187497757213, 1.599625672291268286 ) ) ;
#195450 = CIRCLE ( 'NONE', #181646, 4.021913119055696484 ) ;
#195451 = CARTESIAN_POINT ( 'NONE',  ( -6.312203035614172286, 9.521931420595302953, -1.199719254218452047 ) ) ;
#195452 = CARTESIAN_POINT ( 'NONE',  ( 1.260422244424246108, 2.017472913078500518, 0.09673469748067325957 ) ) ;
#195453 = CARTESIAN_POINT ( 'NONE',  ( 4.260959797893453249, -1.712736962785869288, 1.546631824827559454 ) ) ;
#195454 = CARTESIAN_POINT ( 'NONE',  ( 6.250445965835445428, -1.952298026214387194, -0.1936728439068043650 ) ) ;
#195455 = CARTESIAN_POINT ( 'NONE',  ( 1.709737484509077365, 0.5745576563440238926, -1.875703277996950469 ) ) ;
#195456 = CARTESIAN_POINT ( 'NONE',  ( 10.58621901417202515, 11.24501035948919991, -0.7998128361456281477 ) ) ;
#195457 = CARTESIAN_POINT ( 'NONE',  ( 1.452583904633400591, 1.374772708486753370, 1.500000000000001332 ) ) ;
#195458 = ORIENTED_EDGE ( 'NONE', *, *, #141409, .T. ) ;
#195459 = CARTESIAN_POINT ( 'NONE',  ( 1.130240340503264829, 2.115179321838219551, 0.09787962981822571906 ) ) ;
#195461 = CARTESIAN_POINT ( 'NONE',  ( -6.507023659554960204, 9.678945805201045971, 1.199719254218452047 ) ) ;
#195460 = CARTESIAN_POINT ( 'NONE',  ( -4.620631424159025613, 4.285158171140619032, -0.7998128361456221525 ) ) ;
#195462 = CARTESIAN_POINT ( 'NONE',  ( 1.077780131904103156, -1.795810734350095528, -0.4053039038426771712 ) ) ;
#195463 = ORIENTED_EDGE ( 'NONE', *, *, #82643, .T. ) ;
#195464 = CARTESIAN_POINT ( 'NONE',  ( 4.522458045437067753, 1.018072405813482018, 1.917541202323807203 ) ) ;
#195465 = CARTESIAN_POINT ( 'NONE',  ( 11.99424499309541758, 7.649948518832609956, -0.4322994337658502828 ) ) ;
#195466 = CARTESIAN_POINT ( 'NONE',  ( 1.564851893998190135, 0.6701894319398638000, 2.011955567234039677 ) ) ;
#195467 = CARTESIAN_POINT ( 'NONE',  ( -1.499999999999997780, 2.931250000682818158, 1.214306433183764966E-14 ) ) ;
#195468 = CARTESIAN_POINT ( 'NONE',  ( 6.903072767652295383, 11.20533532890304684, 1.040834085586084257E-14 ) ) ;
#195469 = DIRECTION ( 'NONE',  ( 0.000000000000000000, 0.000000000000000000, -1.000000000000000000 ) ) ;
#195470 = CARTESIAN_POINT ( 'NONE',  ( 2.987629706096385895, 1.454891456164056462, 1.459756821352270473 ) ) ;
#195472 = CARTESIAN_POINT ( 'NONE',  ( 0.6261898170028465938, 0.1349980957352381883, 1.836376839866371569 ) ) ;
#195471 = CARTESIAN_POINT ( 'NONE',  ( -7.666245793523398078, 11.03137162816423356, 1.199719254218453823 ) ) ;
#195473 = CARTESIAN_POINT ( 'NONE',  ( -1.201851678989727383E-14, 3.821875000341423689, 1.575800808251672791 ) ) ;
#195474 = CARTESIAN_POINT ( 'NONE',  ( -0.02244404828160087226, 1.323617703852699057, -2.440988974267483957 ) ) ;
#195475 = CARTESIAN_POINT ( 'NONE',  ( -1.500000000000035971, 8.500000000000000000, -9.886859966642585817 ) ) ;
#195476 = CARTESIAN_POINT ( 'NONE',  ( 3.110884140487602867, 1.641001393266024788, -1.557680395459557499 ) ) ;
#195477 = CARTESIAN_POINT ( 'NONE',  ( -8.161645285746702783, 12.46574390010577105, 0.7216878364870478180 ) ) ;
#195478 = CARTESIAN_POINT ( 'NONE',  ( 2.267558116911760902, 0.4800365151868010716, -1.746770699433045415 ) ) ;
#195479 = CARTESIAN_POINT ( 'NONE',  ( 1.850665572125685721, -1.753200486404655090, -0.7725721188126480898 ) ) ;
#195480 = CARTESIAN_POINT ( 'NONE',  ( 3.578635096964689843, 1.315621898185691974, -1.598582974826658010 ) ) ;
#195481 = CARTESIAN_POINT ( 'NONE',  ( 1.364683531249988757, 1.446875000341421469, 0.000000000000000000 ) ) ;
#195482 = CARTESIAN_POINT ( 'NONE',  ( 1.410939872204178602, 1.737622768476089430, 0.9313336078424112596 ) ) ;
#195483 = CARTESIAN_POINT ( 'NONE',  ( 0.1648913374791864117, -1.719061530832368234, -0.8695707864920312335 ) ) ;
#195484 = CARTESIAN_POINT ( 'NONE',  ( 2.553401164250346245, 0.5009360343536627402, -1.802255699741683870 ) ) ;
#195486 = CARTESIAN_POINT ( 'NONE',  ( 4.595450297557979624, 8.489593704440707711, 0.02661077391274621617 ) ) ;
#195485 = CARTESIAN_POINT ( 'NONE',  ( 1.612422076237954860, -2.289831013633353063, 0.2861181584819341706 ) ) ;
#195487 = CARTESIAN_POINT ( 'NONE',  ( 2.927998328727512867, 0.9930260268339460294, 1.573771836281928627 ) ) ;
#195488 = CARTESIAN_POINT ( 'NONE',  ( -1.364683531250012516, 2.488541667008088876, -0.7879004041258289570 ) ) ;
#195489 = CARTESIAN_POINT ( 'NONE',  ( 5.512196432965448700, 2.060465348046951917, -0.09781390707789237859 ) ) ;
#195490 = CARTESIAN_POINT ( 'NONE',  ( -4.737684612971557740, 7.614716917520386374, 1.199719254218464037 ) ) ;
#195491 = CARTESIAN_POINT ( 'NONE',  ( 7.263417608619159083, 9.497073181520933716, -1.599625672291262513 ) ) ;
#195492 = CARTESIAN_POINT ( 'NONE',  ( -1.494007359806937441, 3.367954574834560511, 0.1499524099051025572 ) ) ;
#195493 = CARTESIAN_POINT ( 'NONE',  ( 6.475619172616331909, 2.016361193322095957, -0.6077647485315963438 ) ) ;
#195494 = CARTESIAN_POINT ( 'NONE',  ( -1.364683531250012516, 2.592708333674753174, 0.7879004041258379498 ) ) ;
#195495 = CARTESIAN_POINT ( 'NONE',  ( 5.712251288600168841, -0.9662322189689103169, -1.933677227328117310 ) ) ;
#195496 = CARTESIAN_POINT ( 'NONE',  ( -0.1227786480478709891, -1.806133744752127068, -0.9041943026713550324 ) ) ;
#195497 = CARTESIAN_POINT ( 'NONE',  ( -1.364683531250014514, -0.5114583329919092369, -0.7879004041258359514 ) ) ;
#195498 = CARTESIAN_POINT ( 'NONE',  ( -5.178851490740209229, 7.065079377328788546, 1.443375672974064550 ) ) ;
#195501 = CARTESIAN_POINT ( 'NONE',  ( 4.311129659465574804, 7.013106455143060636, -1.082531754730548412 ) ) ;
#195500 = CARTESIAN_POINT ( 'NONE',  ( 6.825078400183575589, 6.038285016609903799, 2.450557349082567171 ) ) ;
#195499 = CARTESIAN_POINT ( 'NONE',  ( 7.225569521440261767, 7.394528961293920233, -0.7998128361456341429 ) ) ;
#195502 = CARTESIAN_POINT ( 'NONE',  ( -4.359828915246279024, 7.244161613499399799, -1.199719254218455378 ) ) ;
#195503 = CARTESIAN_POINT ( 'NONE',  ( 4.909388789075159742, -1.913262893431907141, 0.6371506334161003426 ) ) ;
#195504 = CARTESIAN_POINT ( 'NONE',  ( -7.232384877886063990, 10.52520055992070525, -1.199719254218446718 ) ) ;
#195506 = CARTESIAN_POINT ( 'NONE',  ( -5.736508391913536897, 9.706693867292189637, 0.7216878364870267237 ) ) ;
#195505 = CARTESIAN_POINT ( 'NONE',  ( -2.415323921528888196, 5.969628341758991930, 0.7998128361456341429 ) ) ;
#195507 = CARTESIAN_POINT ( 'NONE',  ( -1.364683531249997417, 5.009375000341425022, 1.214306433183764966E-14 ) ) ;
#195509 = CARTESIAN_POINT ( 'NONE',  ( -8.012344526598182026E-15, 9.796875000341399797, -1.575800808251669460 ) ) ;
#195508 = CARTESIAN_POINT ( 'NONE',  ( 6.297764839082774735, -0.7330946318361495351, 2.033732118066629457 ) ) ;
#195510 = DIRECTION ( 'NONE',  ( 0.000000000000000000, 0.000000000000000000, 1.000000000000000000 ) ) ;
#195511 = CARTESIAN_POINT ( 'NONE',  ( -11.82472405718483266, 7.630400978341936202, 2.057497206828635239 ) ) ;
#195512 = AXIS2_PLACEMENT_3D ( 'NONE', #70511, #5506, #104123 ) ;
#195514 = CARTESIAN_POINT ( 'NONE',  ( 5.571888728144736902, -0.9040954357531080232, 1.802425742427179012 ) ) ;
#195513 = CARTESIAN_POINT ( 'NONE',  ( -7.361714222096077620, 7.691014135307965738, 0.7216878364870317197 ) ) ;
#195515 = CARTESIAN_POINT ( 'NONE',  ( -1.364683531250000748, -0.4281249996585800854, 0.000000000000000000 ) ) ;
#195516 = CARTESIAN_POINT ( 'NONE',  ( 1.558790235068749030, -1.477961618093760032, -0.8890178537931183733 ) ) ;
#195517 = CARTESIAN_POINT ( 'NONE',  ( 3.549202351727371862, 7.362762853649070571, -0.7998128361456362523 ) ) ;
#195519 = CARTESIAN_POINT ( 'NONE',  ( 5.155843554946782703, 9.237177590738404831, -0.7998128361456481317 ) ) ;
#195518 = CARTESIAN_POINT ( 'NONE',  ( 6.317736394288122170, 10.31451686007074997, 0.7216878364870438212 ) ) ;
#195520 = CARTESIAN_POINT ( 'NONE',  ( -10.64335489816787650, 5.927586918088680434, -5.550313554347075851 ) ) ;
#195521 = CARTESIAN_POINT ( 'NONE',  ( 0.2625039974461966241, -1.576774366707566433, -0.8037556782162450508 ) ) ;
#195522 = CARTESIAN_POINT ( 'NONE',  ( 1.049477475095396573, -1.818952357203638570, 0.8628315626280655959 ) ) ;
#195523 = CARTESIAN_POINT ( 'NONE',  ( -10.50000000000000000, 0.000000000000000000, -3.600000000000002309 ) ) ;
#195524 = CARTESIAN_POINT ( 'NONE',  ( 2.942613154609276638, 2.189964478704994555, 0.2713889102748042736 ) ) ;
#195525 = CARTESIAN_POINT ( 'NONE',  ( 5.225502712144541206, 0.2199120275673121516, -2.159938666613583802 ) ) ;
#195526 = ORIENTED_EDGE ( 'NONE', *, *, #51634, .F. ) ;
#195527 = CARTESIAN_POINT ( 'NONE',  ( 4.167152111353856547, 5.955039778036558040, 1.599625672291262513 ) ) ;
#195528 = CARTESIAN_POINT ( 'NONE',  ( 10.20892648096591770, 11.01276177065614981, -0.7216878364870257245 ) ) ;
#195530 = CARTESIAN_POINT ( 'NONE',  ( 2.038685622454153190, -1.556895902704044765, 1.281378572682637218 ) ) ;
#195529 = CARTESIAN_POINT ( 'NONE',  ( 2.701940546545733568, 1.501232083741442125, 1.497845299259781049 ) ) ;
#195532 = EDGE_LOOP ( 'NONE', ( #39695, #60383, #86313, #175542 ) ) ;
#195531 = CARTESIAN_POINT ( 'NONE',  ( 2.636723998446516948, 1.707110652976281839, 0.6067464242315090406 ) ) ;
#195533 = CARTESIAN_POINT ( 'NONE',  ( 5.091969210384201361, 8.098325291160362482, 1.199719254218452047 ) ) ;
#195534 = ADVANCED_FACE ( 'NONE', ( #11248 ), #194276, .T. ) ;
#195535 = EDGE_CURVE ( 'NONE', #3330, #97860, #185143, .T. ) ;
#195536 = STYLED_ITEM ( 'NONE', ( #204916 ), #120967 ) ;
#195537 = CARTESIAN_POINT ( 'NONE',  ( 6.959412922516382771, 7.013736585890911535, 0.7998128361456341429 ) ) ;
#195539 = CARTESIAN_POINT ( 'NONE',  ( 1.393601161502202590, -1.900819510297278025, 0.2380969459827488588 ) ) ;
#195538 = CARTESIAN_POINT ( 'NONE',  ( -4.925689880466507908, 4.641059703499347044, -0.7998128361456221525 ) ) ;
#195540 = CARTESIAN_POINT ( 'NONE',  ( -2.680963302752293664, 0.4788041664877169534, -0.1016165050528608921 ) ) ;
#195541 = CARTESIAN_POINT ( 'NONE',  ( 0.6311622855796235054, 3.299999999999983391, 0.3999999999999663824 ) ) ;
#195542 = STYLED_ITEM ( 'NONE', ( #29935 ), #191869 ) ;
#195543 = CARTESIAN_POINT ( 'NONE',  ( 5.951666246274797345, 7.966696592119163256, 1.443375672974062551 ) ) ;
#195544 = CARTESIAN_POINT ( 'NONE',  ( 0.6823417656249899377, 0.6552083336747518416, 1.181850606188755259 ) ) ;
#195545 = DIRECTION ( 'NONE',  ( 0.000000000000000000, 0.000000000000000000, 1.000000000000000000 ) ) ;
#195546 = CARTESIAN_POINT ( 'NONE',  ( -9.267161690140662600, 10.77044237904097734, -1.199719254218441611 ) ) ;
#195547 = CARTESIAN_POINT ( 'NONE',  ( 5.137646372127643524, -1.526005641499485810, -1.531359247741073570 ) ) ;
#195548 = CARTESIAN_POINT ( 'NONE',  ( -5.533136088152923904, 6.588318536667425285, 1.082531754730549078 ) ) ;
#195549 = CARTESIAN_POINT ( 'NONE',  ( 4.570507181582611267, 8.346359121906111511, 0.000000000000000000 ) ) ;
#195550 = CARTESIAN_POINT ( 'NONE',  ( 1.670341986359990205, 2.114562342887704283, -0.1611296783964668855 ) ) ;
#195552 = CARTESIAN_POINT ( 'NONE',  ( -11.76696981052429614, 4.673730779118272061, -4.995440715239800156 ) ) ;
#195551 = CARTESIAN_POINT ( 'NONE',  ( -0.7500000000000215383, 5.691666666666685082, 1.299038105676671107 ) ) ;
#195553 =( BOUNDED_SURFACE ( )  B_SPLINE_SURFACE ( 1, 2, ( 
 ( #164297, #117743, #35342, #113486, #183735, #33222, #148057, #166423, #101421, #167493, #130802, #100354, #47374, #14824, #2822, #133963, #195738, #16948, #198894, #50540, #163242, #80916, #67816, #196794, #31115, #15886, #116663, #147006, #99306, #179493, #85169, #19089, #182661, #34281, #18014, #84103, #150190, #213024, #151253, #1759, #32165, #48435, #114551, #98242, #81970, #214063, #131839, #153375, #39620, #123114, #7094, #38561, #119873, #122028, #185852, #3886, #168554, #71023, #37484, #202082, #53741, #139273, #152309, #24412, #23350, #189073, #103561, #137137, #4946, #170684, #154448, #104637, #118799, #105725, #20153, #201027, #86238, #21204, #169620, #87306, #203165, #36411, #136068, #54810, #8182, #120958, #186929, #88380, #22271, #6028, #73167, #40707, #52669, #72097, #171754, #69956, #138207, #204219, #55872, #205303, #187995, #135012, #89460, #155513, #56942, #106811, #184785, #172841, #90526, #156588, #102490, #160846, #112166, #26562, #191186, #126292, #94797, #28711, #174980, #194403, #158713, #157656, #177096, #161925, #207448, #78517, #74266, #25498, #91606, #107899, #178169, #209562, #46045, #140359, #61207, #108960, #193335, #76384, #206377, #29785, #41785, #77452, #159773, #9254, #173925, #95869, #142493, #93733, #10310, #192251, #58004, #75325, #44981, #141442, #124168, #11372, #59067, #42853, #190130, #125228, #111089, #43913, #92669, #208500, #110027, #210649, #143570, #62275, #60135, #27633, #127365, #12438, #128436, #176041, #144634, #149932, #66500, #1501, #99050, #212773, #115356, #32974, #31920, #165105, #114299, #63341, #47114, #213823, #181347, #79587, #83843, #15635, #116412, #130553, #164056, #145706, #48188, #34032, #129500, #97998, #183477, #13515, #196545, #50293, #117486, #81722, #180297, #113231, #101156, #35084, #195481, #67567, #147804, #166165, #65441, #131592, #197593, #49237, #179236, #133710, #428, #16697, #82782, #199716, #51363, #211705, #30860, #148855, #132639, #198645, #96937, #162987, #14568, #182402, #80664, #146755, #64409, #17753, #100105, #136883, #104381, #22015, #134765, #68642, #39371, #36155, #2570, #135814, #202910, #200773, #4694, #40455, #56693, #155262, #87050, #70769, #54554, #3632, #23093, #201837, #53482, #154195, #167242, #52424, #169368, #120701, #118550, #139026, #203972, #151002, #121774, #18830, #184532, #84914, #102234, #153123, #187743, #89208, #168305, #186676, #171501, #6843, #38303, #88125, #205050, #170428, #19902, #85987, #20953, #152062, #5763, #71843, #119620, #72921, #122860, #69710, #188821, #137952, #185604, #55619, #37235, #103307, #105468, #11119, #172586, #140100, #128186, #44729, #194147, #76137, #43663, #175788, #74007, #7922, #193077, #189885, #156336, #75074, #142240, #206127, #158460, #106557, #210389, #94549, #26307, #10061, #208252, #157407, #176842, #141187, #207197, #93481, #24165, #57757, #108706, #59886, #123917 ),
 ( #41527, #209308, #90268, #25246, #110837, #107639, #173671, #91346, #8999, #144389, #27380, #12194, #58822, #159520, #124975, #77195, #174735, #190936, #78265, #42600, #109779, #191998, #92421, #126035, #143315, #60955, #127112, #28455, #160587, #62031, #161672, #131346, #13265, #148608, #31666, #79338, #178988, #95621, #211452, #197341, #47937, #114051, #180044, #97743, #145455, #132393, #115101, #112976, #213571, #29530, #48983, #64161, #163802, #111916, #14310, #65192, #16442, #32714, #196291, #46863, #147549, #30602, #63086, #129256, #146502, #96691, #195226, #162738, #98796, #80405, #66245, #181098, #212519, #198395, #164850, #130303, #82521, #15378, #177, #81472, #50036, #177916, #45795, #144007, #12868, #111525, #142931, #9682, #11810, #75759, #108330, #58444, #175408, #141868, #92037, #158094, #29144, #42213, #128851, #127809, #78941, #207877, #26991, #43281, #60566, #44340, #208931, #8613, #209999, #124598, #90961, #190558, #125657, #59500, #191619, #109402, #140799, #25929, #93098, #112591, #159139, #10741, #192686, #76811, #126725, #177531, #145066, #157027, #110462, #61641, #174350, #176462, #28075, #94168, #95233, #160209, #24859, #77885, #193763, #45409, #161281, #74695, #211069, #62692, #194834, #46468, #206810, #1941, #130975, #81086, #16059, #199074, #133076, #64829, #84285, #48603, #47550, #66934, #51805, #97360, #182846, #178603, #129925, #195913, #212130, #68003, #99478, #150371, #30211, #165536, #213200, #83205, #180716, #96297, #134143, #146117, #181766, #49654, #113660, #63766, #200151, #32342, #198024, #114721, #82143, #162352, #179665, #149287, #31284, #13932, #115777, #163417, #147174, #80014, #14993, #868, #148235, #214237, #132015, #33399, #196965, #50720, #98408, #164472, #34465, #65865, #17129, #116845, #100536, #166611, #18199, #59557, #192744, #126788, #109459, #45467, #212193, #95296, #63831, #31347, #29206, #145123, #128913, #129989, #43339, #94228, #195977, #194894, #47610, #161345, #60626, #177594, #12926, #160266, #79006, #176520, #125716, #175465, #61700, #211129, #141923, #146178, #77945, #178662, #44399, #11868, #207935, #110520, #96359, #191677, #144066, #97421, #75815, #28132, #112653, #179728, #210061, #127869, #27050, #163475, #93158, #159196, #113724, #193819, #13991, #111584, #62753, #46532, #30274, #10796, #76870, #162414, #80075, #142990, #208990, #69134, #147234, #3064, #66996, #181827, #200206, #135256, #201270, #98468, #134197, #81149, #48662, #36652, #167731, #102738, #199133, #166669, #84343, #197025, #131035, #101663, #164533, #64889, #198085, #50778, #114778, #133134, #15057, #119043, #52910, #149349, #116906, #182905, #65927, #85410, #49712, #115841, #1996, #213262, #180776, #17188, #34522, #32402, #185027, #51859, #16119, #183972, #82202, #148295, #214293, #132074, #929, #33460, #117981, #83263, #99536, #165597, #100594, #18260, #150431, #68061, #35584 ) ),
 .UNSPECIFIED., .F., .F., .T. ) 
 B_SPLINE_SURFACE_WITH_KNOTS ( ( 2, 2 ),
 ( 3, 2, 2, 2, 2, 2, 2, 2, 2, 2, 2, 2, 2, 2, 2, 2, 2, 2, 2, 2, 2, 2, 2, 2, 2, 2, 2, 2, 2, 2, 2, 2, 2, 2, 2, 2, 2, 2, 2, 2, 2, 2, 2, 2, 2, 2, 2, 2, 2, 2, 2, 2, 2, 2, 2, 2, 2, 2, 2, 2, 2, 2, 2, 2, 2, 2, 2, 2, 2, 2, 2, 2, 2, 2, 2, 2, 2, 2, 2, 2, 2, 2, 2, 2, 2, 2, 2, 2, 2, 2, 2, 2, 2, 2, 2, 2, 2, 2, 2, 2, 2, 2, 2, 2, 2, 2, 2, 2, 2, 2, 2, 2, 2, 2, 2, 2, 2, 2, 2, 2, 2, 2, 2, 2, 2, 2, 2, 2, 2, 2, 2, 2, 2, 2, 2, 2, 2, 2, 2, 2, 2, 2, 2, 2, 2, 2, 2, 2, 2, 2, 2, 2, 2, 2, 2, 2, 2, 2, 2, 2, 2, 2, 2, 2, 2, 2, 2, 2, 3 ),
 ( 0.000000000000000000, 1.000000000000000000 ),
 ( 0.000000000000000000, 0.005952380952380952051, 0.01190476190476190410, 0.01785714285714285615, 0.02380952380952380820, 0.02976190476190476025, 0.03571428571428571230, 0.04166666666666666435, 0.04761904761904761640, 0.05357142857142856845, 0.05952380952380952051, 0.06547619047619047949, 0.07142857142857142461, 0.07738095238095238360, 0.08333333333333332871, 0.08928571428571428770, 0.09523809523809523281, 0.1011904761904761918, 0.1071428571428571369, 0.1130952380952380959, 0.1190476190476190410, 0.1250000000000000000, 0.1309523809523809590, 0.1369047619047619180, 0.1428571428571428492, 0.1488095238095238082, 0.1547619047619047672, 0.1607142857142857262, 0.1666666666666666574, 0.1726190476190476164, 0.1785714285714285754, 0.1845238095238095344, 0.1904761904761904656, 0.1964285714285714246, 0.2023809523809523836, 0.2083333333333333426, 0.2142857142857142738, 0.2202380952380952328, 0.2261904761904761918, 0.2321428571428571508, 0.2380952380952380820, 0.2440476190476190410, 0.2500000000000000000, 0.2559523809523809312, 0.2619047619047619180, 0.2678571428571428492, 0.2738095238095238360, 0.2797619047619047672, 0.2857142857142856984, 0.2916666666666666852, 0.2976190476190476164, 0.3035714285714285476, 0.3095238095238095344, 0.3154761904761904656, 0.3214285714285714524, 0.3273809523809523836, 0.3333333333333333148, 0.3392857142857143016, 0.3452380952380952328, 0.3511904761904761640, 0.3571428571428571508, 0.3630952380952380820, 0.3690476190476190688, 0.3750000000000000000, 0.3809523809523809312, 0.3869047619047619180, 0.3928571428571428492, 0.3988095238095238360, 0.4047619047619047672, 0.4107142857142856984, 0.4166666666666666852, 0.4226190476190476164, 0.4285714285714285476, 0.4345238095238095344, 0.4404761904761904656, 0.4464285714285714524, 0.4523809523809523836, 0.4583333333333333148, 0.4642857142857143016, 0.4702380952380952328, 0.4761904761904761640, 0.4821428571428571508, 0.4880952380952380820, 0.4940476190476190688, 0.5000000000000000000, 0.5059523809523809312, 0.5119047619047618625, 0.5178571428571429047, 0.5238095238095238360, 0.5297619047619047672, 0.5357142857142856984, 0.5416666666666666297, 0.5476190476190476719, 0.5535714285714286031, 0.5595238095238095344, 0.5654761904761904656, 0.5714285714285713969, 0.5773809523809523281, 0.5833333333333333703, 0.5892857142857143016, 0.5952380952380952328, 0.6011904761904761640, 0.6071428571428570953, 0.6130952380952381375, 0.6190476190476190688, 0.6250000000000000000, 0.6309523809523809312, 0.6369047619047618625, 0.6428571428571429047, 0.6488095238095238360, 0.6547619047619047672, 0.6607142857142856984, 0.6666666666666666297, 0.6726190476190476719, 0.6785714285714286031, 0.6845238095238095344, 0.6904761904761904656, 0.6964285714285713969, 0.7023809523809523281, 0.7083333333333333703, 0.7142857142857143016, 0.7202380952380952328, 0.7261904761904761640, 0.7321428571428570953, 0.7380952380952381375, 0.7440476190476190688, 0.7500000000000000000, 0.7559523809523809312, 0.7619047619047618625, 0.7678571428571429047, 0.7738095238095238360, 0.7797619047619047672, 0.7857142857142856984, 0.7916666666666666297, 0.7976190476190476719, 0.8035714285714286031, 0.8095238095238095344, 0.8154761904761904656, 0.8214285714285713969, 0.8273809523809523281, 0.8333333333333333703, 0.8392857142857143016, 0.8452380952380952328, 0.8511904761904761640, 0.8571428571428570953, 0.8630952380952381375, 0.8690476190476190688, 0.8750000000000000000, 0.8809523809523809312, 0.8869047619047618625, 0.8928571428571429047, 0.8988095238095238360, 0.9047619047619047672, 0.9107142857142856984, 0.9166666666666666297, 0.9226190476190476719, 0.9285714285714286031, 0.9345238095238095344, 0.9404761904761904656, 0.9464285714285713969, 0.9523809523809523281, 0.9583333333333333703, 0.9642857142857143016, 0.9702380952380952328, 0.9761904761904761640, 0.9821428571428570953, 0.9880952380952381375, 0.9940476190476190688, 1.000000000000000000 ),
 .UNSPECIFIED. ) 
 GEOMETRIC_REPRESENTATION_ITEM ( )  RATIONAL_B_SPLINE_SURFACE ( (
 ( 1.000000000000000000, 0.8660254037844387076, 1.000000000000000000, 0.8660254037844387076, 1.000000000000000000, 0.8660254037844387076, 1.000000000000000000, 0.8660254037844387076, 1.000000000000000000, 0.8660254037844387076, 1.000000000000000000, 0.8660254037844387076, 1.000000000000000000, 0.8660254037844387076, 1.000000000000000000, 0.8660254037844387076, 1.000000000000000000, 0.8660254037844387076, 1.000000000000000000, 0.8660254037844387076, 1.000000000000000000, 0.8660254037844387076, 1.000000000000000000, 0.8660254037844387076, 1.000000000000000000, 0.8660254037844387076, 1.000000000000000000, 0.8660254037844387076, 1.000000000000000000, 0.8660254037844387076, 1.000000000000000000, 0.8660254037844387076, 1.000000000000000000, 0.8660254037844387076, 1.000000000000000000, 0.8660254037844387076, 1.000000000000000000, 0.8660254037844387076, 1.000000000000000000, 0.8660254037844387076, 1.000000000000000000, 0.8660254037844387076, 1.000000000000000000, 0.8660254037844387076, 1.000000000000000000, 0.8660254037844387076, 1.000000000000000000, 0.8660254037844387076, 1.000000000000000000, 0.8660254037844387076, 1.000000000000000000, 0.8660254037844387076, 1.000000000000000000, 0.8660254037844387076, 1.000000000000000000, 0.8660254037844387076, 1.000000000000000000, 0.8660254037844387076, 1.000000000000000000, 0.8660254037844387076, 1.000000000000000000, 0.8660254037844387076, 1.000000000000000000, 0.8660254037844387076, 1.000000000000000000, 0.8660254037844387076, 1.000000000000000000, 0.8660254037844387076, 1.000000000000000000, 0.8660254037844387076, 1.000000000000000000, 0.8660254037844387076, 1.000000000000000000, 0.8660254037844387076, 1.000000000000000000, 0.8660254037844387076, 1.000000000000000000, 0.8660254037844387076, 1.000000000000000000, 0.8660254037844387076, 1.000000000000000000, 0.8660254037844387076, 1.000000000000000000, 0.8660254037844387076, 1.000000000000000000, 0.8660254037844387076, 1.000000000000000000, 0.8660254037844387076, 1.000000000000000000, 0.8660254037844387076, 1.000000000000000000, 0.8660254037844387076, 1.000000000000000000, 0.8660254037844387076, 1.000000000000000000, 0.8660254037844387076, 1.000000000000000000, 0.8660254037844387076, 1.000000000000000000, 0.8660254037844387076, 1.000000000000000000, 0.8660254037844387076, 1.000000000000000000, 0.8660254037844387076, 1.000000000000000000, 0.8660254037844387076, 1.000000000000000000, 0.8660254037844387076, 1.000000000000000000, 0.8660254037844387076, 1.000000000000000000, 0.8660254037844387076, 1.000000000000000000, 0.8660254037844387076, 1.000000000000000000, 0.8660254037844387076, 1.000000000000000000, 0.8660254037844387076, 1.000000000000000000, 0.8660254037844387076, 1.000000000000000000, 0.8660254037844387076, 1.000000000000000000, 0.8660254037844387076, 1.000000000000000000, 0.8660254037844387076, 1.000000000000000000, 0.8660254037844387076, 1.000000000000000000, 0.8660254037844387076, 1.000000000000000000, 0.8660254037844387076, 1.000000000000000000, 0.8660254037844387076, 1.000000000000000000, 0.8660254037844387076, 1.000000000000000000, 0.8660254037844387076, 1.000000000000000000, 0.8660254037844387076, 1.000000000000000000, 0.8660254037844387076, 1.000000000000000000, 0.8660254037844387076, 1.000000000000000000, 0.8660254037844387076, 1.000000000000000000, 0.8660254037844387076, 1.000000000000000000, 0.8660254037844387076, 1.000000000000000000, 0.8660254037844387076, 1.000000000000000000, 0.8660254037844387076, 1.000000000000000000, 0.8660254037844387076, 1.000000000000000000, 0.8660254037844387076, 1.000000000000000000, 0.8660254037844387076, 1.000000000000000000, 0.8660254037844387076, 1.000000000000000000, 0.8660254037844387076, 1.000000000000000000, 0.8660254037844387076, 1.000000000000000000, 0.8660254037844387076, 1.000000000000000000, 0.8660254037844387076, 1.000000000000000000, 0.8660254037844387076, 1.000000000000000000, 0.8660254037844387076, 1.000000000000000000, 0.8660254037844387076, 1.000000000000000000, 0.8660254037844387076, 1.000000000000000000, 0.8660254037844387076, 1.000000000000000000, 0.8660254037844387076, 1.000000000000000000, 0.8660254037844387076, 1.000000000000000000, 0.8660254037844387076, 1.000000000000000000, 0.8660254037844387076, 1.000000000000000000, 0.8660254037844387076, 1.000000000000000000, 0.8660254037844387076, 1.000000000000000000, 0.8660254037844387076, 1.000000000000000000, 0.8660254037844387076, 1.000000000000000000, 0.8660254037844387076, 1.000000000000000000, 0.8660254037844387076, 1.000000000000000000, 0.8660254037844387076, 1.000000000000000000, 0.8660254037844387076, 1.000000000000000000, 0.8660254037844387076, 1.000000000000000000, 0.8660254037844387076, 1.000000000000000000, 0.8660254037844387076, 1.000000000000000000, 0.8660254037844387076, 1.000000000000000000, 0.8660254037844387076, 1.000000000000000000, 0.8660254037844387076, 1.000000000000000000, 0.8660254037844387076, 1.000000000000000000, 0.8660254037844387076, 1.000000000000000000, 0.8660254037844387076, 1.000000000000000000, 0.8660254037844387076, 1.000000000000000000, 0.8660254037844387076, 1.000000000000000000, 0.8660254037844387076, 1.000000000000000000, 0.8660254037844387076, 1.000000000000000000, 0.8660254037844387076, 1.000000000000000000, 0.8660254037844387076, 1.000000000000000000, 0.8660254037844387076, 1.000000000000000000, 0.8660254037844387076, 1.000000000000000000, 0.8660254037844387076, 1.000000000000000000, 0.8660254037844387076, 1.000000000000000000, 0.8660254037844387076, 1.000000000000000000, 0.8660254037844387076, 1.000000000000000000, 0.8660254037844387076, 1.000000000000000000, 0.8660254037844387076, 1.000000000000000000, 0.8660254037844387076, 1.000000000000000000, 0.8660254037844387076, 1.000000000000000000, 0.8660254037844387076, 1.000000000000000000, 0.8660254037844387076, 1.000000000000000000, 0.8660254037844387076, 1.000000000000000000, 0.8660254037844387076, 1.000000000000000000, 0.8660254037844387076, 1.000000000000000000, 0.8660254037844387076, 1.000000000000000000, 0.8660254037844387076, 1.000000000000000000, 0.8660254037844387076, 1.000000000000000000, 0.8660254037844387076, 1.000000000000000000, 0.8660254037844387076, 1.000000000000000000, 0.8660254037844387076, 1.000000000000000000, 0.8660254037844387076, 1.000000000000000000, 0.8660254037844387076, 1.000000000000000000, 0.8660254037844387076, 1.000000000000000000, 0.8660254037844387076, 1.000000000000000000, 0.8660254037844387076, 1.000000000000000000, 0.8660254037844387076, 1.000000000000000000, 0.8660254037844387076, 1.000000000000000000, 0.8660254037844387076, 1.000000000000000000, 0.8660254037844387076, 1.000000000000000000, 0.8660254037844387076, 1.000000000000000000, 0.8660254037844387076, 1.000000000000000000, 0.8660254037844387076, 1.000000000000000000, 0.8660254037844387076, 1.000000000000000000, 0.8660254037844387076, 1.000000000000000000, 0.8660254037844387076, 1.000000000000000000, 0.8660254037844387076, 1.000000000000000000, 0.8660254037844387076, 1.000000000000000000, 0.8660254037844387076, 1.000000000000000000, 0.8660254037844387076, 1.000000000000000000, 0.8660254037844387076, 1.000000000000000000, 0.8660254037844387076, 1.000000000000000000, 0.8660254037844387076, 1.000000000000000000, 0.8660254037844387076, 1.000000000000000000, 0.8660254037844387076, 1.000000000000000000, 0.8660254037844387076, 1.000000000000000000, 0.8660254037844387076, 1.000000000000000000, 0.8660254037844387076, 1.000000000000000000, 0.8660254037844387076, 1.000000000000000000, 0.8660254037844387076, 1.000000000000000000, 0.8660254037844387076, 1.000000000000000000),
 ( 1.000000000000000000, 0.8660254037844387076, 1.000000000000000000, 0.8660254037844387076, 1.000000000000000000, 0.8660254037844387076, 1.000000000000000000, 0.8660254037844387076, 1.000000000000000000, 0.8660254037844387076, 1.000000000000000000, 0.8660254037844387076, 1.000000000000000000, 0.8660254037844387076, 1.000000000000000000, 0.8660254037844387076, 1.000000000000000000, 0.8660254037844387076, 1.000000000000000000, 0.8660254037844387076, 1.000000000000000000, 0.8660254037844387076, 1.000000000000000000, 0.8660254037844387076, 1.000000000000000000, 0.8660254037844387076, 1.000000000000000000, 0.8660254037844387076, 1.000000000000000000, 0.8660254037844387076, 1.000000000000000000, 0.8660254037844387076, 1.000000000000000000, 0.8660254037844387076, 1.000000000000000000, 0.8660254037844387076, 1.000000000000000000, 0.8660254037844387076, 1.000000000000000000, 0.8660254037844387076, 1.000000000000000000, 0.8660254037844387076, 1.000000000000000000, 0.8660254037844387076, 1.000000000000000000, 0.8660254037844387076, 1.000000000000000000, 0.8660254037844387076, 1.000000000000000000, 0.8660254037844387076, 1.000000000000000000, 0.8660254037844387076, 1.000000000000000000, 0.8660254037844387076, 1.000000000000000000, 0.8660254037844387076, 1.000000000000000000, 0.8660254037844387076, 1.000000000000000000, 0.8660254037844387076, 1.000000000000000000, 0.8660254037844387076, 1.000000000000000000, 0.8660254037844387076, 1.000000000000000000, 0.8660254037844387076, 1.000000000000000000, 0.8660254037844387076, 1.000000000000000000, 0.8660254037844387076, 1.000000000000000000, 0.8660254037844387076, 1.000000000000000000, 0.8660254037844387076, 1.000000000000000000, 0.8660254037844387076, 1.000000000000000000, 0.8660254037844387076, 1.000000000000000000, 0.8660254037844387076, 1.000000000000000000, 0.8660254037844387076, 1.000000000000000000, 0.8660254037844387076, 1.000000000000000000, 0.8660254037844387076, 1.000000000000000000, 0.8660254037844387076, 1.000000000000000000, 0.8660254037844387076, 1.000000000000000000, 0.8660254037844387076, 1.000000000000000000, 0.8660254037844387076, 1.000000000000000000, 0.8660254037844387076, 1.000000000000000000, 0.8660254037844387076, 1.000000000000000000, 0.8660254037844387076, 1.000000000000000000, 0.8660254037844387076, 1.000000000000000000, 0.8660254037844387076, 1.000000000000000000, 0.8660254037844387076, 1.000000000000000000, 0.8660254037844387076, 1.000000000000000000, 0.8660254037844387076, 1.000000000000000000, 0.8660254037844387076, 1.000000000000000000, 0.8660254037844387076, 1.000000000000000000, 0.8660254037844387076, 1.000000000000000000, 0.8660254037844387076, 1.000000000000000000, 0.8660254037844387076, 1.000000000000000000, 0.8660254037844387076, 1.000000000000000000, 0.8660254037844387076, 1.000000000000000000, 0.8660254037844387076, 1.000000000000000000, 0.8660254037844387076, 1.000000000000000000, 0.8660254037844387076, 1.000000000000000000, 0.8660254037844387076, 1.000000000000000000, 0.8660254037844387076, 1.000000000000000000, 0.8660254037844387076, 1.000000000000000000, 0.8660254037844387076, 1.000000000000000000, 0.8660254037844387076, 1.000000000000000000, 0.8660254037844387076, 1.000000000000000000, 0.8660254037844387076, 1.000000000000000000, 0.8660254037844387076, 1.000000000000000000, 0.8660254037844387076, 1.000000000000000000, 0.8660254037844387076, 1.000000000000000000, 0.8660254037844387076, 1.000000000000000000, 0.8660254037844387076, 1.000000000000000000, 0.8660254037844387076, 1.000000000000000000, 0.8660254037844387076, 1.000000000000000000, 0.8660254037844387076, 1.000000000000000000, 0.8660254037844387076, 1.000000000000000000, 0.8660254037844387076, 1.000000000000000000, 0.8660254037844387076, 1.000000000000000000, 0.8660254037844387076, 1.000000000000000000, 0.8660254037844387076, 1.000000000000000000, 0.8660254037844387076, 1.000000000000000000, 0.8660254037844387076, 1.000000000000000000, 0.8660254037844387076, 1.000000000000000000, 0.8660254037844387076, 1.000000000000000000, 0.8660254037844387076, 1.000000000000000000, 0.8660254037844387076, 1.000000000000000000, 0.8660254037844387076, 1.000000000000000000, 0.8660254037844387076, 1.000000000000000000, 0.8660254037844387076, 1.000000000000000000, 0.8660254037844387076, 1.000000000000000000, 0.8660254037844387076, 1.000000000000000000, 0.8660254037844387076, 1.000000000000000000, 0.8660254037844387076, 1.000000000000000000, 0.8660254037844387076, 1.000000000000000000, 0.8660254037844387076, 1.000000000000000000, 0.8660254037844387076, 1.000000000000000000, 0.8660254037844387076, 1.000000000000000000, 0.8660254037844387076, 1.000000000000000000, 0.8660254037844387076, 1.000000000000000000, 0.8660254037844387076, 1.000000000000000000, 0.8660254037844387076, 1.000000000000000000, 0.8660254037844387076, 1.000000000000000000, 0.8660254037844387076, 1.000000000000000000, 0.8660254037844387076, 1.000000000000000000, 0.8660254037844387076, 1.000000000000000000, 0.8660254037844387076, 1.000000000000000000, 0.8660254037844387076, 1.000000000000000000, 0.8660254037844387076, 1.000000000000000000, 0.8660254037844387076, 1.000000000000000000, 0.8660254037844387076, 1.000000000000000000, 0.8660254037844387076, 1.000000000000000000, 0.8660254037844387076, 1.000000000000000000, 0.8660254037844387076, 1.000000000000000000, 0.8660254037844387076, 1.000000000000000000, 0.8660254037844387076, 1.000000000000000000, 0.8660254037844387076, 1.000000000000000000, 0.8660254037844387076, 1.000000000000000000, 0.8660254037844387076, 1.000000000000000000, 0.8660254037844387076, 1.000000000000000000, 0.8660254037844387076, 1.000000000000000000, 0.8660254037844387076, 1.000000000000000000, 0.8660254037844387076, 1.000000000000000000, 0.8660254037844387076, 1.000000000000000000, 0.8660254037844387076, 1.000000000000000000, 0.8660254037844387076, 1.000000000000000000, 0.8660254037844387076, 1.000000000000000000, 0.8660254037844387076, 1.000000000000000000, 0.8660254037844387076, 1.000000000000000000, 0.8660254037844387076, 1.000000000000000000, 0.8660254037844387076, 1.000000000000000000, 0.8660254037844387076, 1.000000000000000000, 0.8660254037844387076, 1.000000000000000000, 0.8660254037844387076, 1.000000000000000000, 0.8660254037844387076, 1.000000000000000000, 0.8660254037844387076, 1.000000000000000000, 0.8660254037844387076, 1.000000000000000000, 0.8660254037844387076, 1.000000000000000000, 0.8660254037844387076, 1.000000000000000000, 0.8660254037844387076, 1.000000000000000000, 0.8660254037844387076, 1.000000000000000000, 0.8660254037844387076, 1.000000000000000000, 0.8660254037844387076, 1.000000000000000000, 0.8660254037844387076, 1.000000000000000000, 0.8660254037844387076, 1.000000000000000000, 0.8660254037844387076, 1.000000000000000000, 0.8660254037844387076, 1.000000000000000000, 0.8660254037844387076, 1.000000000000000000, 0.8660254037844387076, 1.000000000000000000, 0.8660254037844387076, 1.000000000000000000, 0.8660254037844387076, 1.000000000000000000, 0.8660254037844387076, 1.000000000000000000, 0.8660254037844387076, 1.000000000000000000, 0.8660254037844387076, 1.000000000000000000, 0.8660254037844387076, 1.000000000000000000, 0.8660254037844387076, 1.000000000000000000, 0.8660254037844387076, 1.000000000000000000, 0.8660254037844387076, 1.000000000000000000, 0.8660254037844387076, 1.000000000000000000, 0.8660254037844387076, 1.000000000000000000, 0.8660254037844387076, 1.000000000000000000, 0.8660254037844387076, 1.000000000000000000, 0.8660254037844387076, 1.000000000000000000, 0.8660254037844387076, 1.000000000000000000) ) ) 
 REPRESENTATION_ITEM ( '' )  SURFACE ( )  );
#195554 = CARTESIAN_POINT ( 'NONE',  ( 3.391827608253958015, -0.8021585586163967330, 1.800962559972321575 ) ) ;
#195555 = CARTESIAN_POINT ( 'NONE',  ( 5.343983030329363615, -1.218012673290536974, -1.474316871017400166 ) ) ;
#195556 = VERTEX_POINT ( 'NONE', #193209 ) ;
#195557 = CARTESIAN_POINT ( 'NONE',  ( -7.720982897393583677, -6.134628647623485698, 7.834948825496934610 ) ) ;
#195558 = CARTESIAN_POINT ( 'NONE',  ( 0.1861046438572169504, -1.272802160389638892, -1.633586439835111648 ) ) ;
#195559 = CARTESIAN_POINT ( 'NONE',  ( 2.677597413788167735, -0.9980636400313472878, 1.665709379616100883 ) ) ;
#195560 = ORIENTED_EDGE ( 'NONE', *, *, #188476, .T. ) ;
#195561 = CARTESIAN_POINT ( 'NONE',  ( -4.240783329467897822, 7.329537114711067503, -0.8835190343243297662 ) ) ;
#195563 = CARTESIAN_POINT ( 'NONE',  ( 6.770317605177710085, 8.992066187497757213, 1.599625672291268286 ) ) ;
#195562 = CARTESIAN_POINT ( 'NONE',  ( -7.607533591043815768, 8.048079742405473525, 0.000000000000000000 ) ) ;
#195565 = CARTESIAN_POINT ( 'NONE',  ( 5.524057522564145728, 8.532151978711786100, 1.199719254218462483 ) ) ;
#195564 = CARTESIAN_POINT ( 'NONE',  ( 2.783241352837596327, 1.478939484563842610, 1.477931775543766202 ) ) ;
#195566 = CARTESIAN_POINT ( 'NONE',  ( 3.540087506499646874, 7.144202834309300698, -0.7216878364870338292 ) ) ;
#195568 = EDGE_LOOP ( 'NONE', ( #63023, #122797, #45817, #28534, #119267, #81685, #116482, #172666, #5360, #122644, #2242 ) ) ;
#195567 = CARTESIAN_POINT ( 'NONE',  ( 6.633470332280523074, -0.1331818211787652029, 1.881796397474523541 ) ) ;
#195569 = CARTESIAN_POINT ( 'NONE',  ( 4.160898416275903067, -1.636102012888400292, 1.481223685352812458 ) ) ;
#195570 = CARTESIAN_POINT ( 'NONE',  ( 2.854729849855553780, 0.7423848465729750989, 2.078289375090878632 ) ) ;
#195571 =( NAMED_UNIT ( * ) SI_UNIT ( $, .STERADIAN. ) SOLID_ANGLE_UNIT ( ) );
#195572 = CARTESIAN_POINT ( 'NONE',  ( 1.646971982979035909, 0.1886418863925183320, 1.902964618272011021 ) ) ;
#195573 = CARTESIAN_POINT ( 'NONE',  ( -1.843739406749240750, 9.999999999999998224, -0.7749999999999996891 ) ) ;
#195574 = CARTESIAN_POINT ( 'NONE',  ( 9.561524646135536543, 12.17819805862340310, -1.599625672291262513 ) ) ;
#195575 = CARTESIAN_POINT ( 'NONE',  ( 4.475093801846619535, 1.891600172242546840, 0.8420093967692193759 ) ) ;
#195576 = AXIS2_PLACEMENT_3D ( 'NONE', #56475, #8780, #172364 ) ;
#195578 = CARTESIAN_POINT ( 'NONE',  ( 1.833122199354455972, 0.2117775504973731793, 2.151289291301178075 ) ) ;
#195577 = CARTESIAN_POINT ( 'NONE',  ( -1.499999999999997780, 3.900000000000021672, 1.214306433183764966E-14 ) ) ;
#195579 = CARTESIAN_POINT ( 'NONE',  ( 5.021103811603734535, -2.081066139062941023, 0.6872292908843835590 ) ) ;
#195580 = CARTESIAN_POINT ( 'NONE',  ( -5.853222892721556825, 6.632591286734531799, 0.9264282755401199720 ) ) ;
#195581 = DIRECTION ( 'NONE',  ( 0.000000000000000000, 0.000000000000000000, 1.000000000000000000 ) ) ;
#195582 = CARTESIAN_POINT ( 'NONE',  ( -8.752797858673307729, 15.44734748039404515, 8.156385747514464768 ) ) ;
#195583 = CARTESIAN_POINT ( 'NONE',  ( 4.389807875774629942, 8.343469298370917997, 0.7998128361456271485 ) ) ;
#195584 = CARTESIAN_POINT ( 'NONE',  ( 1.364683531250000303, 14.81770833367472839, -0.7879004041258355073 ) ) ;
#195585 = CARTESIAN_POINT ( 'NONE',  ( -4.980641328173854632, 6.904110530993182948, 1.599625672291263179 ) ) ;
#195586 = CARTESIAN_POINT ( 'NONE',  ( -0.1048463755018592264, -0.8645036352170620830, -1.819965476435807306 ) ) ;
#195588 = CARTESIAN_POINT ( 'NONE',  ( -9.029367117021344313, 9.636609179387466639, 0.7216878364870438212 ) ) ;
#195587 = CIRCLE ( 'NONE', #102195, 0.07999999999999997391 ) ;
#195589 = CARTESIAN_POINT ( 'NONE',  ( 4.627825472248149552, 2.009385113269086087, -0.4979276649561757417 ) ) ;
#195590 = CARTESIAN_POINT ( 'NONE',  ( 3.721244860960619683, -0.1409348896288381003, 1.921400582950444580 ) ) ;
#195591 = CARTESIAN_POINT ( 'NONE',  ( 5.923477664823041167, -1.533883339688602465, -1.459648931523350068 ) ) ;
#195592 = CARTESIAN_POINT ( 'NONE',  ( 5.636439174979242850, 7.598931675607687453, -1.599625672291262513 ) ) ;
#195593 = CARTESIAN_POINT ( 'NONE',  ( 9.518950567327420842, 3.582805947357989851, 7.307358422849582702 ) ) ;
#195594 = CARTESIAN_POINT ( 'NONE',  ( 4.328926673881399623, -1.836050571085739769, -0.7129182788949259830 ) ) ;
#195595 = CARTESIAN_POINT ( 'NONE',  ( 5.630919443038269634, -2.074398886797897301, 0.9756724061340553700 ) ) ;
#195596 = CARTESIAN_POINT ( 'NONE',  ( 3.510199737632841543, -0.7410081052188907114, -1.668730646197075673 ) ) ;
#195597 = AXIS2_PLACEMENT_3D ( 'NONE', #117608, #167366, #134885 ) ;
#195598 = CARTESIAN_POINT ( 'NONE',  ( 5.722950238744198614, 8.730506807626655430, 1.082531754730549967 ) ) ;
#195600 = EDGE_CURVE ( 'NONE', #66223, #170318, #65156, .T. ) ;
#195599 = CARTESIAN_POINT ( 'NONE',  ( 5.327991180046175224, 5.318337252916401248, -0.7216878364870207285 ) ) ;
#195601 = CARTESIAN_POINT ( 'NONE',  ( -5.284646014276622950, 9.387447126623207794, -0.7998128361456362523 ) ) ;
#195602 = CARTESIAN_POINT ( 'NONE',  ( 4.342354338126830804, 8.288106837781779035, -0.7998128361456381397 ) ) ;
#195603 = ORIENTED_EDGE ( 'NONE', *, *, #85587, .T. ) ;
#195605 = CARTESIAN_POINT ( 'NONE',  ( 5.343998949255959197, -1.280338926806196431, -1.553582282148850524 ) ) ;
#195604 = CARTESIAN_POINT ( 'NONE',  ( 1.118424870118275738, -0.04499623084481922664, 1.840855209834332928 ) ) ;
#195606 = CARTESIAN_POINT ( 'NONE',  ( 5.994848186622900421, -2.281820642442307090, 0.2777966721622132096 ) ) ;
#195607 = CARTESIAN_POINT ( 'NONE',  ( 5.946142449018281262, -0.8852437533515828960, 1.750773106858094952 ) ) ;
#195608 = CARTESIAN_POINT ( 'NONE',  ( -7.203459687562382641, 7.298457811777897319, -0.7998128361456291469 ) ) ;
#195609 = CARTESIAN_POINT ( 'NONE',  ( -4.141125853970233806, 6.918731698685530063, -1.199719254218452047 ) ) ;
#195610 = CARTESIAN_POINT ( 'NONE',  ( -6.608673532018475960, 6.674816973635147477, -0.7998128361456362523 ) ) ;
#195612 = CARTESIAN_POINT ( 'NONE',  ( 6.684453129459355658, -1.736675761049325972, -0.3400495950729911510 ) ) ;
#195611 = CARTESIAN_POINT ( 'NONE',  ( 1.663735998746267652, 1.077533827470295913, 1.791552697131219229 ) ) ;
#195613 = CARTESIAN_POINT ( 'NONE',  ( 1.284279953904125193, 3.003360285806104368, 0.7750000000000065725 ) ) ;
#195614 = CARTESIAN_POINT ( 'NONE',  ( 5.982362851901904754, -0.2873240852911072007, -1.920464370370161600 ) ) ;
#195615 = B_SPLINE_CURVE_WITH_KNOTS ( 'NONE', 3,
 ( #81790, #147873, #200833, #131657 ),
 .UNSPECIFIED., .F., .F.,
 ( 4, 4 ),
 ( 0.001170373960510463426, 0.001235641208627095413 ),
 .UNSPECIFIED. ) ;
#195616 = CARTESIAN_POINT ( 'NONE',  ( -0.1106727585416019261, 5.721739388512169455, -2.597565591738408841 ) ) ;
#195617 = CARTESIAN_POINT ( 'NONE',  ( 1.012787145881738793, -1.698268246007793802, 0.3799501884491280901 ) ) ;
#195618 = CARTESIAN_POINT ( 'NONE',  ( 6.796715079152391148, 6.823922435299587974, 0.7998128361456341429 ) ) ;
#195620 = CARTESIAN_POINT ( 'NONE',  ( 1.224999999999996980, 1.687500000682823353, -2.602085213965210642E-14 ) ) ;
#195619 = CARTESIAN_POINT ( 'NONE',  ( 4.963960565410041603, 8.060099936542098220, -1.154953748940761971 ) ) ;
#195621 = CARTESIAN_POINT ( 'NONE',  ( 1.734533752015484875, 0.1665512568347452815, 1.716820151450085596 ) ) ;
#195623 = EDGE_CURVE ( 'NONE', #138616, #147438, #132353, .T. ) ;
#195622 = CARTESIAN_POINT ( 'NONE',  ( 1.857222401600963302, 0.3706860215506869172, -2.159823580554325329 ) ) ;
#195624 = CARTESIAN_POINT ( 'NONE',  ( 3.791807063958370971, 1.597966631936774684, 1.522356218736670153 ) ) ;
#195625 = CARTESIAN_POINT ( 'NONE',  ( -10.30104275384242740, 4.689840931292195592, -5.506867539468097483 ) ) ;
#195626 = CARTESIAN_POINT ( 'NONE',  ( 1.815514387157551646, -1.860550965366158715, -1.118705476460989168 ) ) ;
#195627 = CARTESIAN_POINT ( 'NONE',  ( 1.230728480726485330, 3.105010058876359835, -0.7749999999999926947 ) ) ;
#195628 = CARTESIAN_POINT ( 'NONE',  ( 1.903655596893740087, -2.052436370740511773, 0.5197080100793128876 ) ) ;
#195629 = FACE_OUTER_BOUND ( 'NONE', #175201, .T. ) ;
#195630 = ORIENTED_EDGE ( 'NONE', *, *, #99196, .F. ) ;
#195632 = CARTESIAN_POINT ( 'NONE',  ( -1.364683531250000748, -0.6781249996585803075, 0.000000000000000000 ) ) ;
#195631 = CARTESIAN_POINT ( 'NONE',  ( 2.279227788079383643, 2.094250403060330168, -0.9326617097511098464 ) ) ;
#195633 = CARTESIAN_POINT ( 'NONE',  ( -15.75000000000000000, 10.90000000000000036, -1.400000000000001910 ) ) ;
#195634 = CARTESIAN_POINT ( 'NONE',  ( 5.626797444871351139, 6.523350759560078593, 1.199719254218462483 ) ) ;
#195635 = CARTESIAN_POINT ( 'NONE',  ( 6.059279899546098136, -1.878006040282210298, 1.186031488430500769 ) ) ;
#195636 = CARTESIAN_POINT ( 'NONE',  ( -5.910991785878158211, 9.839981483592442402, -0.7216878364870278340 ) ) ;
#195637 = CARTESIAN_POINT ( 'NONE',  ( 5.558479791922850133, 6.547609847740540445, -1.082531754730542195 ) ) ;
#195638 = CARTESIAN_POINT ( 'NONE',  ( -8.148087131688699358, 8.608449196499371681, -0.7216878364870267237 ) ) ;
#195639 = CARTESIAN_POINT ( 'NONE',  ( 3.431622278034673901, 7.017660067766835930, -1.734723475976807094E-15 ) ) ;
#195640 = ORIENTED_EDGE ( 'NONE', *, *, #13231, .F. ) ;
#195641 = CARTESIAN_POINT ( 'NONE',  ( 2.742814741689561853, 2.006446121045248887, -0.2004354718553730264 ) ) ;
#195643 = CARTESIAN_POINT ( 'NONE',  ( 2.149356475496758456, 1.796580072245733462, -1.012980232677022974 ) ) ;
#195642 = CARTESIAN_POINT ( 'NONE',  ( 7.070740804726770357, 8.207951346058097286, 1.199719254218462483 ) ) ;
#195644 = DIRECTION ( 'NONE',  ( 0.000000000000000000, -1.000000000000000000, 0.000000000000000000 ) ) ;
#195645 = CARTESIAN_POINT ( 'NONE',  ( 5.682275777458851707, 6.762314840857718501, 1.082531754730549078 ) ) ;
#195646 = ORIENTED_EDGE ( 'NONE', *, *, #138353, .F. ) ;
#195648 = EDGE_CURVE ( 'NONE', #139393, #60282, #209727, .T. ) ;
#195647 = CARTESIAN_POINT ( 'NONE',  ( -7.548736465707863275, -7.034525073441514564, -7.548736465707114540 ) ) ;
#195649 = CARTESIAN_POINT ( 'NONE',  ( -1.001543065824772872E-14, 5.321875000341422357, 1.575800808251672791 ) ) ;
#195650 = CARTESIAN_POINT ( 'NONE',  ( 5.349643074071059878, 2.189064600896481139, -0.1049423877047955811 ) ) ;
#195651 = CARTESIAN_POINT ( 'NONE',  ( 2.953750172290268150, -1.864168560446223033, -0.7691209412190866956 ) ) ;
#195652 = CARTESIAN_POINT ( 'NONE',  ( 1.733694375844633706, 1.821329977863223926, 0.2691589665217360983 ) ) ;
#195653 = EDGE_CURVE ( 'NONE', #175582, #163622, #96812, .T. ) ;
#195654 = CARTESIAN_POINT ( 'NONE',  ( 8.132193210098487057, 8.381980254736715708, 1.040834085586084257E-14 ) ) ;
#195655 = CARTESIAN_POINT ( 'NONE',  ( 5.227504313999177477, -1.733024862908550290, 0.5741523302658231298 ) ) ;
#195656 = CARTESIAN_POINT ( 'NONE',  ( 5.695935454815424848, 1.779625283580280382, 0.9480427965274510482 ) ) ;
#195657 = CARTESIAN_POINT ( 'NONE',  ( -8.864333505236459132, 9.236143932397675727, 1.040834085586084257E-14 ) ) ;
#195659 = CARTESIAN_POINT ( 'NONE',  ( -4.606738333593328072, 8.596554832492683929, 0.7998128361456281477 ) ) ;
#195658 = CARTESIAN_POINT ( 'NONE',  ( 5.788003261412111300, -1.023269635773180752, 2.017978558835635372 ) ) ;
#195660 = CARTESIAN_POINT ( 'NONE',  ( 0.9617104568129207776, 0.4090027284681818642, -2.065791855309044411 ) ) ;
#195661 = CARTESIAN_POINT ( 'NONE',  ( -7.611976899429754084, 7.845337568948314022, 0.7998128361456341429 ) ) ;
#195662 = CARTESIAN_POINT ( 'NONE',  ( 10.40318394038753702, 11.03146944007395724, -0.7998128361456281477 ) ) ;
#195663 = CARTESIAN_POINT ( 'NONE',  ( -2.954552044183079750E-14, 2.734375000341430884, 1.570758158831788265 ) ) ;
#195664 = DIRECTION ( 'NONE',  ( -0.4100809324301146752, 0.000000000000000000, 0.9120491373041521577 ) ) ;
#195665 = CARTESIAN_POINT ( 'NONE',  ( -6.877010230629689858, 9.046264573866535486, 1.599625672291283607 ) ) ;
#195666 = CARTESIAN_POINT ( 'NONE',  ( 0.02393948931068496516, 6.343121002295580624, 3.090828003060728246 ) ) ;
#195667 = CARTESIAN_POINT ( 'NONE',  ( 7.700104897918568447, 7.948153567185284096, 0.000000000000000000 ) ) ;
#195668 = CARTESIAN_POINT ( 'NONE',  ( 5.656792095876843618, 6.122768675584825182, -0.7810860850652520115 ) ) ;
#195669 = CARTESIAN_POINT ( 'NONE',  ( -7.863365906246048809, 12.11775129068834289, -0.7216878364870267237 ) ) ;
#195670 = CARTESIAN_POINT ( 'NONE',  ( 2.285647630545981190, 0.1040316455800850692, -2.219075330209609120 ) ) ;
#195671 = CARTESIAN_POINT ( 'NONE',  ( -5.608575705693957580, 5.613253794934144558, 0.4301505824422513502 ) ) ;
#195672 = CARTESIAN_POINT ( 'NONE',  ( -6.557303570864871034, 7.679217583210999010, -1.199719254218452047 ) ) ;
#195673 = CARTESIAN_POINT ( 'NONE',  ( 5.124091990960999432, 8.065525525174782828, -1.199719254218452047 ) ) ;
#195674 = CARTESIAN_POINT ( 'NONE',  ( 3.068751266904270025, 1.422870340827029345, -1.350941015047700366 ) ) ;
#195675 = CARTESIAN_POINT ( 'NONE',  ( 4.611744806942754238, 8.532119374741881757, -0.7998128361456231517 ) ) ;
#195676 = CARTESIAN_POINT ( 'NONE',  ( -4.037710856648669022, 7.592775851288043221, -0.3149755216912339395 ) ) ;
#195677 = CARTESIAN_POINT ( 'NONE',  ( 2.835626683552519012, 6.459981564119914310, 0.000000000000000000 ) ) ;
#195678 = CARTESIAN_POINT ( 'NONE',  ( -5.804299160426249493, 5.944306240018289778, -0.7216878364870338292 ) ) ;
#195679 = CARTESIAN_POINT ( 'NONE',  ( -5.585596099150174965, 9.460353182409786399, -0.7216878364870207285 ) ) ;
#195680 = CARTESIAN_POINT ( 'NONE',  ( 2.584367824843319283, 1.138156186954141003, 1.789115803205274080 ) ) ;
#195681 = CARTESIAN_POINT ( 'NONE',  ( -4.664887371553763096, 7.600063145858131364, -1.199719254218453823 ) ) ;
#195682 = CARTESIAN_POINT ( 'NONE',  ( 3.995124980148881288, 1.827535992889782523, -1.154293374375232828 ) ) ;
#195683 = CARTESIAN_POINT ( 'NONE',  ( 3.403688466941825030, -0.7492148395099356151, -1.682118234477212315 ) ) ;
#195684 = CARTESIAN_POINT ( 'NONE',  ( -4.884136011505287200, 6.706951837855620546, 1.250136565965910274 ) ) ;
#195685 = CARTESIAN_POINT ( 'NONE',  ( -1.364683531250000748, 0.5718750003414208027, 0.000000000000000000 ) ) ;
#195686 = CARTESIAN_POINT ( 'NONE',  ( 5.419757389058348807, 1.032087642559690543, -1.401099660988463169 ) ) ;
#195687 = DIRECTION ( 'NONE',  ( 0.000000000000000000, 0.000000000000000000, -1.000000000000000000 ) ) ;
#195688 = CARTESIAN_POINT ( 'NONE',  ( 3.538314903486612817, 7.071858454135611538, 1.040834085586084257E-14 ) ) ;
#195689 = CARTESIAN_POINT ( 'NONE',  ( 10.98549472050129694, 9.842702027212720139, -1.592011381755358723 ) ) ;
#195690 = CARTESIAN_POINT ( 'NONE',  ( 2.659225025413253007, -1.880336703546074073, -1.066323988048665017 ) ) ;
#195691 = AXIS2_PLACEMENT_3D ( 'NONE', #31863, #97939, #81659 ) ;
#195692 = CARTESIAN_POINT ( 'NONE',  ( 4.973982425466109802, 1.752763018817087293, 0.9961474888594208377 ) ) ;
#195693 = CARTESIAN_POINT ( 'NONE',  ( -9.802181872555943087, 10.53822639417784046, 0.7216878364870438212 ) ) ;
#195694 = CARTESIAN_POINT ( 'NONE',  ( 2.606508400632711719, -0.8264410288459265175, -1.997682696722333784 ) ) ;
#195695 = CARTESIAN_POINT ( 'NONE',  ( 3.022686310138736676, 1.855048300136890482, 0.6674203052531629821 ) ) ;
#195696 = CIRCLE ( 'NONE', #140371, 0.5000000000000013323 ) ;
#195697 = CARTESIAN_POINT ( 'NONE',  ( 2.870327622459168726, -1.987497926849005836, -0.3399570244180456502 ) ) ;
#195698 = CARTESIAN_POINT ( 'NONE',  ( -6.589834235204424573, 6.767115956813761102, 0.4477994332492858387 ) ) ;
#195699 = CARTESIAN_POINT ( 'NONE',  ( 5.038593826026604994, -1.663644762202406646, 1.001748047271956876 ) ) ;
#195702 = VERTEX_POINT ( 'NONE', #185477 ) ;
#195701 = DIRECTION ( 'NONE',  ( -1.207943261119674327E-30, -2.168404344971008079E-15, 1.000000000000000000 ) ) ;
#195700 = CARTESIAN_POINT ( 'NONE',  ( -7.795575137733361970, 12.03866206075687018, 0.7216878364870458196 ) ) ;
#195703 = CARTESIAN_POINT ( 'NONE',  ( -7.391130018105325661, 8.652015104991543026, -1.199719254218452047 ) ) ;
#195704 = CARTESIAN_POINT ( 'NONE',  ( 4.760848217054122422, 5.583353003765119560, -1.199719254218452047 ) ) ;
#195706 = ORIENTED_EDGE ( 'NONE', *, *, #115682, .F. ) ;
#195705 = CARTESIAN_POINT ( 'NONE',  ( -4.142898457427624415, 6.991076079377632091, 1.199719254218452935 ) ) ;
#195707 = CARTESIAN_POINT ( 'NONE',  ( -7.659993601596706725, 11.88048360193076647, -0.7216878364870267237 ) ) ;
#195708 = CARTESIAN_POINT ( 'NONE',  ( 1.114635189304619356, -0.9934212416997322270, -1.970578525975318573 ) ) ;
#195709 = CARTESIAN_POINT ( 'NONE',  ( -1.642778471874998480, -1.801041666188708090, 2.845375778867863303 ) ) ;
#195710 = CARTESIAN_POINT ( 'NONE',  ( 5.770351633785986145, -0.8788013674413885923, -1.753946858050984048 ) ) ;
#195711 = CARTESIAN_POINT ( 'NONE',  ( 0.6823417656249917140, 4.905208333674755394, 1.181850606188765695 ) ) ;
#195712 = CARTESIAN_POINT ( 'NONE',  ( -1.500000000000013101, 3.160416667349486008, -0.8660254037844313801 ) ) ;
#195713 = CARTESIAN_POINT ( 'NONE',  ( 5.539635733611046220, 6.394625955944754914, -1.222580188273769908 ) ) ;
#195714 = CARTESIAN_POINT ( 'NONE',  ( 5.519577934094861860, 6.572500690266394940, 1.082531754730549078 ) ) ;
#195715 = CARTESIAN_POINT ( 'NONE',  ( 4.769393013670423009, 1.062472638025207416, 1.503447196605799174 ) ) ;
#195716 = ORIENTED_EDGE ( 'NONE', *, *, #141289, .T. ) ;
#195717 = CARTESIAN_POINT ( 'NONE',  ( -0.6125000000000262457, 2.604166667349451458, 1.060881119635917136 ) ) ;
#195718 = CARTESIAN_POINT ( 'NONE',  ( -6.723954117373590833, 9.932031339322813679, -1.199719254218440723 ) ) ;
#195719 = DIRECTION ( 'NONE',  ( -0.5005768354468334014, 0.8656921114426502362, 1.887379141862767696E-15 ) ) ;
#195720 = CARTESIAN_POINT ( 'NONE',  ( 11.96533679318059917, 11.25246011187004491, 0.9151144679398781623 ) ) ;
#195721 = CARTESIAN_POINT ( 'NONE',  ( 8.917589090474498548, 12.70555303101720135, -7.960785596413196608 ) ) ;
#195722 = CARTESIAN_POINT ( 'NONE',  ( 5.015626762051672571, 7.938982758113895422, 1.199719254218462483 ) ) ;
#195723 = CARTESIAN_POINT ( 'NONE',  ( 6.819606862646741874, -2.000071036334325036, 0.4962039222910428760 ) ) ;
#195726 = CARTESIAN_POINT ( 'NONE',  ( 3.755264181858387840, 1.826884192416846631, -0.2291247506851084581 ) ) ;
#195725 = CARTESIAN_POINT ( 'NONE',  ( 1.574410529035878969, 1.253355123444719998, -1.375888611855519583 ) ) ;
#195724 = CARTESIAN_POINT ( 'NONE',  ( -9.985564813494324454, 4.581166929158016821, 6.661451624069083977 ) ) ;
#195727 = CARTESIAN_POINT ( 'NONE',  ( 7.151035956204054855, 10.43029348462504124, 1.199719254218460707 ) ) ;
#195728 = CARTESIAN_POINT ( 'NONE',  ( 0.4382560683119269829, -5.166862915010145052, 10.99126615174920474 ) ) ;
#195729 = CARTESIAN_POINT ( 'NONE',  ( -7.469616286486262524, 7.679250187180907794, 0.7998128361456341429 ) ) ;
#195730 = DIRECTION ( 'NONE',  ( 0.000000000000000000, -1.000000000000000000, 0.000000000000000000 ) ) ;
#195731 = EDGE_CURVE ( 'NONE', #43808, #134523, #44123, .T. ) ;
#195732 = AXIS2_PLACEMENT_3D ( 'NONE', #143353, #77235, #196335 ) ;
#195733 = CARTESIAN_POINT ( 'NONE',  ( 3.246891520140795517, 0.5363302883765566076, 2.140594385818309409 ) ) ;
#195734 = CARTESIAN_POINT ( 'NONE',  ( 5.501357770389488699, 1.845074063491736860, 1.309031944507930589 ) ) ;
#195735 = CARTESIAN_POINT ( 'NONE',  ( -5.070386261830872598, 8.859275038870594088, 0.7216878364870458196 ) ) ;
#195736 = CARTESIAN_POINT ( 'NONE',  ( 5.783446960131396253, 0.1242560548703756929, -1.807377920737750499 ) ) ;
#195737 = CARTESIAN_POINT ( 'NONE',  ( 5.173012249488437853, 1.686445640873093899, -0.9088423865804375890 ) ) ;
#195738 = CARTESIAN_POINT ( 'NONE',  ( 0.6823417656249899377, 5.488541667008087543, -1.181850606188754593 ) ) ;
#195739 = CARTESIAN_POINT ( 'NONE',  ( 5.875831987524620992, 1.115552982110395330, 1.501486808359139946 ) ) ;
#195740 = CARTESIAN_POINT ( 'NONE',  ( 6.320743865583476229, -1.315316497155760489, 1.316877014833318649 ) ) ;
#195741 = CARTESIAN_POINT ( 'NONE',  ( -0.4019237886466837106, 12.94866454968462754, -1.500000000000000666 ) ) ;
#195742 = CARTESIAN_POINT ( 'NONE',  ( 6.789980064821725669, -0.7525070324889830964, 1.600651327395278711 ) ) ;
#195743 = CARTESIAN_POINT ( 'NONE',  ( 1.780482797753998092, -0.5424726148271253878, -1.942096288550937411 ) ) ;
#195745 = CARTESIAN_POINT ( 'NONE',  ( 2.473383067358714715, 0.1024098097114657241, -2.103702895048992882 ) ) ;
#195744 = CARTESIAN_POINT ( 'NONE',  ( -8.157201976916404362, 12.66848607304450702, -0.7998128361456281477 ) ) ;
#195746 = CARTESIAN_POINT ( 'NONE',  ( 7.099665995050449041, 11.43469409420089455, 0.7998128361456462443 ) ) ;
#195748 = CARTESIAN_POINT ( 'NONE',  ( -8.962103233833181193, 10.41454084668224489, -1.199719254218446718 ) ) ;
#195747 = DIRECTION ( 'NONE',  ( 0.000000000000000000, 1.000000000000000000, 0.000000000000000000 ) ) ;
#195749 = CARTESIAN_POINT ( 'NONE',  ( 0.000000000000000000, 3.900000000000000799, 0.000000000000000000 ) ) ;
#195750 = CARTESIAN_POINT ( 'NONE',  ( 2.918227964375613048, -2.017298000423489501, 0.1032239234411459483 ) ) ;
#195751 = CARTESIAN_POINT ( 'NONE',  ( 0.6823417656249899377, 3.426041667008085323, -1.181850606188754593 ) ) ;
#195752 = CARTESIAN_POINT ( 'NONE',  ( 2.510230996824538430, 6.080353262937265413, 0.000000000000000000 ) ) ;
#195753 = CARTESIAN_POINT ( 'NONE',  ( 3.462350783624254191, 0.9684823049558517472, 1.932541222812742987 ) ) ;
#195754 = CARTESIAN_POINT ( 'NONE',  ( -0.3000000000000172529, 3.975028841772365595, -0.9637995837462973725 ) ) ;
#195755 = CARTESIAN_POINT ( 'NONE',  ( 6.587282531393223728, 8.778525268082516320, 1.599625672291268286 ) ) ;
#195756 = CARTESIAN_POINT ( 'NONE',  ( 9.205623113554615600, 11.76297960394566466, 1.443375672974076540 ) ) ;
#195758 = CARTESIAN_POINT ( 'NONE',  ( -15.75000000000000000, 12.69999999999999929, -1.400000000000001910 ) ) ;
#195757 = CARTESIAN_POINT ( 'NONE',  ( 1.364001086256797945, -0.5279541034660294452, 2.105878793243611824 ) ) ;
#195759 = CARTESIAN_POINT ( 'NONE',  ( -5.721177635286839092, 9.618531641235897212, 0.7216878364870458196 ) ) ;
#195760 = CARTESIAN_POINT ( 'NONE',  ( -0.6823417656250212460, 1.051041667008083325, 1.181850606188755259 ) ) ;
#195761 = CARTESIAN_POINT ( 'NONE',  ( 2.103317784989285677, -0.4765762082987561321, 2.138964651187735821 ) ) ;
#195762 = CARTESIAN_POINT ( 'NONE',  ( 0.4957404558455620891, 7.798922855753830596, 1.990826765680269395 ) ) ;
#195763 = CARTESIAN_POINT ( 'NONE',  ( 2.466018556964240549, 2.218949015226141963, -0.4410763869808070337 ) ) ;
#195764 = CARTESIAN_POINT ( 'NONE',  ( -7.212047647465563038, 10.50147379109678880, -1.199719254218446718 ) ) ;
#195765 = CARTESIAN_POINT ( 'NONE',  ( -3.999292125906916073, 5.688926785023260102, 1.443375672974064550 ) ) ;
#195766 = CARTESIAN_POINT ( 'NONE',  ( 1.364683531249988535, 2.967708333674755394, -0.7879004041258239610 ) ) ;
#195767 = CARTESIAN_POINT ( 'NONE',  ( 5.148720134264945791, 7.772403765597828418, 1.171659602702241676 ) ) ;
#195768 = CARTESIAN_POINT ( 'NONE',  ( 1.499999999999997113, 11.14583333333333215, -0.8660254037844378194 ) ) ;
#195769 = CARTESIAN_POINT ( 'NONE',  ( 6.427974226654860956, 7.632296364919712417, -1.082531754730548412 ) ) ;
#195770 = CARTESIAN_POINT ( 'NONE',  ( 3.708038350156193541, -0.7148330724025107052, -1.619118029916452262 ) ) ;
#195771 = CARTESIAN_POINT ( 'NONE',  ( 9.154780037725547714, 11.70366268214508487, 1.599625672291279388 ) ) ;
#195772 = CARTESIAN_POINT ( 'NONE',  ( 5.913141818906856528, 1.943543578741913969, 1.045239939247793792 ) ) ;
#195773 = CARTESIAN_POINT ( 'NONE',  ( -1.364683531250000748, 9.609375000341396245, 0.000000000000000000 ) ) ;
#195774 = CARTESIAN_POINT ( 'NONE',  ( -4.610654757099099221, 7.536791762327691657, 1.199719254218452935 ) ) ;
#195775 = CARTESIAN_POINT ( 'NONE',  ( 5.501577430365036214, -1.966641501487207622, 0.4445218866586594930 ) ) ;
#195776 = EDGE_LOOP ( 'NONE', ( #154053, #175544, #165847, #33717 ) ) ;
#195777 = ADVANCED_FACE ( 'NONE', ( #32845 ), #12598, .T. ) ;
#195778 = CARTESIAN_POINT ( 'NONE',  ( 4.170664822833985319, -1.745344833062393075, -0.6735866001992969476 ) ) ;
#195779 = EDGE_CURVE ( 'NONE', #138623, #95365, #75542, .T. ) ;
#195780 = CARTESIAN_POINT ( 'NONE',  ( 3.116144222688784549, 2.060704436481402890, -0.1983081510379124945 ) ) ;
#195781 = CARTESIAN_POINT ( 'NONE',  ( -6.821160681006823268, 9.051383109298335228, 1.443375672974064550 ) ) ;
#195782 = CARTESIAN_POINT ( 'NONE',  ( -0.5149768381150839902, 3.543642475881736864, -0.4000488691750889725 ) ) ;
#195783 = CARTESIAN_POINT ( 'NONE',  ( -7.334597915313094241, 9.580116872663850813, 1.040834085586084257E-14 ) ) ;
#195784 = CARTESIAN_POINT ( 'NONE',  ( 9.367496997597598352, 3.481540744127370690, 7.500000000000000000 ) ) ;
#195785 = CARTESIAN_POINT ( 'NONE',  ( 1.364683531249988535, 3.717708333674750953, -0.7879004041258239610 ) ) ;
#195786 = CARTESIAN_POINT ( 'NONE',  ( 1.177825114000274898, 1.883588471398514264, -0.3297955356276888184 ) ) ;
#195787 = CARTESIAN_POINT ( 'NONE',  ( 2.594135478747404022, 0.9273930874063830432, -1.728848471177657942 ) ) ;
#195788 = CARTESIAN_POINT ( 'NONE',  ( 1.388045824401448414, -0.05229234656609069859, 2.015604296821980057 ) ) ;
#195789 = EDGE_CURVE ( 'NONE', #108115, #12260, #161369, .T. ) ;
#195790 = CARTESIAN_POINT ( 'NONE',  ( -4.930325137224961907, 5.781076077297750970, -1.199719254218453823 ) ) ;
#195792 =( NAMED_UNIT ( * ) SI_UNIT ( $, .STERADIAN. ) SOLID_ANGLE_UNIT ( ) );
#195791 = CARTESIAN_POINT ( 'NONE',  ( 7.259501185113382604, 10.55683625168592243, -1.199719254218441611 ) ) ;
#195793 = CARTESIAN_POINT ( 'NONE',  ( 6.538353035222548293, 1.949559774641503651, 0.2916953021188176121 ) ) ;
#195794 = CARTESIAN_POINT ( 'NONE',  ( -0.6823417656249969321, 4.467708333674755394, -1.181850606188749264 ) ) ;
#195795 = CARTESIAN_POINT ( 'NONE',  ( 1.388932857043408742, -1.913036705441802265, -0.6274143624813811604 ) ) ;
#195796 = AXIS2_PLACEMENT_3D ( 'NONE', #64452, #196586, #96981 ) ;
#195798 = CARTESIAN_POINT ( 'NONE',  ( 2.126704408204147967, 0.4671447874508818932, 2.064898165909804906 ) ) ;
#195797 = CARTESIAN_POINT ( 'NONE',  ( -6.060131475628484310, 10.01397778830115470, 0.000000000000000000 ) ) ;
#195799 = CARTESIAN_POINT ( 'NONE',  ( 9.450148846975686467, 11.05536808409302907, -7.324943998173960580 ) ) ;
#195800 = CARTESIAN_POINT ( 'NONE',  ( 3.807136610393092813, -1.694265131726957252, 1.189645435975445809 ) ) ;
#195801 = CARTESIAN_POINT ( 'NONE',  ( 5.585032934186686226, 5.480569609498057382, 0.000000000000000000 ) ) ;
#195803 = CARTESIAN_POINT ( 'NONE',  ( 2.205172540517054802, 5.724451730578533848, 1.040834085586084257E-14 ) ) ;
#195802 = CARTESIAN_POINT ( 'NONE',  ( 5.789036971029382528, 1.582348866732422810, 1.366464223246833809 ) ) ;
#195805 = VERTEX_POINT ( 'NONE', #183354 ) ;
#195804 = CARTESIAN_POINT ( 'NONE',  ( 3.979382468966369935, 1.719079831940514502, -0.6148086763930470378 ) ) ;
#195806 = CARTESIAN_POINT ( 'NONE',  ( 8.920375002787457319, 12.49452237230570084, 1.199719254218450271 ) ) ;
#195807 = FILL_AREA_STYLE_COLOUR ( '', #92315 ) ;
#195808 = CARTESIAN_POINT ( 'NONE',  ( 10.16623870845280742, 13.45394180708211351, -7.231736421947215554 ) ) ;
#195809 = CARTESIAN_POINT ( 'NONE',  ( 6.229534195615700654, -2.079954537573494466, 0.7377168454194837910 ) ) ;
#195810 = CARTESIAN_POINT ( 'NONE',  ( 1.364683531250000748, 10.31770833367472839, -0.7879004041258355073 ) ) ;
#195811 = ORIENTED_EDGE ( 'NONE', *, *, #162651, .T. ) ;
#195812 = CARTESIAN_POINT ( 'NONE',  ( 4.828717125059535320, 1.315996081294769304, -1.387672938220223307 ) ) ;
#195813 = CARTESIAN_POINT ( 'NONE',  ( -9.110189153378817295, 12.71597221466224603, 1.199719254218462483 ) ) ;
#195814 = CARTESIAN_POINT ( 'NONE',  ( 6.448874621594486989, 10.67543749183559143, 0.7998128361456462443 ) ) ;
#195815 = CARTESIAN_POINT ( 'NONE',  ( -0.6801582343750022241, 1.130208333674734167, -1.178068619123841643 ) ) ;
#195816 = CARTESIAN_POINT ( 'NONE',  ( -6.328041841479842056, 6.870487382198048998, 0.6860574420480938240 ) ) ;
#195817 = CARTESIAN_POINT ( 'NONE',  ( 0.3273695209934923689, 0.9472894719858866441, -1.578709817245539604 ) ) ;
#195818 = VERTEX_POINT ( 'NONE', #86928 ) ;
#195819 = CARTESIAN_POINT ( 'NONE',  ( -5.887983850084758330, 10.09134126839936840, 0.7998128361456291469 ) ) ;
#195820 = CARTESIAN_POINT ( 'NONE',  ( 4.288257209584379837, -1.849852534125648207, -0.2767368629695772797 ) ) ;
#195821 = DIRECTION ( 'NONE',  ( 1.224646799147343346E-16, 0.000000000000000000, -1.000000000000000000 ) ) ;
#195822 = CARTESIAN_POINT ( 'NONE',  ( 5.169401708560450004, 9.252995436621013425, 0.000000000000000000 ) ) ;
#195823 = MECHANICAL_DESIGN_GEOMETRIC_PRESENTATION_REPRESENTATION (  '', ( #9054 ), #119825 ) ;
#195824 = CARTESIAN_POINT ( 'NONE',  ( 9.508009452425755015, 4.000007913748543587, -7.612499999891275237 ) ) ;
#195825 = CARTESIAN_POINT ( 'NONE',  ( -5.214720930002679999, 7.727253977155453590, 1.197825571464938399 ) ) ;
#195826 = CARTESIAN_POINT ( 'NONE',  ( -6.317736394288148816, 8.393778431468064127, 1.443375672974078761 ) ) ;
#195827 = AXIS2_PLACEMENT_3D ( 'NONE', #100256, #117643, #184689 ) ;
#195828 = CARTESIAN_POINT ( 'NONE',  ( 3.521367211247359741, 5.131347717920458962, -1.599625672291262513 ) ) ;
#195829 = CARTESIAN_POINT ( 'NONE',  ( 1.709744157921966101, 0.5768405975999196800, -1.883039948965541610 ) ) ;
#195830 = CARTESIAN_POINT ( 'NONE',  ( 2.425407844734633223, -1.496065234337567329, -1.352141214786584777 ) ) ;
#195831 = CARTESIAN_POINT ( 'NONE',  ( -8.779068160048691283, 10.20099992726700933, -1.199719254218446718 ) ) ;
#195832 = CARTESIAN_POINT ( 'NONE',  ( 5.987861119090863049, 7.014868056141362551, 1.199719254218452047 ) ) ;
#195833 = CARTESIAN_POINT ( 'NONE',  ( -11.92045683181315674, 11.15275927879484641, -1.382340670101859237 ) ) ;
#195834 = CARTESIAN_POINT ( 'NONE',  ( 2.959115643078192637, 0.3208686883675835877, -2.167707805308824121 ) ) ;
#195835 = CARTESIAN_POINT ( 'NONE',  ( 2.325000000000005063, 0.000000000000000000, -0.5000000000000004441 ) ) ;
#195836 = CARTESIAN_POINT ( 'NONE',  ( -8.622095623286845978, 12.14652976288826913, 1.199719254218462483 ) ) ;
#195837 = CARTESIAN_POINT ( 'NONE',  ( 6.825078400183548055, 2.447738240532343124, 2.338733633852312366 ) ) ;
#195838 = CYLINDRICAL_SURFACE ( 'NONE', #153956, 1.000000000000000000 ) ;
#195839 = CARTESIAN_POINT ( 'NONE',  ( -9.409940793360268785, 3.999985931113709814, -6.919963696468023784 ) ) ;
#195841 = EDGE_CURVE ( 'NONE', #71069, #108467, #140525, .T. ) ;
#195840 = CARTESIAN_POINT ( 'NONE',  ( 7.574201371528760163, 11.98831870009225931, 1.040834085586084257E-14 ) ) ;
#195842 = CARTESIAN_POINT ( 'NONE',  ( -4.715876479964030032, 8.338641909828480081, -0.7613925308670350667 ) ) ;
#195843 = CARTESIAN_POINT ( 'NONE',  ( 5.072158865288222351, 8.931619419562697004, 0.7216878364870317197 ) ) ;
#195844 = VERTEX_POINT ( 'NONE', #199589 ) ;
#195846 = CARTESIAN_POINT ( 'NONE',  ( 1.647136526480545982, 0.1996500767776411833, 2.003181903140099696 ) ) ;
#195845 = CARTESIAN_POINT ( 'NONE',  ( 5.390138975101268493, -0.4531076923771395482, -1.784498753146485539 ) ) ;
#195847 = CARTESIAN_POINT ( 'NONE',  ( 2.636409100479879086, 0.1147267580069409321, -2.295643959171574711 ) ) ;
#195849 = CARTESIAN_POINT ( 'NONE',  ( 1.850234720775156605, -1.851392121210411634, -0.1886080954226591611 ) ) ;
#195848 = CARTESIAN_POINT ( 'NONE',  ( -1.500000000000015099, 9.979166666666671404, -0.8660254037844309360 ) ) ;
#195851 = CARTESIAN_POINT ( 'NONE',  ( -3.285556943750000514, -2.938541666188710266, -1.896917185911906500 ) ) ;
#195850 = APPLICATION_CONTEXT ( 'automotive_design' ) ;
#195852 = CARTESIAN_POINT ( 'NONE',  ( -9.404204974767472081, 15.50982908332066401, -7.453969465644266990 ) ) ;
#195853 = CARTESIAN_POINT ( 'NONE',  ( 5.238497809344139000, 1.134185964801931679, -1.539638564045166857 ) ) ;
#195854 = CARTESIAN_POINT ( 'NONE',  ( -8.239604668803112375, 10.63595808506888396, -1.599625672291263179 ) ) ;
#195855 = CARTESIAN_POINT ( 'NONE',  ( -6.455090533882213322, 6.703562842383589349, -0.7216878364870338292 ) ) ;
#195857 = CARTESIAN_POINT ( 'NONE',  ( 3.432352559540859271, 1.824792983844251371, 0.4109263881779609551 ) ) ;
#195856 = CARTESIAN_POINT ( 'NONE',  ( 4.880461040030859010, -0.2572269614671355842, -2.074807210009928848 ) ) ;
#195858 = CARTESIAN_POINT ( 'NONE',  ( 7.944714827928056167, 8.371181508778631652, 0.7216878364870458196 ) ) ;
#195859 = CARTESIAN_POINT ( 'NONE',  ( 6.286648950733226826, 1.598451336667701339, -0.9137711784916457969 ) ) ;
#195860 = CARTESIAN_POINT ( 'NONE',  ( 2.523789150438203510, 6.096171108819874007, 0.7998128361456462443 ) ) ;
#195861 = CYLINDRICAL_SURFACE ( 'NONE', #210483, 0.7499999999999997780 ) ;
#195862 = CARTESIAN_POINT ( 'NONE',  ( 4.863727610707407223, 1.705404662657764137, -0.2575704655415639310 ) ) ;
#195863 = CARTESIAN_POINT ( 'NONE',  ( -6.898401231254901234, 6.942556279419168419, -0.7998128361456291469 ) ) ;
#195864 =( NAMED_UNIT ( * ) PLANE_ANGLE_UNIT ( ) SI_UNIT ( $, .RADIAN. ) );
#195865 = CARTESIAN_POINT ( 'NONE',  ( 0.000000000000000000, 0.000000000000000000, 6.123233995736775897E-17 ) ) ;
#195866 = AXIS2_PLACEMENT_3D ( 'NONE', #167830, #163582, #53007 ) ;
#195867 = CARTESIAN_POINT ( 'NONE',  ( 1.526556658859585313E-16, 0.000000000000000000, -2.750000000000000000 ) ) ;
#195868 = CARTESIAN_POINT ( 'NONE',  ( 4.346645206408905615, -2.146589105242337592, -0.3245344146646060302 ) ) ;
#195869 = CARTESIAN_POINT ( 'NONE',  ( 3.668406916800326822, -1.225078373119499187, 1.353803248016255178 ) ) ;
#195870 = CARTESIAN_POINT ( 'NONE',  ( 1.235121763443976173, -0.04261391538399812023, -1.961451400788959631 ) ) ;
#195871 = CARTESIAN_POINT ( 'NONE',  ( 6.175037754964278314, 1.841102675566621771, -1.045632355512320144 ) ) ;
#195873 = CARTESIAN_POINT ( 'NONE',  ( 1.364683531249990311, 4.196875000341417028, 1.214306433183764966E-14 ) ) ;
#195872 = CARTESIAN_POINT ( 'NONE',  ( 5.495737418514557326, -2.292545469083116849, -0.002927036808696506075 ) ) ;
#195874 = CARTESIAN_POINT ( 'NONE',  ( 10.85353573482951717, -6.836568542495036205, -0.4635785636673637189 ) ) ;
#195875 = CARTESIAN_POINT ( 'NONE',  ( 9.426996880203592610, 9.892584536526015881, -0.7998128361456281477 ) ) ;
#195876 = PRESENTATION_LAYER_ASSIGNMENT (  '', '', ( #188910 ) ) ;
#195877 = CARTESIAN_POINT ( 'NONE',  ( 2.139458383197485603, 0.002846582261652879763, 2.120667954922689002 ) ) ;
#195878 = CARTESIAN_POINT ( 'NONE',  ( -3.118012141462980669, 6.581505231774690046, 0.7216878364870317197 ) ) ;
#195879 = DIRECTION ( 'NONE',  ( 1.000000000000000000, -7.771561172376097755E-16, -4.440892098500627148E-16 ) ) ;
#195880 = CARTESIAN_POINT ( 'NONE',  ( -5.382223794500845315, 6.341977850748185652, -1.082531754730543971 ) ) ;
#195881 = CARTESIAN_POINT ( 'NONE',  ( 6.737192315218426764, -0.09781360997717462868, -2.168977284074862677 ) ) ;
#195883 = CARTESIAN_POINT ( 'NONE',  ( -1.500000000000001110, 13.55208333401613174, 0.8660254037844419273 ) ) ;
#195882 = CARTESIAN_POINT ( 'NONE',  ( 6.883263157960366030, 0.5727201817382967519, 2.105997115537924902 ) ) ;
#195885 = EDGE_LOOP ( 'NONE', ( #73873, #54084, #145461, #24461 ) ) ;
#195884 = CARTESIAN_POINT ( 'NONE',  ( 1.946216630774719736, -1.453687271215977850, -1.679643103671465632 ) ) ;
#195886 = CARTESIAN_POINT ( 'NONE',  ( 0.1417928296247125686, 0.8878553654741733192, 2.120496703859587662 ) ) ;
#195888 = CARTESIAN_POINT ( 'NONE',  ( 5.647355161340581020, 1.821535332892617820, -0.9675206831420575249 ) ) ;
#195887 = CARTESIAN_POINT ( 'NONE',  ( 9.029367117021314115, 12.51771682229149008, -1.082531754730543083 ) ) ;
#195890 = CARTESIAN_POINT ( 'NONE',  ( -3.475000000000000533, -2.100000000000000977, 0.000000000000000000 ) ) ;
#195889 = CARTESIAN_POINT ( 'NONE',  ( 5.879395890181562834, 6.888325289080478697, -1.199719254218452047 ) ) ;
#195891 = CARTESIAN_POINT ( 'NONE',  ( 5.682802662783380754, 6.658966523782627434, 1.199719254218452935 ) ) ;
#195893 = EDGE_CURVE ( 'NONE', #209617, #140333, #85860, .T. ) ;
#195892 = CARTESIAN_POINT ( 'NONE',  ( 0.000000000000000000, -0.1968749995220437643, -3.793834371823813001 ) ) ;
#195894 = CARTESIAN_POINT ( 'NONE',  ( 0.1331565106231363538, 7.629137130509071163, -2.545925718843544239 ) ) ;
#195895 = CARTESIAN_POINT ( 'NONE',  ( 5.776868925826902590, 1.698781319366513998, -0.7106697882480541573 ) ) ;
#195896 = CIRCLE ( 'NONE', #9115, 0.04999999999999930889 ) ;
#195898 = ORIENTED_EDGE ( 'NONE', *, *, #99066, .F. ) ;
#195897 = CARTESIAN_POINT ( 'NONE',  ( 5.030238685870051185, 5.827365540725222282, -1.199719254218452047 ) ) ;
#195899 = FILL_AREA_STYLE_COLOUR ( '', #3115 ) ;
#195900 = CARTESIAN_POINT ( 'NONE',  ( 1.764246635482754622, -1.222956780391671439, 1.216502489609740723 ) ) ;
#195901 = CARTESIAN_POINT ( 'NONE',  ( 1.587125413319636857, 1.679225032509903626, 1.116207499648947943 ) ) ;
#195902 = CARTESIAN_POINT ( 'NONE',  ( 2.092814488687055441, -0.4990534829178472354, 2.243750245495256035 ) ) ;
#195903 = CARTESIAN_POINT ( 'NONE',  ( -0.6823417656250212460, 3.613541667008085767, 1.181850606188767472 ) ) ;
#195904 = CARTESIAN_POINT ( 'NONE',  ( 2.724197551734920175, -1.300482880258296836, -1.851114353284079472 ) ) ;
#195905 = CARTESIAN_POINT ( 'NONE',  ( 4.178421505988277218, -1.212938584752444093, 1.721516029631239064 ) ) ;
#195906 = CARTESIAN_POINT ( 'NONE',  ( -2.959422669532919326, 6.674686557755516780, 0.7998128361456352531 ) ) ;
#195907 = CARTESIAN_POINT ( 'NONE',  ( 2.213771126746429729, -0.8293587345859743110, -1.563345763006577238 ) ) ;
#195909 = ADVANCED_FACE ( 'NONE', ( #151934 ), #125797, .T. ) ;
#195908 = CARTESIAN_POINT ( 'NONE',  ( 7.149227073107712549, 7.235186428247455837, -0.7998128361456281477 ) ) ;
#195910 = CARTESIAN_POINT ( 'NONE',  ( 4.868786560638889149, 6.773613302202437403, 1.443375672974065660 ) ) ;
#195911 = CARTESIAN_POINT ( 'NONE',  ( -5.298539104842322267, 5.076050465271134016, 0.7998128361456341429 ) ) ;
#195912 = CARTESIAN_POINT ( 'NONE',  ( 5.300874872818828187, 8.167809204055208383, 1.082531754730558626 ) ) ;
#195913 = CARTESIAN_POINT ( 'NONE',  ( 1.499999999999989120, 2.504166666666687302, 0.8660254037844524744 ) ) ;
#195914 = CARTESIAN_POINT ( 'NONE',  ( 6.533471383080789785, -0.1550430487086348341, 2.186663148620856756 ) ) ;
#195915 = CARTESIAN_POINT ( 'NONE',  ( 2.976726284633357533, -0.1618151936485581754, -2.185533650236513914 ) ) ;
#195916 = CARTESIAN_POINT ( 'NONE',  ( -3.113568832632681360, 6.784247404713427798, -0.7998128361456281477 ) ) ;
#195917 = DIRECTION ( 'NONE',  ( 0.000000000000000000, 0.000000000000000000, -1.000000000000000000 ) ) ;
#195918 = CARTESIAN_POINT ( 'NONE',  ( 6.533838320793388554, -2.056994387304663885, 0.5145578593022879232 ) ) ;
#195919 = B_SPLINE_CURVE_WITH_KNOTS ( 'NONE', 3,
 ( #214390, #49807, #163575, #149442, #99626, #130080, #148389, #112752, #197119, #15158 ),
 .UNSPECIFIED., .F., .F.,
 ( 4, 2, 2, 2, 4 ),
 ( 2.539054641909564890E-15, 0.0005184205841295809816, 0.001036841168256622762, 0.001555261752383664759, 0.002073682336510707189 ),
 .UNSPECIFIED. ) ;
#195920 = CARTESIAN_POINT ( 'NONE',  ( -1.201851678989727383E-14, 2.821875000341418804, 1.575800808251672791 ) ) ;
#195921 = CARTESIAN_POINT ( 'NONE',  ( 0.6823417656249934904, 8.442708333674733723, 1.181850606188764807 ) ) ;
#195922 = CARTESIAN_POINT ( 'NONE',  ( -4.446711195602255806, 5.250546485366484717, -1.082531754730544860 ) ) ;
#195923 = CARTESIAN_POINT ( 'NONE',  ( 5.519825572852568030, -0.5132647233585425628, 2.057443900658859182 ) ) ;
#195924 = CARTESIAN_POINT ( 'NONE',  ( -5.641601317062239218, 8.635599732330991429, -1.082531754730549967 ) ) ;
#195925 = ORIENTED_EDGE ( 'NONE', *, *, #145289, .F. ) ;
#195926 = CARTESIAN_POINT ( 'NONE',  ( -6.129694847154231852, 6.323934541200937787, -0.7216878364870338292 ) ) ;
#195927 = CARTESIAN_POINT ( 'NONE',  ( 4.761938266897790761, 6.578680616179308771, 1.599625672291267398 ) ) ;
#195928 = CARTESIAN_POINT ( 'NONE',  ( 6.374545129912786656, -0.09763137639631429276, -1.838803627010993091 ) ) ;
#195929 = CARTESIAN_POINT ( 'NONE',  ( 0.3976372456648717968, 6.957695340450004373, -3.811578153443453854 ) ) ;
#195930 = CARTESIAN_POINT ( 'NONE',  ( 1.364683531249990311, 4.676041667008083103, 0.7879004041258500513 ) ) ;
#195931 = CARTESIAN_POINT ( 'NONE',  ( 2.471852389601780331, -1.665955342129191274, -0.5037381675307306406 ) ) ;
#195932 = DIRECTION ( 'NONE',  ( 0.000000000000000000, 0.000000000000000000, -1.000000000000000000 ) ) ;
#195933 = CARTESIAN_POINT ( 'NONE',  ( 0.7308173252688826560, -1.846041318942293286, -0.6644482084196751126 ) ) ;
#195934 = CARTESIAN_POINT ( 'NONE',  ( 1.364683531249988757, -0.05312499965857975237, 0.000000000000000000 ) ) ;
#195935 = CARTESIAN_POINT ( 'NONE',  ( 7.204675194429079505E-15, -1.793749999044084831, -3.475000000000000089 ) ) ;
#195936 = EDGE_CURVE ( 'NONE', #185401, #110521, #214208, .T. ) ;
#195937 = CARTESIAN_POINT ( 'NONE',  ( 6.157120911006636277, -1.851533521339579380, -1.115484332758958974 ) ) ;
#195938 = CARTESIAN_POINT ( 'NONE',  ( -10.45741655484220267, 11.09474082360439873, -0.7998128361456221525 ) ) ;
#195939 = ADVANCED_FACE ( 'NONE', ( #162086 ), #15976, .T. ) ;
#195940 = CARTESIAN_POINT ( 'NONE',  ( -6.575341312503472757, 7.733948288417905381, 1.082531754730549967 ) ) ;
#195941 = CARTESIAN_POINT ( 'NONE',  ( 5.664953204072169513, -1.952404353424816774, -0.9282482345986733385 ) ) ;
#195943 = EDGE_LOOP ( 'NONE', ( #209105, #63165, #39944, #37059 ) ) ;
#195942 = CARTESIAN_POINT ( 'NONE',  ( 0.000000000000000000, 0.000000000000000000, 0.000000000000000000 ) ) ;
#195944 = CARTESIAN_POINT ( 'NONE',  ( -1.364683531250012516, 4.238541667008090208, -0.7879004041258300672 ) ) ;
#195945 = CARTESIAN_POINT ( 'NONE',  ( 5.747334165637288272, -1.552519754122901663, -1.214743736649764649 ) ) ;
#195946 = CARTESIAN_POINT ( 'NONE',  ( 5.237493459246572947, -1.633055164623600897, -0.5828427842848020735 ) ) ;
#195948 = CARTESIAN_POINT ( 'NONE',  ( 1.452940684028160234, -1.882004992133184285, -1.122693704575933316 ) ) ;
#195947 = CARTESIAN_POINT ( 'NONE',  ( -1.360316468750006225, -0.3593749996585737794, -1.734723475976807094E-15 ) ) ;
#195949 = CARTESIAN_POINT ( 'NONE',  ( 3.206425952641503319, -2.304998342715250281, 0.1115464655990650450 ) ) ;
#195950 = CARTESIAN_POINT ( 'NONE',  ( 5.518845395222173877, 1.902436629287082237, 0.7926794616768815249 ) ) ;
#195951 = CARTESIAN_POINT ( 'NONE',  ( 1.359210844938564033, 1.913264527786652902, -0.3316978906799557536 ) ) ;
#195952 = CARTESIAN_POINT ( 'NONE',  ( -5.219525951136837705, 9.033271343060892633, -0.7216878364870207285 ) ) ;
#195953 = PRODUCT_DEFINITION_SHAPE ( 'NONE', 'NONE',  #214411 ) ;
#195954 = CARTESIAN_POINT ( 'NONE',  ( -5.113360211009450040, 5.994616996712990975, -1.199719254218453823 ) ) ;
#195955 = CARTESIAN_POINT ( 'NONE',  ( -1.499999999999997780, 10.00000000000000178, -4.154462424328202452 ) ) ;
#195956 = CARTESIAN_POINT ( 'NONE',  ( 3.726904977748810133, 1.497142547446396410, -1.502090761940577002 ) ) ;
#195957 = FACE_OUTER_BOUND ( 'NONE', #7860, .T. ) ;
#195958 = CARTESIAN_POINT ( 'NONE',  ( 2.725232599228684993, 2.001511357256777313, 0.2440295182731533341 ) ) ;
#195959 = CARTESIAN_POINT ( 'NONE',  ( -5.029711800545518585, 8.811821500704338561, 0.7216878364870458196 ) ) ;
#195960 = CARTESIAN_POINT ( 'NONE',  ( 4.454274341225270994, 2.206355006892012138, -0.05062909709598743119 ) ) ;
#195961 = CARTESIAN_POINT ( 'NONE',  ( -3.285556943750000514, -0.5760416661887087786, -1.896917185911906500 ) ) ;
#195962 = CYLINDRICAL_SURFACE ( 'NONE', #82628, 1.224999999999996980 ) ;
#195963 = DIRECTION ( 'NONE',  ( 1.000000000000000000, -0.000000000000000000, 1.224646799147353207E-16 ) ) ;
#195964 = CARTESIAN_POINT ( 'NONE',  ( -7.422162748838431412, 7.623887726591770608, -0.7998128361456362523 ) ) ;
#195967 = CIRCLE ( 'NONE', #119946, 6.399999999999999467 ) ;
#195966 = CARTESIAN_POINT ( 'NONE',  ( -0.02900071798685524560, -0.004641455105012376459, -2.173770343569726649 ) ) ;
#195965 = CARTESIAN_POINT ( 'NONE',  ( -4.589286827423546100, 8.493149336607261901, 0.1385767598228414277 ) ) ;
#195968 = CARTESIAN_POINT ( 'NONE',  ( -7.065207446497166366, 9.336104335703744539, 0.000000000000000000 ) ) ;
#195969 = EDGE_LOOP ( 'NONE', ( #195006, #22289, #167828, #12059 ) ) ;
#195970 = CARTESIAN_POINT ( 'NONE',  ( 4.364173291480280881, 0.9696465702416400267, 1.818514982836361593 ) ) ;
#195971 = CARTESIAN_POINT ( 'NONE',  ( -8.068510813464099485, 8.585886501895810596, 0.7216878364870317197 ) ) ;
#195972 = UNCERTAINTY_MEASURE_WITH_UNIT (LENGTH_MEASURE( 1.000000000000000082E-05 ), #189438, 'distance_accuracy_value', 'NONE');
#195973 = DIRECTION ( 'NONE',  ( -0.6483454320283800199, 0.000000000000000000, 0.7613463080411787542 ) ) ;
#195974 = CARTESIAN_POINT ( 'NONE',  ( -5.311043488251275591, 7.219303374425030562, -1.599625672291256295 ) ) ;
#195975 = CARTESIAN_POINT ( 'NONE',  ( -5.815521545619021460, 5.749472989502435460, -0.7998128361456362523 ) ) ;
#195976 = CARTESIAN_POINT ( 'NONE',  ( 3.369790118769320664, 0.4886731666619185677, -1.959541563195909220 ) ) ;
#195977 = CARTESIAN_POINT ( 'NONE',  ( -0.7500000000000215383, 1.191666666666688190, 1.299038105676659116 ) ) ;
#195978 = CARTESIAN_POINT ( 'NONE',  ( 8.432808358020004391, 12.78210081775797669, 0.7216878364870438212 ) ) ;
#195979 = CARTESIAN_POINT ( 'NONE',  ( 6.012151052656117933, 9.101594430485762999, 1.199719254218460707 ) ) ;
#195980 = CARTESIAN_POINT ( 'NONE',  ( 3.309499033229778231, -0.4035708669713148899, 2.020805850887919863 ) ) ;
#195981 =( BOUNDED_CURVE ( )  B_SPLINE_CURVE ( 2, ( #151610, #124518, #60481, #176384, #91954 ),
 .UNSPECIFIED., .F., .T. ) 
 B_SPLINE_CURVE_WITH_KNOTS ( ( 3, 2, 3 ),
 ( 0.1361778335736238410, 0.1375000000000000111, 0.1392051351651994728 ),
 .UNSPECIFIED. ) 
 CURVE ( )  GEOMETRIC_REPRESENTATION_ITEM ( )  RATIONAL_B_SPLINE_CURVE ( ( 0.9419547032718713631, 0.9574871888551554910, 1.000000000000000000, 0.9451732491398672220, 0.9352202683046508813 ) ) 
 REPRESENTATION_ITEM ( '' )  );
#195982 = DIRECTION ( 'NONE',  ( 0.000000000000000000, 1.000000000000000000, 0.000000000000000000 ) ) ;
#195983 = CARTESIAN_POINT ( 'NONE',  ( 3.994848817520957773, 7.812407387083109001, 1.040834085586084257E-14 ) ) ;
#195985 = ORIENTED_EDGE ( 'NONE', *, *, #43825, .T. ) ;
#195984 = CARTESIAN_POINT ( 'NONE',  ( -0.1408020194049965368, 5.721120576699901150, -2.694324532632543345 ) ) ;
#195986 = CARTESIAN_POINT ( 'NONE',  ( 1.323879276782027548, 1.773944146221797524, 0.4926282247687193139 ) ) ;
#195987 = CARTESIAN_POINT ( 'NONE',  ( -0.02224634325198419221, -0.007204097619508199532, -2.289079630542793620 ) ) ;
#195988 = CARTESIAN_POINT ( 'NONE',  ( 4.389807875774629942, 8.343469298370917997, 0.7998128361456271485 ) ) ;
#195989 = CARTESIAN_POINT ( 'NONE',  ( 2.530746307392011563, 2.096003997654236173, 0.5278882200696957128 ) ) ;
#195990 = CARTESIAN_POINT ( 'NONE',  ( -3.633221978782290140, 6.222214161012547429, -1.082531754730549967 ) ) ;
#195991 = CARTESIAN_POINT ( 'NONE',  ( 1.604704241733472037, 1.883313803065278513, 0.7212895827233902768 ) ) ;
#195992 = CARTESIAN_POINT ( 'NONE',  ( 2.724286267170890952, -1.998689782195923081, -1.134749220811093418 ) ) ;
#195993 = CARTESIAN_POINT ( 'NONE',  ( 6.717278222822382183, -7.246166700180828535, -6.830415307812249814 ) ) ;
#195994 = CARTESIAN_POINT ( 'NONE',  ( 0.4615142869485132637, 1.850934062480696252, -0.2700578556205368574 ) ) ;
#195995 = CARTESIAN_POINT ( 'NONE',  ( 4.153168997088651615, -1.638446398916657776, -1.096151307749502868 ) ) ;
#195996 = PRESENTATION_LAYER_ASSIGNMENT (  '', '', ( #178682 ) ) ;
#195997 = CARTESIAN_POINT ( 'NONE',  ( 4.469935555517978720, -0.9463019959239076240, 1.780667052345537238 ) ) ;
#195999 = CARTESIAN_POINT ( 'NONE',  ( 9.585251414737269826, 11.24551007435741568, -1.082531754730537088 ) ) ;
#195998 = CARTESIAN_POINT ( 'NONE',  ( -1.201851678989727383E-14, 3.696875000341422801, -1.575800808251660134 ) ) ;
#196001 = CARTESIAN_POINT ( 'NONE',  ( 5.988920713192999123, -0.3073026951427524356, -2.083404400164515113 ) ) ;
#196000 = CARTESIAN_POINT ( 'NONE',  ( -6.039267359883488950, 9.133230122250985517, 1.199719254218452047 ) ) ;
#196002 = CARTESIAN_POINT ( 'NONE',  ( 6.355931484454268698, -0.7012994977402075003, 1.948090369817329526 ) ) ;
#196003 = CARTESIAN_POINT ( 'NONE',  ( 5.144429221381498607, 8.089252293998699272, -1.199719254218452047 ) ) ;
#196004 = CARTESIAN_POINT ( 'NONE',  ( -5.540478329478883524, 9.615641817700700145, 0.000000000000000000 ) ) ;
#196005 = CARTESIAN_POINT ( 'NONE',  ( -1.501062075862715339, 8.754928401006202066, 2.503798761944588058 ) ) ;
#196006 = CARTESIAN_POINT ( 'NONE',  ( 4.416843060293515144, 1.802029179758830812, 0.8000101564944164245 ) ) ;
#196007 = CARTESIAN_POINT ( 'NONE',  ( 6.381118777440311085, -1.848351591093103652, -0.8147283084726087976 ) ) ;
#196008 = CARTESIAN_POINT ( 'NONE',  ( 0.7499999999999885647, 0.2645833340161538039, 1.299038105676657340 ) ) ;
#196009 = CARTESIAN_POINT ( 'NONE',  ( 4.477368160356545168, 0.002844634383740093052, -2.307868969966973438 ) ) ;
#196010 = CARTESIAN_POINT ( 'NONE',  ( 2.079038939659454854, 1.922984332675440777, 0.7462749415493277194 ) ) ;
#196011 = CARTESIAN_POINT ( 'NONE',  ( 7.131225611108085616, 10.30321839872603462, 1.082531754730558626 ) ) ;
#196012 = CARTESIAN_POINT ( 'NONE',  ( 5.204350862799327793, 7.165104988056252289, -1.599625672291281386 ) ) ;
#196013 = CARTESIAN_POINT ( 'NONE',  ( 4.817943484809818600, 6.714296380401858499, 1.599625672291269396 ) ) ;
#196014 = CARTESIAN_POINT ( 'NONE',  ( -1.364683531250012516, 1.592708333674756727, 0.7879004041258379498 ) ) ;
#196015 = CARTESIAN_POINT ( 'NONE',  ( 3.217027588192558074, 6.975225629525113824, -1.734723475976807094E-15 ) ) ;
#196016 = CARTESIAN_POINT ( 'NONE',  ( 7.443063143778065438, 7.785921210603627962, -0.7216878364870257245 ) ) ;
#196017 = CARTESIAN_POINT ( 'NONE',  ( 3.877515590359277287, -0.1633623659567252084, 2.165103034678467431 ) ) ;
#196018 = CARTESIAN_POINT ( 'NONE',  ( -2.041582876286177406, -0.8887487162373145511, -2.583516629109316121 ) ) ;
#196020 = CARTESIAN_POINT ( 'NONE',  ( 3.157574601152390414, 0.8305207305269333151, 1.643389852989694200 ) ) ;
#196019 = CARTESIAN_POINT ( 'NONE',  ( -4.284013352238274841, 4.100363120473813794, -0.7216878364870207285 ) ) ;
#196021 = CARTESIAN_POINT ( 'NONE',  ( -1.364683531250010295, 5.030208333674757171, 0.7879004041258379498 ) ) ;
#196022 = CARTESIAN_POINT ( 'NONE',  ( 5.284801750429747536, 1.933107837519608685, -1.032524723389722787 ) ) ;
#196023 = DIRECTION ( 'NONE',  ( 1.000000000000000000, -0.000000000000000000, -0.000000000000000000 ) ) ;
#196024 = CARTESIAN_POINT ( 'NONE',  ( 5.770491790047429959, -1.440319307945096217, 1.744843718407377731 ) ) ;
#196025 = CARTESIAN_POINT ( 'NONE',  ( -4.868901516392104334, 6.903810023003053686, -1.445308410833840318 ) ) ;
#196026 = CARTESIAN_POINT ( 'NONE',  ( 4.710809438828709617, 8.349644928513606956, 0.6747337923850562635 ) ) ;
#196027 = CARTESIAN_POINT ( 'NONE',  ( -5.600926855776894975, 6.667407765562058053, -1.082531754730549967 ) ) ;
#196028 = DIRECTION ( 'NONE',  ( 0.000000000000000000, 0.000000000000000000, -1.000000000000000000 ) ) ;
#196029 = CARTESIAN_POINT ( 'NONE',  ( 6.134039733390581617, 0.8703851191177320867, -1.540848210998513990 ) ) ;
#196031 = CARTESIAN_POINT ( 'NONE',  ( 1.364683531250000748, 12.25520833367473195, -0.7879004041258355073 ) ) ;
#196030 = TOROIDAL_SURFACE ( 'NONE', #120020, 11.92000000000000171, 0.08000000000000000167 ) ;
#196032 =( BOUNDED_CURVE ( )  B_SPLINE_CURVE ( 2, ( #94527, #191975, #43642, #28434, #47918, #130283, #208231, #129233, #78245 ),
 .UNSPECIFIED., .F., .T. ) 
 B_SPLINE_CURVE_WITH_KNOTS ( ( 3, 2, 2, 2, 3 ),
 ( 0.7589285714285713969, 0.7619047619047618625, 0.7678571428571429047, 0.7738095238095238360, 0.7767857142857143016 ),
 .UNSPECIFIED. ) 
 CURVE ( )  GEOMETRIC_REPRESENTATION_ITEM ( )  RATIONAL_B_SPLINE_CURVE ( ( 0.9330127018922194093, 0.9330127018922194093, 1.000000000000000000, 0.8660254037844387076, 1.000000000000000000, 0.8660254037844387076, 1.000000000000000000, 0.9330127018922194093, 0.9330127018922194093 ) ) 
 REPRESENTATION_ITEM ( '' )  );
#196033 = CARTESIAN_POINT ( 'NONE',  ( 4.002593568968414672, -1.991494762441379462, -0.2932518702276361022 ) ) ;
#196034 = CARTESIAN_POINT ( 'NONE',  ( 5.472687561410540802, 9.536552588287639409, 0.7998128361456462443 ) ) ;
#196035 = CARTESIAN_POINT ( 'NONE',  ( 2.661270901210018636, -1.831774207203272775, -1.038945448840204122 ) ) ;
#196036 = CARTESIAN_POINT ( 'NONE',  ( 2.390125374076298659, -0.7353994070154221685, -1.769027144041198429 ) ) ;
#196037 = CARTESIAN_POINT ( 'NONE',  ( 2.347533153460546806, 5.890539112345938300, 0.000000000000000000 ) ) ;
#196038 = CARTESIAN_POINT ( 'NONE',  ( 3.209381719453743287, -1.608569549925453313, -1.136198915559688105 ) ) ;
#196039 = CARTESIAN_POINT ( 'NONE',  ( 2.043623373375623942, 0.7184291972081280342, -1.727395513401897453 ) ) ;
#196040 = CARTESIAN_POINT ( 'NONE',  ( 2.541395235131336694, 1.794889867694851260, -0.7924082849640816661 ) ) ;
#196043 = ORIENTED_EDGE ( 'NONE', *, *, #18861, .F. ) ;
#196042 = CARTESIAN_POINT ( 'NONE',  ( 0.08795244648929222142, 1.102731429460445334, 1.562230693318837238 ) ) ;
#196041 = CARTESIAN_POINT ( 'NONE',  ( 4.476996172482918368, -0.003761094005936410634, -1.725068444937064349 ) ) ;
#196045 = CARTESIAN_POINT ( 'NONE',  ( 4.514501963670558560, 8.210743357683563559, 1.040834085586084257E-14 ) ) ;
#196044 = CARTESIAN_POINT ( 'NONE',  ( 1.207977004800918852, -0.5332226995428279714, 2.141375170867452660 ) ) ;
#196046 = EDGE_CURVE ( 'NONE', #41517, #135108, #85897, .T. ) ;
#196047 = CARTESIAN_POINT ( 'NONE',  ( 1.364683531249986537, 0.2177083336747502595, -0.7879004041258309554 ) ) ;
#196048 = PRODUCT_DEFINITION ( 'UNKNOWN', '', #21037, #117584 ) ;
#196049 = CARTESIAN_POINT ( 'NONE',  ( 6.666881909320486521, -1.711340306973156977, -0.7558587634414122292 ) ) ;
#196050 = CARTESIAN_POINT ( 'NONE',  ( 0.3903331394470910820, 6.430882235217429077, -3.207842980289837165 ) ) ;
#196051 = CARTESIAN_POINT ( 'NONE',  ( 6.701130199342107296, -6.864242587301194298, -6.729185404178121388 ) ) ;
#196052 = CARTESIAN_POINT ( 'NONE',  ( 0.008622056077349157799, 14.55305231409391808, 11.95585894185517084 ) ) ;
#196053 = CARTESIAN_POINT ( 'NONE',  ( 0.8364851226981102617, -1.151554295457988930, 1.720357586142134076 ) ) ;
#196054 = CARTESIAN_POINT ( 'NONE',  ( 0.7499999999999902300, 1.483333333333357373, 1.299038105676657340 ) ) ;
#196055 = CARTESIAN_POINT ( 'NONE',  ( 6.531277313481192337, 8.642909503859968368, 1.599625672291281386 ) ) ;
#196056 = CARTESIAN_POINT ( 'NONE',  ( -8.864333505236459132, 9.236143932397675727, 1.040834085586084257E-14 ) ) ;
#196057 = CARTESIAN_POINT ( 'NONE',  ( 6.229045230835819069, 6.231917288922055320, -0.7998128361456481317 ) ) ;
#196058 = CARTESIAN_POINT ( 'NONE',  ( 5.373730994130427874, 0.4134100146411868737, -2.079626175754036410 ) ) ;
#196059 = CARTESIAN_POINT ( 'NONE',  ( 2.898410978271408922, 6.603506251283770112, -0.7998128361456362523 ) ) ;
#196060 = CARTESIAN_POINT ( 'NONE',  ( 0.6823417656249899377, 0.5927083336747518416, 1.181850606188755259 ) ) ;
#196061 = VERTEX_POINT ( 'NONE', #213977 ) ;
#196062 = MECHANICAL_DESIGN_GEOMETRIC_PRESENTATION_REPRESENTATION (  '', ( #109697 ), #78534 ) ;
#196063 = CARTESIAN_POINT ( 'NONE',  ( -1.201851678989727383E-14, 2.212500000000021672, 1.732050807568877637 ) ) ;
#196065 = CARTESIAN_POINT ( 'NONE',  ( 9.571693261567954636, 12.19006144329456731, 1.443375672974076540 ) ) ;
#196064 = CARTESIAN_POINT ( 'NONE',  ( 6.268018250734934682, -1.947192974725008963, 0.2387856323943157166 ) ) ;
#196066 = CARTESIAN_POINT ( 'NONE',  ( 3.778672575519220977, -1.986742196792599335, 0.3418835855632795795 ) ) ;
#196067 = CARTESIAN_POINT ( 'NONE',  ( 3.872214865662172656, -1.895674933386840344, -0.2753630107846723463 ) ) ;
#196068 = EDGE_CURVE ( 'NONE', #91043, #131458, #73177, .T. ) ;
#196069 = CARTESIAN_POINT ( 'NONE',  ( 1.118978350340808614, -0.04878210919301297771, 2.191179638975069732 ) ) ;
#196070 = CARTESIAN_POINT ( 'NONE',  ( -1.947641667917469510, 3.752373307046521944, 0.4616076617487344658 ) ) ;
#196071 = CARTESIAN_POINT ( 'NONE',  ( 1.499999999999989120, 0.8062500006828163812, 0.000000000000000000 ) ) ;
#196072 = CARTESIAN_POINT ( 'NONE',  ( -5.859094939400033120, 9.987361195942037639, -0.7998128361456231517 ) ) ;
#196074 = CARTESIAN_POINT ( 'NONE',  ( 5.712555019607242990, 2.040694153135207412, 0.5639581637400041814 ) ) ;
#196073 = CARTESIAN_POINT ( 'NONE',  ( -4.121315508874269007, 5.831287398485176077, -1.443375672974053447 ) ) ;
#196075 = CARTESIAN_POINT ( 'NONE',  ( -1.364683531250010295, 8.942708333674731946, 0.7879004041258445001 ) ) ;
#196077 = CARTESIAN_POINT ( 'NONE',  ( -5.908321080505254841, 10.11506803722328129, 0.7998128361456291469 ) ) ;
#196076 = CARTESIAN_POINT ( 'NONE',  ( 2.366838851271795718, 0.09958507307840713807, -2.088488507012337347 ) ) ;
#196079 = ORIENTED_EDGE ( 'NONE', *, *, #158865, .F. ) ;
#196078 = CARTESIAN_POINT ( 'NONE',  ( 1.271983708484729636, -1.098657341177114999, 1.329575768613028286 ) ) ;
#196080 = CARTESIAN_POINT ( 'NONE',  ( 7.447506452608354088, 7.583179037664891098, 0.7998128361456341429 ) ) ;
#196081 = CARTESIAN_POINT ( 'NONE',  ( -1.505691858957076246, 13.24428365067345403, -0.1501137743024005267 ) ) ;
#196082 = DIRECTION ( 'NONE',  ( 1.224643483124940471E-16, 0.002327115863039739760, 0.9999972922622140103 ) ) ;
#196083 = CARTESIAN_POINT ( 'NONE',  ( 10.95855051086948251, -7.723431457505092190, -0.6286713519883923018 ) ) ;
#196085 = CARTESIAN_POINT ( 'NONE',  ( 8.066738210006674237, 11.39464976410773467, 1.082531754730558626 ) ) ;
#196084 = CARTESIAN_POINT ( 'NONE',  ( 7.467843683028853263, 7.606905806488803101, 0.7998128361456341429 ) ) ;
#196086 = ORIENTED_EDGE ( 'NONE', *, *, #200959, .F. ) ;
#196087 = DIRECTION ( 'NONE',  ( -0.000000000000000000, 1.000000000000000000, -0.000000000000000000 ) ) ;
#196088 = ORIENTED_EDGE ( 'NONE', *, *, #66969, .F. ) ;
#196090 = CARTESIAN_POINT ( 'NONE',  ( 1.717148478332259254, 1.506203170942743030, 1.006022724715895045 ) ) ;
#196089 = CARTESIAN_POINT ( 'NONE',  ( 6.313256805818848960, 7.394496357324014113, 1.199719254218452047 ) ) ;
#196091 = CARTESIAN_POINT ( 'NONE',  ( -6.775324078527193983, 8.927630729746953264, -1.599625672291263179 ) ) ;
#196092 = CARTESIAN_POINT ( 'NONE',  ( 3.520313441042647540, 7.258782781191745137, 0.7998128361456321445 ) ) ;
#196093 = CARTESIAN_POINT ( 'NONE',  ( 5.875479466675786355, 7.948088359245467416, -1.599625672291283607 ) ) ;
#196094 = CARTESIAN_POINT ( 'NONE',  ( 6.639320575229278099, 0.5905802482995252678, 1.949996947996739172 ) ) ;
#196095 = DIRECTION ( 'NONE',  ( -0.000000000000000000, -1.000000000000000000, -0.000000000000000000 ) ) ;
#196096 = CARTESIAN_POINT ( 'NONE',  ( 4.839368334287259543, 6.711050605271530856, 1.249743143419468350 ) ) ;
#196097 = CARTESIAN_POINT ( 'NONE',  ( 8.676855123066012254, 11.14608361504227574, -1.443375672974052559 ) ) ;
#196098 = CARTESIAN_POINT ( 'NONE',  ( 3.209261600960995775, -1.519886386175553605, -1.073685847751577604 ) ) ;
#196099 = CARTESIAN_POINT ( 'NONE',  ( -0.05329673158829557195, -1.711387015114009369, -0.8607133870397830622 ) ) ;
#196100 = CARTESIAN_POINT ( 'NONE',  ( 0.2350025537052654601, -1.671451849548213797, 0.7345932495873632728 ) ) ;
#196101 = CARTESIAN_POINT ( 'NONE',  ( 1.455305287003863635, 4.347738815597921302, -0.3947446046151246724 ) ) ;
#196102 = CARTESIAN_POINT ( 'NONE',  ( -1.849150832860085414, 8.949220158640459388, 0.7750000000000013545 ) ) ;
#196103 = CARTESIAN_POINT ( 'NONE',  ( 4.678042868546113731, 8.270637144445508682, 0.5573067791126932180 ) ) ;
#196104 = CARTESIAN_POINT ( 'NONE',  ( -3.470524135418306511, 5.072030796119872953, -1.443375672974053447 ) ) ;
#196105 = CARTESIAN_POINT ( 'NONE',  ( 7.117667457494414762, 11.24776976714476184, 1.040834085586084257E-14 ) ) ;
#196106 = CARTESIAN_POINT ( 'NONE',  ( 4.135575292396717728, 1.855891543885644479, -0.6595280497384666818 ) ) ;
#196107 = CARTESIAN_POINT ( 'NONE',  ( 2.033984416766075665, -2.056095976692096094, 0.5180656111221926263 ) ) ;
#196108 = CARTESIAN_POINT ( 'NONE',  ( -5.904739593951539689, 6.847616600153594746, 1.199719254218450271 ) ) ;
#196109 = CARTESIAN_POINT ( 'NONE',  ( -11.94105721237523099, 10.19999999999999929, -1.187919463087248939 ) ) ;
#196110 = CARTESIAN_POINT ( 'NONE',  ( 5.560537033210596114, -1.979929515673630513, -0.9395970221138388867 ) ) ;
#196111 = CARTESIAN_POINT ( 'NONE',  ( 0.07999999999999327094, -9.900000000000005684, 10.91970695577496286 ) ) ;
#196112 = CARTESIAN_POINT ( 'NONE',  ( 5.157218254430565807, -1.627291586725558181, -1.030705938667796140 ) ) ;
#196113 = CARTESIAN_POINT ( 'NONE',  ( -7.379715684540041565, 7.504089808251839244, 1.040834085586084257E-14 ) ) ;
#196114 = CARTESIAN_POINT ( 'NONE',  ( 0.2526013166088726392, -1.469656019175567208, 1.082793315970068004 ) ) ;
#196115 = CARTESIAN_POINT ( 'NONE',  ( 0.8564375766340023288, 2.204168734417511821, -0.1118928034387969561 ) ) ;
#196116 = FILL_AREA_STYLE_COLOUR ( '', #37743 ) ;
#196117 = LINE ( 'NONE', #47754, #43619 ) ;
#196118 = ORIENTED_EDGE ( 'NONE', *, *, #134087, .T. ) ;
#196119 = ORIENTED_EDGE ( 'NONE', *, *, #15602, .F. ) ;
#196120 = CARTESIAN_POINT ( 'NONE',  ( 5.682459527512692787, 1.176241607570350567, -1.579419126353029279 ) ) ;
#196121 = CARTESIAN_POINT ( 'NONE',  ( 1.417416744832197484, -1.080314125112752155, -1.613661906057413331 ) ) ;
#196122 = VECTOR ( 'NONE', #132279, 1000.000000000000000 ) ;
#196123 = CARTESIAN_POINT ( 'NONE',  ( 0.7024996975148189993, -1.423740904080775138, -1.427721366232127753 ) ) ;
#196125 = CARTESIAN_POINT ( 'NONE',  ( 5.998848716047340268, 0.3616406339099677014, 1.825274704766747913 ) ) ;
#196124 = CARTESIAN_POINT ( 'NONE',  ( -5.956828388357799042, 8.042995434541133193, 1.599625672291263179 ) ) ;
#196126 = CARTESIAN_POINT ( 'NONE',  ( 5.550083779947807550, 7.568460058062819407, -1.599625672291283607 ) ) ;
#196127 = CARTESIAN_POINT ( 'NONE',  ( 1.500000000000001332, 11.37499999999999645, 0.000000000000000000 ) ) ;
#196128 = CARTESIAN_POINT ( 'NONE',  ( -5.904739593951539689, 6.847616600153594746, 1.199719254218450271 ) ) ;
#196129 = CARTESIAN_POINT ( 'NONE',  ( -7.761116589180078407, 8.019333873657032541, 0.000000000000000000 ) ) ;
#196130 = CARTESIAN_POINT ( 'NONE',  ( 1.171705676731093604, 1.309414992938146893, 1.757219779060022580 ) ) ;
#196131 = CARTESIAN_POINT ( 'NONE',  ( 3.334942599281629949, 5.874221551595115720, -1.082531754730543083 ) ) ;
#196132 = ORIENTED_EDGE ( 'NONE', *, *, #96704, .F. ) ;
#196133 = LINE ( 'NONE', #197179, #95081 ) ;
#196134 = DIRECTION ( 'NONE',  ( 0.7592566023653005702, -0.6507913734559639396, 0.000000000000000000 ) ) ;
#196135 = CARTESIAN_POINT ( 'NONE',  ( 1.154616158753757338, -1.440623569337009968, 1.121372061650728558 ) ) ;
#196136 = CARTESIAN_POINT ( 'NONE',  ( -3.164938793786285842, 5.779846795137578930, -1.199719254218452935 ) ) ;
#196137 = CARTESIAN_POINT ( 'NONE',  ( -6.514548575684607989, 6.824011503973982151, -0.5624163230865379948 ) ) ;
#196138 = CARTESIAN_POINT ( 'NONE',  ( -1.999999999999988010, 2.428614679364265457E-14, 0.5999999999999969802 ) ) ;
#196139 = CARTESIAN_POINT ( 'NONE',  ( 8.215351014876830504, 11.67199438640995801, -1.199719254218446718 ) ) ;
#196140 = CARTESIAN_POINT ( 'NONE',  ( 6.270122753791413928, 0.9430518052575274091, 1.563124558401955300 ) ) ;
#196141 = CARTESIAN_POINT ( 'NONE',  ( 4.575024454672827368, 1.791946274209740952, 0.7988320279663924106 ) ) ;
#196142 = CARTESIAN_POINT ( 'NONE',  ( -6.679363233026820446, 10.94434087183997129, 0.000000000000000000 ) ) ;
#196143 = CARTESIAN_POINT ( 'NONE',  ( 5.937581207780954884, 9.014596278131406848, -1.199719254218440723 ) ) ;
#196144 = CARTESIAN_POINT ( 'NONE',  ( 4.247736854543925133, 2.191053489037126045, -0.05455935714590579716 ) ) ;
#196145 = VECTOR ( 'NONE', #204258, 1000.000000000000000 ) ;
#196146 = CARTESIAN_POINT ( 'NONE',  ( 6.609000000000042618, 6.036791015687303918, 2.594900324319386886 ) ) ;
#196147 = CARTESIAN_POINT ( 'NONE',  ( 3.661042849074844785, 1.635018244968543977, -1.269851595989857085 ) ) ;
#196149 = CARTESIAN_POINT ( 'NONE',  ( -1.364683531250000748, 1.071875000341421247, 0.000000000000000000 ) ) ;
#196148 = CARTESIAN_POINT ( 'NONE',  ( 1.255262969126037241E-15, 5.999999999999998224, -10.25000000000000000 ) ) ;
#196150 = ORIENTED_EDGE ( 'NONE', *, *, #150235, .F. ) ;
#196151 = CARTESIAN_POINT ( 'NONE',  ( 4.237165586469007650, 2.298153656159235503, -0.05646909981197979073 ) ) ;
#196152 = CARTESIAN_POINT ( 'NONE',  ( 8.609064354997688184, 9.146255957026539818, 1.040834085586084257E-14 ) ) ;
#196154 = CARTESIAN_POINT ( 'NONE',  ( -1.642778471875000035, -0.1677083328553742592, -2.845375778867859751 ) ) ;
#196153 = CARTESIAN_POINT ( 'NONE',  ( 7.024532985656141371, 7.367912369453226695, 0.7216878364870328300 ) ) ;
#196155 = CARTESIAN_POINT ( 'NONE',  ( 6.620655732516649294, 4.703748234811334861, 2.289014941052476715 ) ) ;
#196156 = CARTESIAN_POINT ( 'NONE',  ( -6.563028877466991595, 9.814561569423593923, 1.199719254218452935 ) ) ;
#196157 = CARTESIAN_POINT ( 'NONE',  ( 4.329980137697307718, 1.904743498531726198, 0.3774997404530285317 ) ) ;
#196158 = ORIENTED_EDGE ( 'NONE', *, *, #111366, .F. ) ;
#196159 = CARTESIAN_POINT ( 'NONE',  ( -0.2514851628625219271, -9.242341987627245459, 9.497468999145645796 ) ) ;
#196160 = CARTESIAN_POINT ( 'NONE',  ( 4.254103502353132171, 0.8128351696983120434, -1.731171583500931366 ) ) ;
#196161 = CARTESIAN_POINT ( 'NONE',  ( 4.650083499807233345, 5.295740330745369207, -1.000000000000000888 ) ) ;
#196162 = CARTESIAN_POINT ( 'NONE',  ( 5.526277428723715524, 1.024295688422135031, -1.387495638070087134 ) ) ;
#196163 = CARTESIAN_POINT ( 'NONE',  ( 4.153529959351897283, 1.954779968807466295, -0.4946301968136583849 ) ) ;
#196164 = CARTESIAN_POINT ( 'NONE',  ( 4.641406123262603600, 0.8788069589312655916, 2.124244668743579201 ) ) ;
#196165 = CARTESIAN_POINT ( 'NONE',  ( -11.89942855770814134, 12.30000000000000071, 0.6999999999999992895 ) ) ;
#196166 = CARTESIAN_POINT ( 'NONE',  ( 0.5752038918783763943, -2.079344756725898691, -0.7397341299467049547 ) ) ;
#196168 = CARTESIAN_POINT ( 'NONE',  ( -3.499413046103020175, 7.096749297179887783, 0.7216878364870338292 ) ) ;
#196167 = CARTESIAN_POINT ( 'NONE',  ( -3.874835629217528776, 7.473463894690999254, -0.3237328633659316002 ) ) ;
#196169 = CARTESIAN_POINT ( 'NONE',  ( 5.448444396454582339, 0.5145788473605721336, 1.693291817928108234 ) ) ;
#196170 = ADVANCED_FACE ( 'NONE', ( #12605 ), #97099, .T. ) ;
#196172 = CARTESIAN_POINT ( 'NONE',  ( 1.957357739143847919, 0.3891275796813770116, -2.258848713223185367 ) ) ;
#196171 = CARTESIAN_POINT ( 'NONE',  ( 5.254667053748194760, 8.288139441751686931, 1.199719254218452047 ) ) ;
#196173 = CARTESIAN_POINT ( 'NONE',  ( 1.552286559517775499, -1.491368903747305019, -0.8966978864634599367 ) ) ;
#196174 = CARTESIAN_POINT ( 'NONE',  ( -10.17567228521070710, -0.02076350362892331880, 2.499999999999999556 ) ) ;
#196175 = CARTESIAN_POINT ( 'NONE',  ( 0.8953158854557360380, 0.1194439997053517860, 1.729786500971510765 ) ) ;
#196176 = CARTESIAN_POINT ( 'NONE',  ( -1.360316468750044860, 1.151041667008095404, -0.7853790794159261068 ) ) ;
#196177 = CARTESIAN_POINT ( 'NONE',  ( -11.48243876534946217, 12.29999999999998295, 3.199999999999997957 ) ) ;
#196178 = CARTESIAN_POINT ( 'NONE',  ( 0.9597157272863182653, 1.774996621215488624, 1.250093255441329543 ) ) ;
#196179 = CARTESIAN_POINT ( 'NONE',  ( 2.641814858895009444, 2.006371511526034546, -0.2024640970367599380 ) ) ;
#196180 = CARTESIAN_POINT ( 'NONE',  ( 0.7499999999999885647, -0.4854166659838468623, 1.299038105676657340 ) ) ;
#196181 = CARTESIAN_POINT ( 'NONE',  ( 6.024042007596412063, -1.072333998858214343, -1.600281699052849893 ) ) ;
#196182 = CARTESIAN_POINT ( 'NONE',  ( -1.364683531250010295, 12.63020833367473372, 0.7879004041258445001 ) ) ;
#196183 = CARTESIAN_POINT ( 'NONE',  ( 1.986886853112525442, -1.362214788617806649, 1.754679387841934002 ) ) ;
#196184 = ORIENTED_EDGE ( 'NONE', *, *, #119838, .F. ) ;
#196185 = CARTESIAN_POINT ( 'NONE',  ( 6.764644832398833962, -7.632775601084119010, 6.764644832401402574 ) ) ;
#196186 = PRESENTATION_STYLE_ASSIGNMENT (( #161565 ) ) ;
#196187 = CARTESIAN_POINT ( 'NONE',  ( 7.065770611016287006, 11.39514947949436774, 1.040834085586084257E-14 ) ) ;
#196188 =( NAMED_UNIT ( * ) PLANE_ANGLE_UNIT ( ) SI_UNIT ( $, .RADIAN. ) );
#196189 = PRESENTATION_STYLE_ASSIGNMENT (( #146395 ) ) ;
#196190 = CARTESIAN_POINT ( 'NONE',  ( 5.565861978284946332, -1.097836388496459037, 1.350534753149737366 ) ) ;
#196191 = CARTESIAN_POINT ( 'NONE',  ( 3.139059813392345077, -0.1416510307416830594, -1.956792864499560691 ) ) ;
#196193 = CARTESIAN_POINT ( 'NONE',  ( -7.537970219518089543, 8.857015346601659900, -1.082531754730543971 ) ) ;
#196192 = CARTESIAN_POINT ( 'NONE',  ( 4.857899112398166075, 4.561970474086296079, 1.040834085586084257E-14 ) ) ;
#196194 = CARTESIAN_POINT ( 'NONE',  ( -1.464648953335778270, 4.228397023187225656, -0.3340396966001182300 ) ) ;
#196195 = CARTESIAN_POINT ( 'NONE',  ( 4.745575995134789338, -1.744828745684245508, -1.440138369970354493 ) ) ;
#196196 = CARTESIAN_POINT ( 'NONE',  ( 1.346217686498082378, -0.9293675016086970775, 1.841534056632480265 ) ) ;
#196197 = CARTESIAN_POINT ( 'NONE',  ( -7.881367368245678406, 8.089350105908421185, 0.7998128361456602331 ) ) ;
#196198 = ADVANCED_FACE ( 'NONE', ( #79747 ), #124520, .F. ) ;
#196199 = CARTESIAN_POINT ( 'NONE',  ( 2.501149491322187224, 1.817439291034177451, -1.347377658580677817 ) ) ;
#196200 = VERTEX_POINT ( 'NONE', #196704 ) ;
#196201 = CARTESIAN_POINT ( 'NONE',  ( 1.499999999999989120, 1.306250000682816825, 0.000000000000000000 ) ) ;
#196202 = CARTESIAN_POINT ( 'NONE',  ( 2.178771278573924608, -0.08713135167291724548, -1.868625915979430951 ) ) ;
#196203 = CARTESIAN_POINT ( 'NONE',  ( 1.793227186479518398, 1.284509341651525638, -1.165198513391290103 ) ) ;
#196204 = CARTESIAN_POINT ( 'NONE',  ( 5.776942576169182608, 2.025397260235710206, -0.8375503648087383457 ) ) ;
#196205 = CARTESIAN_POINT ( 'NONE',  ( 6.739320262688799801, -2.065560010629815313, 1.029036360498974068 ) ) ;
#196206 = CARTESIAN_POINT ( 'NONE',  ( 3.924826023212550030, 2.051882857192890430, 0.6804245187241527715 ) ) ;
#196207 = CARTESIAN_POINT ( 'NONE',  ( 4.294824717068760123, 1.560567246164183519, 1.155581451937383930 ) ) ;
#196208 = AXIS2_PLACEMENT_3D ( 'NONE', #77054, #126975, #14169 ) ;
#196209 = CARTESIAN_POINT ( 'NONE',  ( -3.429849674132948500, 5.024577257953626308, -1.443375672974051449 ) ) ;
#196210 = CARTESIAN_POINT ( 'NONE',  ( -0.07933194154489606187, 7.849261790823902629, -9.499668754385620417 ) ) ;
#196211 = CARTESIAN_POINT ( 'NONE',  ( 1.125000000000000888, -2.052068128417952497, 6.471134675641443159E-14 ) ) ;
#196212 = CARTESIAN_POINT ( 'NONE',  ( 4.632932323280743780, 6.889805956345480986, 1.213532624337316124 ) ) ;
#196213 = CARTESIAN_POINT ( 'NONE',  ( -1.162044386198238837E-16, 2.062499999999991562, 1.224999999999974332 ) ) ;
#196214 = CARTESIAN_POINT ( 'NONE',  ( 1.292131300536165872, -3.232243495192088201, 3.032550610867861707 ) ) ;
#196215 = DIRECTION ( 'NONE',  ( 0.000000000000000000, 0.000000000000000000, 1.000000000000000000 ) ) ;
#196216 = CARTESIAN_POINT ( 'NONE',  ( 5.766250055133458119, 1.862018000461727052, -0.7743128548072516493 ) ) ;
#196217 = CARTESIAN_POINT ( 'NONE',  ( -10.66756793585402363, 11.33991743478486391, 0.7998128361456462443 ) ) ;
#196218 = CARTESIAN_POINT ( 'NONE',  ( 7.476431642932036326, 10.80992178580769014, 1.199719254218460707 ) ) ;
#196219 = DIRECTION ( 'NONE',  ( 0.9486832980505138790, -0.3162277660168376636, -3.312310031615527152E-15 ) ) ;
#196221 = CARTESIAN_POINT ( 'NONE',  ( -4.164650907004922686, 7.866613389087279806, 0.1028172011370054872 ) ) ;
#196220 = CARTESIAN_POINT ( 'NONE',  ( 2.771877994228102882, 0.9767612972278701955, 1.542236413651025151 ) ) ;
#196222 = CARTESIAN_POINT ( 'NONE',  ( -3.023105066167347310, 5.702484939155337607, 2.420000000000010587 ) ) ;
#196223 = ORIENTED_EDGE ( 'NONE', *, *, #71920, .F. ) ;
#196224 = CARTESIAN_POINT ( 'NONE',  ( -6.089020385868876062, 6.276481003034692030, -0.7216878364870338292 ) ) ;
#196225 = CARTESIAN_POINT ( 'NONE',  ( 4.689424523294686509, 8.358602041046323095, -0.7454045323363467368 ) ) ;
#196226 = CARTESIAN_POINT ( 'NONE',  ( -8.890396042259075315, 11.39521468743417998, -1.599625672291263179 ) ) ;
#196227 = CARTESIAN_POINT ( 'NONE',  ( 0.1233147457768641181, 1.759488896278412540, 0.9916404401272023161 ) ) ;
#196228 = CARTESIAN_POINT ( 'NONE',  ( 1.330900338397854155, 1.421537331630345014, -1.573617108223644312 ) ) ;
#196229 = VERTEX_POINT ( 'NONE', #212934 ) ;
#196230 = CARTESIAN_POINT ( 'NONE',  ( -6.134138155540168391, 6.121192367743780949, 0.000000000000000000 ) ) ;
#196231 = CARTESIAN_POINT ( 'NONE',  ( 5.529027716274630855, 5.344953845275508542, 1.040834085586084257E-14 ) ) ;
#196232 = CARTESIAN_POINT ( 'NONE',  ( 0.1632417891470130944, -1.931755829615459996, -0.9703963252955111196 ) ) ;
#196233 = CARTESIAN_POINT ( 'NONE',  ( 6.240861317752083970, 2.010826688392798101, -0.1511364921914087889 ) ) ;
#196234 = VERTEX_POINT ( 'NONE', #64570 ) ;
#196235 = CARTESIAN_POINT ( 'NONE',  ( -9.809487834687324437, 11.40315621434539395, 1.199719254218462483 ) ) ;
#196236 = CARTESIAN_POINT ( 'NONE',  ( -1.854512760316423536, 2.488359591189891251, 2.484105960264900936 ) ) ;
#196239 = ORIENTED_EDGE ( 'NONE', *, *, #5890, .T. ) ;
#196238 = CARTESIAN_POINT ( 'NONE',  ( 0.000000000000000000, -0.5000000000000004441, 0.000000000000000000 ) ) ;
#196237 = CARTESIAN_POINT ( 'NONE',  ( -3.969505113751027547, 7.853116076009993840, 1.214306433183764966E-14 ) ) ;
#196240 = CARTESIAN_POINT ( 'NONE',  ( 6.148788998471866662, 7.076870205577955986, 1.084632487400632339 ) ) ;
#196241 = CARTESIAN_POINT ( 'NONE',  ( 5.782577320554741718, -1.967585831723076772, 0.4389650999883643046 ) ) ;
#196242 = CARTESIAN_POINT ( 'NONE',  ( 5.050657991863417351, -1.557144343216086968, -0.9820927893566462341 ) ) ;
#196243 = CARTESIAN_POINT ( 'NONE',  ( -0.02299388927988389730, 6.948790505698306141, -2.506045543530223352 ) ) ;
#196244 = CARTESIAN_POINT ( 'NONE',  ( 3.229449743806306561, 0.05664919459314603917, 2.307159798345681523 ) ) ;
#196245 = CARTESIAN_POINT ( 'NONE',  ( 7.015418140428412386, 7.149352350113456822, 0.7998128361456331437 ) ) ;
#196246 = CARTESIAN_POINT ( 'NONE',  ( 6.221977808853903724, -1.195094089922192016, -1.800988070004491792 ) ) ;
#196247 = CARTESIAN_POINT ( 'NONE',  ( 5.960781091502512119, 10.10599504006161986, 0.7998128361456462443 ) ) ;
#196248 = CARTESIAN_POINT ( 'NONE',  ( 1.575622484978753679, -1.037422314974449478, 1.641571771860099727 ) ) ;
#196249 = CARTESIAN_POINT ( 'NONE',  ( -2.788173145904702555, 6.404619103530779789, -0.7998128361456281477 ) ) ;
#196250 = ORIENTED_EDGE ( 'NONE', *, *, #200174, .T. ) ;
#196251 = CARTESIAN_POINT ( 'NONE',  ( 4.587492961451061113, 1.418373992658492400, -1.808456645134959073 ) ) ;
#196252 = CARTESIAN_POINT ( 'NONE',  ( 5.431895982697334091, 6.433277491268158954, -1.247050338538328029 ) ) ;
#196253 = CARTESIAN_POINT ( 'NONE',  ( -3.481411583659053566, 7.283673624236017830, 0.000000000000000000 ) ) ;
#196254 = CARTESIAN_POINT ( 'NONE',  ( 5.067206508511894469, 0.1826785619755930679, -1.861722072867748823 ) ) ;
#196257 = CARTESIAN_POINT ( 'NONE',  ( -5.773793314573309132, 7.829454515125894964, 1.599625672291263179 ) ) ;
#196256 = CARTESIAN_POINT ( 'NONE',  ( 0.7499999999999885647, 0.2645833340161538039, 1.299038105676657340 ) ) ;
#196255 = CARTESIAN_POINT ( 'NONE',  ( 1.142663480069527671, 1.843847066288730074, 0.5072560978593986247 ) ) ;
#196258 = CARTESIAN_POINT ( 'NONE',  ( 3.194164748978207680, -0.8942147705085048415, 2.017778291555922809 ) ) ;
#196259 = CARTESIAN_POINT ( 'NONE',  ( -1.495402192688975340, 8.717956978849768390, -2.557532308801403698 ) ) ;
#196260 = CARTESIAN_POINT ( 'NONE',  ( 3.541704441667858472, 5.155074486744371853, -1.599625672291262513 ) ) ;
#196261 = CARTESIAN_POINT ( 'NONE',  ( 5.004368096775565711, 8.852530189631227842, -0.7216878364870458196 ) ) ;
#196262 = CARTESIAN_POINT ( 'NONE',  ( -2.611917148927046295, 6.198987107056845858, 1.040834085586084257E-14 ) ) ;
#196263 = CARTESIAN_POINT ( 'NONE',  ( -6.929625909916163451, 7.257187447756535903, 0.7216878364870317197 ) ) ;
#196264 = CARTESIAN_POINT ( 'NONE',  ( 1.669145487688096896, 0.1492116152736686074, -1.965789094590511654 ) ) ;
#196265 = CARTESIAN_POINT ( 'NONE',  ( 0.6929124517485165669, -2.290651033777380441, -0.2787006195923043550 ) ) ;
#196266 = CARTESIAN_POINT ( 'NONE',  ( 0.8714495147512549833, -0.2914478312704605889, 1.939986204769503786 ) ) ;
#196267 = CARTESIAN_POINT ( 'NONE',  ( 5.067260671706765862, 1.791893645760339826, 1.021364248522889762 ) ) ;
#196268 = CARTESIAN_POINT ( 'NONE',  ( 3.701012746850603996, 7.261672604726938651, 1.040834085586084257E-14 ) ) ;
#196269 = CARTESIAN_POINT ( 'NONE',  ( 5.204350862799327793, 7.165104988056252289, -1.599625672291281386 ) ) ;
#196270 = ORIENTED_EDGE ( 'NONE', *, *, #172200, .T. ) ;
#196271 = CARTESIAN_POINT ( 'NONE',  ( -10.62011439820619429, 11.28455497419572318, -0.7998128361456221525 ) ) ;
#196272 = CARTESIAN_POINT ( 'NONE',  ( -4.921546165693497343, 4.882379070747932204, 0.5514684743740734252 ) ) ;
#196273 = CARTESIAN_POINT ( 'NONE',  ( 3.755245360860917536, 5.404205559136275205, -1.443375672974051449 ) ) ;
#196275 = VECTOR ( 'NONE', #77846, 1000.000000000000000 ) ;
#196274 = CARTESIAN_POINT ( 'NONE',  ( 0.4093307213487142326, -1.744552795675001100, 1.292164652415381365 ) ) ;
#196276 = CARTESIAN_POINT ( 'NONE',  ( 11.07790593930098311, 13.79999999999999893, 0.6999999999999992895 ) ) ;
#196277 = CARTESIAN_POINT ( 'NONE',  ( 10.85075961359305197, 3.974415841077577838, -3.932216895623887432 ) ) ;
#196278 = CARTESIAN_POINT ( 'NONE',  ( 6.773846765317333762, -7.246166700180801001, 6.773846765317311558 ) ) ;
#196279 = CARTESIAN_POINT ( 'NONE',  ( 0.8076147168173102298, -1.862120749842037570, 0.1771838942275505424 ) ) ;
#196280 = CARTESIAN_POINT ( 'NONE',  ( 5.694645791630270182, -0.5191100231263061637, -2.098234375727751733 ) ) ;
#196281 = CARTESIAN_POINT ( 'NONE',  ( -5.968994907891031154, 6.102274133640173126, 0.7348006213908353512 ) ) ;
#196282 = CARTESIAN_POINT ( 'NONE',  ( -0.02244404828157658613, 7.629137130509074716, -2.789100637983293662 ) ) ;
#196283 = CARTESIAN_POINT ( 'NONE',  ( 1.364683531249986537, -0.3447916663252443836, -0.7879004041258309554 ) ) ;
#196284 = CARTESIAN_POINT ( 'NONE',  ( 1.980978873585538480, -1.748965405663160944, -0.7736543689686598002 ) ) ;
#196285 = CARTESIAN_POINT ( 'NONE',  ( 3.361912448646987794, 0.7947379027260987883, 1.581431320561203169 ) ) ;
#196286 = CARTESIAN_POINT ( 'NONE',  ( 0.3461628310420067911, 0.9829124436787042285, -1.640176041098049264 ) ) ;
#196287 = CARTESIAN_POINT ( 'NONE',  ( -4.554649539187067830, 7.401175998105142817, 1.199719254218464037 ) ) ;
#196289 = CARTESIAN_POINT ( 'NONE',  ( 5.501554071977204252, -1.867810700675033297, 0.4244617614653464766 ) ) ;
#196288 = CARTESIAN_POINT ( 'NONE',  ( 3.328416922175579273, -3.193033774422709303, -0.09933519640907825798 ) ) ;
#196290 = CARTESIAN_POINT ( 'NONE',  ( 6.373500198570408060, -0.2424619166165129514, 1.954513512140013676 ) ) ;
#196291 = CARTESIAN_POINT ( 'NONE',  ( -0.7500000000000215383, 4.691666666666684193, 1.299038105676671107 ) ) ;
#196292 = CARTESIAN_POINT ( 'NONE',  ( 0.5102161431939798986, -0.7575819503438313562, 1.980855387931411915 ) ) ;
#196293 = CARTESIAN_POINT ( 'NONE',  ( 4.592568387165754551, -0.4099775813008778025, -1.825014511474598589 ) ) ;
#196295 = ORIENTED_EDGE ( 'NONE', *, *, #166752, .F. ) ;
#196294 = CARTESIAN_POINT ( 'NONE',  ( 0.5393321728033516615, -1.288848960320065462, -1.293324666950084190 ) ) ;
#196297 = CARTESIAN_POINT ( 'NONE',  ( 4.812442952513422689, 8.115120723895499211, -0.8517184758452013282 ) ) ;
#196296 = CARTESIAN_POINT ( 'NONE',  ( 4.530015419921377351, -1.356323209173672106, -1.740806116466916409 ) ) ;
#196298 = ADVANCED_FACE ( 'NONE', ( #66651 ), #149009, .T. ) ;
#196299 = CARTESIAN_POINT ( 'NONE',  ( 1.364683531249986537, -0.5947916663252456049, -0.7879004041258309554 ) ) ;
#196300 = CARTESIAN_POINT ( 'NONE',  ( 2.313000242259897199, -1.596077997345384247, 1.306617308116851062 ) ) ;
#196301 = CARTESIAN_POINT ( 'NONE',  ( 4.638861114170084399, 8.563755066507100722, 0.7998128361456462443 ) ) ;
#196302 = CARTESIAN_POINT ( 'NONE',  ( -9.338868881714763148, 9.789768538289042255, -0.7998128361456291469 ) ) ;
#196303 =( LENGTH_UNIT ( ) NAMED_UNIT ( * ) SI_UNIT ( .MILLI., .METRE. ) );
#196304 = CARTESIAN_POINT ( 'NONE',  ( 9.836604141914616406, 11.43479190611061647, 1.199719254218452047 ) ) ;
#196305 = CYLINDRICAL_SURFACE ( 'NONE', #34283, 11.00000000000000000 ) ;
#196306 =( NAMED_UNIT ( * ) SI_UNIT ( $, .STERADIAN. ) SOLID_ANGLE_UNIT ( ) );
#196307 = PLANE ( 'NONE',  #186258 ) ;
#196308 = CIRCLE ( 'NONE', #161825, 2.000000000000000000 ) ;
#196309 = ORIENTED_EDGE ( 'NONE', *, *, #49744, .F. ) ;
#196310 = CARTESIAN_POINT ( 'NONE',  ( 4.369627354678314646, -0.3570511267821044332, 2.039192500141631115 ) ) ;
#196311 = CARTESIAN_POINT ( 'NONE',  ( 1.499999999999991118, 5.754166666666685970, 0.8660254037844524744 ) ) ;
#196312 = CARTESIAN_POINT ( 'NONE',  ( 1.159701560084012595, 0.4228694819443152286, -2.119656415666733906 ) ) ;
#196313 = CARTESIAN_POINT ( 'NONE',  ( -5.733196416021622888, 7.293175961584016598, -1.208997762321398550 ) ) ;
#196314 = CARTESIAN_POINT ( 'NONE',  ( 2.192062543670767027, 1.244387780127395482, 1.590672870423719187 ) ) ;
#196315 = FACE_OUTER_BOUND ( 'NONE', #4088, .T. ) ;
#196316 = ORIENTED_EDGE ( 'NONE', *, *, #194701, .F. ) ;
#196318 = CARTESIAN_POINT ( 'NONE',  ( 8.432808358020029260, 8.940623960552603222, 0.7216878364870438212 ) ) ;
#196317 = CARTESIAN_POINT ( 'NONE',  ( 0.07479286986305545837, 0.7422478802248284602, -1.939684878352589070 ) ) ;
#196319 = CARTESIAN_POINT ( 'NONE',  ( -2.791320394097926997E-15, -5.754340240174641963, 10.93220419382255848 ) ) ;
#196320 = CARTESIAN_POINT ( 'NONE',  ( -4.543390873910949423, 6.393985001019784953, 1.443375672974058777 ) ) ;
#196321 = CARTESIAN_POINT ( 'NONE',  ( 0.6027503803631119039, 1.865048444749048739, 0.7672877736318934883 ) ) ;
#196322 = CARTESIAN_POINT ( 'NONE',  ( 5.161759341795384870, 1.079763445194487970, 1.907048802792680631 ) ) ;
#196323 = CARTESIAN_POINT ( 'NONE',  ( 0.7499999999999902300, 4.847916667349482012, -1.299038105676658228 ) ) ;
#196324 = CARTESIAN_POINT ( 'NONE',  ( 5.062724140118718630, 0.5608846916410530348, 1.828269531156314631 ) ) ;
#196325 = CARTESIAN_POINT ( 'NONE',  ( -5.101945877444165944, 4.846691699973280976, 0.000000000000000000 ) ) ;
#196326 = CARTESIAN_POINT ( 'NONE',  ( 5.436456408955479880, 9.286356877182658565, -0.7216878364870267237 ) ) ;
#196328 = CARTESIAN_POINT ( 'NONE',  ( 2.179314750421776026, 1.560514648525725967, 1.277027416600539755 ) ) ;
#196327 = CARTESIAN_POINT ( 'NONE',  ( -10.58855478214856660, 11.45566145536924552, -0.7216878364870217277 ) ) ;
#196329 = CARTESIAN_POINT ( 'NONE',  ( -8.012344526598182026E-15, 12.35937500034139624, -1.575800808251669460 ) ) ;
#196331 = CARTESIAN_POINT ( 'NONE',  ( -5.666381855868691808, 5.575476684793721383, 0.000000000000000000 ) ) ;
#196330 = CARTESIAN_POINT ( 'NONE',  ( 0.4863598079122740114, -2.275998871909711951, -0.2730087134108442615 ) ) ;
#196332 = CARTESIAN_POINT ( 'NONE',  ( 4.647282941162062642, -1.334376716645750971, -1.092789356466111972 ) ) ;
#196333 = CARTESIAN_POINT ( 'NONE',  ( -0.1399997263889594112, -0.002789056014654289761, -2.000146600338557956 ) ) ;
#196334 = CARTESIAN_POINT ( 'NONE',  ( 4.467575310902914154, 5.170924936596891008, 1.199719254218464037 ) ) ;
#196335 = DIRECTION ( 'NONE',  ( 0.000000000000000000, 0.000000000000000000, -1.000000000000000000 ) ) ;
#196336 = FACE_OUTER_BOUND ( 'NONE', #28540, .T. ) ;
#196337 = VECTOR ( 'NONE', #197018, 1000.000000000000000 ) ;
#196338 = DIRECTION ( 'NONE',  ( 1.214306433183764966E-17, 1.000000000000000000, 5.200009205990155575E-32 ) ) ;
#196339 = ORIENTED_EDGE ( 'NONE', *, *, #87041, .F. ) ;
#196341 = B_SPLINE_CURVE_WITH_KNOTS ( 'NONE', 3,
 ( #180176, #78399, #143447, #80539, #13394, #130438, #79470 ),
 .UNSPECIFIED., .F., .F.,
 ( 4, 3, 4 ),
 ( 0.0001788552925466778897, 0.0009000000022260264132, 0.002103779968145178675 ),
 .UNSPECIFIED. ) ;
#196340 = CARTESIAN_POINT ( 'NONE',  ( 5.531847899045232886, -1.765878665049234186, 0.4030928165594855339 ) ) ;
#196342 = ORIENTED_EDGE ( 'NONE', *, *, #98928, .T. ) ;
#196343 = CARTESIAN_POINT ( 'NONE',  ( 5.367048706163317640, 7.354919138647580290, -1.599625672291281386 ) ) ;
#196345 = EDGE_CURVE ( 'NONE', #162762, #6079, #71339, .T. ) ;
#196344 = CYLINDRICAL_SURFACE ( 'NONE', #59639, 1.250000000000000000 ) ;
#196346 = CARTESIAN_POINT ( 'NONE',  ( 6.164714480961021259, 0.5753438643430182076, 1.717747506070513852 ) ) ;
#196347 = CARTESIAN_POINT ( 'NONE',  ( 6.414416072596830887, 8.576847732820027659, -1.443375672974078761 ) ) ;
#196348 = CARTESIAN_POINT ( 'NONE',  ( 0.000000000000000000, -4.000000000000003553, 0.000000000000000000 ) ) ;
#196349 = CARTESIAN_POINT ( 'NONE',  ( 2.677880624963273171, -1.125664371729949265, 1.880105217535378959 ) ) ;
#196351 = CARTESIAN_POINT ( 'NONE',  ( 8.106885785967500979, 11.54545161934907682, 1.199719254218460707 ) ) ;
#196350 = CARTESIAN_POINT ( 'NONE',  ( 6.127394093140170916, 0.1359088500606409067, -1.856169418941427729 ) ) ;
#196352 = CARTESIAN_POINT ( 'NONE',  ( 3.655789272196503514, 1.066996606607173659, 1.590710377612122750 ) ) ;
#196353 = CARTESIAN_POINT ( 'NONE',  ( 1.500000000000039524, 6.999999999999999112, 10.89724735885167561 ) ) ;
#196354 = ADVANCED_FACE ( 'NONE', ( #153271 ), #103461, .F. ) ;
#196355 = CARTESIAN_POINT ( 'NONE',  ( 0.2333690889706726279, 7.629137130509075604, -2.653349640194931247 ) ) ;
#196356 = CARTESIAN_POINT ( 'NONE',  ( 1.364683531249988757, 0.3843750003414206362, 0.000000000000000000 ) ) ;
#196357 = CARTESIAN_POINT ( 'NONE',  ( 4.961921032921539521, 7.772363057508363759, -1.082531754730549078 ) ) ;
#196358 = CARTESIAN_POINT ( 'NONE',  ( -9.002250809794000830, 11.52571191622492464, -1.443375672974059665 ) ) ;
#196359 = CARTESIAN_POINT ( 'NONE',  ( 1.534274790466340299, 1.065227450066742687, -1.880959520452238465 ) ) ;
#196360 = EDGE_CURVE ( 'NONE', #95942, #116100, #212479, .T. ) ;
#196361 = CARTESIAN_POINT ( 'NONE',  ( -5.743814354044916470, 6.730146830254374990, -1.199719254218453823 ) ) ;
#196362 = CARTESIAN_POINT ( 'NONE',  ( 3.867818961648523235, 7.734482231890414283, 1.040834085586084257E-14 ) ) ;
#196363 = CARTESIAN_POINT ( 'NONE',  ( 2.449991753796490368, 1.825138167369045661, 0.04731899098397300552 ) ) ;
#196364 = CARTESIAN_POINT ( 'NONE',  ( -4.548924232584923288, 5.265832011892554121, -1.199719254218446718 ) ) ;
#196365 = CARTESIAN_POINT ( 'NONE',  ( 3.873894609034499226, 1.013791609252197690, 1.518000939925365778 ) ) ;
#196366 = CARTESIAN_POINT ( 'NONE',  ( 9.681426354872456841, 13.43812210156014508, -8.165041025796162089 ) ) ;
#196367 = CARTESIAN_POINT ( 'NONE',  ( 2.478646075381494285, -1.315928518397539548, 1.387899491812602859 ) ) ;
#196368 = ORIENTED_EDGE ( 'NONE', *, *, #210558, .T. ) ;
#196369 = CARTESIAN_POINT ( 'NONE',  ( 4.264079249230395163, -1.964438661470244263, 0.1424843695872201332 ) ) ;
#196370 = ORIENTED_EDGE ( 'NONE', *, *, #40535, .F. ) ;
#196371 = CARTESIAN_POINT ( 'NONE',  ( 4.511236532831874868, -1.903902423773628838, 0.3822933785788319438 ) ) ;
#196372 = ORIENTED_EDGE ( 'NONE', *, *, #35863, .F. ) ;
#196373 = CARTESIAN_POINT ( 'NONE',  ( -5.589704470584107909, 9.743348658981940247, -0.7998128361456362523 ) ) ;
#196375 = CARTESIAN_POINT ( 'NONE',  ( 4.746395313581045272, 1.087821826000658909, -1.820160695957805608 ) ) ;
#196374 = CARTESIAN_POINT ( 'NONE',  ( 5.345657705538078730, 9.458627433094950021, 0.7998128361456331437 ) ) ;
#196376 = CARTESIAN_POINT ( 'NONE',  ( -0.07538891330676925073, -7.154544010627095219, 9.499700864329915007 ) ) ;
#196377 = CARTESIAN_POINT ( 'NONE',  ( 4.408913874118179699, 7.341020650511065782, -1.198271334459002802 ) ) ;
#196378 = CARTESIAN_POINT ( 'NONE',  ( -2.110982172923218325, 5.614562968385698127, -0.4421859227901755451 ) ) ;
#196379 = ORIENTED_EDGE ( 'NONE', *, *, #189556, .T. ) ;
#196380 = CARTESIAN_POINT ( 'NONE',  ( 5.065906673361608270, 5.939254536123854677, -1.199719254218450271 ) ) ;
#196381 = CARTESIAN_POINT ( 'NONE',  ( 4.660252114795294887, 6.460046772059735432, -1.599625672291256295 ) ) ;
#196382 = CARTESIAN_POINT ( 'NONE',  ( 3.598294619042395226, -0.9903900195140210583, 1.752531985089557098 ) ) ;
#196383 = CARTESIAN_POINT ( 'NONE',  ( -11.92046840572485777, 11.15252124794268695, 1.382231356234940867 ) ) ;
#196384 = CARTESIAN_POINT ( 'NONE',  ( 4.969292227364340953, 0.1756445257206709631, -1.817221496977147854 ) ) ;
#196385 = CARTESIAN_POINT ( 'NONE',  ( 1.152881054890652957, -0.5012615762394446728, -2.008655542368184221 ) ) ;
#196386 = CARTESIAN_POINT ( 'NONE',  ( -8.107412671292051343, 10.48173408797264194, 1.443375672974090751 ) ) ;
#196387 = CARTESIAN_POINT ( 'NONE',  ( -6.065932567686177279, 7.134227558401057934, 1.164772332933713184 ) ) ;
#196388 = CARTESIAN_POINT ( 'NONE',  ( 1.123270288254022198, 2.908552654332631437, -0.7749999999939810591 ) ) ;
#196389 = CARTESIAN_POINT ( 'NONE',  ( 5.893391625361731556, 1.417579469995243091, 1.220656814419220249 ) ) ;
#196390 = CARTESIAN_POINT ( 'NONE',  ( 5.587931867126699537, 9.671004278289832001, -0.7998128361456291469 ) ) ;
#196391 = CARTESIAN_POINT ( 'NONE',  ( -5.274285450916075035, 6.112086766612214284, 1.199719254218450271 ) ) ;
#196392 = CARTESIAN_POINT ( 'NONE',  ( 4.552840656090682891, 4.206068941727564514, 1.214306433183764966E-14 ) ) ;
#196393 = CARTESIAN_POINT ( 'NONE',  ( -1.364683531250010295, 9.942708333674728394, 0.7879004041258445001 ) ) ;
#196394 = CARTESIAN_POINT ( 'NONE',  ( -5.935772324684618795, 5.819489221753827657, 0.000000000000000000 ) ) ;
#196396 = CARTESIAN_POINT ( 'NONE',  ( -8.093291352714894415, 8.406871097780989288, -0.7998128361456362523 ) ) ;
#196395 = CARTESIAN_POINT ( 'NONE',  ( 7.173763318588945559, -6.681223591462591926, -7.173763318588971316 ) ) ;
#196397 = CARTESIAN_POINT ( 'NONE',  ( -5.473741331615264549, 7.409117525016355010, -1.599625672291256295 ) ) ;
#196398 = CARTESIAN_POINT ( 'NONE',  ( 1.358353136502856939, -2.070434559563800736, -0.003889755252693693176 ) ) ;
#196399 = CARTESIAN_POINT ( 'NONE',  ( 2.618900020153229757, 0.2622993368636802325, 2.100875384797147305 ) ) ;
#196400 = CARTESIAN_POINT ( 'NONE',  ( 9.589694723567584234, 10.08239868711733855, -0.7998128361456281477 ) ) ;
#196401 = CARTESIAN_POINT ( 'NONE',  ( -1.201851678989727383E-14, 3.493750000682815493, 1.732050807568877637 ) ) ;
#196402 = CARTESIAN_POINT ( 'NONE',  ( 0.6023233765659050665, 1.963792105354182249, 0.1503755929508752975 ) ) ;
#196403 = CARTESIAN_POINT ( 'NONE',  ( 4.765179230921094522, 7.000095391635957398, 1.399907146243694722 ) ) ;
#196404 = CARTESIAN_POINT ( 'NONE',  ( 4.039966587192257208, 6.696749537490852333, 1.082531754730558626 ) ) ;
#196406 = DIRECTION ( 'NONE',  ( -1.000000000000000000, 0.000000000000000000, 0.000000000000000000 ) ) ;
#196405 = CARTESIAN_POINT ( 'NONE',  ( -1.737499999999997824, -3.091666666666666341, 3.009438278150925683 ) ) ;
#196407 = CARTESIAN_POINT ( 'NONE',  ( 2.396762456488350956, 1.839990291603439632, -1.366890742103431755 ) ) ;
#196408 = CARTESIAN_POINT ( 'NONE',  ( 0.4865809202317071813, -0.2202831055867389420, -1.812292406919484344 ) ) ;
#196409 = CARTESIAN_POINT ( 'NONE',  ( 1.933716311909071006, -1.854087253938462521, 0.4680378644332866545 ) ) ;
#196410 = ORIENTED_EDGE ( 'NONE', *, *, #207563, .T. ) ;
#196411 = CARTESIAN_POINT ( 'NONE',  ( 7.253248993186724114, 9.485209796849769504, 1.443375672974076540 ) ) ;
#196412 = CARTESIAN_POINT ( 'NONE',  ( 1.635022589147613115, 1.879998146294536543, 0.7206230416607807276 ) ) ;
#196413 = CARTESIAN_POINT ( 'NONE',  ( 1.235121763443976395, -0.04261391538399812023, -1.961451400788959631 ) ) ;
#196414 = CARTESIAN_POINT ( 'NONE',  ( -9.806625181386236179, 10.33548422123910449, -0.7998128361456291469 ) ) ;
#196415 = EDGE_CURVE ( 'NONE', #129544, #93416, #36721, .T. ) ;
#196416 = CARTESIAN_POINT ( 'NONE',  ( -6.852756576703439961, 10.08230087520760954, 1.199719254218453823 ) ) ;
#196417 = CARTESIAN_POINT ( 'NONE',  ( -11.91110530558079006, 8.003273469779060179, -1.051614653808552013 ) ) ;
#196419 = CARTESIAN_POINT ( 'NONE',  ( 2.061070876156974041, 0.3059375065844106012, -1.743026645166842803 ) ) ;
#196418 = CARTESIAN_POINT ( 'NONE',  ( 3.626972257435066460, -1.931581639804475614, 0.8003350836045771688 ) ) ;
#196420 = EDGE_CURVE ( 'NONE', #7171, #89957, #202093, .T. ) ;
#196422 = CARTESIAN_POINT ( 'NONE',  ( 5.455124386806871506, 0.4517125544712205509, -2.247162937307800590 ) ) ;
#196421 = CARTESIAN_POINT ( 'NONE',  ( -10.91033749632886973, 4.885617943545219610, -4.996452313011736202 ) ) ;
#196423 = CARTESIAN_POINT ( 'NONE',  ( 4.206796582046585797, -0.2943472477981134428, 1.715077512146965688 ) ) ;
#196424 = CARTESIAN_POINT ( 'NONE',  ( 8.483651433849084711, 10.92067931095586886, 1.599625672291281386 ) ) ;
#196425 = CARTESIAN_POINT ( 'NONE',  ( 7.100579091573050228, -6.583980363594990948, -6.484567079770450881 ) ) ;
#196426 = CARTESIAN_POINT ( 'NONE',  ( 4.376141123711778214, -0.2964218048276610618, 1.708115672221988346 ) ) ;
#196427 = CARTESIAN_POINT ( 'NONE',  ( 4.387298408599741961, 0.1025060220480543544, 2.168864852262440301 ) ) ;
#196428 = CARTESIAN_POINT ( 'NONE',  ( 4.630273154266905777, 5.360739087188218122, 1.199719254218464037 ) ) ;
#196429 = CARTESIAN_POINT ( 'NONE',  ( 5.260953973667149342, -0.05432152012316109058, -2.015980820358989511 ) ) ;
#196430 = CARTESIAN_POINT ( 'NONE',  ( 0.2187500114561492792, -0.7852927567033060052, 1.895863743164095894 ) ) ;
#196431 = AXIS2_PLACEMENT_3D ( 'NONE', #80240, #13091, #197180 ) ;
#196432 = CARTESIAN_POINT ( 'NONE',  ( -1.201851678989727383E-14, 4.868750000682822154, -1.732050807568863648 ) ) ;
#196433 = CARTESIAN_POINT ( 'NONE',  ( 3.592722855893375478, -0.3746021097269113809, -1.889456300395859989 ) ) ;
#196434 = CARTESIAN_POINT ( 'NONE',  ( 1.500000000000001332, 10.15625000068279249, 0.000000000000000000 ) ) ;
#196435 = CARTESIAN_POINT ( 'NONE',  ( 5.484718290073375080, -1.409174384840453653, 1.717275654355006509 ) ) ;
#196436 = ORIENTED_EDGE ( 'NONE', *, *, #165975, .T. ) ;
#196437 = CARTESIAN_POINT ( 'NONE',  ( 6.883263157960373135, 2.058310207169287143, 2.252834201749584153 ) ) ;
#196438 = CARTESIAN_POINT ( 'NONE',  ( -1.201851678989727383E-14, 3.712500000000020339, 1.732050807568877637 ) ) ;
#196439 = CARTESIAN_POINT ( 'NONE',  ( 4.625302960556422427, 8.547937220624488575, 1.040834085586084257E-14 ) ) ;
#196440 = CARTESIAN_POINT ( 'NONE',  ( 1.295894383074674749, 2.050542657126565249, -0.8545418985851579441 ) ) ;
#196441 = CARTESIAN_POINT ( 'NONE',  ( 10.39230484541318589, 3.447199233515649386, -6.000000000000107470 ) ) ;
#196442 = CARTESIAN_POINT ( 'NONE',  ( 6.480434237652115570, 10.50433101066207442, 0.7216878364870438212 ) ) ;
#196443 = CARTESIAN_POINT ( 'NONE',  ( -8.473482818416657736, 12.82955435488738516, -0.7216878364870267237 ) ) ;
#196444 = CARTESIAN_POINT ( 'NONE',  ( 4.523580528814945545, 5.306540700819438960, 1.199719254218452047 ) ) ;
#196446 = AXIS2_PLACEMENT_3D ( 'NONE', #48275, #181435, #213911 ) ;
#196445 = MECHANICAL_DESIGN_GEOMETRIC_PRESENTATION_REPRESENTATION (  '', ( #6243 ), #16596 ) ;
#196447 = CARTESIAN_POINT ( 'NONE',  ( -4.014622883422336308, 5.777089012116397804, -1.443375672974066548 ) ) ;
#196449 = CARTESIAN_POINT ( 'NONE',  ( 3.842276591979614242, -1.019319043456867524, 1.793165911747495844 ) ) ;
#196448 = CARTESIAN_POINT ( 'NONE',  ( -15.75000000000000000, 11.29999999999999893, -0.7000000000000009548 ) ) ;
#196450 = CARTESIAN_POINT ( 'NONE',  ( -4.939248034080176097, 4.656877549381960080, 1.214306433183764966E-14 ) ) ;
#196451 = CARTESIAN_POINT ( 'NONE',  ( -1.500000000000011324, 4.702083334016148974, 0.8660254037844403729 ) ) ;
#196452 = CARTESIAN_POINT ( 'NONE',  ( 1.364683531249988757, -0.1156249996585798079, 0.000000000000000000 ) ) ;
#196453 = CARTESIAN_POINT ( 'NONE',  ( 6.766881895623299670, -1.710433013466134744, -0.7576501205904457859 ) ) ;
#196454 = CARTESIAN_POINT ( 'NONE',  ( 5.344279299745758216, 0.3302840285365048478, -1.702201177978326818 ) ) ;
#196455 = CARTESIAN_POINT ( 'NONE',  ( 4.774825072940077852, 1.621577360410943802, -0.6326411939767513370 ) ) ;
#196456 = CARTESIAN_POINT ( 'NONE',  ( 3.551346171775753735, 6.230655402791975384, 1.199719254218462483 ) ) ;
#196457 = CARTESIAN_POINT ( 'NONE',  ( 3.404133285375851248, -0.9304739769722850662, -2.095221664589861810 ) ) ;
#196458 = CARTESIAN_POINT ( 'NONE',  ( 1.364683531249990311, 4.926041667008083991, 0.7879004041258500513 ) ) ;
#196459 = CARTESIAN_POINT ( 'NONE',  ( 1.025062291269123405, -1.166378923895025510, -1.424538887614942739 ) ) ;
#196460 = EDGE_CURVE ( 'NONE', #118760, #49550, #106663, .T. ) ;
#196461 = CARTESIAN_POINT ( 'NONE',  ( 1.814759087649916003, 3.975067388631702059, -0.4606438099578838985 ) ) ;
#196462 = CARTESIAN_POINT ( 'NONE',  ( 1.606192798902779328, -0.6535759462080005244, -1.704761432720684144 ) ) ;
#196463 = CARTESIAN_POINT ( 'NONE',  ( 2.760388869050140137, 1.913803604375517109, -0.6351994527180188088 ) ) ;
#196464 = CARTESIAN_POINT ( 'NONE',  ( 1.447511513890851864, 0.6336015447323711802, -2.097855558553712640 ) ) ;
#196465 = CARTESIAN_POINT ( 'NONE',  ( 8.982121351223291583, 14.65570953369224050, -7.241029012671043930 ) ) ;
#196466 = CARTESIAN_POINT ( 'NONE',  ( 4.120224405726905736, -1.080582774747363306, -1.807441255628852828 ) ) ;
#196467 = CARTESIAN_POINT ( 'NONE',  ( -7.063961727919978451, 8.200042423116789436, 1.199719254218450271 ) ) ;
#196468 = CARTESIAN_POINT ( 'NONE',  ( 8.825981184337843288, 13.64596675382960100, 9.281099656089114802 ) ) ;
#196469 = CARTESIAN_POINT ( 'NONE',  ( 1.223191768902037957, -1.870915810643185795, -0.8869332102946840823 ) ) ;
#196470 = CARTESIAN_POINT ( 'NONE',  ( 5.301401758143367893, 6.143722458377430584, 1.199719254218462483 ) ) ;
#196471 = CARTESIAN_POINT ( 'NONE',  ( -1.953008978358306879E-14, -0.5156249996585442474, 1.570758158831760287 ) ) ;
#196472 = CARTESIAN_POINT ( 'NONE',  ( 3.633539341399088407, -0.1543397204060332761, 2.114911865293423787 ) ) ;
#196473 = CARTESIAN_POINT ( 'NONE',  ( -1.364683531250014514, 0.9885416670080898749, -0.7879004041258289570 ) ) ;
#196474 = CARTESIAN_POINT ( 'NONE',  ( 0.3813102713988948955, 1.798072043455358981, -0.6920631024385316410 ) ) ;
#196475 = ORIENTED_EDGE ( 'NONE', *, *, #65745, .F. ) ;
#196476 = CARTESIAN_POINT ( 'NONE',  ( -6.252245114557387851, 7.323316050852266557, -1.199719254218453823 ) ) ;
#196477 = CARTESIAN_POINT ( 'NONE',  ( 10.58621901417202515, 11.24501035948919991, -0.7998128361456281477 ) ) ;
#196478 = CARTESIAN_POINT ( 'NONE',  ( 6.333067150914808430, 8.481940657524365434, 1.443375672974063439 ) ) ;
#196479 = CARTESIAN_POINT ( 'NONE',  ( -1.737500000000000266, -3.514583332377418934, -3.009438278150923907 ) ) ;
#196480 = CARTESIAN_POINT ( 'NONE',  ( -7.040761844198392794, 7.108643661186573759, -0.7998128361456291469 ) ) ;
#196481 = CARTESIAN_POINT ( 'NONE',  ( 3.375264624815476289, -1.783316433176849625, -0.9482593927577113169 ) ) ;
#196482 = CARTESIAN_POINT ( 'NONE',  ( 0.9562493570349944738, 2.103547740682055966, -0.1031677049159150372 ) ) ;
#196483 = CARTESIAN_POINT ( 'NONE',  ( -6.306477729012051725, 7.386587434382707151, 1.199719254218452047 ) ) ;
#196484 = CARTESIAN_POINT ( 'NONE',  ( 9.413438726589914651, 9.876766690643398405, 0.000000000000000000 ) ) ;
#196485 = CARTESIAN_POINT ( 'NONE',  ( 5.506657433377460720, 0.5384353192533465338, 1.781376027434707687 ) ) ;
#196486 = CARTESIAN_POINT ( 'NONE',  ( 8.239604668803105270, 10.63595808506888396, -1.599625672291268286 ) ) ;
#196487 = CARTESIAN_POINT ( 'NONE',  ( -1.264911064067348656, 3.850000000000018296, 0.5000000000000064393 ) ) ;
#196488 = CARTESIAN_POINT ( 'NONE',  ( -9.571693261567968847, 12.19006144329456731, 1.443375672974076540 ) ) ;
#196489 = CARTESIAN_POINT ( 'NONE',  ( -6.157374318900681764, 10.33535380535947290, 0.7998128361456481317 ) ) ;
#196490 = CARTESIAN_POINT ( 'NONE',  ( 0.08116279290028630133, -0.1557560750096824431, -2.127278773206460638 ) ) ;
#196492 = CARTESIAN_POINT ( 'NONE',  ( -4.338283617754775889, 7.407916770541659091, 1.160293660280581785 ) ) ;
#196491 = CARTESIAN_POINT ( 'NONE',  ( -6.622231685632140596, 6.690634819517756959, 0.000000000000000000 ) ) ;
#196493 = CARTESIAN_POINT ( 'NONE',  ( -1.364683531250000748, 0.7593750003414210248, 0.000000000000000000 ) ) ;
#196494 = CARTESIAN_POINT ( 'NONE',  ( 2.407222047678575283, 0.3756278383273171095, 1.692465640204628974 ) ) ;
#196495 = CARTESIAN_POINT ( 'NONE',  ( 1.060061488152568510, -1.571881217706198042, -0.7472303940359821262 ) ) ;
#196497 = CARTESIAN_POINT ( 'NONE',  ( 7.958272981541723468, 8.386999354661243800, 1.040834085586084257E-14 ) ) ;
#196496 = CARTESIAN_POINT ( 'NONE',  ( 6.112023189137078205, -2.291079414021851779, 0.2760875835842706016 ) ) ;
#196498 = CARTESIAN_POINT ( 'NONE',  ( -10.93359526636954193, 4.740328704497578372, 4.433404364989353752 ) ) ;
#196499 = CARTESIAN_POINT ( 'NONE',  ( 2.600915689618611193, 1.657045147975671817, -1.224973224035642794 ) ) ;
#196500 = CARTESIAN_POINT ( 'NONE',  ( 3.818592820543298405, 7.606775390609172405, -0.7998128361456221525 ) ) ;
#196501 = STYLED_ITEM ( 'NONE', ( #212568 ), #152368 ) ;
#196502 = CARTESIAN_POINT ( 'NONE',  ( 1.089219988750099732, 1.203171814842165288, -1.617568698395126292 ) ) ;
#196503 = CARTESIAN_POINT ( 'NONE',  ( 1.249999999999997558, -0.5000000000000004441, 1.734723475976807094E-15 ) ) ;
#196504 = CARTESIAN_POINT ( 'NONE',  ( -5.960744811863571968, 6.983232364376142698, 1.199719254218452935 ) ) ;
#196505 = CARTESIAN_POINT ( 'NONE',  ( 0.7253841367629434433, -1.872807053274931244, 0.6160819575430801498 ) ) ;
#196507 = CARTESIAN_POINT ( 'NONE',  ( -5.478903473698247595, 8.445785581739666981, -1.082531754730549967 ) ) ;
#196506 = CARTESIAN_POINT ( 'NONE',  ( 4.500206361630255003, -0.8965733778899236395, 1.689174240301967389 ) ) ;
#196508 = CARTESIAN_POINT ( 'NONE',  ( 5.865903189996044098, 2.174886565178067777, -0.3735607071253948530 ) ) ;
#196509 = CARTESIAN_POINT ( 'NONE',  ( -7.580417283372126391, 8.016444050121833698, 0.7216878364870317197 ) ) ;
#196510 = CARTESIAN_POINT ( 'NONE',  ( 7.147083253059300922, 8.367293879104554577, 1.199719254218452935 ) ) ;
#196511 = CARTESIAN_POINT ( 'NONE',  ( -7.957709816578236506, 8.248692638954882028, 0.7998128361456341429 ) ) ;
#196512 = CARTESIAN_POINT ( 'NONE',  ( 6.639320575229281651, -0.0007625845807879281287, 2.103388539994067497 ) ) ;
#196513 = CARTESIAN_POINT ( 'NONE',  ( -1.201851678989727383E-14, 4.118750000682818602, -1.732050807568863648 ) ) ;
#196514 = CARTESIAN_POINT ( 'NONE',  ( 4.717980713983113361, -2.264103904663441913, 0.4450920570577068247 ) ) ;
#196515 = CARTESIAN_POINT ( 'NONE',  ( 5.723093114104088386, -1.772945450647535948, -0.8403097561825512152 ) ) ;
#196516 = CARTESIAN_POINT ( 'NONE',  ( 2.008577182894935476, 0.6104510041588117053, 1.864461945915835583 ) ) ;
#196517 = DIRECTION ( 'NONE',  ( 0.6507913734559658270, -0.7592566023652989049, 0.000000000000000000 ) ) ;
#196518 = CARTESIAN_POINT ( 'NONE',  ( -9.437944175107181977, 14.51387423797986642, 7.411204044495644183 ) ) ;
#196519 = ORIENTED_EDGE ( 'NONE', *, *, #178101, .F. ) ;
#196520 = CARTESIAN_POINT ( 'NONE',  ( 0.4095560439901060334, -2.008447366592306604, 0.6704124886842844910 ) ) ;
#196522 = CARTESIAN_POINT ( 'NONE',  ( -6.008234629150358330, 10.16135750065076060, 0.000000000000000000 ) ) ;
#196521 = CARTESIAN_POINT ( 'NONE',  ( -4.924636110261798372, 6.768494766770632332, 1.599625672291267398 ) ) ;
#196523 = CARTESIAN_POINT ( 'NONE',  ( 0.8140990769837241903, 1.700254657383608814, 0.7068247239481674216 ) ) ;
#196524 = ORIENTED_EDGE ( 'NONE', *, *, #202148, .F. ) ;
#196525 = CARTESIAN_POINT ( 'NONE',  ( 3.819318941869216388, -1.912159422281418220, -1.028266076255865968 ) ) ;
#196526 = CARTESIAN_POINT ( 'NONE',  ( 11.28784473853554537, 8.874586039915849156, -4.090552291126032358 ) ) ;
#196527 = CARTESIAN_POINT ( 'NONE',  ( 1.846092968827160119, -1.388944967848893430, -1.602481653760478020 ) ) ;
#196528 = CARTESIAN_POINT ( 'NONE',  ( -1.201851678989727383E-14, 3.368750000682815049, -1.732050807568863648 ) ) ;
#196529 = CARTESIAN_POINT ( 'NONE',  ( 7.781490099239519509, 11.16582331816642260, 1.199719254218460707 ) ) ;
#196530 = CARTESIAN_POINT ( 'NONE',  ( -1.842580630436563949, 2.498881177628073491, -2.492971354622253610 ) ) ;
#196531 = MECHANICAL_DESIGN_GEOMETRIC_PRESENTATION_REPRESENTATION (  '', ( #206871 ), #51345 ) ;
#196532 = CARTESIAN_POINT ( 'NONE',  ( 3.743479925124373331, -1.557965094614376378, -1.348979221448711519 ) ) ;
#196534 = CARTESIAN_POINT ( 'NONE',  ( 0.8195642880178370948, 1.096917009463085790, -1.478703137254427924 ) ) ;
#196533 = CARTESIAN_POINT ( 'NONE',  ( -9.189729191964438826, 9.615772233580322848, 1.040834085586084257E-14 ) ) ;
#196535 = CARTESIAN_POINT ( 'NONE',  ( 1.364683531249988535, 2.905208333674754506, -0.7879004041258239610 ) ) ;
#196536 = CARTESIAN_POINT ( 'NONE',  ( 3.929058411375439874, -1.000000000000000888, -0.7500000000000006661 ) ) ;
#196537 = DIRECTION ( 'NONE',  ( 0.000000000000000000, 0.000000000000000000, -1.000000000000000000 ) ) ;
#196538 = CARTESIAN_POINT ( 'NONE',  ( -0.02244404828157658613, -0.004869073801674199918, -2.189079685368473527 ) ) ;
#196539 = CARTESIAN_POINT ( 'NONE',  ( 1.230147817042701375, -1.435374304221140651, -1.748800500726248153 ) ) ;
#196540 = CARTESIAN_POINT ( 'NONE',  ( -10.31739171031960822, 11.13930453823545186, 1.040834085586084257E-14 ) ) ;
#196541 = CARTESIAN_POINT ( 'NONE',  ( 1.248006495514828895, 0.8912474588982389756, -1.577060073313638622 ) ) ;
#196542 = EDGE_CURVE ( 'NONE', #97523, #147312, #213118, .T. ) ;
#196543 = CARTESIAN_POINT ( 'NONE',  ( 1.516650397601801759, 0.1914660871255029484, 1.906153142492900132 ) ) ;
#196544 = CARTESIAN_POINT ( 'NONE',  ( 2.963400493335893948, 1.747644659881589568, 1.109742091278065113 ) ) ;
#196545 = CARTESIAN_POINT ( 'NONE',  ( -0.6823417656250212460, 1.613541667008083769, 1.181850606188755259 ) ) ;
#196546 = CARTESIAN_POINT ( 'NONE',  ( 1.340630715518615679, 0.3825088487559283323, 1.933841885654476567 ) ) ;
#196547 = CARTESIAN_POINT ( 'NONE',  ( 5.162690889178682241, -1.394081347390314640, 1.329872870702011545 ) ) ;
#196549 = CARTESIAN_POINT ( 'NONE',  ( 6.229241538080760421, 6.920885192246182704, -0.8282608007674150397 ) ) ;
#196548 = CARTESIAN_POINT ( 'NONE',  ( 0.8566255916394946990, 2.304767657353411270, -0.1186049529825431298 ) ) ;
#196550 = CARTESIAN_POINT ( 'NONE',  ( -1.364683531250012516, 3.238541667008084879, -0.7879004041258289570 ) ) ;
#196551 = CARTESIAN_POINT ( 'NONE',  ( 5.459457826130150515, 1.684308464339222100, 1.190431669587647567 ) ) ;
#196552 = CARTESIAN_POINT ( 'NONE',  ( -5.117312914154178216, 8.057616602233474978, -1.199719254218452047 ) ) ;
#196553 = CARTESIAN_POINT ( 'NONE',  ( 10.97011102005664185, 13.79999999999998472, 1.696376167609456198 ) ) ;
#196554 =( BOUNDED_SURFACE ( )  B_SPLINE_SURFACE ( 3, 2, ( 
 ( #152726, #149534, #101845 ),
 ( #136495, #2176, #203582 ),
 ( #84526, #170034, #54166 ),
 ( #137565, #186279, #119223 ),
 ( #21620, #35771, #168974 ),
 ( #55234, #4307, #120304 ),
 ( #37916, #71452, #183090 ),
 ( #103990, #121381, #3247 ),
 ( #150615, #133319, #38984 ),
 ( #166853, #87728, #19512 ) ),
 .UNSPECIFIED., .F., .F., .T. ) 
 B_SPLINE_SURFACE_WITH_KNOTS ( ( 4, 2, 2, 2, 4 ),
 ( 3, 3 ),
 ( 0.000000000000000000, 0.0004557710599321653476, 0.0009115421198643306952, 0.001367313179796496043, 0.001823084239728661390 ),
 ( 0.000000000000000000, 1.000000000000000000 ),
 .UNSPECIFIED. ) 
 GEOMETRIC_REPRESENTATION_ITEM ( )  RATIONAL_B_SPLINE_SURFACE ( (
 ( 1.000000000000000000, 0.5613739026647618369, 1.000000000000000000),
 ( 1.000000000000000000, 0.5542214518087537067, 1.000000000000000000),
 ( 1.000000000000000000, 0.5635694824811526837, 1.000000000000000000),
 ( 1.000000000000000000, 0.6084377562511148474, 1.000000000000000000),
 ( 1.000000000000000000, 0.6447860777916630814, 1.000000000000000000),
 ( 1.000000000000000000, 0.7192854197611785461, 1.000000000000000000),
 ( 1.000000000000000000, 0.7560301986938927632, 1.000000000000000000),
 ( 1.000000000000000000, 0.8079200278152608439, 1.000000000000000000),
 ( 1.000000000000000000, 0.8228378482302226571, 1.000000000000000000),
 ( 1.000000000000000000, 0.8275596917170975342, 1.000000000000000000) ) ) 
 REPRESENTATION_ITEM ( '' )  SURFACE ( )  );
#196555 = CARTESIAN_POINT ( 'NONE',  ( 6.106491565043327796, -0.7546634490227432934, -1.966289716088761796 ) ) ;
#196556 = CARTESIAN_POINT ( 'NONE',  ( -0.6823417656250003738, 3.030208333674754062, -1.181850606188749264 ) ) ;
#196557 = CARTESIAN_POINT ( 'NONE',  ( 5.132170659515546518, 1.116069247042193124, -1.851066442873222639 ) ) ;
#196558 = CARTESIAN_POINT ( 'NONE',  ( 0.9250624443557056154, -1.167992581197497604, -1.423340509374780405 ) ) ;
#196559 = CARTESIAN_POINT ( 'NONE',  ( 5.004559639922408820, -2.004681531738555123, -0.2449335584770311880 ) ) ;
#196560 = CARTESIAN_POINT ( 'NONE',  ( -0.8775925178581088781, 2.800000000000024691, 1.062197627458028260 ) ) ;
#196561 = CARTESIAN_POINT ( 'NONE',  ( -6.087247782855839340, 6.204136622861004646, 0.000000000000000000 ) ) ;
#196562 = ADVANCED_FACE ( 'NONE', ( #2725 ), #150090, .F. ) ;
#196565 = CARTESIAN_POINT ( 'NONE',  ( 4.528060117284232966, 6.305822774963486310, 1.443375672974062551 ) ) ;
#196564 = CARTESIAN_POINT ( 'NONE',  ( 1.642778471875001811, -2.442708332855377140, 2.845375778867859751 ) ) ;
#196563 = CARTESIAN_POINT ( 'NONE',  ( -7.093554249807959344, 14.55189866933985421, -9.633885861679724272 ) ) ;
#196566 = CARTESIAN_POINT ( 'NONE',  ( -3.980200614063634568, 6.801261928786307642, 1.199719254218452935 ) ) ;
#196567 = CARTESIAN_POINT ( 'NONE',  ( 3.257046257486408969, 0.04465439498414420366, -2.016188763087948033 ) ) ;
#196568 = CARTESIAN_POINT ( 'NONE',  ( -6.516665389662827934, 10.75452672124865217, 0.000000000000000000 ) ) ;
#196570 = CARTESIAN_POINT ( 'NONE',  ( -10.96785329849814161, -5.223431457505069098, 0.4373225248172953883 ) ) ;
#196569 = CARTESIAN_POINT ( 'NONE',  ( -4.115063316947640715, 4.759660943649018705, 1.199719254218462483 ) ) ;
#196571 = CARTESIAN_POINT ( 'NONE',  ( -15.75000000000000000, 10.89999999999998259, 1.799999999999999600 ) ) ;
#196573 = CARTESIAN_POINT ( 'NONE',  ( -8.012344526598182026E-15, 9.546875000341396245, -1.575800808251669460 ) ) ;
#196572 = CARTESIAN_POINT ( 'NONE',  ( 4.944278945467968533, 2.155654431248493985, 0.1625706239713892443 ) ) ;
#196574 = FILL_AREA_STYLE_COLOUR ( '', #82736 ) ;
#196575 = CARTESIAN_POINT ( 'NONE',  ( -11.91093491413953309, 8.002894165250459935, -1.053637727194525642 ) ) ;
#196577 = CARTESIAN_POINT ( 'NONE',  ( 5.501577430365036214, -1.966641501487207622, 0.4445218866586594930 ) ) ;
#196576 = CARTESIAN_POINT ( 'NONE',  ( -5.544921637864824504, 8.452530429942200385, -1.082531754730543971 ) ) ;
#196578 = CARTESIAN_POINT ( 'NONE',  ( -1.364683531250014514, 0.09270833367475767028, 0.7879004041258379498 ) ) ;
#196579 = CARTESIAN_POINT ( 'NONE',  ( 1.382971869717847690, 1.594974721182834010, -0.6572114825635144708 ) ) ;
#196580 = CARTESIAN_POINT ( 'NONE',  ( 4.064412189046650248, 7.963840997188264659, 0.7998128361456271485 ) ) ;
#196582 = CARTESIAN_POINT ( 'NONE',  ( 5.169401708560450004, 9.252995436621013425, 0.000000000000000000 ) ) ;
#196581 = CARTESIAN_POINT ( 'NONE',  ( 6.724481002698112775, 8.868313807946373473, -1.443375672974057666 ) ) ;
#196583 = CARTESIAN_POINT ( 'NONE',  ( -10.49167095263961613, 5.343775707538775066, -5.730694126968514546 ) ) ;
#196584 = CARTESIAN_POINT ( 'NONE',  ( 0.3327835722091445070, -1.621720136574826610, 0.7089735832957798634 ) ) ;
#196585 = CARTESIAN_POINT ( 'NONE',  ( 0.7506400166778016692, 1.983664654656223991, 0.3420602577784581655 ) ) ;
#196586 = DIRECTION ( 'NONE',  ( -0.000000000000000000, -1.000000000000000000, -0.000000000000000000 ) ) ;
#196587 = CARTESIAN_POINT ( 'NONE',  ( 3.276612781706738087, -1.315965827422488132, 1.771305981150771647 ) ) ;
#196588 = CARTESIAN_POINT ( 'NONE',  ( 4.891568528303794849, -1.987603774517988642, 0.8738605845971869623 ) ) ;
#196589 = VERTEX_POINT ( 'NONE', #71997 ) ;
#196590 = CARTESIAN_POINT ( 'NONE',  ( 9.205623113554624481, 10.80261038964432707, 1.082531754730549967 ) ) ;
#196592 = CARTESIAN_POINT ( 'NONE',  ( 1.915638884950950027, -1.319244919589783516, -1.525031147761625405 ) ) ;
#196591 = CARTESIAN_POINT ( 'NONE',  ( 2.262495435604610527, 2.120074037919957632, 0.04929290001921824566 ) ) ;
#196594 = ORIENTED_EDGE ( 'NONE', *, *, #20726, .T. ) ;
#196593 = CARTESIAN_POINT ( 'NONE',  ( 1.792921450925293536, -0.09139298786187435852, -1.809423198457478676 ) ) ;
#196595 = CARTESIAN_POINT ( 'NONE',  ( 6.723917837734620484, 6.809268663637336516, 0.000000000000000000 ) ) ;
#196596 = CARTESIAN_POINT ( 'NONE',  ( 6.636879889089462026, 7.701780277814560982, -1.199719254218446718 ) ) ;
#196598 = CARTESIAN_POINT ( 'NONE',  ( 1.745192250125559008, 0.3234662751879986975, -1.888026716711376674 ) ) ;
#196597 = CARTESIAN_POINT ( 'NONE',  ( -4.440459003675619520, 5.139289244831666714, 1.199719254218462483 ) ) ;
#196600 = CIRCLE ( 'NONE', #65155, 0.09999999999999982514 ) ;
#196599 = VECTOR ( 'NONE', #154608, 1000.000000000000114 ) ;
#196601 = CARTESIAN_POINT ( 'NONE',  ( -1.523611765266693174, 0.5999999999999998668, 1.789163823896770200 ) ) ;
#196602 = CARTESIAN_POINT ( 'NONE',  ( 9.611339018008546731, -6.606549254265010163, -0.3046331935817545578 ) ) ;
#196603 = CARTESIAN_POINT ( 'NONE',  ( 4.473827502385202770, 8.163289819517311585, 1.040834085586084257E-14 ) ) ;
#196604 = EDGE_CURVE ( 'NONE', #207604, #185122, #168320, .T. ) ;
#196605 = CARTESIAN_POINT ( 'NONE',  ( 0.6823417656249882723, 0.7385416670080829915, -1.181850606188749264 ) ) ;
#196606 = DIRECTION ( 'NONE',  ( 0.000000000000000000, 1.000000000000000000, 0.000000000000000000 ) ) ;
#196607 = CARTESIAN_POINT ( 'NONE',  ( -9.820183334999905256, 10.35130206712171130, 1.040834085586084257E-14 ) ) ;
#196608 = CARTESIAN_POINT ( 'NONE',  ( 4.733375416736937069, -1.977748744329570263, 0.8730265686548792647 ) ) ;
#196609 = EDGE_CURVE ( 'NONE', #4315, #4590, #149821, .T. ) ;
#196610 = CARTESIAN_POINT ( 'NONE',  ( -6.482206841109545259, 6.735198534148810090, 0.7216878364870257245 ) ) ;
#196611 = CARTESIAN_POINT ( 'NONE',  ( 6.075462232699553766, 6.260663157670496304, -0.7216878364870458196 ) ) ;
#196612 = CARTESIAN_POINT ( 'NONE',  ( 1.441811196653530747, -1.994930912159533554, 0.7194735443712959588 ) ) ;
#196613 = CARTESIAN_POINT ( 'NONE',  ( -0.1298852118744101003, 4.098067735550426249, -2.281510303361510061 ) ) ;
#196614 = CARTESIAN_POINT ( 'NONE',  ( 2.759003776822867238, -1.713332664616385781, -0.9749793123631170788 ) ) ;
#196615 = CARTESIAN_POINT ( 'NONE',  ( 5.150612376422202487, 1.885107930906554152, 0.3209214958604587054 ) ) ;
#196616 = ORIENTED_EDGE ( 'NONE', *, *, #157243, .T. ) ;
#196617 = CARTESIAN_POINT ( 'NONE',  ( 1.499999999999974909, 4.545833333333353821, -0.8660254037844394848 ) ) ;
#196618 = CARTESIAN_POINT ( 'NONE',  ( 0.2915762745691782287, -1.893489616766583339, 0.8377075429084477332 ) ) ;
#196619 = CARTESIAN_POINT ( 'NONE',  ( 2.044773883198697462, -1.559800846558807130, -1.156617037343915966 ) ) ;
#196620 = ORIENTED_EDGE ( 'NONE', *, *, #69925, .T. ) ;
#196621 = CARTESIAN_POINT ( 'NONE',  ( -0.5000000000000091038, 3.949999999999960654, 0.3999999999999455103 ) ) ;
#196623 = CARTESIAN_POINT ( 'NONE',  ( -2.736367132584055707E-14, -7.616807913964303900, 10.09384657274620523 ) ) ;
#196622 = CARTESIAN_POINT ( 'NONE',  ( -6.509323148336870091, 7.727203440215372865, 1.082531754730549078 ) ) ;
#196625 = CARTESIAN_POINT ( 'NONE',  ( 7.820355676984174664, 8.018169799436671852, -0.7998128361456281477 ) ) ;
#196624 = CARTESIAN_POINT ( 'NONE',  ( 2.625039678221803729, -1.950394636745816701, 0.7532777691767779116 ) ) ;
#196626 = CARTESIAN_POINT ( 'NONE',  ( 5.899206235277530297, 7.015400374979486209, -1.082531754730548412 ) ) ;
#196628 = ORIENTED_EDGE ( 'NONE', *, *, #31081, .T. ) ;
#196627 = CARTESIAN_POINT ( 'NONE',  ( 5.865855438783555087, 0.5507134639845879809, -1.831277125143706552 ) ) ;
#196629 = CARTESIAN_POINT ( 'NONE',  ( 4.231241840954825584, 0.1069408422738199749, 2.204416794138922331 ) ) ;
#196630 = CARTESIAN_POINT ( 'NONE',  ( 2.538337413235943973, 1.040872164564849767, -1.945885072647230318 ) ) ;
#196631 = CARTESIAN_POINT ( 'NONE',  ( -0.3636750363432391664, -6.893137084989841235, -10.99449589488467183 ) ) ;
#196632 = CARTESIAN_POINT ( 'NONE',  ( 1.629408300089076889, -0.2329066467734330903, 1.897959532673603844 ) ) ;
#196633 =( BOUNDED_SURFACE ( )  B_SPLINE_SURFACE ( 3, 2, ( 
 ( #84385, #151533, #86518 ),
 ( #150472, #68102, #181865 ),
 ( #134238, #51896, #118019 ),
 ( #98510, #184008, #3101 ),
 ( #186137, #69172, #202374 ),
 ( #164572, #152583, #75609 ),
 ( #9535, #173126, #22565 ),
 ( #73462, #42063, #141720 ) ),
 .UNSPECIFIED., .F., .F., .T. ) 
 B_SPLINE_SURFACE_WITH_KNOTS ( ( 4, 2, 2, 4 ),
 ( 3, 3 ),
 ( 0.000000000000000000, 0.003124171923498968943, 0.004686257885248453631, 0.006248343846997937885 ),
 ( 0.000000000000000000, 1.000000000000000000 ),
 .UNSPECIFIED. ) 
 GEOMETRIC_REPRESENTATION_ITEM ( )  RATIONAL_B_SPLINE_SURFACE ( (
 ( 1.000000000000000000, 0.7762074382822432561, 1.000000000000000000),
 ( 1.000000000000000000, 0.7833327749266361106, 1.000000000000000000),
 ( 1.000000000000000000, 0.7920843030290980469, 1.000000000000000000),
 ( 1.000000000000000000, 0.8126253899334039410, 1.000000000000000000),
 ( 1.000000000000000000, 0.8207498793991692132, 1.000000000000000000),
 ( 1.000000000000000000, 0.8408199112011192078, 1.000000000000000000),
 ( 1.000000000000000000, 0.8529121798795707976, 1.000000000000000000),
 ( 1.000000000000000000, 0.8665632151524114146, 1.000000000000000000) ) ) 
 REPRESENTATION_ITEM ( '' )  SURFACE ( )  );
#196634 = CARTESIAN_POINT ( 'NONE',  ( -5.093612336809997920, 4.836969235900084207, -0.4916062289654357098 ) ) ;
#196635 = CARTESIAN_POINT ( 'NONE',  ( 10.72180055030867329, 11.40318881831530540, 0.7998128361456341429 ) ) ;
#196636 = CARTESIAN_POINT ( 'NONE',  ( 4.545415791725802457, 1.850806902094417783, -0.9279678557222793556 ) ) ;
#196638 = CARTESIAN_POINT ( 'NONE',  ( 1.253037233087474611, -1.703760181015579134, 1.330383891403746688 ) ) ;
#196637 = CARTESIAN_POINT ( 'NONE',  ( 0.06814526087292921419, -6.511064858252400001, 10.88932262995847822 ) ) ;
#196639 = CARTESIAN_POINT ( 'NONE',  ( 3.913774547416096095, -1.127657808996849198, -1.879056921112078893 ) ) ;
#196640 = LINE ( 'NONE', #2664, #6935 ) ;
#196641 = AXIS2_PLACEMENT_3D ( 'NONE', #81295, #82343, #77287 ) ;
#196642 = FACE_OUTER_BOUND ( 'NONE', #137749, .T. ) ;
#196643 = CARTESIAN_POINT ( 'NONE',  ( -0.008622056139523381901, 15.44694768828586540, 11.95585894197802013 ) ) ;
#196644 = CARTESIAN_POINT ( 'NONE',  ( -0.6823417656250003738, 14.96354166700806410, 1.181850606188754593 ) ) ;
#196645 = CARTESIAN_POINT ( 'NONE',  ( -5.503684012504701961, 5.385662534202396934, 0.000000000000000000 ) ) ;
#196646 = CARTESIAN_POINT ( 'NONE',  ( 6.604150274805285825, -0.1349072972122930258, 1.703313905121685456 ) ) ;
#196647 = CARTESIAN_POINT ( 'NONE',  ( -8.622622508611375025, 12.04318144581317895, 1.082531754730560403 ) ) ;
#196648 = CARTESIAN_POINT ( 'NONE',  ( 4.469627305733424372, -0.3590069766891256231, 2.038746214588673666 ) ) ;
#196649 = CARTESIAN_POINT ( 'NONE',  ( 3.598194957300792307, -1.924334687528261201, -0.09379112422614949152 ) ) ;
#196650 = CARTESIAN_POINT ( 'NONE',  ( 5.448860601978118723, -1.914358274237770496, -0.9046119500179942152 ) ) ;
#196651 = CARTESIAN_POINT ( 'NONE',  ( 6.173040012923759257, 6.096301524699504704, -0.7998128361456281477 ) ) ;
#196652 = CARTESIAN_POINT ( 'NONE',  ( 9.444297818688886181, 3.530917896769821152, 7.404075800242620353 ) ) ;
#196653 = CARTESIAN_POINT ( 'NONE',  ( 3.819166351039466001, -1.734870831597424612, -0.9322225710242746377 ) ) ;
#196654 = CARTESIAN_POINT ( 'NONE',  ( 6.298803545911215274, 1.902247386433516541, 1.278772944020603930 ) ) ;
#196655 = CARTESIAN_POINT ( 'NONE',  ( 4.283705427790140519, 1.194290084605063251, 1.380960126487425166 ) ) ;
#196656 = CARTESIAN_POINT ( 'NONE',  ( 3.217027588192558074, 6.975225629525113824, -1.734723475976807094E-15 ) ) ;
#196657 = CARTESIAN_POINT ( 'NONE',  ( 5.314433026432511475, 5.302519407033794430, 1.040834085586084257E-14 ) ) ;
#196658 = CARTESIAN_POINT ( 'NONE',  ( -5.932574734431526942, 9.079031735882207244, 1.199719254218454489 ) ) ;
#196659 = CARTESIAN_POINT ( 'NONE',  ( 6.367489420273535039, 7.457767740854454708, -1.199719254218452047 ) ) ;
#196660 = ORIENTED_EDGE ( 'NONE', *, *, #202477, .T. ) ;
#196661 = CARTESIAN_POINT ( 'NONE',  ( 4.939702229944241907, -1.910329301133410151, 0.6354416197995541582 ) ) ;
#196662 = CARTESIAN_POINT ( 'NONE',  ( 0.2987795159231512176, -2.099866535080958663, 0.9347484894880775386 ) ) ;
#196663 = CARTESIAN_POINT ( 'NONE',  ( 4.469553177461598636, -0.3394721387663233170, 1.932013773527320843 ) ) ;
#196664 = CARTESIAN_POINT ( 'NONE',  ( -6.775324078527193983, 8.927630729746953264, -1.599625672291263179 ) ) ;
#196666 = CARTESIAN_POINT ( 'NONE',  ( -3.100010679019018500, 6.768429558830820980, 1.040834085586084257E-14 ) ) ;
#196665 = B_SPLINE_CURVE_WITH_KNOTS ( 'NONE', 3,
 ( #209627, #80723, #61268, #127429, #163049, #210709, #112225, #79648, #145764, #193399 ),
 .UNSPECIFIED., .F., .F.,
 ( 4, 3, 3, 4 ),
 ( 0.000000000000000000, 0.0001748246942969784896, 0.0003306242286995172888, 0.0004873602920373641223 ),
 .UNSPECIFIED. ) ;
#196667 = CARTESIAN_POINT ( 'NONE',  ( 0.000000000000000000, 2.800000000000024691, 1.214306433183764966E-14 ) ) ;
#196668 = CARTESIAN_POINT ( 'NONE',  ( -4.773352600463090845, 7.726605912919016106, 1.199719254218452935 ) ) ;
#196670 = CARTESIAN_POINT ( 'NONE',  ( 6.666889860676148416, -1.620333765578816587, -0.7124167289687727278 ) ) ;
#196669 = CARTESIAN_POINT ( 'NONE',  ( 0.6618065864371965867, 1.033746398093362773, 1.817239694416083795 ) ) ;
#196671 = CARTESIAN_POINT ( 'NONE',  ( -0.3977480831933914440, 3.051780253777475860, 2.024501290749185056 ) ) ;
#196672 = CARTESIAN_POINT ( 'NONE',  ( 6.228462243142912413, 0.1929387083638624822, 1.932343765256574697 ) ) ;
#196673 = CARTESIAN_POINT ( 'NONE',  ( -0.1102773484824119132, 0.6802821481026833927, -2.283667859588431881 ) ) ;
#196674 = CARTESIAN_POINT ( 'NONE',  ( 1.258879523317941285, 1.714807473692409268, -0.2965960235774521836 ) ) ;
#196675 = AXIS2_PLACEMENT_3D ( 'NONE', #86252, #20165, #35357 ) ;
#196676 = CARTESIAN_POINT ( 'NONE',  ( 4.950698647284403009, 8.927565521807144577, 1.040834085586084257E-14 ) ) ;
#196677 = DIRECTION ( 'NONE',  ( 1.000000000000000000, 0.000000000000000000, -1.465138070926357285E-17 ) ) ;
#196678 = CARTESIAN_POINT ( 'NONE',  ( 1.382971869717847690, 1.594974721182834010, -0.6572114825635144708 ) ) ;
#196679 = CARTESIAN_POINT ( 'NONE',  ( 1.751786407749492014, 2.185395279939935431, -0.1653414253460702699 ) ) ;
#196680 = CARTESIAN_POINT ( 'NONE',  ( 6.889999999999967706, 0.005249217920031550542, 1.719840535937327664 ) ) ;
#196681 = CARTESIAN_POINT ( 'NONE',  ( 4.301547675229603129, 1.771612934706376707, 1.315755017190944676 ) ) ;
#196682 = CARTESIAN_POINT ( 'NONE',  ( 1.534277631021633059, 1.291084678180357104, 1.745351423456573015 ) ) ;
#196683 = CARTESIAN_POINT ( 'NONE',  ( 0.2404813148422607627, 0.3085585699703840556, 1.799268721412583316 ) ) ;
#196684 = CARTESIAN_POINT ( 'NONE',  ( 2.518900147204519158, 0.2643050731806431686, 2.100751150841919657 ) ) ;
#196685 = CARTESIAN_POINT ( 'NONE',  ( 6.773846765317307117, -7.246166700180829423, -6.773846765317326657 ) ) ;
#196686 = VERTEX_POINT ( 'NONE', #125134 ) ;
#196687 = TOROIDAL_SURFACE ( 'NONE', #92967, 6.500000000000000000, 0.2999999999999999889 ) ;
#196689 = CARTESIAN_POINT ( 'NONE',  ( -1.364683531250014514, 0.09270833367475767028, 0.7879004041258379498 ) ) ;
#196688 = CARTESIAN_POINT ( 'NONE',  ( 3.017397247018727580, -2.208655522623126366, 0.6135670354654331193 ) ) ;
#196690 = CARTESIAN_POINT ( 'NONE',  ( 4.220665892555866883, 3.818531717603609987, -0.7998128361456211532 ) ) ;
#196691 = CARTESIAN_POINT ( 'NONE',  ( 3.842846474469570062, 6.570739089268092137, -1.199719254218452047 ) ) ;
#196692 = CARTESIAN_POINT ( 'NONE',  ( 4.688250436721117964, 1.278455086129190121, 1.816331037743470933 ) ) ;
#196693 = CARTESIAN_POINT ( 'NONE',  ( -6.968527767744110868, 9.153035033833367251, 1.443375672974078761 ) ) ;
#196694 = DIRECTION ( 'NONE',  ( 0.000000000000000000, 0.000000000000000000, -1.000000000000000000 ) ) ;
#196695 = CARTESIAN_POINT ( 'NONE',  ( 5.694061328059515148, 5.745419092265303007, -0.7216878364870207285 ) ) ;
#196696 = CARTESIAN_POINT ( 'NONE',  ( -6.927853306458756855, 9.105581495667113501, 1.443375672974078761 ) ) ;
#196697 = CARTESIAN_POINT ( 'NONE',  ( 4.584065335196260804, 6.441438539186039591, 1.443375672974065660 ) ) ;
#196698 = EDGE_LOOP ( 'NONE', ( #207502, #188156, #79807, #44667 ) ) ;
#196699 = CARTESIAN_POINT ( 'NONE',  ( 2.408827471728996361, -1.163269702728772392, -1.646838680093346996 ) ) ;
#196701 = CARTESIAN_POINT ( 'NONE',  ( 1.850508050571671559, -2.052242141108654661, -0.2064673365099172486 ) ) ;
#196700 = CARTESIAN_POINT ( 'NONE',  ( 8.111855979677986994, 8.358253485912799263, 1.040834085586084257E-14 ) ) ;
#196702 = DIRECTION ( 'NONE',  ( -0.3090169943749582759, 0.000000000000000000, -0.9510565162951500895 ) ) ;
#196703 = CARTESIAN_POINT ( 'NONE',  ( 4.489158259456265121, 7.291082831790689056, -1.082531754730548412 ) ) ;
#196704 = CARTESIAN_POINT ( 'NONE',  ( -4.285785955251283141, 8.014184357852876417, 0.000000000000000000 ) ) ;
#196705 = CARTESIAN_POINT ( 'NONE',  ( 0.6823417656249917140, 4.342708333674755394, 1.181850606188765695 ) ) ;
#196706 = CARTESIAN_POINT ( 'NONE',  ( 4.558633756138521065, -1.956834287480881063, -0.9866608250781592204 ) ) ;
#196707 = CARTESIAN_POINT ( 'NONE',  ( 2.531875153343257523, -1.674887184936912909, 1.122499117612890673 ) ) ;
#196708 = CARTESIAN_POINT ( 'NONE',  ( 0.5207438388301621757, -1.748553680932497745, 0.5769860859521497298 ) ) ;
#196709 = CARTESIAN_POINT ( 'NONE',  ( 7.690499447449630210, 9.995335326823163058, 1.599625672291281386 ) ) ;
#196710 = CARTESIAN_POINT ( 'NONE',  ( 4.911078036072877850, 1.588895129109271220, 0.8988584441092376531 ) ) ;
#196711 = CARTESIAN_POINT ( 'NONE',  ( 6.188124994278807023, 1.678003296889327034, 1.117835524071027598 ) ) ;
#196712 = CARTESIAN_POINT ( 'NONE',  ( -8.365544474831901667, 9.718555627847388578, 1.199719254218462483 ) ) ;
#196714 = CARTESIAN_POINT ( 'NONE',  ( -5.498713818794216834, 8.572860667638675380, -1.199719254218452047 ) ) ;
#196713 = CARTESIAN_POINT ( 'NONE',  ( 4.663087558633967511, -2.018941045467276929, -1.021363250454855764 ) ) ;
#196715 = CARTESIAN_POINT ( 'NONE',  ( 1.207801281821162975, -0.5101631384078918474, 2.043215687033891559 ) ) ;
#196716 = CARTESIAN_POINT ( 'NONE',  ( -5.589704470584107909, 9.743348658981940247, -0.7998128361456362523 ) ) ;
#196717 = CARTESIAN_POINT ( 'NONE',  ( 4.896967953096117654, 0.3505727482827174502, 2.040303948762006492 ) ) ;
#196718 = CARTESIAN_POINT ( 'NONE',  ( 8.971744963941056028, 11.49012176272984931, 1.599625672291281386 ) ) ;
#196719 = CARTESIAN_POINT ( 'NONE',  ( 3.998552203707626873, 7.829812396822075193, -0.1602144209190259072 ) ) ;
#196720 =( LENGTH_UNIT ( ) NAMED_UNIT ( * ) SI_UNIT ( .MILLI., .METRE. ) );
#196721 = CARTESIAN_POINT ( 'NONE',  ( -7.167456763118792651, 11.51378332361394818, 0.000000000000000000 ) ) ;
#196722 = UNCERTAINTY_MEASURE_WITH_UNIT (LENGTH_MEASURE( 1.000000000000000082E-05 ), #25166, 'distance_accuracy_value', 'NONE');
#196723 = CARTESIAN_POINT ( 'NONE',  ( 0.5717273634750134059, 6.816772624464344510, 3.722363499285739952 ) ) ;
#196724 = CARTESIAN_POINT ( 'NONE',  ( 7.537407054554579489, 7.758339416593960536, 0.000000000000000000 ) ) ;
#196725 = CARTESIAN_POINT ( 'NONE',  ( 4.670798236633449285, 6.855725761985807409, -1.225018586207384352 ) ) ;
#196726 = CARTESIAN_POINT ( 'NONE',  ( -8.948018195339354719, 12.42280974699582607, 1.082531754730560403 ) ) ;
#196728 = CARTESIAN_POINT ( 'NONE',  ( 1.898975720090949837, -2.179683001098455808, -0.4277757613022105110 ) ) ;
#196727 = CARTESIAN_POINT ( 'NONE',  ( 1.547299434221154124, 0.2130619955753136618, 2.109896976817266179 ) ) ;
#196729 = CARTESIAN_POINT ( 'NONE',  ( 4.913571454530422322, 8.125067815752732514, -1.031885869761673069 ) ) ;
#196730 = CARTESIAN_POINT ( 'NONE',  ( -6.947627372360122955, 7.070263120700404968, 0.000000000000000000 ) ) ;
#196731 = CARTESIAN_POINT ( 'NONE',  ( 5.636439174979242850, 7.598931675607687453, -1.599625672291262513 ) ) ;
#196732 = CARTESIAN_POINT ( 'NONE',  ( 3.191801227909254912, -1.315628469008291557, -1.455533501494077342 ) ) ;
#196733 = CARTESIAN_POINT ( 'NONE',  ( 5.931855901178834323, 6.879252291918818152, 1.199719254218462483 ) ) ;
#196734 = CARTESIAN_POINT ( 'NONE',  ( -4.245236785304952853, 7.324258608653995140, 0.8904289178662868620 ) ) ;
#196735 = CARTESIAN_POINT ( 'NONE',  ( 3.765413976293345844, 5.416068943807445635, 1.599625672291267398 ) ) ;
#196736 = CARTESIAN_POINT ( 'NONE',  ( -6.644904684473536882, 6.925012684740138980, 0.7216878364870317197 ) ) ;
#196737 = CARTESIAN_POINT ( 'NONE',  ( -5.910991785878158211, 9.839981483592442402, -0.7216878364870278340 ) ) ;
#196739 = CARTESIAN_POINT ( 'NONE',  ( 2.496466685713152334, -1.086271176545396067, 1.821091972856798913 ) ) ;
#196738 = CIRCLE ( 'NONE', #79223, 10.24999999999998934 ) ;
#196740 = CARTESIAN_POINT ( 'NONE',  ( -4.586401103172829785, 8.572828063668767484, 0.7998128361456281477 ) ) ;
#196741 = CARTESIAN_POINT ( 'NONE',  ( 5.740667459973674447, -1.913685094937540132, -0.4313615418530327150 ) ) ;
#196742 = CARTESIAN_POINT ( 'NONE',  ( 3.555696680978126079, 0.5271953485486252644, -2.096301903996622862 ) ) ;
#196743 = CARTESIAN_POINT ( 'NONE',  ( 3.350949008998193257, 0.4442310927498266948, -1.786741727165648497 ) ) ;
#196744 = CARTESIAN_POINT ( 'NONE',  ( -5.429614816329291216, 6.304498938506903016, 1.045551501023216368 ) ) ;
#196745 = CARTESIAN_POINT ( 'NONE',  ( -1.402160292154681736E-14, 0.1343750003414218575, 1.575800808251672791 ) ) ;
#196746 = CARTESIAN_POINT ( 'NONE',  ( 6.228409164912255491, 0.1778687648950585953, 1.731214608917114317 ) ) ;
#196747 = CARTESIAN_POINT ( 'NONE',  ( -5.329763783503577379, 6.351050847909847086, 1.082531754730549078 ) ) ;
#196748 = CARTESIAN_POINT ( 'NONE',  ( 4.690757960648224589, 6.495636925554817864, 1.443375672974062551 ) ) ;
#196749 = SURFACE_STYLE_USAGE ( .BOTH. , #12650 ) ;
#196750 = CARTESIAN_POINT ( 'NONE',  ( 2.887745953747706373, 1.527789104365802286, 1.529575784674996886 ) ) ;
#196751 = ADVANCED_FACE ( 'NONE', ( #90424 ), #140263, .T. ) ;
#196752 = CARTESIAN_POINT ( 'NONE',  ( 4.833361152654930493, -1.319026006086077230, 1.524810761284051575 ) ) ;
#196753 = CARTESIAN_POINT ( 'NONE',  ( -9.612367721964622191, 10.31677655182129527, -0.7216878364870267237 ) ) ;
#196754 = AXIS2_PLACEMENT_3D ( 'NONE', #142977, #55292, #106224 ) ;
#196755 = CARTESIAN_POINT ( 'NONE',  ( 1.885829143180400624, 1.490600019384461072, 1.565824011241300440 ) ) ;
#196756 = CARTESIAN_POINT ( 'NONE',  ( 2.618384893494442256, 1.290362544248652599, -1.490430290494165755 ) ) ;
#196757 = CARTESIAN_POINT ( 'NONE',  ( -6.486624235763164492, 6.835203243035253173, 0.7121179707554707861 ) ) ;
#196758 = CARTESIAN_POINT ( 'NONE',  ( 4.071774441262452804, -1.115447612638842401, 1.589602391900000411 ) ) ;
#196760 = EDGE_LOOP ( 'NONE', ( #169735, #101311, #50899, #108759 ) ) ;
#196759 = CARTESIAN_POINT ( 'NONE',  ( -9.124274191872631334, 12.62844174295135069, -1.082531754730543083 ) ) ;
#196761 = CARTESIAN_POINT ( 'NONE',  ( -6.770317605177755382, 8.992066187497757213, 1.599625672291269396 ) ) ;
#196762 = CARTESIAN_POINT ( 'NONE',  ( 5.435893244436359240, 5.306573304789342416, -0.7998128361456481317 ) ) ;
#196764 = ORIENTED_EDGE ( 'NONE', *, *, #106881, .T. ) ;
#196763 = CARTESIAN_POINT ( 'NONE',  ( -5.875479466675803231, 7.948088359245467416, -1.599625672291271394 ) ) ;
#196765 = CARTESIAN_POINT ( 'NONE',  ( -9.639484029191951464, 10.34841224358651601, 0.7216878364870438212 ) ) ;
#196766 = CARTESIAN_POINT ( 'NONE',  ( 1.378255502416312117, 1.315327575222959622, 1.771799650011764538 ) ) ;
#196767 = CARTESIAN_POINT ( 'NONE',  ( 3.285556943750000514, -2.413541666188708579, 1.896917185911906500 ) ) ;
#196768 = CARTESIAN_POINT ( 'NONE',  ( 5.436364959771895045, -1.092926877770916017, 1.628904810760459121 ) ) ;
#196769 = CARTESIAN_POINT ( 'NONE',  ( 0.6823417656249917140, 4.655208333674755394, 1.181850606188765695 ) ) ;
#196770 = CARTESIAN_POINT ( 'NONE',  ( 0.7499999999999885647, 3.347916667349487341, -1.299038105676658228 ) ) ;
#196771 = CARTESIAN_POINT ( 'NONE',  ( 0.1745949693968328054, 4.098633874596197657, -2.310325329485760637 ) ) ;
#196772 = CARTESIAN_POINT ( 'NONE',  ( 4.751808913491627706, 0.7073710267669359730, 1.700028372310140368 ) ) ;
#196773 = ORIENTED_EDGE ( 'NONE', *, *, #59598, .T. ) ;
#196774 = CARTESIAN_POINT ( 'NONE',  ( -7.157815033010924921, 10.43820240756634199, 1.199719254218453823 ) ) ;
#196775 = CARTESIAN_POINT ( 'NONE',  ( 0.5101186646354113341, -1.387778780781445676E-14, 1.261047121698059215 ) ) ;
#196776 = CARTESIAN_POINT ( 'NONE',  ( 4.904590598983499916, -2.104870323260544129, -0.2570220051709286579 ) ) ;
#196777 = CARTESIAN_POINT ( 'NONE',  ( -15.75000000000000000, 9.799999999999982947, 3.199999999999997957 ) ) ;
#196778 = CARTESIAN_POINT ( 'NONE',  ( 6.419949431270806528, 7.448694743692793274, 1.199719254218462483 ) ) ;
#196779 = ORIENTED_EDGE ( 'NONE', *, *, #197807, .T. ) ;
#196780 = CARTESIAN_POINT ( 'NONE',  ( 6.784453644556415419, -2.020073987206136401, -0.4066529033334795873 ) ) ;
#196781 = VECTOR ( 'NONE', #160017, 1000.000000000000000 ) ;
#196784 = CARTESIAN_POINT ( 'NONE',  ( 3.561895345837225779, -1.234009368583251387, 1.366721199326895952 ) ) ;
#196783 = CARTESIAN_POINT ( 'NONE',  ( 0.9064450206472760563, 0.5352286137044174330, 1.782442419352270102 ) ) ;
#196782 =( NAMED_UNIT ( * ) PLANE_ANGLE_UNIT ( ) SI_UNIT ( $, .RADIAN. ) );
#196785 = CARTESIAN_POINT ( 'NONE',  ( 6.747154001095143627, 11.02343010125301959, -0.7998128361456291469 ) ) ;
#196786 = DIRECTION ( 'NONE',  ( 0.8660254037844433705, 0.000000000000000000, 0.4999999999999917843 ) ) ;
#196787 = CARTESIAN_POINT ( 'NONE',  ( -6.095272577795516789, 9.268845886473535245, 1.199719254218452047 ) ) ;
#196788 = CARTESIAN_POINT ( 'NONE',  ( -2.081668171172168513E-14, 6.120000000000041851, 2.580000000000011173 ) ) ;
#196789 = CARTESIAN_POINT ( 'NONE',  ( 3.475398437264758833, 0.05438942809191970457, -2.206374867412825402 ) ) ;
#196790 = CARTESIAN_POINT ( 'NONE',  ( 5.325545376182048152, -2.150690057981026193, 0.7024452394915041697 ) ) ;
#196791 = CARTESIAN_POINT ( 'NONE',  ( -6.073689629242158716, 9.069426419882418600, -1.082531754730538864 ) ) ;
#196792 = CARTESIAN_POINT ( 'NONE',  ( 6.310821775929002619, -0.4926439853468951857, -1.743236492463080767 ) ) ;
#196793 = CARTESIAN_POINT ( 'NONE',  ( 5.313669575012682778, -1.220653882476211427, -1.476441452469556159 ) ) ;
#196794 = CARTESIAN_POINT ( 'NONE',  ( -1.364683531250010295, 5.342708333674750953, 0.7879004041258379498 ) ) ;
#196795 = CARTESIAN_POINT ( 'NONE',  ( 5.858239598252557911, 0.7595784280203803362, 1.709674162104061645 ) ) ;
#196796 = AXIS2_PLACEMENT_3D ( 'NONE', #149417, #165666, #33529 ) ;
#196797 = CARTESIAN_POINT ( 'NONE',  ( 6.250447302982959030, -1.852220608400175994, -0.1812639614414724432 ) ) ;
#196798 = CARTESIAN_POINT ( 'NONE',  ( 6.596581986989779267, -0.4770763175313968429, -1.704276504685025673 ) ) ;
#196799 = CARTESIAN_POINT ( 'NONE',  ( 1.147673126774436225, 1.985868168208399842, -0.3494872464938902357 ) ) ;
#196801 = CARTESIAN_POINT ( 'NONE',  ( 2.965558217497352267, 0.3084109246280877237, -2.083234000326895430 ) ) ;
#196800 = CARTESIAN_POINT ( 'NONE',  ( -7.641992139597101108, 12.06740792950531649, 0.7998128361456481317 ) ) ;
#196802 = CARTESIAN_POINT ( 'NONE',  ( 8.259941899223605333, 10.65968485389279508, -1.599625672291268286 ) ) ;
#196804 = CARTESIAN_POINT ( 'NONE',  ( -7.506410603460441422, 11.90922947067921278, -0.7998128361456291469 ) ) ;
#196803 = CARTESIAN_POINT ( 'NONE',  ( 1.451998047844732964, 7.315968950354620581, 4.301760722576522866 ) ) ;
#196805 = FACE_OUTER_BOUND ( 'NONE', #98941, .T. ) ;
#196806 = CARTESIAN_POINT ( 'NONE',  ( 1.986587785418312047, -1.239364722674634933, 1.594781737346209871 ) ) ;
#196807 = CARTESIAN_POINT ( 'NONE',  ( -1.364683531249997417, 2.759375000341422801, 1.214306433183764966E-14 ) ) ;
#196808 = CARTESIAN_POINT ( 'NONE',  ( 2.686486993802192913, 6.285985259411197568, 0.7998128361456362523 ) ) ;
#196809 = ADVANCED_FACE ( 'NONE', ( #74171 ), #66206, .F. ) ;
#196810 = CARTESIAN_POINT ( 'NONE',  ( 2.864712396292764751, -1.492883925411473856, 1.563474562115530375 ) ) ;
#196811 = CARTESIAN_POINT ( 'NONE',  ( 6.890000000000037872, 2.400824642991986391, 2.659875214078717853 ) ) ;
#196813 = CARTESIAN_POINT ( 'NONE',  ( -3.469446951953614189E-15, 3.236073672982384242, -5.377642775528101993E-14 ) ) ;
#196812 = CARTESIAN_POINT ( 'NONE',  ( 4.598150373690133463, 5.393538853173795111, -1.199719254218452047 ) ) ;
#196814 =( BOUNDED_SURFACE ( )  B_SPLINE_SURFACE ( 1, 2, ( 
 ( #84065, #150155, #13732, #1724, #148023, #48404, #66713, #67781, #133931, #31082, #647, #79805, #129720, #117708, #100320, #183699, #65658, #33190, #165321, #63563, #211929, #199936, #163210, #145917, #64628, #131805, #195704, #214033, #96089, #51583, #113453, #15853, #197815, #49447, #146973, #14792, #130767, #196762, #82995, #80883, #212990, #198862, #114517, #180512, #32132, #164264, #115566, #181562, #99273, #81939, #132857, #16915, #149070, #50509, #116631, #20118, #136032, #152275, #151220, #36375, #37448, #123078, #86203, #103526, #203129, #169585, #21168, #121992, #23315, #101384, #70988, #72059, #134979, #184748, #102453, #104601, #39585, #54772, #35307, #87271, #153339, #119837, #187958, #167458, #4911, #185817, #168519, #118763, #105688, #73130, #202045, #3848, #137101, #55836, #204180, #53705, #155473, #120919, #69921, #138170, #19054, #186892, #171716, #85133, #200989, #52635, #68860, #139233, #170648, #7057, #2788, #22234, #38524, #154410, #88346, #5989, #205264, #89423, #56905, #60101, #124133, #156552, #210616, #191152, #208466, #125190, #92637, #160812, #8147, #159740, #74230, #94765, #126260, #140324, #91568, #90489, #57969, #93699, #158678, #10276, #142458, #192218, #206342, #144601, #209530, #25461, #176007, #24375, #143534, #108925, #43881, #40673, #207413, #11338, #177062, #61172, #76351, #173886, #27599, #157621, #190094, #41748, #42820, #9218, #107859, #75290, #193302, #141405, #78484, #77419, #59032, #174947, #26529, #109995, #127333, #44947, #111055, #28678, #12403, #62243, #189035, #106776, #172804, #64374, #146721, #164021, #147768, #97963, #112132, #32938, #13478, #194369, #161891, #14532, #113196, #80629, #30826, #29750, #129466, #130520, #1466, #179201, #196510, #81682, #48152, #114266, #391, #116376, #46012, #15595, #165069, #79554, #63305, #195449, #197556, #132604, #213784, #128402, #180262, #31886, #212738, #66463, #178135, #65407, #131554, #47078, #211669, #198610, #166130, #49200, #96903, #115321, #148819, #82746, #181311, #33994, #99012, #162954, #16661, #95834, #50256 ),
 ( #100068, #145672, #182364, #17717, #83805, #149898, #133674, #187707, #35048, #70733, #153085, #2531, #101119, #89174, #69674, #87013, #3597, #185567, #39335, #167206, #38268, #18795, #105432, #4661, #84879, #184499, #183444, #150967, #186642, #37197, #103271, #20918, #136846, #68607, #23057, #88088, #118515, #54519, #117450, #21978, #201803, #202871, #199679, #85953, #104345, #55585, #154160, #169334, #52387, #5727, #137917, #134730, #120664, #71806, #203937, #170389, #121740, #171468, #119583, #200737, #51322, #135780, #36118, #102201, #168268, #155226, #67531, #19868, #152028, #53445, #174699, #76101, #59851, #209275, #188782, #25210, #143284, #126003, #60921, #92390, #206089, #108671, #26273, #91314, #158426, #107606, #56659, #40419, #207163, #10026, #72885, #77163, #8965, #109745, #123882, #157371, #138992, #41493, #27347, #122822, #75039, #176808, #6807, #189847, #43630, #110803, #141155, #173637, #106522, #94517, #28424, #172548, #127079, #58786, #159487, #124942, #190904, #42568, #142204, #24133, #193042, #208219, #191964, #175755, #44696, #205013, #90235, #156301, #93449, #11086, #7884, #73972, #140067, #57724, #65163, #12163, #194113, #182114, #98764, #33744, #130272, #97712, #15348, #128153, #61997, #32684, #29498, #210358, #129221, #196261, #45763, #212487, #160555, #50003, #148578, #80373, #64129, #47908, #211424, #16411, #195195, #46832, #147519, #78234, #111881, #162706, #114018, #177885, #132361, #197311, #144357, #115070, #95590, #161639, #13234, #79307, #146468, #145423, #131318, #63054, #112945, #178957, #30572, #96653, #14278, #180014, #31635, #163770, #81441, #213540, #48952, #181066, #164820, #82491, #147, #66213, #198363, #116127, #138461, #139537, #199428, #34800, #100875, #172021, #107077, #56133, #190383, #170937, #22537, #187185, #40968, #99822, #88645, #38812, #166962, #183194, #189327, #140624, #55066, #2280, #154703, #123362, #57202, #200492, #8433, #104898, #18552, #205562, #165888, #84629, #173099, #17473, #51071, #117196, #133422, #206636, #23614, #74521, #83557, #89722, #134489 ) ),
 .UNSPECIFIED., .F., .F., .T. ) 
 B_SPLINE_SURFACE_WITH_KNOTS ( ( 2, 2 ),
 ( 3, 2, 2, 2, 2, 2, 2, 2, 2, 2, 2, 2, 2, 2, 2, 2, 2, 2, 2, 2, 2, 2, 2, 2, 2, 2, 2, 2, 2, 2, 2, 2, 2, 2, 2, 2, 2, 2, 2, 2, 2, 2, 2, 2, 2, 2, 2, 2, 2, 2, 2, 2, 2, 2, 2, 2, 2, 2, 2, 2, 2, 2, 2, 2, 2, 2, 2, 2, 2, 2, 2, 2, 2, 2, 2, 2, 2, 2, 2, 2, 2, 2, 2, 2, 2, 2, 2, 2, 2, 2, 2, 2, 2, 2, 2, 2, 2, 2, 2, 2, 2, 2, 2, 2, 2, 2, 2, 2, 2, 2, 2, 2, 2, 2, 2, 2, 2, 2, 2, 2, 3 ),
 ( 0.000000000000000000, 1.000000000000000000 ),
 ( 0.000000000000000000, 0.008333333333333333218, 0.01666666666666666644, 0.02500000000000000139, 0.03333333333333333287, 0.04166666666666666435, 0.05000000000000000278, 0.05833333333333333426, 0.06666666666666666574, 0.07499999999999999722, 0.08333333333333332871, 0.09166666666666666019, 0.1000000000000000056, 0.1083333333333333370, 0.1166666666666666685, 0.1250000000000000000, 0.1333333333333333315, 0.1416666666666666630, 0.1499999999999999944, 0.1583333333333333259, 0.1666666666666666574, 0.1749999999999999889, 0.1833333333333333204, 0.1916666666666666796, 0.2000000000000000111, 0.2083333333333333426, 0.2166666666666666741, 0.2250000000000000056, 0.2333333333333333370, 0.2416666666666666685, 0.2500000000000000000, 0.2583333333333333592, 0.2666666666666666630, 0.2750000000000000222, 0.2833333333333333259, 0.2916666666666666852, 0.2999999999999999889, 0.3083333333333333481, 0.3166666666666666519, 0.3250000000000000111, 0.3333333333333333148, 0.3416666666666666741, 0.3499999999999999778, 0.3583333333333333370, 0.3666666666666666408, 0.3750000000000000000, 0.3833333333333333592, 0.3916666666666666630, 0.4000000000000000222, 0.4083333333333333259, 0.4166666666666666852, 0.4249999999999999889, 0.4333333333333333481, 0.4416666666666666519, 0.4500000000000000111, 0.4583333333333333148, 0.4666666666666666741, 0.4749999999999999778, 0.4833333333333333370, 0.4916666666666666408, 0.5000000000000000000, 0.5083333333333333037, 0.5166666666666667185, 0.5250000000000000222, 0.5333333333333333259, 0.5416666666666666297, 0.5500000000000000444, 0.5583333333333333481, 0.5666666666666666519, 0.5749999999999999556, 0.5833333333333333703, 0.5916666666666666741, 0.5999999999999999778, 0.6083333333333332815, 0.6166666666666666963, 0.6250000000000000000, 0.6333333333333333037, 0.6416666666666667185, 0.6500000000000000222, 0.6583333333333333259, 0.6666666666666666297, 0.6750000000000000444, 0.6833333333333333481, 0.6916666666666666519, 0.6999999999999999556, 0.7083333333333333703, 0.7166666666666666741, 0.7249999999999999778, 0.7333333333333332815, 0.7416666666666666963, 0.7500000000000000000, 0.7583333333333333037, 0.7666666666666667185, 0.7750000000000000222, 0.7833333333333333259, 0.7916666666666666297, 0.8000000000000000444, 0.8083333333333333481, 0.8166666666666666519, 0.8249999999999999556, 0.8333333333333333703, 0.8416666666666666741, 0.8499999999999999778, 0.8583333333333332815, 0.8666666666666666963, 0.8750000000000000000, 0.8833333333333333037, 0.8916666666666667185, 0.9000000000000000222, 0.9083333333333333259, 0.9166666666666666297, 0.9250000000000000444, 0.9333333333333333481, 0.9416666666666666519, 0.9499999999999999556, 0.9583333333333333703, 0.9666666666666666741, 0.9749999999999999778, 0.9833333333333332815, 0.9916666666666666963, 1.000000000000000000 ),
 .UNSPECIFIED. ) 
 GEOMETRIC_REPRESENTATION_ITEM ( )  RATIONAL_B_SPLINE_SURFACE ( (
 ( 1.000000000000000000, 0.8660254037844387076, 1.000000000000000000, 0.8660254037844387076, 1.000000000000000000, 0.8660254037844387076, 1.000000000000000000, 0.8660254037844387076, 1.000000000000000000, 0.8660254037844387076, 1.000000000000000000, 0.8660254037844387076, 1.000000000000000000, 0.8660254037844387076, 1.000000000000000000, 0.8660254037844387076, 1.000000000000000000, 0.8660254037844387076, 1.000000000000000000, 0.8660254037844387076, 1.000000000000000000, 0.8660254037844387076, 1.000000000000000000, 0.8660254037844387076, 1.000000000000000000, 0.8660254037844387076, 1.000000000000000000, 0.8660254037844387076, 1.000000000000000000, 0.8660254037844387076, 1.000000000000000000, 0.8660254037844387076, 1.000000000000000000, 0.8660254037844387076, 1.000000000000000000, 0.8660254037844387076, 1.000000000000000000, 0.8660254037844387076, 1.000000000000000000, 0.8660254037844387076, 1.000000000000000000, 0.8660254037844387076, 1.000000000000000000, 0.8660254037844387076, 1.000000000000000000, 0.8660254037844387076, 1.000000000000000000, 0.8660254037844387076, 1.000000000000000000, 0.8660254037844387076, 1.000000000000000000, 0.8660254037844387076, 1.000000000000000000, 0.8660254037844387076, 1.000000000000000000, 0.8660254037844387076, 1.000000000000000000, 0.8660254037844387076, 1.000000000000000000, 0.8660254037844387076, 1.000000000000000000, 0.8660254037844387076, 1.000000000000000000, 0.8660254037844387076, 1.000000000000000000, 0.8660254037844387076, 1.000000000000000000, 0.8660254037844387076, 1.000000000000000000, 0.8660254037844387076, 1.000000000000000000, 0.8660254037844387076, 1.000000000000000000, 0.8660254037844387076, 1.000000000000000000, 0.8660254037844387076, 1.000000000000000000, 0.8660254037844387076, 1.000000000000000000, 0.8660254037844387076, 1.000000000000000000, 0.8660254037844387076, 1.000000000000000000, 0.8660254037844387076, 1.000000000000000000, 0.8660254037844387076, 1.000000000000000000, 0.8660254037844387076, 1.000000000000000000, 0.8660254037844387076, 1.000000000000000000, 0.8660254037844387076, 1.000000000000000000, 0.8660254037844387076, 1.000000000000000000, 0.8660254037844387076, 1.000000000000000000, 0.8660254037844387076, 1.000000000000000000, 0.8660254037844387076, 1.000000000000000000, 0.8660254037844387076, 1.000000000000000000, 0.8660254037844387076, 1.000000000000000000, 0.8660254037844387076, 1.000000000000000000, 0.8660254037844387076, 1.000000000000000000, 0.8660254037844387076, 1.000000000000000000, 0.8660254037844387076, 1.000000000000000000, 0.8660254037844387076, 1.000000000000000000, 0.8660254037844387076, 1.000000000000000000, 0.8660254037844387076, 1.000000000000000000, 0.8660254037844387076, 1.000000000000000000, 0.8660254037844387076, 1.000000000000000000, 0.8660254037844387076, 1.000000000000000000, 0.8660254037844387076, 1.000000000000000000, 0.8660254037844387076, 1.000000000000000000, 0.8660254037844387076, 1.000000000000000000, 0.8660254037844387076, 1.000000000000000000, 0.8660254037844387076, 1.000000000000000000, 0.8660254037844387076, 1.000000000000000000, 0.8660254037844387076, 1.000000000000000000, 0.8660254037844387076, 1.000000000000000000, 0.8660254037844387076, 1.000000000000000000, 0.8660254037844387076, 1.000000000000000000, 0.8660254037844387076, 1.000000000000000000, 0.8660254037844387076, 1.000000000000000000, 0.8660254037844387076, 1.000000000000000000, 0.8660254037844387076, 1.000000000000000000, 0.8660254037844387076, 1.000000000000000000, 0.8660254037844387076, 1.000000000000000000, 0.8660254037844387076, 1.000000000000000000, 0.8660254037844387076, 1.000000000000000000, 0.8660254037844387076, 1.000000000000000000, 0.8660254037844387076, 1.000000000000000000, 0.8660254037844387076, 1.000000000000000000, 0.8660254037844387076, 1.000000000000000000, 0.8660254037844387076, 1.000000000000000000, 0.8660254037844387076, 1.000000000000000000, 0.8660254037844387076, 1.000000000000000000, 0.8660254037844387076, 1.000000000000000000, 0.8660254037844387076, 1.000000000000000000, 0.8660254037844387076, 1.000000000000000000, 0.8660254037844387076, 1.000000000000000000, 0.8660254037844387076, 1.000000000000000000, 0.8660254037844387076, 1.000000000000000000, 0.8660254037844387076, 1.000000000000000000, 0.8660254037844387076, 1.000000000000000000, 0.8660254037844387076, 1.000000000000000000, 0.8660254037844387076, 1.000000000000000000, 0.8660254037844387076, 1.000000000000000000, 0.8660254037844387076, 1.000000000000000000, 0.8660254037844387076, 1.000000000000000000, 0.8660254037844387076, 1.000000000000000000, 0.8660254037844387076, 1.000000000000000000, 0.8660254037844387076, 1.000000000000000000, 0.8660254037844387076, 1.000000000000000000, 0.8660254037844387076, 1.000000000000000000, 0.8660254037844387076, 1.000000000000000000, 0.8660254037844387076, 1.000000000000000000, 0.8660254037844387076, 1.000000000000000000, 0.8660254037844387076, 1.000000000000000000, 0.8660254037844387076, 1.000000000000000000, 0.8660254037844387076, 1.000000000000000000, 0.8660254037844387076, 1.000000000000000000, 0.8660254037844387076, 1.000000000000000000, 0.8660254037844387076, 1.000000000000000000, 0.8660254037844387076, 1.000000000000000000, 0.8660254037844387076, 1.000000000000000000, 0.8660254037844387076, 1.000000000000000000, 0.8660254037844387076, 1.000000000000000000, 0.8660254037844387076, 1.000000000000000000, 0.8660254037844387076, 1.000000000000000000),
 ( 1.000000000000000000, 0.8660254037844387076, 1.000000000000000000, 0.8660254037844387076, 1.000000000000000000, 0.8660254037844387076, 1.000000000000000000, 0.8660254037844387076, 1.000000000000000000, 0.8660254037844387076, 1.000000000000000000, 0.8660254037844387076, 1.000000000000000000, 0.8660254037844387076, 1.000000000000000000, 0.8660254037844387076, 1.000000000000000000, 0.8660254037844387076, 1.000000000000000000, 0.8660254037844387076, 1.000000000000000000, 0.8660254037844387076, 1.000000000000000000, 0.8660254037844387076, 1.000000000000000000, 0.8660254037844387076, 1.000000000000000000, 0.8660254037844387076, 1.000000000000000000, 0.8660254037844387076, 1.000000000000000000, 0.8660254037844387076, 1.000000000000000000, 0.8660254037844387076, 1.000000000000000000, 0.8660254037844387076, 1.000000000000000000, 0.8660254037844387076, 1.000000000000000000, 0.8660254037844387076, 1.000000000000000000, 0.8660254037844387076, 1.000000000000000000, 0.8660254037844387076, 1.000000000000000000, 0.8660254037844387076, 1.000000000000000000, 0.8660254037844387076, 1.000000000000000000, 0.8660254037844387076, 1.000000000000000000, 0.8660254037844387076, 1.000000000000000000, 0.8660254037844387076, 1.000000000000000000, 0.8660254037844387076, 1.000000000000000000, 0.8660254037844387076, 1.000000000000000000, 0.8660254037844387076, 1.000000000000000000, 0.8660254037844387076, 1.000000000000000000, 0.8660254037844387076, 1.000000000000000000, 0.8660254037844387076, 1.000000000000000000, 0.8660254037844387076, 1.000000000000000000, 0.8660254037844387076, 1.000000000000000000, 0.8660254037844387076, 1.000000000000000000, 0.8660254037844387076, 1.000000000000000000, 0.8660254037844387076, 1.000000000000000000, 0.8660254037844387076, 1.000000000000000000, 0.8660254037844387076, 1.000000000000000000, 0.8660254037844387076, 1.000000000000000000, 0.8660254037844387076, 1.000000000000000000, 0.8660254037844387076, 1.000000000000000000, 0.8660254037844387076, 1.000000000000000000, 0.8660254037844387076, 1.000000000000000000, 0.8660254037844387076, 1.000000000000000000, 0.8660254037844387076, 1.000000000000000000, 0.8660254037844387076, 1.000000000000000000, 0.8660254037844387076, 1.000000000000000000, 0.8660254037844387076, 1.000000000000000000, 0.8660254037844387076, 1.000000000000000000, 0.8660254037844387076, 1.000000000000000000, 0.8660254037844387076, 1.000000000000000000, 0.8660254037844387076, 1.000000000000000000, 0.8660254037844387076, 1.000000000000000000, 0.8660254037844387076, 1.000000000000000000, 0.8660254037844387076, 1.000000000000000000, 0.8660254037844387076, 1.000000000000000000, 0.8660254037844387076, 1.000000000000000000, 0.8660254037844387076, 1.000000000000000000, 0.8660254037844387076, 1.000000000000000000, 0.8660254037844387076, 1.000000000000000000, 0.8660254037844387076, 1.000000000000000000, 0.8660254037844387076, 1.000000000000000000, 0.8660254037844387076, 1.000000000000000000, 0.8660254037844387076, 1.000000000000000000, 0.8660254037844387076, 1.000000000000000000, 0.8660254037844387076, 1.000000000000000000, 0.8660254037844387076, 1.000000000000000000, 0.8660254037844387076, 1.000000000000000000, 0.8660254037844387076, 1.000000000000000000, 0.8660254037844387076, 1.000000000000000000, 0.8660254037844387076, 1.000000000000000000, 0.8660254037844387076, 1.000000000000000000, 0.8660254037844387076, 1.000000000000000000, 0.8660254037844387076, 1.000000000000000000, 0.8660254037844387076, 1.000000000000000000, 0.8660254037844387076, 1.000000000000000000, 0.8660254037844387076, 1.000000000000000000, 0.8660254037844387076, 1.000000000000000000, 0.8660254037844387076, 1.000000000000000000, 0.8660254037844387076, 1.000000000000000000, 0.8660254037844387076, 1.000000000000000000, 0.8660254037844387076, 1.000000000000000000, 0.8660254037844387076, 1.000000000000000000, 0.8660254037844387076, 1.000000000000000000, 0.8660254037844387076, 1.000000000000000000, 0.8660254037844387076, 1.000000000000000000, 0.8660254037844387076, 1.000000000000000000, 0.8660254037844387076, 1.000000000000000000, 0.8660254037844387076, 1.000000000000000000, 0.8660254037844387076, 1.000000000000000000, 0.8660254037844387076, 1.000000000000000000, 0.8660254037844387076, 1.000000000000000000, 0.8660254037844387076, 1.000000000000000000, 0.8660254037844387076, 1.000000000000000000, 0.8660254037844387076, 1.000000000000000000, 0.8660254037844387076, 1.000000000000000000, 0.8660254037844387076, 1.000000000000000000, 0.8660254037844387076, 1.000000000000000000, 0.8660254037844387076, 1.000000000000000000, 0.8660254037844387076, 1.000000000000000000, 0.8660254037844387076, 1.000000000000000000, 0.8660254037844387076, 1.000000000000000000, 0.8660254037844387076, 1.000000000000000000, 0.8660254037844387076, 1.000000000000000000, 0.8660254037844387076, 1.000000000000000000, 0.8660254037844387076, 1.000000000000000000, 0.8660254037844387076, 1.000000000000000000, 0.8660254037844387076, 1.000000000000000000, 0.8660254037844387076, 1.000000000000000000, 0.8660254037844387076, 1.000000000000000000, 0.8660254037844387076, 1.000000000000000000, 0.8660254037844387076, 1.000000000000000000, 0.8660254037844387076, 1.000000000000000000, 0.8660254037844387076, 1.000000000000000000, 0.8660254037844387076, 1.000000000000000000, 0.8660254037844387076, 1.000000000000000000, 0.8660254037844387076, 1.000000000000000000, 0.8660254037844387076, 1.000000000000000000) ) ) 
 REPRESENTATION_ITEM ( '' )  SURFACE ( )  );
#196815 = CARTESIAN_POINT ( 'NONE',  ( 8.717529583462638954, 12.15390636647303069, 1.082531754730546636 ) ) ;
#196816 = DIRECTION ( 'NONE',  ( -1.000000000000000000, 5.459311322609750190E-16, -5.329070518200750605E-15 ) ) ;
#196817 = CARTESIAN_POINT ( 'NONE',  ( -8.039621903223732602, 8.481906429956900695, 1.040834085586084257E-14 ) ) ;
#196818 = CARTESIAN_POINT ( 'NONE',  ( 1.364683531249986537, 0.3635416670080869328, 0.7879004041258500513 ) ) ;
#196819 = CARTESIAN_POINT ( 'NONE',  ( 1.206853476500208133, 1.935082376036290075, 1.028754739392373496 ) ) ;
#196820 = CARTESIAN_POINT ( 'NONE',  ( 0.4909524369918957798, 7.516007857509691803, 2.014442075801145648 ) ) ;
#196821 = CARTESIAN_POINT ( 'NONE',  ( 2.958202477073975878, 2.251720482184274008, -0.2206431264100849887 ) ) ;
#196822 = CARTESIAN_POINT ( 'NONE',  ( -8.345207244411405156, 9.694828859023472134, 1.199719254218462483 ) ) ;
#196823 = CARTESIAN_POINT ( 'NONE',  ( -4.568734577680894304, 5.392907097791561633, -1.082531754730543971 ) ) ;
#196824 = CARTESIAN_POINT ( 'NONE',  ( -1.364683531250012516, 3.551041667008086211, -0.7879004041258300672 ) ) ;
#196825 = CARTESIAN_POINT ( 'NONE',  ( 4.604167169973131912, 8.362045362587558373, -0.1994984680026238300 ) ) ;
#196826 = CARTESIAN_POINT ( 'NONE',  ( 0.7500000000000006661, 11.33333333333333393, 1.299038105676657340 ) ) ;
#196827 = CARTESIAN_POINT ( 'NONE',  ( 5.225741863424510747, 5.061396693608882558, 0.7998128361456352531 ) ) ;
#196828 = EDGE_CURVE ( 'NONE', #10803, #98551, #185617, .T. ) ;
#196829 = CARTESIAN_POINT ( 'NONE',  ( 2.934531203469164851, 0.2125141484592401875, 1.756833830538252483 ) ) ;
#196830 = CARTESIAN_POINT ( 'NONE',  ( 6.299877592275240801, -0.7493655176046759570, 2.075778730795534877 ) ) ;
#196831 = CARTESIAN_POINT ( 'NONE',  ( 1.364683531250000303, 9.005208333674731946, -0.7879004041258355073 ) ) ;
#196832 = AXIS2_PLACEMENT_3D ( 'NONE', #188337, #39976, #172107 ) ;
#196833 = CARTESIAN_POINT ( 'NONE',  ( -4.599959256786493533, 8.588645909551377855, 0.000000000000000000 ) ) ;
#196834 = CARTESIAN_POINT ( 'NONE',  ( 5.273064617572334356, 1.777004185780726386, -0.9530273427700783895 ) ) ;
#196836 = VERTEX_POINT ( 'NONE', #158622 ) ;
#196835 = CARTESIAN_POINT ( 'NONE',  ( 4.974790932252576958, -1.306838681284767212, 1.254843474919357105 ) ) ;
#196837 = CARTESIAN_POINT ( 'NONE',  ( 2.377632874612686020, 1.149002834218125102, 1.476114537088555112 ) ) ;
#196838 = CARTESIAN_POINT ( 'NONE',  ( 3.590741003927796271, 2.018730135711533258, 0.4582614309688318732 ) ) ;
#196839 = CARTESIAN_POINT ( 'NONE',  ( -6.089020385868856522, 9.157588645938716354, -1.082531754730549967 ) ) ;
#196840 = CARTESIAN_POINT ( 'NONE',  ( 2.513799616133075343, -0.5961229146635020903, 1.817204401178821760 ) ) ;
#196841 =( NAMED_UNIT ( * ) PLANE_ANGLE_UNIT ( ) SI_UNIT ( $, .RADIAN. ) );
#196842 = CARTESIAN_POINT ( 'NONE',  ( 0.000000000000000000, -2.500000000000002220, 0.000000000000000000 ) ) ;
#196843 = CARTESIAN_POINT ( 'NONE',  ( -4.669816416521347158, 7.043937703794544092, 1.217519100783383212 ) ) ;
#196844 = EDGE_CURVE ( 'NONE', #130259, #85478, #10219, .T. ) ;
#196845 = CARTESIAN_POINT ( 'NONE',  ( -1.364683531249997417, 4.321875000341417028, 1.214306433183764966E-14 ) ) ;
#196846 = CARTESIAN_POINT ( 'NONE',  ( 1.037202349414727109, -0.04413313863061394532, 1.912034500058952036 ) ) ;
#196847 = CARTESIAN_POINT ( 'NONE',  ( 2.295295855072278624, -1.753792786583353580, 0.8793850528211948347 ) ) ;
#196848 = ADVANCED_FACE ( 'NONE', ( #27542 ), #39525, .F. ) ;
#196849 = CARTESIAN_POINT ( 'NONE',  ( 0.5267199648841465187, 1.994564833640038781, -0.2930222482238133419 ) ) ;
#196850 = CARTESIAN_POINT ( 'NONE',  ( -5.646044625448194410, 5.551749915969804938, 0.000000000000000000 ) ) ;
#196851 = CARTESIAN_POINT ( 'NONE',  ( 8.229962938695207342, 9.560377169021284871, 1.199719254218462483 ) ) ;
#196852 = CARTESIAN_POINT ( 'NONE',  ( 0.2626887844769665303, -1.667795467377327423, -0.8471929967568125885 ) ) ;
#196853 = CARTESIAN_POINT ( 'NONE',  ( -1.364683531250012516, 2.530208333674753174, 0.7879004041258379498 ) ) ;
#196855 = CARTESIAN_POINT ( 'NONE',  ( 2.654045540373184409, 1.135223644230592743, 1.786994778491631797 ) ) ;
#196854 = CARTESIAN_POINT ( 'NONE',  ( -7.429504990608782222, 8.730472579540773381, 1.082531754730549967 ) ) ;
#196856 = CARTESIAN_POINT ( 'NONE',  ( 8.731030487143305763, 13.51342317695541873, -8.232470247100428296 ) ) ;
#196857 = CARTESIAN_POINT ( 'NONE',  ( 3.789561645344252661, -1.914057400617325433, 0.7896510022299551013 ) ) ;
#196858 = CARTESIAN_POINT ( 'NONE',  ( 5.248941747146098180, 6.152795455539095570, -1.199719254218452047 ) ) ;
#196860 = CARTESIAN_POINT ( 'NONE',  ( 4.813308228051395687, 5.574280006603454574, 1.199719254218462483 ) ) ;
#196859 = CARTESIAN_POINT ( 'NONE',  ( 6.052696072153842977, -1.792546385985850810, -1.075631278504029620 ) ) ;
#196862 = ORIENTED_EDGE ( 'NONE', *, *, #83855, .T. ) ;
#196861 = CARTESIAN_POINT ( 'NONE',  ( 4.559475717982610199, 0.3993622990657343941, -1.781190812766835441 ) ) ;
#196863 = CARTESIAN_POINT ( 'NONE',  ( 9.348510611822643313, 10.86534945433664134, 1.199719254218453823 ) ) ;
#196864 = PRESENTATION_STYLE_ASSIGNMENT (( #132969 ) ) ;
#196865 = CARTESIAN_POINT ( 'NONE',  ( 8.846954724764692912, 13.14807067402342255, -7.639157931441056704 ) ) ;
#196866 = CARTESIAN_POINT ( 'NONE',  ( 6.668967514498191029, -2.014860697535350020, -0.9005387006749266954 ) ) ;
#196867 = CARTESIAN_POINT ( 'NONE',  ( 0.6823417656249934904, 11.00520833367472839, 1.181850606188764807 ) ) ;
#196868 = ORIENTED_EDGE ( 'NONE', *, *, #69678, .F. ) ;
#196869 = CARTESIAN_POINT ( 'NONE',  ( 5.039673278062164918, -1.814583965733532978, 0.6035816954967700987 ) ) ;
#196870 = CARTESIAN_POINT ( 'NONE',  ( -8.676328237741483207, 12.20980114641871062, -1.199719254218446718 ) ) ;
#196871 = AXIS2_PLACEMENT_3D ( 'NONE', #177783, #182010, #33641 ) ;
#196872 = CARTESIAN_POINT ( 'NONE',  ( 5.621827251160867789, 9.710548892996357040, 1.040834085586084257E-14 ) ) ;
#196873 = CARTESIAN_POINT ( 'NONE',  ( 1.360316468749965590, 1.067708333674703081, -0.7853790794159083433 ) ) ;
#196874 = CARTESIAN_POINT ( 'NONE',  ( 3.484082288587588838, 7.008587070086755411, -0.7216878364870267237 ) ) ;
#196875 = CARTESIAN_POINT ( 'NONE',  ( 6.909076424898653812, 5.229711127717879826, 1.214306433183764966E-14 ) ) ;
#196876 = CARTESIAN_POINT ( 'NONE',  ( 0.000000000000000000, 4.446947634372834912, 11.95586206896558146 ) ) ;
#196877 = CARTESIAN_POINT ( 'NONE',  ( 0.5382993156314471728, -1.579489783069366604, 0.9460463261394757017 ) ) ;
#196878 = EDGE_LOOP ( 'NONE', ( #13404, #74501, #1916, #127058, #143457, #206184 ) ) ;
#196879 = CARTESIAN_POINT ( 'NONE',  ( -5.752402313948099533, 9.933162809573264695, -0.7998128361456362523 ) ) ;
#196880 = CARTESIAN_POINT ( 'NONE',  ( 5.149604166610964207, 0.5880212298954893280, -1.775756280894603467 ) ) ;
#196881 = CARTESIAN_POINT ( 'NONE',  ( -1.812013678032658559, 0.3846686717400374933, 0.6718421233638942613 ) ) ;
#196882 = CARTESIAN_POINT ( 'NONE',  ( -6.773376349083141790, -7.246166700180801001, -6.661184041420938229 ) ) ;
#196883 = CARTESIAN_POINT ( 'NONE',  ( -1.436838838544729491, 7.449283400311742298, -4.203727439823573775 ) ) ;
#196884 = CARTESIAN_POINT ( 'NONE',  ( -6.507550544879489252, 9.575597488125954015, 1.082531754730548412 ) ) ;
#196885 = CARTESIAN_POINT ( 'NONE',  ( 6.145923705696426431, 6.064665832934283962, 0.7998128361456341429 ) ) ;
#196886 = CARTESIAN_POINT ( 'NONE',  ( 0.7956772557287052905, -1.388798143503049420, -1.396678344884971112 ) ) ;
#196887 = CARTESIAN_POINT ( 'NONE',  ( 2.390250109419411295, -0.7743331304885041622, -1.862010821188607945 ) ) ;
#196888 = CARTESIAN_POINT ( 'NONE',  ( -6.808165692356648258, 11.09461040772476714, 0.7998128361456481317 ) ) ;
#196889 = CARTESIAN_POINT ( 'NONE',  ( 4.746236293235721604, 7.694970221153795364, 1.199719254218451159 ) ) ;
#196890 = CARTESIAN_POINT ( 'NONE',  ( -11.89829993707161648, 11.32919228251126142, -1.561606677374349772 ) ) ;
#196891 = CARTESIAN_POINT ( 'NONE',  ( 2.203317661949526052, -0.4785072280911427667, 2.138412878249687399 ) ) ;
#196892 = SURFACE_STYLE_USAGE ( .BOTH. , #210993 ) ;
#196893 = CARTESIAN_POINT ( 'NONE',  ( -9.917953063596627317, 11.52969898140628047, -1.199719254218441611 ) ) ;
#196894 = DIRECTION ( 'NONE',  ( 0.000000000000000000, -1.000000000000000000, 0.000000000000000000 ) ) ;
#196895 = CARTESIAN_POINT ( 'NONE',  ( 1.349890321011279370, 8.200329036966271801, 10.79298809153610073 ) ) ;
#196896 = CARTESIAN_POINT ( 'NONE',  ( 4.800995793014950941, 5.734154859006458160, -1.082531754730548412 ) ) ;
#196897 = CARTESIAN_POINT ( 'NONE',  ( 7.248805684800777804, 11.60869039890961218, 1.040834085586084257E-14 ) ) ;
#196898 = CARTESIAN_POINT ( 'NONE',  ( -9.367496997601190145, 14.57669131240758276, 7.413898975931879853 ) ) ;
#196899 = CARTESIAN_POINT ( 'NONE',  ( 7.024532985656136930, 8.328281583754568729, 1.082531754730549967 ) ) ;
#196900 = ORIENTED_EDGE ( 'NONE', *, *, #14467, .F. ) ;
#196902 = CARTESIAN_POINT ( 'NONE',  ( 1.928386798537110147, -0.9510432213125822321, -1.774292727131807856 ) ) ;
#196901 = CARTESIAN_POINT ( 'NONE',  ( 4.651808992177354440, 0.7092673950449077669, 1.699362209096597187 ) ) ;
#196903 = CARTESIAN_POINT ( 'NONE',  ( 2.654040013917441598, -0.3913916837698909745, -2.264681309554557043 ) ) ;
#196905 = CARTESIAN_POINT ( 'NONE',  ( 1.639267886685547460, 1.721996695667164845, -0.7061035538288776836 ) ) ;
#196904 = CARTESIAN_POINT ( 'NONE',  ( -0.1290005225502433017, 7.629137130509076492, -2.773995091683974401 ) ) ;
#196906 = CARTESIAN_POINT ( 'NONE',  ( -1.642778471875000035, -1.567708332855376252, -2.845375778867859751 ) ) ;
#196907 = LINE ( 'NONE', #45351, #39740 ) ;
#196908 = CARTESIAN_POINT ( 'NONE',  ( 5.941656858135131891, -1.798430535887390658, 0.6506349336675710804 ) ) ;
#196909 = CARTESIAN_POINT ( 'NONE',  ( -9.345647958521597687, 9.797677461230342999, 0.7998128361456462443 ) ) ;
#196910 = CARTESIAN_POINT ( 'NONE',  ( -7.119440060951841787, 7.478637290631501067, 0.000000000000000000 ) ) ;
#196912 = CARTESIAN_POINT ( 'NONE',  ( 3.520239479114236403, 1.187513476551487424, -1.445374034619356207 ) ) ;
#196911 = CARTESIAN_POINT ( 'NONE',  ( 5.021074897447791230, -1.984789774362485604, 0.6572858584967393725 ) ) ;
#196913 = CARTESIAN_POINT ( 'NONE',  ( 7.348156068926750883, 8.635565504245116486, -1.082531754730537976 ) ) ;
#196914 = CARTESIAN_POINT ( 'NONE',  ( 5.987831981441136264, -1.833028718050220940, -0.1737628300680846560 ) ) ;
#196915 = CARTESIAN_POINT ( 'NONE',  ( 3.388648328411762556, 6.040841252200647382, 1.199719254218462483 ) ) ;
#196917 = CARTESIAN_POINT ( 'NONE',  ( 4.059776932288224671, 6.823824623389866950, 1.199719254218462483 ) ) ;
#196916 = DIRECTION ( 'NONE',  ( -1.000000000000000000, 8.673617379884035472E-16, 0.000000000000000000 ) ) ;
#196918 = CARTESIAN_POINT ( 'NONE',  ( 4.635198054048816019, -1.575417825122129134, 0.7027606912313691945 ) ) ;
#196919 = CARTESIAN_POINT ( 'NONE',  ( -6.735703387890906946, 6.752742128827836865, -0.7998128361456291469 ) ) ;
#196920 = CARTESIAN_POINT ( 'NONE',  ( 0.7383815455153321938, 1.732312080274291732, -0.08293238807991276662 ) ) ;
#196921 = DIRECTION ( 'NONE',  ( 0.000000000000000000, 0.000000000000000000, -1.000000000000000000 ) ) ;
#196922 = CARTESIAN_POINT ( 'NONE',  ( 1.914442667406905496, 3.262253226108020154, 0.4355078757043838178 ) ) ;
#196923 = EDGE_CURVE ( 'NONE', #198335, #155131, #68081, .T. ) ;
#196924 = CARTESIAN_POINT ( 'NONE',  ( 9.578353140444622937, -9.943513495888055331, -0.1579188828665808730 ) ) ;
#196925 = CARTESIAN_POINT ( 'NONE',  ( 4.856392247755495717, -2.170420479375735123, -0.05992511257937349622 ) ) ;
#196926 = CARTESIAN_POINT ( 'NONE',  ( 3.615676881913011176, -1.798418494116042821, 0.3134422064149794407 ) ) ;
#196927 = CARTESIAN_POINT ( 'NONE',  ( 0.7077677203753615087, 0.6208407433182620005, -1.860969989990405749 ) ) ;
#196928 = CARTESIAN_POINT ( 'NONE',  ( 5.542236361656130761, 0.8606211682868989410, 1.934736125387125361 ) ) ;
#196930 = CARTESIAN_POINT ( 'NONE',  ( -0.6823417656250212460, 4.363541667008085767, 1.181850606188767472 ) ) ;
#196929 = CARTESIAN_POINT ( 'NONE',  ( 5.935170609274059039, -1.657740282732190096, -1.583558971889464706 ) ) ;
#196931 = CARTESIAN_POINT ( 'NONE',  ( 3.289951133708768793, 7.658661826345697143, 2.499999999999998668 ) ) ;
#196932 = CARTESIAN_POINT ( 'NONE',  ( 9.402743226277308963, 10.92862083786708816, -1.199719254218446718 ) ) ;
#196933 = CARTESIAN_POINT ( 'NONE',  ( 0.9441710812277158693, -1.348169866081018853, -1.636719737310005973 ) ) ;
#196934 = CARTESIAN_POINT ( 'NONE',  ( -3.877268743828284681, 5.546566172598190292, 1.443375672974064550 ) ) ;
#196935 = CARTESIAN_POINT ( 'NONE',  ( 5.594708818112484217, 5.774250729507365953, 0.6894988139244705438 ) ) ;
#196936 = CARTESIAN_POINT ( 'NONE',  ( -4.650083499362882122, 6.448183387388563226, 1.443375672974064550 ) ) ;
#196937 = CARTESIAN_POINT ( 'NONE',  ( 6.016515519638066856, 0.8726334679417474538, 1.988148615226674298 ) ) ;
#196939 = CARTESIAN_POINT ( 'NONE',  ( -6.009258394948636914E-15, 12.46875000068279959, -1.732050807568875195 ) ) ;
#196938 = CARTESIAN_POINT ( 'NONE',  ( 6.883263157960390011, 6.036220326785228352, 2.548703601196927515 ) ) ;
#196941 = ORIENTED_EDGE ( 'NONE', *, *, #196604, .F. ) ;
#196940 = CARTESIAN_POINT ( 'NONE',  ( 2.104415045828517350, -0.9466870704337572162, 2.009588771043930411 ) ) ;
#196942 = CARTESIAN_POINT ( 'NONE',  ( 5.818982467333652764, 0.9914020171761170896, -1.755767668913270407 ) ) ;
#196944 = CARTESIAN_POINT ( 'NONE',  ( 5.084863090169797317, 1.972218467801799102, 0.6036872243675943661 ) ) ;
#196943 = CARTESIAN_POINT ( 'NONE',  ( 3.497113557321089861, 6.167384019261527683, -1.199719254218446718 ) ) ;
#196946 = CARTESIAN_POINT ( 'NONE',  ( -3.475000000000000533, -3.149999999999999911, 0.000000000000000000 ) ) ;
#196945 = CARTESIAN_POINT ( 'NONE',  ( 6.204791576909545192, 7.267953590263130259, -1.199719254218452047 ) ) ;
#196947 = CARTESIAN_POINT ( 'NONE',  ( 4.766573523656222555, 7.718696989977711809, 1.199719254218452047 ) ) ;
#196948 = CARTESIAN_POINT ( 'NONE',  ( -3.285556943750000070, -3.346874999522041261, 0.000000000000000000 ) ) ;
#196949 = CARTESIAN_POINT ( 'NONE',  ( 0.2329586101569528500, 5.725166970077667727, -2.439795138137319963 ) ) ;
#196950 = CARTESIAN_POINT ( 'NONE',  ( 4.897927690869709139, -0.6253142351902387652, -1.731941863025769246 ) ) ;
#196952 = ORIENTED_EDGE ( 'NONE', *, *, #92980, .F. ) ;
#196951 = CARTESIAN_POINT ( 'NONE',  ( 5.518332215962025167, 6.396807992499198292, -1.199719254218445830 ) ) ;
#196953 = CARTESIAN_POINT ( 'NONE',  ( -0.2104748580754391973, 0.7011259924453935310, -2.185273273056092425 ) ) ;
#196954 = CARTESIAN_POINT ( 'NONE',  ( 1.412684849630441386, 1.518645404226389051, 0.8176530575639671117 ) ) ;
#196955 = CARTESIAN_POINT ( 'NONE',  ( 0.07540816263147330500, 1.497505997221737495, 1.350731191893522976 ) ) ;
#196956 = CARTESIAN_POINT ( 'NONE',  ( 1.969760627029959688, -2.255332599139341809, -0.4437108664413855763 ) ) ;
#196957 = CARTESIAN_POINT ( 'NONE',  ( -0.6823417656249969321, 3.780208333674754506, -1.181850606188749264 ) ) ;
#196958 = CARTESIAN_POINT ( 'NONE',  ( 1.616897013105462522, 1.519709519468028791, -1.676125853178417113 ) ) ;
#196959 = CARTESIAN_POINT ( 'NONE',  ( 3.949915024511057471, 0.7098439763573929362, -1.982976504383345162 ) ) ;
#196960 = CARTESIAN_POINT ( 'NONE',  ( -7.024532985656169792, 9.288650798055913427, 1.443375672974064550 ) ) ;
#196961 = CARTESIAN_POINT ( 'NONE',  ( 2.196244507144041513, -0.4668761045134894871, -1.706985182271273382 ) ) ;
#196962 = CARTESIAN_POINT ( 'NONE',  ( 6.531277313481192337, 8.642909503859968368, 1.599625672291281386 ) ) ;
#196963 = CARTESIAN_POINT ( 'NONE',  ( 5.573810548549551491, 6.635772073796838200, -1.082531754730548412 ) ) ;
#196964 = CARTESIAN_POINT ( 'NONE',  ( -4.252453736180621391, 8.112946458852704268, -0.7998128361456281477 ) ) ;
#196965 = CARTESIAN_POINT ( 'NONE',  ( 0.7499999999999902300, 1.733333333333357595, 1.299038105676657340 ) ) ;
#196966 = ADVANCED_FACE ( 'NONE', ( #110997 ), #95374, .F. ) ;
#196967 = CARTESIAN_POINT ( 'NONE',  ( 6.451452576676337536, -1.984925862664425500, 0.9976300440488919952 ) ) ;
#196968 = CARTESIAN_POINT ( 'NONE',  ( 3.539196308827243787, -1.659330947522210886, -1.431560661003590695 ) ) ;
#196969 = CARTESIAN_POINT ( 'NONE',  ( -3.276266675996675204, 6.974061555304760240, -0.7998128361456281477 ) ) ;
#196970 = CARTESIAN_POINT ( 'NONE',  ( 0.4229270055062719358, 8.019365653748165457, -1.955756443285229240 ) ) ;
#196971 = CARTESIAN_POINT ( 'NONE',  ( 6.410795937096152919, -0.5649949523399040441, -2.043744576961013859 ) ) ;
#196972 = CARTESIAN_POINT ( 'NONE',  ( -1.201851678989727383E-14, 3.446875000341421469, -1.575800808251660134 ) ) ;
#196973 = CARTESIAN_POINT ( 'NONE',  ( 1.364683531250000303, 9.255208333674733723, -0.7879004041258355073 ) ) ;
#196974 = CARTESIAN_POINT ( 'NONE',  ( -5.097502569058225852, 5.049433873430440478, -0.7216878364870207285 ) ) ;
#196975 = CARTESIAN_POINT ( 'NONE',  ( 5.888958097455845753, -2.014202512972632420, -0.6635655960139997811 ) ) ;
#196976 = CARTESIAN_POINT ( 'NONE',  ( -6.617788377246196951, 7.853746207276256719, -1.082531754730549967 ) ) ;
#196977 = ORIENTED_EDGE ( 'NONE', *, *, #126765, .T. ) ;
#196978 = CARTESIAN_POINT ( 'NONE',  ( -4.285785955695645910, 7.053815144069948140, 1.082531754730549967 ) ) ;
#196979 = CARTESIAN_POINT ( 'NONE',  ( 4.981731378017507872, 7.899438143407371271, -1.199719254218452047 ) ) ;
#196980 = CARTESIAN_POINT ( 'NONE',  ( 6.620655732516647518, 0.007553340620044743381, 1.826407896915738238 ) ) ;
#196981 = CARTESIAN_POINT ( 'NONE',  ( -0.4000000000000513700, 3.949999999999967315, 0.8338124244295243015 ) ) ;
#196982 = DIRECTION ( 'NONE',  ( 0.000000000000000000, 0.000000000000000000, -1.000000000000000000 ) ) ;
#196983 = CARTESIAN_POINT ( 'NONE',  ( -1.201851678989727383E-14, 4.259375000341417028, -1.575800808251660134 ) ) ;
#196984 = CARTESIAN_POINT ( 'NONE',  ( 2.014833872101874146, -1.687939792665555494, 0.4236265878580796618 ) ) ;
#196985 = CARTESIAN_POINT ( 'NONE',  ( 3.358669367883368118, 4.941533567329135401, -1.599625672291262513 ) ) ;
#196987 = ADVANCED_FACE ( 'NONE', ( #3580 ), #32991, .T. ) ;
#196986 = CARTESIAN_POINT ( 'NONE',  ( 0.2737812321212430566, -1.924752420120953822, 0.3788971555385572954 ) ) ;
#196988 = CARTESIAN_POINT ( 'NONE',  ( -1.364683531250014514, -0.4489583329919089039, -0.7879004041258359514 ) ) ;
#196989 = CARTESIAN_POINT ( 'NONE',  ( -4.237421715137035250, 7.350374185294469953, -0.8920271880306808177 ) ) ;
#196990 = AXIS2_PLACEMENT_3D ( 'NONE', #11768, #28034, #159099 ) ;
#196991 = CARTESIAN_POINT ( 'NONE',  ( 6.491117449447131982, 1.883434485765375310, -1.060826435891427666 ) ) ;
#196992 = EDGE_CURVE ( 'NONE', #177247, #80420, #117540, .T. ) ;
#196993 = CARTESIAN_POINT ( 'NONE',  ( -3.110706179331648169, 5.716575411607132118, 1.199719254218462483 ) ) ;
#196994 = CARTESIAN_POINT ( 'NONE',  ( -5.978782553502159480, 8.958701498185728695, 1.082531754730548412 ) ) ;
#196995 = CARTESIAN_POINT ( 'NONE',  ( 5.559502693676295237, 0.4258712887980077300, -2.119171757835013548 ) ) ;
#196997 = EDGE_LOOP ( 'NONE', ( #202632, #199990, #92752, #159926 ) ) ;
#196996 = CARTESIAN_POINT ( 'NONE',  ( -3.135678666510573365, 6.880318554229450712, 0.000000000000000000 ) ) ;
#196998 = CARTESIAN_POINT ( 'NONE',  ( -1.201851678989727383E-14, 3.571875000341422357, 1.575800808251672791 ) ) ;
#196999 = CARTESIAN_POINT ( 'NONE',  ( 6.538353035222548293, 1.949559774641503651, 0.2916953021188176121 ) ) ;
#197000 = CARTESIAN_POINT ( 'NONE',  ( 4.938689436542594180, 0.9992198110298566860, 1.416717458774526373 ) ) ;
#197002 = CARTESIAN_POINT ( 'NONE',  ( 2.173600921376659834, 1.351110561487681716, 1.725424542402646422 ) ) ;
#197001 = CARTESIAN_POINT ( 'NONE',  ( 1.360316468749955598, -0.7135416663252973635, -0.7853790794159122290 ) ) ;
#197003 = CARTESIAN_POINT ( 'NONE',  ( 2.925200879784293218, 2.172439923367448067, 0.7784344579512092466 ) ) ;
#197004 = CARTESIAN_POINT ( 'NONE',  ( 5.061820804786828276, 2.038956591669589535, -0.2981446164109917696 ) ) ;
#197005 = CARTESIAN_POINT ( 'NONE',  ( 1.007640649619114148, -0.8727987561519714443, -1.734835989144311919 ) ) ;
#197006 = CARTESIAN_POINT ( 'NONE',  ( -6.195713011320795438, 8.251417818006149929, -1.443375672974058777 ) ) ;
#197007 = CARTESIAN_POINT ( 'NONE',  ( -5.330290668828105538, 6.247702530834755130, 1.199719254218452935 ) ) ;
#197008 = CARTESIAN_POINT ( 'NONE',  ( -5.607373391640464888, 5.677249416569920548, -0.2774322056599042852 ) ) ;
#197009 = CARTESIAN_POINT ( 'NONE',  ( 4.201511661969238531, 1.892856375164463367, -0.9562558712687405649 ) ) ;
#197010 = CARTESIAN_POINT ( 'NONE',  ( 5.427194451788625251, 7.548169490501462242, -1.275334042231127230 ) ) ;
#197011 = CARTESIAN_POINT ( 'NONE',  ( 2.813125141109920069, 1.117832431973438734, -1.678005364621336426 ) ) ;
#197012 = CARTESIAN_POINT ( 'NONE',  ( -6.195713011320804320, 7.291048603704809672, -1.082531754730543083 ) ) ;
#197013 = CARTESIAN_POINT ( 'NONE',  ( 4.788207028248289809, -1.043783763870303360, 1.944324211313207318 ) ) ;
#197014 = CARTESIAN_POINT ( 'NONE',  ( -1.642778471875000035, -0.6052083328553746755, -2.845375778867859751 ) ) ;
#197015 = CARTESIAN_POINT ( 'NONE',  ( -11.81900460097218186, 12.34242865125860078, 1.592493057836596115 ) ) ;
#197016 = CARTESIAN_POINT ( 'NONE',  ( -7.533490631048818109, 8.818102486758951031, -1.199719254218452047 ) ) ;
#197018 = DIRECTION ( 'NONE',  ( -0.000000000000000000, -0.000000000000000000, 1.000000000000000000 ) ) ;
#197017 = CARTESIAN_POINT ( 'NONE',  ( -5.426384371074921553, 7.636973626576035734, -1.343385757368668498 ) ) ;
#197019 = ORIENTED_EDGE ( 'NONE', *, *, #24813, .F. ) ;
#197020 = CARTESIAN_POINT ( 'NONE',  ( 4.891509840769978190, 1.525608517091806782, 1.385742337522611223 ) ) ;
#197021 = CARTESIAN_POINT ( 'NONE',  ( -6.238160075619175515, 10.29195416494877513, 0.000000000000000000 ) ) ;
#197022 = CARTESIAN_POINT ( 'NONE',  ( -0.2108831679770960255, -0.001785917861228669690, -1.896958272444612792 ) ) ;
#197023 = CARTESIAN_POINT ( 'NONE',  ( -6.064574784014443942, 5.969758757638621738, -0.7998128361456291469 ) ) ;
#197024 = CARTESIAN_POINT ( 'NONE',  ( 3.686198542540094714, 1.123799323442754572, 1.677924191584168501 ) ) ;
#197025 = CARTESIAN_POINT ( 'NONE',  ( 1.499999999999985123, -0.2041666666666457353, -0.8660254037844323793 ) ) ;
#197026 = CARTESIAN_POINT ( 'NONE',  ( 9.788623719386617239, 11.48277776311499387, -1.082531754730537088 ) ) ;
#197027 = CARTESIAN_POINT ( 'NONE',  ( 5.459129407796876166, 9.520734742405036144, 1.040834085586084257E-14 ) ) ;
#197028 = CARTESIAN_POINT ( 'NONE',  ( 3.045831416509756195, 0.7432089164593397301, -1.922393172558758634 ) ) ;
#197029 = CARTESIAN_POINT ( 'NONE',  ( 0.000000000000000000, 5.000000000000000888, 0.000000000000000000 ) ) ;
#197030 = CARTESIAN_POINT ( 'NONE',  ( 5.250031796989762967, 7.148123067953287446, 1.599625672291267398 ) ) ;
#197031 =( GEOMETRIC_REPRESENTATION_CONTEXT ( 3 ) GLOBAL_UNCERTAINTY_ASSIGNED_CONTEXT ( ( #139483 ) ) GLOBAL_UNIT_ASSIGNED_CONTEXT ( ( #111266, #210816, #113403 ) ) REPRESENTATION_CONTEXT ( 'NONE', 'WORKASPACE' ) );
#197033 = ORIENTED_EDGE ( 'NONE', *, *, #205891, .T. ) ;
#197032 = CARTESIAN_POINT ( 'NONE',  ( -0.2408018239684097672, 5.720833683022617855, -2.694520676430669059 ) ) ;
#197034 = CARTESIAN_POINT ( 'NONE',  ( 0.9371597039556851527, 0.7481776565299683712, -1.682445429299509909 ) ) ;
#197035 = CARTESIAN_POINT ( 'NONE',  ( 0.3644775225865644619, 2.281660525247240834, -0.3449698035877246105 ) ) ;
#197036 = CARTESIAN_POINT ( 'NONE',  ( 7.374709211190586089, 7.568525266002632534, 0.000000000000000000 ) ) ;
#197037 = CARTESIAN_POINT ( 'NONE',  ( 2.952577552874091626, 0.7252333659365679530, 2.036452211405047397 ) ) ;
#197038 = CARTESIAN_POINT ( 'NONE',  ( -4.663641653420935285, 5.503632019488245319, 1.082531754730560403 ) ) ;
#197039 = CARTESIAN_POINT ( 'NONE',  ( 2.044158018538293042, 0.8666093899718421145, 1.820985203412978093 ) ) ;
#197040 = CARTESIAN_POINT ( 'NONE',  ( 2.759436883174094746, -2.292065780239035178, -0.1713596109048869109 ) ) ;
#197041 = DIRECTION ( 'NONE',  ( -0.7592566023652994600, -0.6507913734559651608, -0.000000000000000000 ) ) ;
#197042 = CARTESIAN_POINT ( 'NONE',  ( 0.6548940681232479077, -1.578012236938080015, -1.004313744925364071 ) ) ;
#197043 = CARTESIAN_POINT ( 'NONE',  ( 5.102397915883716273, -0.6633297369818305089, -1.856656708325474581 ) ) ;
#197044 = CARTESIAN_POINT ( 'NONE',  ( 4.434779938697545276, -1.616694733667634942, 1.205040202231235869 ) ) ;
#197046 = CARTESIAN_POINT ( 'NONE',  ( 8.717529583462633624, 13.11427558077437894, 0.7216878364870438212 ) ) ;
#197045 = CARTESIAN_POINT ( 'NONE',  ( -0.6823417656250212460, 3.801041667008085767, 1.181850606188767472 ) ) ;
#197048 = CARTESIAN_POINT ( 'NONE',  ( 5.760410450299061402, 0.8521563956989952615, 1.926159629354136316 ) ) ;
#197047 = CARTESIAN_POINT ( 'NONE',  ( -6.847031270101295419, 7.946956888995021728, -1.199719254218446718 ) ) ;
#197049 = CARTESIAN_POINT ( 'NONE',  ( 6.443811375169310907, 1.424792453395683500, 1.502365266013883538 ) ) ;
#197050 = CARTESIAN_POINT ( 'NONE',  ( 6.654354466208897811, 6.657835053532175529, 0.7998128361456341429 ) ) ;
#197051 = CARTESIAN_POINT ( 'NONE',  ( -5.052384799386910430, 9.046199365926717917, 1.214306433183764966E-14 ) ) ;
#197052 = CARTESIAN_POINT ( 'NONE',  ( 6.539320575229278454, 0.5749733277502915296, 2.156147827957733742 ) ) ;
#197053 = CARTESIAN_POINT ( 'NONE',  ( 5.871354875427445386, -1.734483768580237673, -1.034654692648151464 ) ) ;
#197054 = CARTESIAN_POINT ( 'NONE',  ( -1.500000000000013101, -0.04791666598384902026, 0.8660254037844403729 ) ) ;
#197055 = CARTESIAN_POINT ( 'NONE',  ( 2.895503172138352177, 1.978892393434032559, -1.186989842046539234 ) ) ;
#197056 = CARTESIAN_POINT ( 'NONE',  ( 1.674751860914457824, 1.388166878297650397, -1.525640323027994683 ) ) ;
#197057 = CARTESIAN_POINT ( 'NONE',  ( 5.978782553946477840, 9.919070713005490703, 1.040834085586084257E-14 ) ) ;
#197058 = EDGE_CURVE ( 'NONE', #127597, #34591, #188553, .T. ) ;
#197059 = CARTESIAN_POINT ( 'NONE',  ( 6.801350335910821165, 7.963938809097990124, 1.199719254218452047 ) ) ;
#197060 = CARTESIAN_POINT ( 'NONE',  ( 6.333594036239346359, 7.418223126147930557, 1.199719254218453823 ) ) ;
#197061 = CARTESIAN_POINT ( 'NONE',  ( 0.6823417656249882723, 0.9885416670080832136, -1.181850606188749264 ) ) ;
#197062 = CARTESIAN_POINT ( 'NONE',  ( 5.225741863424510747, 5.061396693608882558, 0.7998128361456352531 ) ) ;
#197063 = CARTESIAN_POINT ( 'NONE',  ( 5.450014562569148957, 9.302174723065263606, 1.040834085586084257E-14 ) ) ;
#197064 = CARTESIAN_POINT ( 'NONE',  ( 4.246645257758387970, -2.146983142244869747, -0.3225670219409969008 ) ) ;
#197065 = CARTESIAN_POINT ( 'NONE',  ( -1.867619373655151183, -0.8887487162373142180, -2.711732807817992974 ) ) ;
#197067 = CARTESIAN_POINT ( 'NONE',  ( 2.401689157922583640, -0.7064633820979376866, -1.700523668893457296 ) ) ;
#197066 = CARTESIAN_POINT ( 'NONE',  ( -5.097502569058221411, 6.009803087731781623, -1.082531754730544860 ) ) ;
#197068 = B_SPLINE_CURVE_WITH_KNOTS ( 'NONE', 3,
 ( #119969, #185946, #5045, #170779, #72189, #155607 ),
 .UNSPECIFIED., .F., .F.,
 ( 4, 2, 4 ),
 ( 0.000000000000000000, 3.619701867372329955E-05, 7.239403734744659911E-05 ),
 .UNSPECIFIED. ) ;
#197069 = CARTESIAN_POINT ( 'NONE',  ( 0.6823417656249899377, 4.176041667008085767, -1.181850606188754593 ) ) ;
#197070 = CARTESIAN_POINT ( 'NONE',  ( 4.880524338131243312, -0.2681524694418158661, -2.175044001020635331 ) ) ;
#197071 = CARTESIAN_POINT ( 'NONE',  ( 8.118347949970196709, 14.25971613632666823, 8.777447096691743056 ) ) ;
#197072 = CARTESIAN_POINT ( 'NONE',  ( 5.541944591929171438, 0.9225863094920858654, -2.066052574227566385 ) ) ;
#197073 = CARTESIAN_POINT ( 'NONE',  ( -5.830469385422084372, 6.191968629596825480, -0.9632026293319171373 ) ) ;
#197074 = CARTESIAN_POINT ( 'NONE',  ( 4.597299534708283453, 8.487268731053720927, 0.09294953129799360392 ) ) ;
#197075 = AXIS2_PLACEMENT_3D ( 'NONE', #95077, #12712, #33243 ) ;
#197076 = CARTESIAN_POINT ( 'NONE',  ( -6.414416072596857532, 6.656109304217339151, -0.7216878364870338292 ) ) ;
#197077 = CARTESIAN_POINT ( 'NONE',  ( 5.912764389335563919, 6.070849007079172743, -0.7216878364870458196 ) ) ;
#197078 = CARTESIAN_POINT ( 'NONE',  ( 6.872329512321287304, -1.085958120241878877, 1.397742320866280252 ) ) ;
#197079 = CARTESIAN_POINT ( 'NONE',  ( 3.861980204584365861, 0.6760143841026149403, -1.896330825423567568 ) ) ;
#197080 = CARTESIAN_POINT ( 'NONE',  ( 6.714312387265682247, 8.856450423275211037, 1.599625672291281386 ) ) ;
#197081 = CARTESIAN_POINT ( 'NONE',  ( 2.995255089933103854, 1.807040913553149997, -1.081249443666182808 ) ) ;
#197082 = CARTESIAN_POINT ( 'NONE',  ( 1.810024464468898309, 1.101340386757416967, -1.567151550741460397 ) ) ;
#197083 = CARTESIAN_POINT ( 'NONE',  ( 3.602716132929354664, 5.226254793216122074, 1.599625672291267398 ) ) ;
#197084 = CARTESIAN_POINT ( 'NONE',  ( 3.121499051359075239, 0.2915335129191589103, -1.947736612120597455 ) ) ;
#197085 = CARTESIAN_POINT ( 'NONE',  ( 0.4791068267422092797, 1.747065859276742072, -0.6691465683838908607 ) ) ;
#197086 = CARTESIAN_POINT ( 'NONE',  ( 1.205434515183744226, -1.544416933936803904, -1.209700862059132964 ) ) ;
#197088 = ORIENTED_EDGE ( 'NONE', *, *, #60315, .F. ) ;
#197087 = CARTESIAN_POINT ( 'NONE',  ( 0.5801457039020865292, 0.9447208859736742070, 1.662703529197881558 ) ) ;
#197089 = CARTESIAN_POINT ( 'NONE',  ( 5.992340707560163793, 6.093411701682730275, 0.7216878364870317197 ) ) ;
#197090 = CARTESIAN_POINT ( 'NONE',  ( -0.6823417656250003738, 0.2802083336747515641, -1.181850606188749264 ) ) ;
#197091 = CARTESIAN_POINT ( 'NONE',  ( 11.41108574530281494, 12.34163144622374375, -3.405883542057589253 ) ) ;
#197092 = CARTESIAN_POINT ( 'NONE',  ( 2.535011536075338689, 5.133042487381368701, -0.9999999999999956701 ) ) ;
#197093 = CARTESIAN_POINT ( 'NONE',  ( 6.719590346122157776, 0.3599300073104904074, -2.038585587018165945 ) ) ;
#197094 = CARTESIAN_POINT ( 'NONE',  ( 0.6079806153083644471, 0.6509857562557037625, -1.965403638620793147 ) ) ;
#197095 = CARTESIAN_POINT ( 'NONE',  ( 1.499999999999987121, 2.295833333333350268, -0.8660254037844262731 ) ) ;
#197096 = CARTESIAN_POINT ( 'NONE',  ( 5.829115978871627135, 8.888053511070525659, 1.199719254218462483 ) ) ;
#197097 = CARTESIAN_POINT ( 'NONE',  ( -8.097244055859620815, 10.46987070330147063, -1.599625672291263179 ) ) ;
#197098 = CARTESIAN_POINT ( 'NONE',  ( 4.369470645354133431, 8.319742529546998000, 0.7998128361456271485 ) ) ;
#197099 = CARTESIAN_POINT ( 'NONE',  ( 5.901066629635802308, -0.3109326959268610691, -2.097457242586676429 ) ) ;
#197100 = CARTESIAN_POINT ( 'NONE',  ( 5.435893244436359240, 5.306573304789342416, -0.7998128361456481317 ) ) ;
#197101 = EDGE_CURVE ( 'NONE', #130319, #80292, #147611, .T. ) ;
#197102 = CARTESIAN_POINT ( 'NONE',  ( 0.6823417656249882723, 1.426041667008083547, -1.181850606188749264 ) ) ;
#197103 = ORIENTED_EDGE ( 'NONE', *, *, #31466, .F. ) ;
#197104 = CARTESIAN_POINT ( 'NONE',  ( 0.7499999999999902300, 1.983333333333357817, 1.299038105676669330 ) ) ;
#197106 = CARTESIAN_POINT ( 'NONE',  ( 3.011882680530176604, 6.665613560593854459, 0.7998128361456341429 ) ) ;
#197105 = CARTESIAN_POINT ( 'NONE',  ( 6.074655751228532630, 1.318658252384183438, -1.452748870126779890 ) ) ;
#197107 = ADVANCED_FACE ( 'NONE', ( #1054 ), #206337, .F. ) ;
#197108 = CARTESIAN_POINT ( 'NONE',  ( 4.587267430073429963, 1.242536178122002344, -1.587594670648798445 ) ) ;
#197109 = CARTESIAN_POINT ( 'NONE',  ( 3.309697661505988986, -1.145383095959727315, -1.535415057543190409 ) ) ;
#197110 = CARTESIAN_POINT ( 'NONE',  ( 0.000000000000000000, 3.466143782776612170, 0.000000000000000000 ) ) ;
#197111 = CARTESIAN_POINT ( 'NONE',  ( 2.033021410476544943, -1.955939774129427988, 0.9887309579383956049 ) ) ;
#197112 = DIRECTION ( 'NONE',  ( 0.000000000000000000, 1.000000000000000000, -8.546850786086437571E-32 ) ) ;
#197113 = CARTESIAN_POINT ( 'NONE',  ( 3.743291833738107144, -1.414529149469236691, -1.224010458943748603 ) ) ;
#197114 = CARTESIAN_POINT ( 'NONE',  ( -1.402160292154681736E-14, -1.006249999317181620, 1.732050807568877637 ) ) ;
#197115 = CARTESIAN_POINT ( 'NONE',  ( -5.208303565944065738, 9.228104593576741621, -0.7998128361456231517 ) ) ;
#197116 = EDGE_CURVE ( 'NONE', #63111, #152681, #202448, .T. ) ;
#197118 = CARTESIAN_POINT ( 'NONE',  ( 5.290659027526918301, 1.602671996148979483, -1.383575156158120878 ) ) ;
#197117 = CARTESIAN_POINT ( 'NONE',  ( -3.416291520963659512, 5.969128626890772615, 1.082531754730560403 ) ) ;
#197119 = CARTESIAN_POINT ( 'NONE',  ( -0.9215813951549834959, 13.25030900364159336, -1.183391796694308828 ) ) ;
#197121 = CARTESIAN_POINT ( 'NONE',  ( -5.610041701004606196, 9.767075427805856691, -0.7998128361456362523 ) ) ;
#197120 = CARTESIAN_POINT ( 'NONE',  ( 1.857086946601906652, 0.3542020299988774545, -2.060351931225719468 ) ) ;
#197123 = ORIENTED_EDGE ( 'NONE', *, *, #2690, .F. ) ;
#197122 = CARTESIAN_POINT ( 'NONE',  ( 0.9380131109506375520, 1.698111720264935620, 0.3011209518388803241 ) ) ;
#197124 = CARTESIAN_POINT ( 'NONE',  ( 5.991813822235618758, 9.077867661661846554, 1.199719254218462483 ) ) ;
#197125 = FILL_AREA_STYLE ('',( #2094 ) ) ;
#197126 = CARTESIAN_POINT ( 'NONE',  ( 0.08522810233020440551, -9.999176686163549377, 9.579508557966974536 ) ) ;
#197127 = DIRECTION ( 'NONE',  ( -0.6483454320283799088, 0.000000000000000000, 0.7613463080411786432 ) ) ;
#197129 = CARTESIAN_POINT ( 'NONE',  ( 9.042925270190625753, 11.57316545335434199, 1.443375672974076540 ) ) ;
#197128 = CARTESIAN_POINT ( 'NONE',  ( 5.524057522564145728, 8.532151978711786100, 1.199719254218462483 ) ) ;
#197130 = LINE ( 'NONE', #48768, #16651 ) ;
#197132 = CARTESIAN_POINT ( 'NONE',  ( 1.611653755202663518, -0.6102688749147866520, 1.705724428093706946 ) ) ;
#197131 = CARTESIAN_POINT ( 'NONE',  ( 5.987861119090863049, 7.014868056141362551, 1.199719254218452047 ) ) ;
#197133 = CARTESIAN_POINT ( 'NONE',  ( -7.528855374290365887, 7.678086112960552434, -0.7998128361456291469 ) ) ;
#197134 = CARTESIAN_POINT ( 'NONE',  ( 3.897079088924235712, 6.634010472798538949, 1.199719254218462483 ) ) ;
#197135 = CARTESIAN_POINT ( 'NONE',  ( 5.956828388357757298, 8.042995434541133193, 1.599625672291269396 ) ) ;
#197136 = CARTESIAN_POINT ( 'NONE',  ( 6.539320575229250920, 3.702490941164796379, 2.411252750440337156 ) ) ;
#197137 =( NAMED_UNIT ( * ) PLANE_ANGLE_UNIT ( ) SI_UNIT ( $, .RADIAN. ) );
#197138 = CARTESIAN_POINT ( 'NONE',  ( 4.285325189395043033, 7.238007417033815116, 0.9681492361576886641 ) ) ;
#197139 = CARTESIAN_POINT ( 'NONE',  ( 9.761507412159302177, 10.49077285704843199, -0.7216878364870257245 ) ) ;
#197140 = EDGE_LOOP ( 'NONE', ( #138259, #207906, #91763, #19944 ) ) ;
#197141 = COLOUR_RGB ( '', 0.31764706, 0.68627451, 0.89019608) ;
#197142 = CARTESIAN_POINT ( 'NONE',  ( 3.402650393365719506, 0.4499446578831092780, 1.805719076957598368 ) ) ;
#197143 = CARTESIAN_POINT ( 'NONE',  ( 0.9838322988516207124, -1.915793139027978542, 0.001352086710114385869 ) ) ;
#197144 = CARTESIAN_POINT ( 'NONE',  ( 6.686557393816916495, -1.889396554722815758, -0.3748701224956552669 ) ) ;
#197145 = CARTESIAN_POINT ( 'NONE',  ( 5.916483165358987328, 0.8355632440216669288, 1.894440869009452300 ) ) ;
#197146 = ADVANCED_FACE ( 'NONE', ( #150552 ), #133861, .T. ) ;
#197147 = CARTESIAN_POINT ( 'NONE',  ( 4.615647837050825153, 8.347533190886938570, 0.2882115401751338402 ) ) ;
#197148 = DIRECTION ( 'NONE',  ( 1.000000000000000000, 0.000000000000000000, 0.000000000000000000 ) ) ;
#197149 = DIRECTION ( 'NONE',  ( 0.9632918427306580433, 0.000000000000000000, -0.2684563758389303945 ) ) ;
#197150 = CARTESIAN_POINT ( 'NONE',  ( 9.734391104931955141, 10.45913716528321125, 0.7216878364870438212 ) ) ;
#197151 = CARTESIAN_POINT ( 'NONE',  ( 4.662928361469391270, 1.524974937183399160, -1.246301010749743199 ) ) ;
#197152 = CARTESIAN_POINT ( 'NONE',  ( 1.735180256192244697, 1.979698633766859617, 0.7602586827493148514 ) ) ;
#197153 = CARTESIAN_POINT ( 'NONE',  ( -4.218558352146454915, 8.073401844146177453, 1.040834085586084257E-14 ) ) ;
#197154 = CARTESIAN_POINT ( 'NONE',  ( -11.52546672121288296, 8.148966486963653111, -3.186023502380144645 ) ) ;
#197155 = DIRECTION ( 'NONE',  ( 0.000000000000000000, 0.000000000000000000, -1.000000000000000000 ) ) ;
#197156 = CARTESIAN_POINT ( 'NONE',  ( 5.736325210887869730, 0.4244523575273988492, 2.149783713274712404 ) ) ;
#197157 = DIRECTION ( 'NONE',  ( 0.000000000000000000, -1.000000000000000000, 0.000000000000000000 ) ) ;
#197158 = CARTESIAN_POINT ( 'NONE',  ( 4.331023931135844940, 0.09395156538319178463, 1.924209479612617235 ) ) ;
#197159 = CARTESIAN_POINT ( 'NONE',  ( -6.205881626753225966, 8.263281202677319470, 1.599625672291283607 ) ) ;
#197160 = DIRECTION ( 'NONE',  ( -1.000000000000000000, 5.578564026256504688E-16, 0.000000000000000000 ) ) ;
#197161 = CARTESIAN_POINT ( 'NONE',  ( 0.6455096168876961471, -1.890800792967793686, 1.137844069391671820 ) ) ;
#197162 = CARTESIAN_POINT ( 'NONE',  ( 0.000000000000000000, 2.480000000000016858, 0.000000000000000000 ) ) ;
#197163 = CARTESIAN_POINT ( 'NONE',  ( -0.2376451031371414890, -9.050179744156148232, 9.497303347810662544 ) ) ;
#197164 = ORIENTED_EDGE ( 'NONE', *, *, #181495, .T. ) ;
#197165 = CARTESIAN_POINT ( 'NONE',  ( -10.50000000000000000, 0.000000000000000000, 3.599999999999999201 ) ) ;
#197166 = ORIENTED_EDGE ( 'NONE', *, *, #149738, .T. ) ;
#197167 = CARTESIAN_POINT ( 'NONE',  ( 6.280130250669472503, -1.091077088088190372, -1.639371140202023014 ) ) ;
#197168 = CARTESIAN_POINT ( 'NONE',  ( 0.9427985035241670531, -1.531986193156938292, -1.193500027965375354 ) ) ;
#197169 = CARTESIAN_POINT ( 'NONE',  ( 6.819654193105592732, -1.783474119298094296, 1.449237643660877151 ) ) ;
#197171 = CARTESIAN_POINT ( 'NONE',  ( 5.805462856137336480, -1.465901670865896067, -1.146230774367855254 ) ) ;
#197170 = CARTESIAN_POINT ( 'NONE',  ( -5.284646014276622950, 9.387447126623207794, -0.7998128361456362523 ) ) ;
#197172 = CARTESIAN_POINT ( 'NONE',  ( 5.417364897112183719, 8.477953592343014932, 1.199719254218451159 ) ) ;
#197173 = CARTESIAN_POINT ( 'NONE',  ( 1.220146605508150803E-14, 11.43749999999999822, -1.499999999999998446 ) ) ;
#197174 = CARTESIAN_POINT ( 'NONE',  ( 3.840479349152599919, 7.346192795665340114, 0.4818892653144311033 ) ) ;
#197175 = CARTESIAN_POINT ( 'NONE',  ( -4.693093728624763372, 8.627026450037540428, 0.7998128361456481317 ) ) ;
#197176 = CARTESIAN_POINT ( 'NONE',  ( -3.336159340019098973, -0.9254121791666594099, 0.08595556041762617006 ) ) ;
#197177 = CARTESIAN_POINT ( 'NONE',  ( 0.9607770615731696662, -1.983481723135366304, -0.9323335341336475013 ) ) ;
#197178 = CARTESIAN_POINT ( 'NONE',  ( 3.850152436600926542, 7.435668909435648288, -0.7216878364870197293 ) ) ;
#197179 = CARTESIAN_POINT ( 'NONE',  ( 1.163414459189984696E-15, 7.849261790823902629, -9.499999999999992895 ) ) ;
#197180 = DIRECTION ( 'NONE',  ( 0.000000000000000000, 0.000000000000000000, 1.000000000000000000 ) ) ;
#197181 = CARTESIAN_POINT ( 'NONE',  ( 1.471042373949003501, 0.1361147407585860392, -1.820667060309004937 ) ) ;
#197182 = CARTESIAN_POINT ( 'NONE',  ( -2.286521462199063492, 5.819358805874190743, 1.040834085586084257E-14 ) ) ;
#197183 = CARTESIAN_POINT ( 'NONE',  ( -0.4135277324232147222, 2.752648330311642688, -1.957052666557069109 ) ) ;
#197184 = CARTESIAN_POINT ( 'NONE',  ( 6.509000000000012776, 6.036089120385641493, 2.694901645009006863 ) ) ;
#197185 = CARTESIAN_POINT ( 'NONE',  ( 9.541187415715040032, 12.15447128979948310, -1.599625672291262513 ) ) ;
#197186 = CARTESIAN_POINT ( 'NONE',  ( 6.428339884752386268, 1.046657586246093175, -1.495688092090130095 ) ) ;
#197187 = CARTESIAN_POINT ( 'NONE',  ( 4.434394140398959294, -1.132915509570767476, 1.601352629973289199 ) ) ;
#197188 = CARTESIAN_POINT ( 'NONE',  ( -8.097244055859620815, 10.46987070330147063, -1.599625672291263179 ) ) ;
#197189 = CARTESIAN_POINT ( 'NONE',  ( 4.625302960556422427, 8.547937220624488575, 1.040834085586084257E-14 ) ) ;
#197190 = CARTESIAN_POINT ( 'NONE',  ( 5.250683377293950294, 2.089169806880130320, 0.3621421040747307973 ) ) ;
#197191 = CARTESIAN_POINT ( 'NONE',  ( 4.142245973918059043, 0.5854081421233224836, 2.111838497463234710 ) ) ;
#197192 = CARTESIAN_POINT ( 'NONE',  ( 5.834086172582112262, 5.700855377634248100, 1.040834085586084257E-14 ) ) ;
#197193 = CARTESIAN_POINT ( 'NONE',  ( 3.133707330959301096, 1.967300496787489639, -0.6450458050009516553 ) ) ;
#197195 = CARTESIAN_POINT ( 'NONE',  ( -1.402160292154681736E-14, 0.1343750003414218575, 1.575800808251672791 ) ) ;
#197194 = CARTESIAN_POINT ( 'NONE',  ( 1.806654366501771136, 2.518449987798942136, 2.499999999999998668 ) ) ;
#197196 = ORIENTED_EDGE ( 'NONE', *, *, #159826, .T. ) ;
#197197 = CARTESIAN_POINT ( 'NONE',  ( 3.217717873326145117, 2.243214920517083044, 0.5014430322199947554 ) ) ;
#197198 = CARTESIAN_POINT ( 'NONE',  ( 7.266807147244743526, 11.42176607185347414, -0.7216878364870267237 ) ) ;
#197200 = CARTESIAN_POINT ( 'NONE',  ( -3.285556943749998737, -1.130208332855377140, 1.896917185911908499 ) ) ;
#197199 = CARTESIAN_POINT ( 'NONE',  ( 7.214347136247488912, 7.589362211809770997, -0.7216878364870317197 ) ) ;
#197201 = CARTESIAN_POINT ( 'NONE',  ( 6.720655732516647163, 0.002698097948191854455, 1.926293798961113080 ) ) ;
#197202 = CARTESIAN_POINT ( 'NONE',  ( -10.04024307340833566, 4.584664385129866737, -6.492703511775993697 ) ) ;
#197203 = CARTESIAN_POINT ( 'NONE',  ( 3.292849172082324305, 1.531446531863265736, 1.193990500783614905 ) ) ;
#197204 = ORIENTED_EDGE ( 'NONE', *, *, #193907, .T. ) ;
#197205 = LINE ( 'NONE', #30465, #180934 ) ;
#197206 = CARTESIAN_POINT ( 'NONE',  ( 3.586107075002854305, 1.066394011600999780, 1.587261316105821551 ) ) ;
#197207 = PRESENTATION_STYLE_ASSIGNMENT (( #81336 ) ) ;
#197208 = CARTESIAN_POINT ( 'NONE',  ( 5.034089265250761613, 0.8841871275974706457, -1.480748092288231454 ) ) ;
#197209 = CARTESIAN_POINT ( 'NONE',  ( 3.397672961473942266, -1.985868886743065609, 0.3494831190506141883 ) ) ;
#197210 = CARTESIAN_POINT ( 'NONE',  ( 4.694093285409329575, 1.999278280869060342, 1.134256664920972213 ) ) ;
#197211 = CARTESIAN_POINT ( 'NONE',  ( -2.788906526875773208E-15, 11.18749999999999822, -1.499999999999998446 ) ) ;
#197212 = CARTESIAN_POINT ( 'NONE',  ( 1.243116305521356990, 0.4334984505205765060, 2.163720904216937857 ) ) ;
#197213 = CARTESIAN_POINT ( 'NONE',  ( -5.153507786970285665, 5.185049637652990207, -0.7216878364870338292 ) ) ;
#197214 = CARTESIAN_POINT ( 'NONE',  ( 5.887929786387328335, -0.7941975946151798027, 1.581623468068603433 ) ) ;
#197216 = CARTESIAN_POINT ( 'NONE',  ( 2.133172796342793998, -2.046422403899459841, 1.032916798664377911 ) ) ;
#197215 = CARTESIAN_POINT ( 'NONE',  ( 5.306037014901791693, 7.283738832175834510, 1.599625672291269396 ) ) ;
#197217 = CARTESIAN_POINT ( 'NONE',  ( 0.7436347644121766853, 0.5012835123295921180, 1.666554394910790382 ) ) ;
#197218 = CARTESIAN_POINT ( 'NONE',  ( 0.5151702941667745117, 4.156692335018007611, 0.3998358608512675438 ) ) ;
#197219 = CARTESIAN_POINT ( 'NONE',  ( -5.354544322754380303, 5.211666229493680191, 0.7998128361456281477 ) ) ;
#197220 = CARTESIAN_POINT ( 'NONE',  ( 1.360316468750007779, 1.296875000341410455, -2.602085213965210642E-14 ) ) ;
#197221 = CARTESIAN_POINT ( 'NONE',  ( -11.86145017354119879, 13.50485634456125261, -1.100000000000000533 ) ) ;
#197222 =( BOUNDED_SURFACE ( )  B_SPLINE_SURFACE ( 3, 2, ( 
 ( #185336, #118282, #20693 ),
 ( #82508, #148595, #36960 ),
 ( #99841, #68375, #164 ),
 ( #184267, #35892, #168037 ),
 ( #19640, #120428, #69441 ),
 ( #66231, #149659, #133440 ) ),
 .UNSPECIFIED., .F., .F., .F. ) 
 B_SPLINE_SURFACE_WITH_KNOTS ( ( 4, 2, 4 ),
 ( 3, 3 ),
 ( 0.000000000000000000, 0.0003766365702389428338, 0.0007532731404778856676 ),
 ( 0.000000000000000000, 1.000000000000000000 ),
 .UNSPECIFIED. ) 
 GEOMETRIC_REPRESENTATION_ITEM ( )  RATIONAL_B_SPLINE_SURFACE ( (
 ( 1.000000000000000000, 0.7452309222762957264, 1.000000000000000000),
 ( 1.000000000000000000, 0.7451892422674365468, 1.000000000000000000),
 ( 1.000000000000000000, 0.7429606254235103791, 1.000000000000000000),
 ( 1.000000000000000000, 0.7311462761269298394, 1.000000000000000000),
 ( 1.000000000000000000, 0.7212257702788642533, 1.000000000000000000),
 ( 1.000000000000000000, 0.7071067811865551223, 1.000000000000000000) ) ) 
 REPRESENTATION_ITEM ( '' )  SURFACE ( )  );
#197223 = CARTESIAN_POINT ( 'NONE',  ( 1.627621631281210179, 0.1606834768266463820, -2.165304058017766486 ) ) ;
#197224 = CARTESIAN_POINT ( 'NONE',  ( 1.833220611596135363, -1.622487599052296670, -1.197302888167578683 ) ) ;
#197225 = CARTESIAN_POINT ( 'NONE',  ( 1.499999999999989120, 0.5562500006828161592, 0.000000000000000000 ) ) ;
#197226 = CARTESIAN_POINT ( 'NONE',  ( 5.900991307970250510, 1.573582866467116759, -1.111162877451849162 ) ) ;
#197227 = CARTESIAN_POINT ( 'NONE',  ( -1.402160292154681736E-14, 12.92187500034139980, 1.575800808251682339 ) ) ;
#197228 = CARTESIAN_POINT ( 'NONE',  ( 2.109928881651984778, 1.720655366031418332, 1.405045424887063410 ) ) ;
#197229 = VERTEX_POINT ( 'NONE', #67120 ) ;
#197230 = CARTESIAN_POINT ( 'NONE',  ( -9.578206935422265644, -9.900000000000005684, 0.1671882239536719994 ) ) ;
#197231 = CARTESIAN_POINT ( 'NONE',  ( -0.2316791905390819806, 3.431749620889657848, -1.989589857879307866 ) ) ;
#197232 = CARTESIAN_POINT ( 'NONE',  ( 8.380911511541880188, 12.92948053010758258, 0.7998128361456462443 ) ) ;
#197233 = SURFACE_STYLE_FILL_AREA ( #78159 ) ;
#197234 = CARTESIAN_POINT ( 'NONE',  ( 5.530708837500646347, -1.570004293196942013, 0.7514903552788397834 ) ) ;
#197236 = ADVANCED_FACE ( 'NONE', ( #135368 ), #116267, .F. ) ;
#197235 = CARTESIAN_POINT ( 'NONE',  ( 3.842202535371820993, -0.9690557767615382012, 1.705768119890891610 ) ) ;
#197238 = CARTESIAN_POINT ( 'NONE',  ( -6.805829924380121909, 8.963220883242035697, 1.443375672974078761 ) ) ;
#197237 = CARTESIAN_POINT ( 'NONE',  ( 3.822509244049070887, 6.547012320444182798, -1.199719254218452047 ) ) ;
#197239 = CARTESIAN_POINT ( 'NONE',  ( -5.833005281931015418, 6.047509994665502653, 0.4702358434125544773 ) ) ;
#197240 = CARTESIAN_POINT ( 'NONE',  ( 4.499490165225078719, 1.813563011714003803, 1.352382200441957227 ) ) ;
#197241 = CARTESIAN_POINT ( 'NONE',  ( 0.8540550061131615411, -0.7440666694851668650, 1.923960566027690833 ) ) ;
#197242 = CARTESIAN_POINT ( 'NONE',  ( -5.994676475536691029, 10.14553965476814845, 0.7998128361456481317 ) ) ;
#197243 = CARTESIAN_POINT ( 'NONE',  ( -4.894130264408878439, 4.812166184672871161, -0.7216878364870197293 ) ) ;
#197244 = CARTESIAN_POINT ( 'NONE',  ( 2.237552233957947667, -2.020869686619676919, 1.017492276205993695 ) ) ;
#197245 = ORIENTED_EDGE ( 'NONE', *, *, #170654, .T. ) ;
#197246 = CARTESIAN_POINT ( 'NONE',  ( 1.499999999999987121, 1.577083334016150751, -0.8660254037844253849 ) ) ;
#197247 = CARTESIAN_POINT ( 'NONE',  ( 2.635844295777586943, 0.8854499327175249235, -1.647724587607077851 ) ) ;
#197248 = CARTESIAN_POINT ( 'NONE',  ( 1.670155932360503970, 1.196126419257515838, 1.255837360413303738 ) ) ;
#197249 = CARTESIAN_POINT ( 'NONE',  ( 4.968408144156593487, -2.063508908063705238, -0.7385586828293493333 ) ) ;
#197250 = CARTESIAN_POINT ( 'NONE',  ( 6.668959562645871308, -2.105872948262592192, -0.9439719561973120010 ) ) ;
#197251 = CARTESIAN_POINT ( 'NONE',  ( 3.573254463033649131, 0.05508235185803719847, -2.161170636208443963 ) ) ;
#197252 = CARTESIAN_POINT ( 'NONE',  ( 4.927648248775200912, 0.9969592527751047761, -1.666372862991059245 ) ) ;
#197253 = CARTESIAN_POINT ( 'NONE',  ( -2.602802303699316866, 5.980427087717073320, 1.040834085586084257E-14 ) ) ;
#197254 = CARTESIAN_POINT ( 'NONE',  ( 6.485618507650338316, 1.290063292742931633, 1.354747167150817333 ) ) ;
#197255 = CARTESIAN_POINT ( 'NONE',  ( 0.7812500000000006661, 0.7852924748300293967, 1.895863743164072357 ) ) ;
#197256 = CARTESIAN_POINT ( 'NONE',  ( 4.065672160753666553, 7.505179260319745360, -0.5311146244057519672 ) ) ;
#197257 = LINE ( 'NONE', #13180, #124675 ) ;
#197258 = EDGE_CURVE ( 'NONE', #108056, #80159, #125581, .T. ) ;
#197259 = CARTESIAN_POINT ( 'NONE',  ( 0.6801582343749796866, 1.723958333674766141, 1.178068619123784355 ) ) ;
#197260 = CARTESIAN_POINT ( 'NONE',  ( 5.168592345394213972, 1.356298078840772803, 1.492257005506092193 ) ) ;
#197261 = CARTESIAN_POINT ( 'NONE',  ( -2.277406616971334508, 5.600798786534425311, 1.040834085586084257E-14 ) ) ;
#197262 = CARTESIAN_POINT ( 'NONE',  ( 8.769426429940780920, 9.125419011219408461, 0.7998128361456462443 ) ) ;
#197263 = CARTESIAN_POINT ( 'NONE',  ( 3.878514461961128479, 6.682628084666728085, -1.199719254218448494 ) ) ;
#197265 = DIRECTION ( 'NONE',  ( 0.000000000000000000, 1.000000000000000000, 0.000000000000000000 ) ) ;
#197264 = CARTESIAN_POINT ( 'NONE',  ( 2.543341688579534576, -1.352695106659363766, -1.226303905950577366 ) ) ;
#197266 = CARTESIAN_POINT ( 'NONE',  ( -0.1296875068448125057, 1.390030859318210688, -2.083197486262199138 ) ) ;
#197267 = CARTESIAN_POINT ( 'NONE',  ( -7.681709917290613809, -6.443545996361864425, -7.726139724254739605 ) ) ;
#197268 = ORIENTED_EDGE ( 'NONE', *, *, #116150, .T. ) ;
#197269 = CARTESIAN_POINT ( 'NONE',  ( -4.285785955251283141, 8.014184357852876417, 0.000000000000000000 ) ) ;
#197270 = CARTESIAN_POINT ( 'NONE',  ( 3.285556943750000070, -3.521874999522042859, 0.000000000000000000 ) ) ;
#197271 = CARTESIAN_POINT ( 'NONE',  ( -7.472515219426274946, 11.86968485597268064, 0.000000000000000000 ) ) ;
#197272 = CARTESIAN_POINT ( 'NONE',  ( -0.1052055632086721232, -1.960199907271743314, -0.4866737942672630379 ) ) ;
#197273 = CARTESIAN_POINT ( 'NONE',  ( 6.322901860479969827, 1.648133277211549563, -1.489392227938668434 ) ) ;
#197274 = ORIENTED_EDGE ( 'NONE', *, *, #43007, .T. ) ;
#197275 = CARTESIAN_POINT ( 'NONE',  ( -6.961185525973791144, 7.086080966583015339, 0.7998128361456341429 ) ) ;
#197276 = CARTESIAN_POINT ( 'NONE',  ( 5.030238685870051185, 5.827365540725222282, -1.199719254218452047 ) ) ;
#197277 = CARTESIAN_POINT ( 'NONE',  ( 6.526252491562488878, 1.188822440972692185, -1.683233108126303446 ) ) ;
#197278 = CARTESIAN_POINT ( 'NONE',  ( 5.238907797441370029, 2.013986022392059816, -0.1017483359899013229 ) ) ;
#197279 = ORIENTED_EDGE ( 'NONE', *, *, #168859, .F. ) ;
#197280 = VERTEX_POINT ( 'NONE', #206735 ) ;
#197281 = ORIENTED_EDGE ( 'NONE', *, *, #204645, .F. ) ;
#197282 = CARTESIAN_POINT ( 'NONE',  ( -8.459397779922852578, 11.95671561229694824, 1.199719254218453823 ) ) ;
#197283 = CARTESIAN_POINT ( 'NONE',  ( -0.6125000000000019318, 0.2708333340161322988, -1.060881119635941339 ) ) ;
#197284 =( BOUNDED_CURVE ( )  B_SPLINE_CURVE ( 2, ( #209390, #41609, #75155, #40531, #106635, #91425, #28537, #127195, #56767 ),
 .UNSPECIFIED., .F., .T. ) 
 B_SPLINE_CURVE_WITH_KNOTS ( ( 3, 2, 2, 2, 3 ),
 ( 0.3593749999999997224, 0.3645833333333333148, 0.3750000000000000000, 0.3854166666666666852, 0.3906250000000002220 ),
 .UNSPECIFIED. ) 
 CURVE ( )  GEOMETRIC_REPRESENTATION_ITEM ( )  RATIONAL_B_SPLINE_CURVE ( ( 0.9330127018922194093, 0.9330127018922158566, 1.000000000000000000, 0.8660254037844387076, 1.000000000000000000, 0.8660254037844387076, 1.000000000000000000, 0.9330127018922165227, 0.9330127018922194093 ) ) 
 REPRESENTATION_ITEM ( '' )  );
#197287 = EDGE_LOOP ( 'NONE', ( #83535, #107441, #43739 ) ) ;
#197286 = CARTESIAN_POINT ( 'NONE',  ( -1.257539916218606724, 3.172412844624492134, -0.7749999999999918066 ) ) ;
#197285 = CARTESIAN_POINT ( 'NONE',  ( -4.444040490229335560, 8.406740681901359480, 0.7998128361456352531 ) ) ;
#197288 = CARTESIAN_POINT ( 'NONE',  ( 6.090086331970060662, 7.118959255344424086, 1.132899493623270359 ) ) ;
#197289 = CARTESIAN_POINT ( 'NONE',  ( 5.483749906247235906, 1.861732415968733401, 0.7741956105717237024 ) ) ;
#197290 = CARTESIAN_POINT ( 'NONE',  ( 4.751808913491627706, 0.7073710267669359730, 1.700028372310140368 ) ) ;
#197291 = CARTESIAN_POINT ( 'NONE',  ( -0.5773502691896261751, -4.295408888568413630, -0.9999999999999991118 ) ) ;
#197292 = CARTESIAN_POINT ( 'NONE',  ( 3.756711156304150201, 0.8293906405268698379, 2.153668854807685662 ) ) ;
#197293 = CARTESIAN_POINT ( 'NONE',  ( 6.801350335910821165, 7.963938809097990124, 1.199719254218452047 ) ) ;
#197294 = CARTESIAN_POINT ( 'NONE',  ( 5.589210384452774960, 1.909260796540311000, -1.013481389624170115 ) ) ;
#197295 = CARTESIAN_POINT ( 'NONE',  ( 7.955937213120826357, 8.176348258262782664, 0.7998128361456481317 ) ) ;
#197296 = CARTESIAN_POINT ( 'NONE',  ( 1.522887052880964598, -1.828065777178315532, 0.6558840488102948285 ) ) ;
#197297 = CARTESIAN_POINT ( 'NONE',  ( -2.774614992291035698, 6.388801257648172971, 1.040834085586084257E-14 ) ) ;
#197298 = EDGE_LOOP ( 'NONE', ( #125199, #23329, #18213, #132754 ) ) ;
#197299 = CIRCLE ( 'NONE', #10519, 0.7500000000000011102 ) ;
#197300 = CARTESIAN_POINT ( 'NONE',  ( 4.271116411733427043, -2.292556078035115075, 0.1642532200917065921 ) ) ;
#197301 = CARTESIAN_POINT ( 'NONE',  ( -9.342754679277470942, 15.44694753537003962, -7.460282140120185090 ) ) ;
#197302 = CARTESIAN_POINT ( 'NONE',  ( -4.411198876399886615, 6.239761003923544713, -1.599625672291271394 ) ) ;
#197303 = CARTESIAN_POINT ( 'NONE',  ( 3.203821283898714345, -1.868584281295191607, 0.09040415888627445495 ) ) ;
#197304 = B_SPLINE_CURVE_WITH_KNOTS ( 'NONE', 3,
 ( #158748, #25534, #206417, #159808, #125264, #77487 ),
 .UNSPECIFIED., .F., .F.,
 ( 4, 2, 4 ),
 ( 0.000000000000000000, 0.0003767011250903910184, 0.0007534022501807820368 ),
 .UNSPECIFIED. ) ;
#197307 = CARTESIAN_POINT ( 'NONE',  ( -6.343235766347277149, 8.493804042195527870, -1.599625672291271394 ) ) ;
#197306 = CARTESIAN_POINT ( 'NONE',  ( 0.7499999999999867883, -0.1520833326505155458, -1.299038105676652899 ) ) ;
#197305 = CARTESIAN_POINT ( 'NONE',  ( 1.476665317443916603, -1.350161712199383413, 1.354623164920423450 ) ) ;
#197308 = CARTESIAN_POINT ( 'NONE',  ( 2.578998426009218470, -2.112161100990978202, -0.6396139477699357423 ) ) ;
#197309 = CARTESIAN_POINT ( 'NONE',  ( 6.883263157960391787, -0.001104538646235289417, 1.946037152736757925 ) ) ;
#197310 = CARTESIAN_POINT ( 'NONE',  ( 3.172244755473273781, 6.644776614786712443, 0.000000000000000000 ) ) ;
#197311 = CARTESIAN_POINT ( 'NONE',  ( 7.173672674962134899, 7.541908673643526129, -0.7216878364870317197 ) ) ;
#197312 = CARTESIAN_POINT ( 'NONE',  ( -4.634189577772691138, 4.300976017023221409, 1.214306433183764966E-14 ) ) ;
#197313 = CARTESIAN_POINT ( 'NONE',  ( -5.587368702163209910, 9.532697562583475559, 0.000000000000000000 ) ) ;
#197314 = CARTESIAN_POINT ( 'NONE',  ( 0.7374959811429316892, -1.390993636481972606, -1.397171308748794250 ) ) ;
#197315 = CARTESIAN_POINT ( 'NONE',  ( 1.378406844460399405, 1.376398589878137013, 1.852031911770692263 ) ) ;
#197316 = CARTESIAN_POINT ( 'NONE',  ( 0.9769180011504545735, 1.811320799089161993, 0.7541596914439269161 ) ) ;
#197317 = CARTESIAN_POINT ( 'NONE',  ( 5.823111402427982419, -1.862227451873458728, -0.8870778100700682511 ) ) ;
#197318 = CARTESIAN_POINT ( 'NONE',  ( 4.365362273920238678, 7.076377838673507448, 1.082531754730558626 ) ) ;
#197319 = ADVANCED_FACE ( 'NONE', ( #22637 ), #65791, .T. ) ;
#197320 = CARTESIAN_POINT ( 'NONE',  ( 5.611095471209277541, 7.639640364534566075, 1.599625672291268286 ) ) ;
#197321 = VERTEX_POINT ( 'NONE', #132229 ) ;
#197322 = CARTESIAN_POINT ( 'NONE',  ( -0.6823417656250212460, 4.363541667008085767, 1.181850606188767472 ) ) ;
#197323 = CARTESIAN_POINT ( 'NONE',  ( 10.88932262995847822, -6.511064858252405330, -0.06814526087292289980 ) ) ;
#197324 = CARTESIAN_POINT ( 'NONE',  ( 5.151735183068521629, 5.112705256442466428, 1.040834085586084257E-14 ) ) ;
#197325 = CARTESIAN_POINT ( 'NONE',  ( 0.8839112305873472186, -2.062193702853211352, 0.6791930824729536242 ) ) ;
#197326 = CARTESIAN_POINT ( 'NONE',  ( 2.873292495919350653, 6.437382019922593734, -0.3438188498175620555 ) ) ;
#197327 = CARTESIAN_POINT ( 'NONE',  ( 11.44779963594995564, 10.90000000000000391, -3.600000000000078693 ) ) ;
#197328 = CARTESIAN_POINT ( 'NONE',  ( -2.978872658371960025, 6.473523904506141236, -0.4823651620584931687 ) ) ;
#197329 = CARTESIAN_POINT ( 'NONE',  ( 1.563515255687727645, 1.843751956470768283, -0.3144994141817195055 ) ) ;
#197330 = CARTESIAN_POINT ( 'NONE',  ( 5.747404748698970778, -1.700087083557629386, -1.334863535946126722 ) ) ;
#197331 = CARTESIAN_POINT ( 'NONE',  ( -6.070455375431035527, 6.038045056918933895, -0.4763334965118305453 ) ) ;
#197332 = CARTESIAN_POINT ( 'NONE',  ( 0.000000000000000000, 4.006659545634088992, 0.000000000000000000 ) ) ;
#197333 = CARTESIAN_POINT ( 'NONE',  ( 0.6823417656249882723, -0.6572916663252492686, 1.181850606188755259 ) ) ;
#197334 = CARTESIAN_POINT ( 'NONE',  ( 1.822773347178743508, 1.416086463930026573, -1.285276961632122905 ) ) ;
#197335 = AXIS2_PLACEMENT_3D ( 'NONE', #193522, #128614, #145878 ) ;
#197336 = CARTESIAN_POINT ( 'NONE',  ( 3.590472238826939666, -0.3446705786002961514, -1.735762067166376710 ) ) ;
#197337 = CARTESIAN_POINT ( 'NONE',  ( 0.5746843702075511429, -1.384840223850939855, 1.318951758179337741 ) ) ;
#197339 = CARTESIAN_POINT ( 'NONE',  ( 5.396063265741290138, -0.8654563178034151427, -1.709049623916969018 ) ) ;
#197338 = CARTESIAN_POINT ( 'NONE',  ( 3.300611021875788698, -3.189313111690857294, -0.4679188877521224255 ) ) ;
#197340 = CARTESIAN_POINT ( 'NONE',  ( 6.197704753879455630, -1.425424270160932094, -1.359389694413483562 ) ) ;
#197341 = CARTESIAN_POINT ( 'NONE',  ( -1.201851678989727383E-14, 5.087500000000019007, -1.732050807568863648 ) ) ;
#197342 = CARTESIAN_POINT ( 'NONE',  ( 1.318772358905948794, -0.7683209907942339933, -1.976687055281033611 ) ) ;
#197343 = DIRECTION ( 'NONE',  ( 0.000000000000000000, 0.000000000000000000, 1.000000000000000000 ) ) ;
#197344 = CARTESIAN_POINT ( 'NONE',  ( 5.436355746168001879, 1.843147576875401983, 0.3187000444574567548 ) ) ;
#197346 = EDGE_LOOP ( 'NONE', ( #144076, #127491, #154531, #202735 ) ) ;
#197345 = CARTESIAN_POINT ( 'NONE',  ( 0.4162703231485806454, 1.261427835099769634, -1.320066674804179385 ) ) ;
#197348 = CARTESIAN_POINT ( 'NONE',  ( 9.834497819152550946, 3.956598013261174884, 6.044631300485357350 ) ) ;
#197347 = CARTESIAN_POINT ( 'NONE',  ( 5.022202109028018668, -1.178465353167540197, -1.865713892744431446 ) ) ;
#197349 = CARTESIAN_POINT ( 'NONE',  ( -1.364683531250010295, 5.301041667008085767, -0.7879004041258300672 ) ) ;
#197350 = CARTESIAN_POINT ( 'NONE',  ( 2.242701489527811454, -2.022432087814116652, -0.4046766347945063846 ) ) ;
#197351 = CARTESIAN_POINT ( 'NONE',  ( 5.341022448779654930, 8.318611059296550536, 1.199719254218462483 ) ) ;
#197352 = CARTESIAN_POINT ( 'NONE',  ( -7.853197290813634268, 10.18514947741448573, 1.599625672291295375 ) ) ;
#197353 = FILL_AREA_STYLE_COLOUR ( '', #202759 ) ;
#197354 = CARTESIAN_POINT ( 'NONE',  ( 11.86687215968023601, 11.10942212305790022, -1.056395335932036383 ) ) ;
#197355 = CARTESIAN_POINT ( 'NONE',  ( -0.3000000000000068723, 3.172938907704321743, -0.5000000000000195399 ) ) ;
#197356 = EDGE_LOOP ( 'NONE', ( #150897, #27319, #125381, #96628 ) ) ;
#197357 = CARTESIAN_POINT ( 'NONE',  ( 4.193848433072798088, -1.425472641756184489, -1.501718461524886195 ) ) ;
#197358 = CARTESIAN_POINT ( 'NONE',  ( 1.499999999999990896, 5.275000000000022560, 1.214306433183764966E-14 ) ) ;
#197359 = CARTESIAN_POINT ( 'NONE',  ( 1.792469030454997059, -2.151019407201111289, -0.2137723215496489249 ) ) ;
#197360 = CARTESIAN_POINT ( 'NONE',  ( -4.934256961717153445, 8.002024883745839645, -1.000413331142641526 ) ) ;
#197361 = CARTESIAN_POINT ( 'NONE',  ( 1.717450570094357865, 1.680397536943441406, 1.120097702336475987 ) ) ;
#197362 = CARTESIAN_POINT ( 'NONE',  ( 0.07755575628183573877, -0.002876890934064984216, -2.188974970840869005 ) ) ;
#197363 = ADVANCED_FACE ( 'NONE', ( #98632 ), #138363, .T. ) ;
#197364 = EDGE_LOOP ( 'NONE', ( #186948, #208045, #118345, #211853 ) ) ;
#197365 = VERTEX_POINT ( 'NONE', #38956 ) ;
#197367 = CARTESIAN_POINT ( 'NONE',  ( 8.785320351975350661, 9.351887953500479966, -0.7216878364870197293 ) ) ;
#197366 = CARTESIAN_POINT ( 'NONE',  ( 0.000000000000000000, -2.537500000000000977, -4.012584370867899430 ) ) ;
#197368 = CARTESIAN_POINT ( 'NONE',  ( 0.2336117360935245635, 0.6279853779636718203, -1.916355031878452797 ) ) ;
#197369 = CARTESIAN_POINT ( 'NONE',  ( 4.775033345069852331, 2.044829088842615494, -0.7888500489584143738 ) ) ;
#197370 = CARTESIAN_POINT ( 'NONE',  ( -1.201851678989727383E-14, 3.993750000682817713, 1.732050807568877637 ) ) ;
#197371 = CARTESIAN_POINT ( 'NONE',  ( 3.392734571251673881, -1.844325299564765208, -0.5055192353106837677 ) ) ;
#197372 = CARTESIAN_POINT ( 'NONE',  ( -4.627410500965859264, 4.293067094081919777, 0.7998128361456341429 ) ) ;
#197373 = ADVANCED_FACE ( 'NONE', ( #134358 ), #154841, .T. ) ;
#197374 = CARTESIAN_POINT ( 'NONE',  ( 7.090551149822744925, 7.374657217655760100, 0.7216878364870317197 ) ) ;
#197376 = CARTESIAN_POINT ( 'NONE',  ( 1.898064762488653079, -0.9530305783747442527, -1.777002450075705120 ) ) ;
#197375 = DIRECTION ( 'NONE',  ( -0.2684563758389253985, 0.000000000000000000, 0.9632918427306595976 ) ) ;
#197377 = CARTESIAN_POINT ( 'NONE',  ( -0.6823417656250039265, 12.63020833367473017, -1.181850606188755259 ) ) ;
#197379 = CARTESIAN_POINT ( 'NONE',  ( -4.411198876399886615, 6.239761003923544713, -1.599625672291271394 ) ) ;
#197378 = CARTESIAN_POINT ( 'NONE',  ( 0.7675861853312654359, 2.207383698986573162, -0.6181827981695892094 ) ) ;
#197380 = CARTESIAN_POINT ( 'NONE',  ( 3.961678648311004025, 1.711676862058534088, -0.2113787121680379411 ) ) ;
#197381 = CARTESIAN_POINT ( 'NONE',  ( 0.1405533004714175083, 0.2365636613079393491, -2.314604644119310439 ) ) ;
#197382 = CARTESIAN_POINT ( 'NONE',  ( 2.659370686574860976, 6.254349567645977714, -0.7998128361456291469 ) ) ;
#197383 = CARTESIAN_POINT ( 'NONE',  ( -1.458777222063855072, 1.000000000000000888, 1.713029193092652669 ) ) ;
#197384 = CARTESIAN_POINT ( 'NONE',  ( 4.878236342818665250, 4.585697242910212523, 1.040834085586084257E-14 ) ) ;
#197385 = CARTESIAN_POINT ( 'NONE',  ( 0.1755611466353265426, 6.947017789483680872, -2.839095415174418768 ) ) ;
#197386 = ORIENTED_EDGE ( 'NONE', *, *, #12829, .T. ) ;
#197387 = CARTESIAN_POINT ( 'NONE',  ( -15.75000000000000000, 10.90000000000000036, -1.400000000000001910 ) ) ;
#197388 = ORIENTED_EDGE ( 'NONE', *, *, #205767, .T. ) ;
#197389 = CARTESIAN_POINT ( 'NONE',  ( 4.881432045509231266, 0.1721252788823707247, -1.803262557370821417 ) ) ;
#197390 = EDGE_LOOP ( 'NONE', ( #62104, #209172, #51700, #117278 ) ) ;
#197391 = CARTESIAN_POINT ( 'NONE',  ( 5.391302360089590628, 6.318882837306503575, -1.199719254218452047 ) ) ;
#197392 = CARTESIAN_POINT ( 'NONE',  ( 6.773846765307952822, -7.473374494058216300, -6.773846765307982132 ) ) ;
#197393 = CARTESIAN_POINT ( 'NONE',  ( 5.936161223257452768, -1.012099431654609472, -1.502142840615662944 ) ) ;
#197394 = CARTESIAN_POINT ( 'NONE',  ( 6.007671464186825183, 8.102312356341712984, 1.443375672974064550 ) ) ;
#197395 = CARTESIAN_POINT ( 'NONE',  ( -11.81911962874442068, 9.842894265158834699, -1.591749704452499303 ) ) ;
#197396 = CARTESIAN_POINT ( 'NONE',  ( 3.468858241077877214, 0.05382521638562161315, -2.190950023606648145 ) ) ;
#197398 = CARTESIAN_POINT ( 'NONE',  ( 7.228468454380276853, 11.58496363008569574, 1.040834085586084257E-14 ) ) ;
#197397 = CARTESIAN_POINT ( 'NONE',  ( 6.672303541529164050, -0.8785034406106060345, -1.640621795851913367 ) ) ;
#197399 = CARTESIAN_POINT ( 'NONE',  ( 3.356958492073054412, 0.04375785802200299335, -1.915270648069177462 ) ) ;
#197400 = CARTESIAN_POINT ( 'NONE',  ( -1.438721403180282410, 7.870009100117679068, 3.684356824110524453 ) ) ;
#197402 = ADVANCED_FACE ( 'NONE', ( #118137 ), #126963, .T. ) ;
#197401 = AXIS2_PLACEMENT_3D ( 'NONE', #141107, #172507, #106480 ) ;
#197403 = CARTESIAN_POINT ( 'NONE',  ( -4.702146809683744877, 5.356480858934594025, 2.500000000000011102 ) ) ;
#197404 = CARTESIAN_POINT ( 'NONE',  ( -0.6823417656250003738, -0.5322916663252491576, -1.181850606188749264 ) ) ;
#197405 = CARTESIAN_POINT ( 'NONE',  ( 6.371969008742804697, 7.496680600697164465, -1.082531754730543083 ) ) ;
#197407 = CARTESIAN_POINT ( 'NONE',  ( 5.489508092091861080, -0.5117143178510559220, 2.054485130609058796 ) ) ;
#197406 = CARTESIAN_POINT ( 'NONE',  ( -4.274898507010545856, 3.881803101134051470, -0.7998128361456221525 ) ) ;
#197408 = CARTESIAN_POINT ( 'NONE',  ( 0.8487565004985967443, 0.6285140637429244004, 2.068326486519965979 ) ) ;
#197409 = CARTESIAN_POINT ( 'NONE',  ( -5.611095471209320174, 7.639640364534566075, 1.599625672291263179 ) ) ;
#197410 = CARTESIAN_POINT ( 'NONE',  ( 4.553559489343365740, 6.405848385690952718, -1.599625672291269396 ) ) ;
#197411 = CARTESIAN_POINT ( 'NONE',  ( 0.5865807246496178573, -0.2182756592755269454, -1.812417144444453232 ) ) ;
#197412 = CARTESIAN_POINT ( 'NONE',  ( -3.066115294984855133, 6.728884944124295053, 0.7998128361456341429 ) ) ;
#197413 = CARTESIAN_POINT ( 'NONE',  ( 3.047666980291532823, 0.6586017179070653427, -1.702814618940437619 ) ) ;
#197414 = CARTESIAN_POINT ( 'NONE',  ( 8.390031855354989077, 12.96148178021487318, 8.510248056045641718 ) ) ;
#197415 = EDGE_LOOP ( 'NONE', ( #141125, #66101, #105109, #54246, #157184 ) ) ;
#197416 = CARTESIAN_POINT ( 'NONE',  ( 3.016014308207531247, 1.960325316701009735, -0.1901906172739661061 ) ) ;
#197417 = VERTEX_POINT ( 'NONE', #121352 ) ;
#197418 = CARTESIAN_POINT ( 'NONE',  ( 5.091328012616338938, -0.6953414466571452568, 1.813493487445563046 ) ) ;
#197419 = CARTESIAN_POINT ( 'NONE',  ( -4.787964524281469458, 5.614988695530339413, -1.199719254218453823 ) ) ;
#197421 = CARTESIAN_POINT ( 'NONE',  ( 5.713165544288242970, 1.732532623411761286, -1.222520872474173848 ) ) ;
#197420 = CARTESIAN_POINT ( 'NONE',  ( 6.879836604291781121, 6.991173891287354003, -0.7998128361456341429 ) ) ;
#197422 = CARTESIAN_POINT ( 'NONE',  ( -0.07802162204111612320, -7.185026885904014726, 9.499679971350929009 ) ) ;
#197423 = CARTESIAN_POINT ( 'NONE',  ( 2.438023429326571456, -1.102505324871098757, -1.562262158393577405 ) ) ;
#197424 = CARTESIAN_POINT ( 'NONE',  ( 5.389300372041062381, 6.501875383066589187, -1.316743393031569509 ) ) ;
#197425 = CARTESIAN_POINT ( 'NONE',  ( 0.2331563151865694850, 5.724144821786467219, -2.539778028485844885 ) ) ;
#197426 = ORIENTED_EDGE ( 'NONE', *, *, #12907, .T. ) ;
#197427 = CARTESIAN_POINT ( 'NONE',  ( 4.228163802615382494, 6.026220084508304708, -1.599625672291269396 ) ) ;
#197428 = CARTESIAN_POINT ( 'NONE',  ( 4.253507506385319381, 5.985511395581417204, 1.599625672291267398 ) ) ;
#197429 = PRESENTATION_LAYER_ASSIGNMENT (  '', '', ( #48859 ) ) ;
#197430 = CARTESIAN_POINT ( 'NONE',  ( 4.072905994182826284, -1.490248019560231452, 1.353564014653575009 ) ) ;
#197431 = CARTESIAN_POINT ( 'NONE',  ( -0.3265810047278985828, 2.653141922745489989, 1.973618857176524521 ) ) ;
#197432 = CARTESIAN_POINT ( 'NONE',  ( 5.109893933574640279, -1.816543354971979163, 0.1824992186492402357 ) ) ;
#197433 = CARTESIAN_POINT ( 'NONE',  ( 0.8716356842100521085, -0.3054578492302991721, 2.047597563663336118 ) ) ;
#197434 = CARTESIAN_POINT ( 'NONE',  ( -8.893785580884703279, 10.43879993486270585, 1.082531754730558626 ) ) ;
#197435 = CARTESIAN_POINT ( 'NONE',  ( -5.840188366348757931, 7.302172906674928576, 1.289283945506283890 ) ) ;
#197436 = CARTESIAN_POINT ( 'NONE',  ( -0.6125000000000105915, 1.604166667349450570, 1.060881119635899816 ) ) ;
#197437 = EDGE_CURVE ( 'NONE', #184826, #196061, #69595, .T. ) ;
#197438 = CARTESIAN_POINT ( 'NONE',  ( 6.016445890116215445, 1.255022122864515310, -1.387330985440645037 ) ) ;
#197439 = CARTESIAN_POINT ( 'NONE',  ( 7.800018446563675489, 7.994443030612759848, -0.7998128361456281477 ) ) ;
#197440 = CARTESIAN_POINT ( 'NONE',  ( -5.773074481320628948, 5.629675071162500544, 0.000000000000000000 ) ) ;
#197441 =( GEOMETRIC_REPRESENTATION_CONTEXT ( 3 ) GLOBAL_UNCERTAINTY_ASSIGNED_CONTEXT ( ( #35581 ) ) GLOBAL_UNIT_ASSIGNED_CONTEXT ( ( #45925, #23502, #28590 ) ) REPRESENTATION_CONTEXT ( 'NONE', 'WORKASPACE' ) );
#197442 = CARTESIAN_POINT ( 'NONE',  ( 1.364683531250000303, 10.06770833367473017, -0.7879004041258355073 ) ) ;
#197443 = CARTESIAN_POINT ( 'NONE',  ( -4.401593425930945713, 8.286942763561420122, 1.040834085586084257E-14 ) ) ;
#197444 = CARTESIAN_POINT ( 'NONE',  ( 2.523789150438203510, 6.096171108819874007, 0.7998128361456462443 ) ) ;
#197445 = CARTESIAN_POINT ( 'NONE',  ( -4.963693635934603776, 4.963599794778024155, 0.000000000000000000 ) ) ;
#197446 = CARTESIAN_POINT ( 'NONE',  ( -4.232116505760120440, 8.089219690028791376, -0.7998128361456281477 ) ) ;
#197447 = CARTESIAN_POINT ( 'NONE',  ( 1.041946221393402539, 1.387617377995558288, 1.536584593769604323 ) ) ;
#197448 = CARTESIAN_POINT ( 'NONE',  ( 2.056417290815291121, -1.299724242359597826, 1.671285701813587821 ) ) ;
#197449 = CARTESIAN_POINT ( 'NONE',  ( 9.399880572976245574, 9.860948844760784482, 0.7998128361456462443 ) ) ;
#197450 = CARTESIAN_POINT ( 'NONE',  ( 10.91970695577495754, -5.907420853759267843, 0.08000000000000194456 ) ) ;
#197451 = CARTESIAN_POINT ( 'NONE',  ( 6.438344962566215024, -1.112565956905732456, 1.745730973219234539 ) ) ;
#197452 = CARTESIAN_POINT ( 'NONE',  ( 5.221388208558932931, 6.626734370510860117, 1.385765457383714816 ) ) ;
#197453 = CARTESIAN_POINT ( 'NONE',  ( 4.636525346193557162, 7.392734756325715750, -1.082531754730549078 ) ) ;
#197455 = CARTESIAN_POINT ( 'NONE',  ( 4.650083499362867911, 6.448183387388563226, 1.443375672974062551 ) ) ;
#197454 = CARTESIAN_POINT ( 'NONE',  ( 0.000000000000000000, -3.587500000000000355, -4.012584370867899430 ) ) ;
#197456 = CARTESIAN_POINT ( 'NONE',  ( 2.467065147740226116, 0.1108469335737295169, -2.289696780367215467 ) ) ;
#197457 = FACE_OUTER_BOUND ( 'NONE', #137996, .T. ) ;
#197458 = CARTESIAN_POINT ( 'NONE',  ( 2.373185085050379506, -1.665764800640230803, -0.9392108107411781814 ) ) ;
#197459 = ORIENTED_EDGE ( 'NONE', *, *, #211412, .T. ) ;
#197460 = CARTESIAN_POINT ( 'NONE',  ( 6.710922848640084482, 9.812865175846695820, -1.082531754730537976 ) ) ;
#197461 = CARTESIAN_POINT ( 'NONE',  ( 0.4924401237900773443, -1.114920267122095021, 1.676101429157205613 ) ) ;
#197462 = CARTESIAN_POINT ( 'NONE',  ( 1.287862062775881666, -1.240280065097350448, -1.519972987346601023 ) ) ;
#197463 = CARTESIAN_POINT ( 'NONE',  ( -9.972185678051314284, 11.59297036493672017, 1.199719254218462483 ) ) ;
#197464 = CARTESIAN_POINT ( 'NONE',  ( -7.725448601688521322, 7.907444878258402809, 1.040834085586084257E-14 ) ) ;
#197465 = CARTESIAN_POINT ( 'NONE',  ( -11.51813239974987191, 7.080297235915058884, -3.210003848481874922 ) ) ;
#197467 = CARTESIAN_POINT ( 'NONE',  ( 2.377515701973518691, 1.086635889927405341, 1.396898309679272865 ) ) ;
#197466 = CARTESIAN_POINT ( 'NONE',  ( 3.873056903084231450, 1.968474739099084436, -0.7045419632574521085 ) ) ;
#197468 = CARTESIAN_POINT ( 'NONE',  ( 0.07933194154487524519, -7.473374494045017968, -9.499668754385622194 ) ) ;
#197469 = B_SPLINE_CURVE_WITH_KNOTS ( 'NONE', 1,
 ( #214409, #63946 ),
 .UNSPECIFIED., .F., .F.,
 ( 2, 2 ),
 ( 0.2265555213262071821, 0.4428258268412663679 ),
 .UNSPECIFIED. ) ;
#197471 = CARTESIAN_POINT ( 'NONE',  ( 4.804755513996577854, 1.992766236949112812, 1.132715491657744877 ) ) ;
#197470 = CARTESIAN_POINT ( 'NONE',  ( -1.225000000000012523, 2.000000000000001776, -1.214306433183764966E-14 ) ) ;
#197472 = CARTESIAN_POINT ( 'NONE',  ( 4.294662974013852441, 1.399676235010495873, 1.034011069942197159 ) ) ;
#197473 = CARTESIAN_POINT ( 'NONE',  ( 9.576136569953906275, 10.06658084123472641, 0.000000000000000000 ) ) ;
#197474 = CARTESIAN_POINT ( 'NONE',  ( 5.682802662783380754, 6.658966523782627434, 1.199719254218452935 ) ) ;
#197475 = CARTESIAN_POINT ( 'NONE',  ( 4.463993690379265189, 1.392342236284923152, 1.032948281618131903 ) ) ;
#197476 = CARTESIAN_POINT ( 'NONE',  ( 8.920901888111986366, 12.39117405523060889, 1.082531754730546636 ) ) ;
#197477 = CARTESIAN_POINT ( 'NONE',  ( 4.967309339809048652, 1.886637975807739176, 1.074439269227177363 ) ) ;
#197478 = CARTESIAN_POINT ( 'NONE',  ( 4.304877467538922531, 4.981110786005563007, 1.199719254218464037 ) ) ;
#197479 = CARTESIAN_POINT ( 'NONE',  ( 5.243375144629232487, 0.3886363430659239837, -1.978554426619572926 ) ) ;
#197480 = CARTESIAN_POINT ( 'NONE',  ( 0.5937500000000017764, -1.895863743164141191, -0.7852924748299565660 ) ) ;
#197481 = MECHANICAL_DESIGN_GEOMETRIC_PRESENTATION_REPRESENTATION (  '', ( #86792 ), #79971 ) ;
#197482 = CARTESIAN_POINT ( 'NONE',  ( 1.499999999999989120, 4.577083334016148974, -0.8660254037844323793 ) ) ;
#197483 = CARTESIAN_POINT ( 'NONE',  ( 2.467692127658027701, 1.889608252265186694, -0.3738381972786026797 ) ) ;
#197484 = CARTESIAN_POINT ( 'NONE',  ( 1.499999999999993117, 9.385416667349465669, 0.8660254037844409281 ) ) ;
#197485 = CARTESIAN_POINT ( 'NONE',  ( 5.221006152755099272, 1.681885564164938840, -1.451226649161361015 ) ) ;
#197486 = ORIENTED_EDGE ( 'NONE', *, *, #64145, .F. ) ;
#197488 = CIRCLE ( 'NONE', #207841, 12.00000000000000178 ) ;
#197487 = CARTESIAN_POINT ( 'NONE',  ( 6.983263157960370116, 7.052597238847845063, 2.544342084569085838 ) ) ;
#197489 = CARTESIAN_POINT ( 'NONE',  ( -0.7500000000000006661, 2.858333333333358706, -1.299038105676652011 ) ) ;
#197490 = CARTESIAN_POINT ( 'NONE',  ( 6.154511665599609493, 9.267681812253174556, 1.199719254218462483 ) ) ;
#197491 = CARTESIAN_POINT ( 'NONE',  ( 1.946216630774719736, -1.453687271215977850, -1.679643103671465632 ) ) ;
#197493 = EDGE_CURVE ( 'NONE', #107567, #195016, #168708, .T. ) ;
#197492 = CARTESIAN_POINT ( 'NONE',  ( 6.877413162628408294, -0.1429737755889188278, 1.930079329684093237 ) ) ;
#197494 = CARTESIAN_POINT ( 'NONE',  ( 8.053180056837369705, 11.37883191874353805, -1.082531754730543083 ) ) ;
#197495 = CARTESIAN_POINT ( 'NONE',  ( 4.913904330310220558, 4.697586238308844919, 0.000000000000000000 ) ) ;
#197496 = CARTESIAN_POINT ( 'NONE',  ( -3.011319516011047082, 6.527306845405913549, 0.7216878364870328300 ) ) ;
#197498 = CARTESIAN_POINT ( 'NONE',  ( 4.598127328184369311, 0.8849438138122868169, -1.863347811608778271 ) ) ;
#197497 = CARTESIAN_POINT ( 'NONE',  ( -0.4465194593918104249, 3.080450244942120719, -0.4155024747329819634 ) ) ;
#197499 = CARTESIAN_POINT ( 'NONE',  ( -3.903858165731105778, 6.641919395739846799, 1.199719254218464037 ) ) ;
#197500 = DIRECTION ( 'NONE',  ( 0.000000000000000000, -1.000000000000000000, -0.000000000000000000 ) ) ;
#197501 = CARTESIAN_POINT ( 'NONE',  ( -1.402160292154681736E-14, -0.9281249996585830830, 1.575800808251672791 ) ) ;
#197502 = CARTESIAN_POINT ( 'NONE',  ( 5.940666398231567058, 0.3644617591120716260, 1.834516074763043347 ) ) ;
#197503 = CARTESIAN_POINT ( 'NONE',  ( 4.904772540272760217, -0.9336124152922348207, -1.461164293347013921 ) ) ;
#197504 = CARTESIAN_POINT ( 'NONE',  ( 4.827569786946327213, 0.8888792617508225469, -1.496182039812316678 ) ) ;
#197505 = CARTESIAN_POINT ( 'NONE',  ( 4.857899112398166075, 4.561970474086296079, 1.040834085586084257E-14 ) ) ;
#197506 = CARTESIAN_POINT ( 'NONE',  ( 2.402247335887615964, -0.8806970201959153366, -2.116636687559919849 ) ) ;
#197507 = CARTESIAN_POINT ( 'NONE',  ( 0.6823417656249882723, -1.157291666325249713, 1.181850606188755259 ) ) ;
#197508 = CARTESIAN_POINT ( 'NONE',  ( 5.776921370525399446, 1.931409454660049319, -0.8010388902379047549 ) ) ;
#197509 = CARTESIAN_POINT ( 'NONE',  ( 1.341482821134845738, 1.838956754096718882, 0.09199767257135617327 ) ) ;
#197510 = LINE ( 'NONE', #120619, #140078 ) ;
#197511 = CARTESIAN_POINT ( 'NONE',  ( 2.584611472894111195, -0.6298744119781033435, 1.915600275669691488 ) ) ;
#197512 = CARTESIAN_POINT ( 'NONE',  ( 0.8322822162843239724, 2.159637434087835928, 0.3711470721824081109 ) ) ;
#197513 = CARTESIAN_POINT ( 'NONE',  ( 10.07587973459925124, 13.99570152553757474, -7.402601053387023455 ) ) ;
#197514 = CARTESIAN_POINT ( 'NONE',  ( -5.865874016206865882, 9.995270118883347266, 0.000000000000000000 ) ) ;
#197515 = CARTESIAN_POINT ( 'NONE',  ( 1.592325325408463055, 1.022198633559557646, -1.800363622228560168 ) ) ;
#197516 = CARTESIAN_POINT ( 'NONE',  ( 4.873266149108180123, 7.772895376346490970, 1.199719254218462483 ) ) ;
#197517 = CARTESIAN_POINT ( 'NONE',  ( -0.6801582343750316451, -0.7864583329919294652, 1.178068619123805227 ) ) ;
#197518 = CARTESIAN_POINT ( 'NONE',  ( 3.668700845920089826, 0.7647225481513253431, 1.977962425194310203 ) ) ;
#197519 = CARTESIAN_POINT ( 'NONE',  ( 1.364683531249986537, -0.1364583329919154264, 0.7879004041258500513 ) ) ;
#197520 = CARTESIAN_POINT ( 'NONE',  ( 6.287720257080702702, 1.262826302610157381, 1.318732360701305062 ) ) ;
#197521 = ORIENTED_EDGE ( 'NONE', *, *, #126517, .F. ) ;
#197522 = CARTESIAN_POINT ( 'NONE',  ( -4.630991987519598396, 7.560518531151607213, 1.199719254218452935 ) ) ;
#197523 = CARTESIAN_POINT ( 'NONE',  ( 8.723781775389312543, 12.26516360700784958, -1.199719254218446718 ) ) ;
#197524 = CARTESIAN_POINT ( 'NONE',  ( 7.485510208076452621, 7.905719128943566432, 0.000000000000000000 ) ) ;
#197525 = CARTESIAN_POINT ( 'NONE',  ( 3.475000000000000533, -2.202083332377417157, -2.006292185433951047 ) ) ;
#197526 = CARTESIAN_POINT ( 'NONE',  ( -5.205440912643032547, 8.160432600470439723, 1.199719254218452047 ) ) ;
#197527 = CARTESIAN_POINT ( 'NONE',  ( 3.691669705439902138, 1.900360886217996370, -0.6845428438169256502 ) ) ;
#197528 = CARTESIAN_POINT ( 'NONE',  ( 1.659346488253128804, -1.806016679666972546, -1.082987972701171309 ) ) ;
#197529 = CARTESIAN_POINT ( 'NONE',  ( -5.284646014276622950, 9.387447126623207794, -0.7998128361456362523 ) ) ;
#197530 = CARTESIAN_POINT ( 'NONE',  ( 9.426996880203592610, 9.892584536526015881, -0.7998128361456281477 ) ) ;
#197531 = CARTESIAN_POINT ( 'NONE',  ( 5.155058861800134729, 1.548501282276077529, -1.031774840880594901 ) ) ;
#197532 = CARTESIAN_POINT ( 'NONE',  ( 8.209625708274705502, 9.536650400197368427, 1.199719254218462483 ) ) ;
#197533 = CARTESIAN_POINT ( 'NONE',  ( 4.881461487140826172, 4.938218254980607291, -0.7598994375367192911 ) ) ;
#197534 = CARTESIAN_POINT ( 'NONE',  ( -2.767835915484202047, 6.380892334706859792, -0.7998128361456281477 ) ) ;
#197535 = CARTESIAN_POINT ( 'NONE',  ( -6.018930129462987999, 9.109503353427070849, 1.199719254218452047 ) ) ;
#197536 = CARTESIAN_POINT ( 'NONE',  ( 0.1984014031938194922, -2.161264429664040421, -0.05129915172277095536 ) ) ;
#197538 = CARTESIAN_POINT ( 'NONE',  ( -4.849785647588779725, 6.920107565692508622, 1.442884047295606820 ) ) ;
#197537 = CARTESIAN_POINT ( 'NONE',  ( -7.110325215724114578, 7.260077271291732082, 0.000000000000000000 ) ) ;
#197539 = CARTESIAN_POINT ( 'NONE',  ( -1.364683531250000748, 0.009375000341420303140, 0.000000000000000000 ) ) ;
#197540 = CARTESIAN_POINT ( 'NONE',  ( 2.161130077686782336, -0.4579326675830681093, -1.672196941802698733 ) ) ;
#197541 = CARTESIAN_POINT ( 'NONE',  ( 1.780815255366276162, 1.198741944763829004, 1.261882163386177869 ) ) ;
#197543 = CARTESIAN_POINT ( 'NONE',  ( 8.270110514656037637, 8.750809809961280550, 0.7216878364870458196 ) ) ;
#197542 = CARTESIAN_POINT ( 'NONE',  ( 0.3062966595402705217, -0.6107984557060777142, 2.225206381879496487 ) ) ;
#197544 = CARTESIAN_POINT ( 'NONE',  ( -10.90756946389101323, 4.636105284860338571, -4.485523696119586567 ) ) ;
#197545 = CARTESIAN_POINT ( 'NONE',  ( 2.407559617977403477, -0.4546984313768054342, 2.009812782922258734 ) ) ;
#197546 = CARTESIAN_POINT ( 'NONE',  ( 5.789495288235341874, 6.713164910151406595, 1.199719254218462483 ) ) ;
#197547 = CARTESIAN_POINT ( 'NONE',  ( 1.317732270343049406, -1.591076063098846749, 1.238129638497114771 ) ) ;
#197548 = CARTESIAN_POINT ( 'NONE',  ( 6.925078400183545035, 2.404074903924419804, 2.624186486869657831 ) ) ;
#197549 = CARTESIAN_POINT ( 'NONE',  ( -4.125423880308188629, 8.035021303660014880, -0.7998128361456481317 ) ) ;
#197550 = CIRCLE ( 'NONE', #28097, 0.04999999999999969746 ) ;
#197551 = CARTESIAN_POINT ( 'NONE',  ( 0.4792893823705188794, 1.840408107720743924, -0.7072656782263522235 ) ) ;
#197553 = CARTESIAN_POINT ( 'NONE',  ( -7.946487431385463651, 8.443525889470736345, 0.7216878364870317197 ) ) ;
#197552 = CARTESIAN_POINT ( 'NONE',  ( 5.080287894202283105, 0.9478536798121822704, 1.660923459347658282 ) ) ;
#197554 = CARTESIAN_POINT ( 'NONE',  ( 5.690102719724574598, -0.9953569382129350274, 1.969734210959340093 ) ) ;
#197555 = CARTESIAN_POINT ( 'NONE',  ( -7.715998819508785189, 8.174622508947939181, -0.7216878364870338292 ) ) ;
#197556 = CARTESIAN_POINT ( 'NONE',  ( 7.309781096423290769, 8.557108029695882578, 1.199719254218452935 ) ) ;
#197557 = CARTESIAN_POINT ( 'NONE',  ( -5.451787166026575981, 5.533042246551999277, 0.000000000000000000 ) ) ;
#197558 = CARTESIAN_POINT ( 'NONE',  ( 0.2936253167127310659, 1.883648094304795961, -0.7291253699766816476 ) ) ;
#197559 = EDGE_LOOP ( 'NONE', ( #158796, #96512, #110531, #43846 ) ) ;
#197560 = CARTESIAN_POINT ( 'NONE',  ( 1.187787545756531227, 2.830338437039773947, 0.7750000000000117906 ) ) ;
#197561 = CARTESIAN_POINT ( 'NONE',  ( 4.893776379751743733, 1.706213512276737232, 1.553814486356275060 ) ) ;
#197562 = CARTESIAN_POINT ( 'NONE',  ( 4.703538834289092030, -1.515240342570793430, -1.246145567450624991 ) ) ;
#197563 = CARTESIAN_POINT ( 'NONE',  ( 1.604273143990111672, 1.959273547513197711, 0.1016356785708133759 ) ) ;
#197564 = CARTESIAN_POINT ( 'NONE',  ( 8.048736748007069508, 12.54194330598362406, -0.7998128361456352531 ) ) ;
#197565 = CARTESIAN_POINT ( 'NONE',  ( -9.438383064798124167, 14.67447095286016001, 7.309821827705476061 ) ) ;
#197566 = VERTEX_POINT ( 'NONE', #84498 ) ;
#197567 = CARTESIAN_POINT ( 'NONE',  ( 0.2689693067343159605, -0.2660441693766130711, -2.100534484541769498 ) ) ;
#197569 = CARTESIAN_POINT ( 'NONE',  ( -8.667740277838301921, 9.006785167099828016, -0.7998128361456291469 ) ) ;
#197568 = CARTESIAN_POINT ( 'NONE',  ( -5.596818484342970912, 5.424043074688562172, -0.7998128361456221525 ) ) ;
#197570 = CARTESIAN_POINT ( 'NONE',  ( 0.5152501731416662123, -0.9825955030486510644, -1.556829690179861059 ) ) ;
#197571 = VERTEX_POINT ( 'NONE', #135400 ) ;
#197572 = CARTESIAN_POINT ( 'NONE',  ( 4.100555696908855019, 2.160072011501934064, 0.2185761814032516903 ) ) ;
#197573 = CARTESIAN_POINT ( 'NONE',  ( 10.41996096743601186, 10.52647388830694375, -5.960368362366588180 ) ) ;
#197574 = CARTESIAN_POINT ( 'NONE',  ( 1.969135536805465492, -1.636093909763213228, 1.349083368969570262 ) ) ;
#197575 = CARTESIAN_POINT ( 'NONE',  ( 0.7499999999999885647, 2.597916667349486897, -1.299038105676658228 ) ) ;
#197576 = CARTESIAN_POINT ( 'NONE',  ( 7.730120138085914583, 12.17022392774227768, 0.7998128361456462443 ) ) ;
#197577 = CARTESIAN_POINT ( 'NONE',  ( -0.6125000000000262457, 0.4583333333333244886, -1.060881119635996850 ) ) ;
#197578 = CARTESIAN_POINT ( 'NONE',  ( 6.395636025722083673, 6.905704815116233242, -0.7835738547974178125 ) ) ;
#197579 = CARTESIAN_POINT ( 'NONE',  ( 2.513025655421320170, 1.839406356194466463, 0.9293899518807801075 ) ) ;
#197580 = VECTOR ( 'NONE', #84971, 1000.000000000000000 ) ;
#197582 = CARTESIAN_POINT ( 'NONE',  ( 6.509000000000010111, 0.007656933339201026957, 1.900274884395844133 ) ) ;
#197581 = CARTESIAN_POINT ( 'NONE',  ( -9.528683032306089373, 10.01121838064558744, 0.7998128361456462443 ) ) ;
#197583 = CARTESIAN_POINT ( 'NONE',  ( -1.364683531249997417, 2.759375000341422801, 1.214306433183764966E-14 ) ) ;
#197584 = CARTESIAN_POINT ( 'NONE',  ( -0.02244404828160087226, 4.081832076214893412, -2.743766916979750281 ) ) ;
#197585 = CYLINDRICAL_SURFACE ( 'NONE', #139450, 1.500000000000000222 ) ;
#197586 = CARTESIAN_POINT ( 'NONE',  ( 5.391234928627540057, -0.05113397888981999900, -1.911771334517261556 ) ) ;
#197587 = CARTESIAN_POINT ( 'NONE',  ( 11.87815913191725947, 12.29692179368584881, -1.708869976696599791 ) ) ;
#197588 = CARTESIAN_POINT ( 'NONE',  ( 1.757462551082995095, -1.940025152074912551, -1.163771565304895450 ) ) ;
#197589 = CARTESIAN_POINT ( 'NONE',  ( -9.327646496521989405, 10.94497100310623594, -1.082531754730539753 ) ) ;
#197590 = CARTESIAN_POINT ( 'NONE',  ( 1.599580717682536291, 1.250984903983554997, 1.310507481138773800 ) ) ;
#197591 = CARTESIAN_POINT ( 'NONE',  ( 2.096773827148257219, 1.713186613203399489, 0.8573791853930428086 ) ) ;
#197592 = CARTESIAN_POINT ( 'NONE',  ( 2.770052221688572125, -2.048192801557855436, 0.3012726569043902569 ) ) ;
#197593 = CARTESIAN_POINT ( 'NONE',  ( -1.364683531250000748, 1.321875000341421469, 0.000000000000000000 ) ) ;
#197594 = AXIS2_PLACEMENT_3D ( 'NONE', #14106, #2106, #84454 ) ;
#197595 = CARTESIAN_POINT ( 'NONE',  ( 2.043765361886350274, 0.7562441204337754241, -1.820841827831324533 ) ) ;
#197596 = CARTESIAN_POINT ( 'NONE',  ( 5.356054764349521768, 1.924192155146129624, -0.09673933992536233595 ) ) ;
#197598 = CARTESIAN_POINT ( 'NONE',  ( 5.954584599377941601, 7.113081392617206511, -1.094866876611422235 ) ) ;
#197597 = CARTESIAN_POINT ( 'NONE',  ( 1.173011757359025520, -1.460375281577396489, 1.786833355454720884 ) ) ;
#197599 = CARTESIAN_POINT ( 'NONE',  ( -1.201851678989727383E-14, 2.071875000341422801, 1.575800808251672791 ) ) ;
#197600 = CARTESIAN_POINT ( 'NONE',  ( 5.564908101581790945, 1.564332607353050131, -1.344557729249852729 ) ) ;
#197601 = CARTESIAN_POINT ( 'NONE',  ( -6.600121851754250812, 6.594563670001734046, 0.7998128361456341429 ) ) ;
#197602 = CARTESIAN_POINT ( 'NONE',  ( 3.018661757337009810, 6.673522483535157868, 0.000000000000000000 ) ) ;
#197604 = CARTESIAN_POINT ( 'NONE',  ( -1.201851678989727383E-14, 5.337500000000020783, -1.732050807568863648 ) ) ;
#197603 = CARTESIAN_POINT ( 'NONE',  ( -0.01685825368398767912, -0.1589125243241385210, -2.071875930555002743 ) ) ;
#197605 = CARTESIAN_POINT ( 'NONE',  ( 0.6823417656249882723, 2.738541667008084879, -1.181850606188749264 ) ) ;
#197606 = CARTESIAN_POINT ( 'NONE',  ( 4.376362478467909156, -1.248523626585487989, 1.764366501186130698 ) ) ;
#197607 = CARTESIAN_POINT ( 'NONE',  ( 5.690105174167163327, 1.204846223408085670, 1.620761788888310351 ) ) ;
#197608 = DIRECTION ( 'NONE',  ( 0.000000000000000000, 0.000000000000000000, 1.000000000000000000 ) ) ;
#197609 = CARTESIAN_POINT ( 'NONE',  ( -6.249945626219832739, 6.393950773452325542, 1.040834085586084257E-14 ) ) ;
#197612 = CARTESIAN_POINT ( 'NONE',  ( 5.205967797967541166, 5.175976640491323444, -0.7216878364870197293 ) ) ;
#197611 = CARTESIAN_POINT ( 'NONE',  ( 1.001543065824772753E-15, -1.421874999522042327, 3.793834371823811669 ) ) ;
#197610 = CARTESIAN_POINT ( 'NONE',  ( 6.770317605177710085, 8.992066187497757213, 1.599625672291268286 ) ) ;
#197613 = CARTESIAN_POINT ( 'NONE',  ( -3.467853430045390706, 7.267855778353407459, 0.7998128361456352531 ) ) ;
#197614 = CARTESIAN_POINT ( 'NONE',  ( 3.801970467005914678, -1.040791964576088358, -1.727064642965264740 ) ) ;
#197615 = CARTESIAN_POINT ( 'NONE',  ( -6.177711549321182716, 10.35908057418338402, 0.7998128361456481317 ) ) ;
#197617 = CARTESIAN_POINT ( 'NONE',  ( -7.146556367734805626, 9.431011410480991231, 1.443375672974064550 ) ) ;
#197616 = CARTESIAN_POINT ( 'NONE',  ( -4.762992037102518950, 4.451245552908022596, -0.7998128361456221525 ) ) ;
#197618 = CARTESIAN_POINT ( 'NONE',  ( -1.364683531250010295, 4.780208333674755394, 0.7879004041258379498 ) ) ;
#197620 = CARTESIAN_POINT ( 'NONE',  ( 1.364683531249996529, 9.963541667008064096, 0.7879004041258403923 ) ) ;
#197619 = CARTESIAN_POINT ( 'NONE',  ( 4.680646922328831394, -2.095996545452833981, -0.5284188670612932626 ) ) ;
#197621 = CARTESIAN_POINT ( 'NONE',  ( -11.96431501343968584, 7.947166663703205458, 1.055127650031288278 ) ) ;
#197622 = ADVANCED_FACE ( 'NONE', ( #101818 ), #6426, .T. ) ;
#197624 = CARTESIAN_POINT ( 'NONE',  ( 5.800407700000974387, 1.352143934286989868, -1.496062775417882129 ) ) ;
#197623 = CARTESIAN_POINT ( 'NONE',  ( -7.659993601596720936, 8.999375959026737704, -1.082531754730543083 ) ) ;
#197625 = CARTESIAN_POINT ( 'NONE',  ( -1.364683531250014514, 0.05104166700808546175, -0.7879004041258359514 ) ) ;
#197626 = CARTESIAN_POINT ( 'NONE',  ( 0.6797846375097577054, -0.9621480743811950953, 1.431375779520219549 ) ) ;
#197627 = CARTESIAN_POINT ( 'NONE',  ( 3.223806664999388172, 6.983134552466421674, -0.7998128361456362523 ) ) ;
#197629 = CARTESIAN_POINT ( 'NONE',  ( 6.047819040147648373, 9.213483425884394507, 1.199719254218452047 ) ) ;
#197628 = CARTESIAN_POINT ( 'NONE',  ( 8.609064354997688184, 9.146255957026539818, 1.040834085586084257E-14 ) ) ;
#197630 = CARTESIAN_POINT ( 'NONE',  ( -11.59406913519968363, 8.291489155621126983, -2.927768694594159893 ) ) ;
#197631 = CARTESIAN_POINT ( 'NONE',  ( 6.503191328365395485, 1.555263205862934983, 1.038959965768880389 ) ) ;
#197632 = CARTESIAN_POINT ( 'NONE',  ( 0.6275903186243469989, -0.2933333519314991755, 1.991482607974030206 ) ) ;
#197633 = CARTESIAN_POINT ( 'NONE',  ( 0.000000000000000000, 8.920000000000001705, 0.000000000000000000 ) ) ;
#197634 = CARTESIAN_POINT ( 'NONE',  ( 3.890826896997583884, 4.602014803661035103, -1.082531754730543083 ) ) ;
#197635 = CARTESIAN_POINT ( 'NONE',  ( 3.540233119088306513, 0.9941544567689840628, -1.970234943098593039 ) ) ;
#197636 = AXIS2_PLACEMENT_3D ( 'NONE', #179332, #73535, #141788 ) ;
#197637 = CARTESIAN_POINT ( 'NONE',  ( -5.438229012412888252, 9.358701257874761481, -0.7216878364870338292 ) ) ;
#197638 = VERTEX_POINT ( 'NONE', #100747 ) ;
#197640 = CARTESIAN_POINT ( 'NONE',  ( 8.554831740098649107, 11.96409221588171157, 1.082531754730546636 ) ) ;
#197639 = AXIS2_PLACEMENT_3D ( 'NONE', #97802, #15441, #81530 ) ;
#197642 = CARTESIAN_POINT ( 'NONE',  ( 1.880482680076976720, -0.5405129038237622696, -1.942536604102131026 ) ) ;
#197641 = CARTESIAN_POINT ( 'NONE',  ( 1.946092837771850492, -1.387361170020007695, -1.603719225630481970 ) ) ;
#197644 = ORIENTED_EDGE ( 'NONE', *, *, #151935, .F. ) ;
#197643 = CARTESIAN_POINT ( 'NONE',  ( 2.707043852439145581, 1.551706383644942289, -0.9346757785875584590 ) ) ;
#197645 = CARTESIAN_POINT ( 'NONE',  ( 7.537407054554579489, 7.758339416593960536, 0.000000000000000000 ) ) ;
#197646 = CARTESIAN_POINT ( 'NONE',  ( 6.257251587906815793, 7.258880593101466161, 1.199719254218462483 ) ) ;
#197648 = CARTESIAN_POINT ( 'NONE',  ( 0.04005665835727333091, 0.7356861536649759170, 1.769027722964914728 ) ) ;
#197647 = CARTESIAN_POINT ( 'NONE',  ( -6.064574784014443942, 5.969758757638621738, -0.7998128361456291469 ) ) ;
#197649 = CARTESIAN_POINT ( 'NONE',  ( -2.680963214763168789, 0.4786715097226356130, -0.1016399112248461689 ) ) ;
#197650 = CARTESIAN_POINT ( 'NONE',  ( -5.249999999999987566, -0.9165151389911689872, 1.199999999999999734 ) ) ;
#197651 = EDGE_CURVE ( 'NONE', #70696, #12842, #18424, .T. ) ;
#197652 = CARTESIAN_POINT ( 'NONE',  ( 5.626270559546814098, 7.587068290936515247, 1.443375672974062551 ) ) ;
#197653 = CARTESIAN_POINT ( 'NONE',  ( 0.6823417656249882723, -0.2614583329919109578, -1.181850606188749264 ) ) ;
#197654 = PLANE ( 'NONE',  #126261 ) ;
#197655 = CARTESIAN_POINT ( 'NONE',  ( -7.947050595904583403, 12.42330946186405249, 0.7998128361456481317 ) ) ;
#197656 = CARTESIAN_POINT ( 'NONE',  ( 4.381803836707322652, 1.409801062080328959, 1.638821348427916602 ) ) ;
#197657 = CARTESIAN_POINT ( 'NONE',  ( -5.641601317062239218, 8.635599732330991429, -1.082531754730549967 ) ) ;
#197658 = CARTESIAN_POINT ( 'NONE',  ( 4.394251184604957672, 8.140727125432173139, -0.7216878364870357165 ) ) ;
#197659 = CARTESIAN_POINT ( 'NONE',  ( 2.215225606797793567, 1.700350911433265555, -1.266953333846132512 ) ) ;
#197660 = DIRECTION ( 'NONE',  ( 1.000000000000000000, 0.000000000000000000, -3.491481338843133355E-15 ) ) ;
#197661 = CARTESIAN_POINT ( 'NONE',  ( 3.180892574772069992, -0.1416633064414400678, -1.966302885814166013 ) ) ;
#197662 = CARTESIAN_POINT ( 'NONE',  ( 5.959226163113887864, -1.611951592244726950, 1.028742869173946861 ) ) ;
#197663 = ORIENTED_EDGE ( 'NONE', *, *, #145289, .T. ) ;
#197664 = CARTESIAN_POINT ( 'NONE',  ( 10.99970480893080627, -6.134628647623513231, 0.08058608058608522640 ) ) ;
#197665 = CARTESIAN_POINT ( 'NONE',  ( 6.637161372131059167, -0.09511470475139816028, -1.967365288627285214 ) ) ;
#197666 = CARTESIAN_POINT ( 'NONE',  ( 1.693202460532976295, -0.6543010362765960819, 1.828533997230662234 ) ) ;
#197667 = VERTEX_POINT ( 'NONE', #85562 ) ;
#197668 = CARTESIAN_POINT ( 'NONE',  ( 2.278002604729090219, 5.615589014598373119, 0.4951895290833923657 ) ) ;
#197670 = CARTESIAN_POINT ( 'NONE',  ( 7.309781096423290769, 8.557108029695882578, 1.199719254218452935 ) ) ;
#197669 = CARTESIAN_POINT ( 'NONE',  ( -7.105881907338178038, 7.462819444748888920, -0.7216878364870338292 ) ) ;
#197672 = CARTESIAN_POINT ( 'NONE',  ( 7.955937213120826357, 8.176348258262782664, 0.7998128361456481317 ) ) ;
#197671 = CARTESIAN_POINT ( 'NONE',  ( 2.835970919032384963, 2.074939634868844252, 0.2550863383830522801 ) ) ;
#197674 = CARTESIAN_POINT ( 'NONE',  ( 6.197485614778188712, 6.403023770095574108, -0.7216878364870458196 ) ) ;
#197673 = CARTESIAN_POINT ( 'NONE',  ( 6.500244582748090139, 9.671036882259738121, 1.199719254218460707 ) ) ;
#197676 = ORIENTED_EDGE ( 'NONE', *, *, #54068, .T. ) ;
#197675 = CARTESIAN_POINT ( 'NONE',  ( 6.639320575229252341, 0.005161017367553630275, 1.896863882003448021 ) ) ;
#197677 = CARTESIAN_POINT ( 'NONE',  ( 4.389439674793148782, 1.972019932058775016, -0.9908447712502415072 ) ) ;
#197678 = CARTESIAN_POINT ( 'NONE',  ( 1.518904762042364354, 1.481482853740143435, -1.635709697223409531 ) ) ;
#197679 = CARTESIAN_POINT ( 'NONE',  ( -10.98550897202509269, 12.34280431172945214, 1.591908179352832242 ) ) ;
#197680 = CARTESIAN_POINT ( 'NONE',  ( 0.7680391878876170475, 1.910087531778673187, -0.09433495293535018589 ) ) ;
#197681 = CARTESIAN_POINT ( 'NONE',  ( 0.1833691866889655686, 7.629137130509075604, -2.653448492709729933 ) ) ;
#197682 = CARTESIAN_POINT ( 'NONE',  ( 8.536830278099042602, 13.11138575775759563, -0.7998128361456352531 ) ) ;
#197683 = CARTESIAN_POINT ( 'NONE',  ( 3.965334771736851671, 1.774175476309115984, 1.066894043611272824 ) ) ;
#197685 = CARTESIAN_POINT ( 'NONE',  ( 1.868271315571629509, 1.111147431007172726, 1.854118885846419262 ) ) ;
#197684 = CARTESIAN_POINT ( 'NONE',  ( -4.060830702492950195, 4.696389560118578999, -1.199719254218452047 ) ) ;
#197686 = CARTESIAN_POINT ( 'NONE',  ( 3.491892070630482348, -2.189115664112693871, -0.1057334378413293807 ) ) ;
#197687 = DIRECTION ( 'NONE',  ( -3.491481338843133750E-15, -0.000000000000000000, -1.000000000000000000 ) ) ;
#197688 = PLANE ( 'NONE',  #86734 ) ;
#197689 = CARTESIAN_POINT ( 'NONE',  ( 0.4294077647110361440, -6.532648833121148968, 9.469892045836676431 ) ) ;
#197691 = EDGE_CURVE ( 'NONE', #93524, #17896, #139641, .T. ) ;
#197690 = CARTESIAN_POINT ( 'NONE',  ( 1.364683531250000303, 14.56770833367473372, -0.7879004041258355073 ) ) ;
#197692 = CARTESIAN_POINT ( 'NONE',  ( -4.679499295372141709, 5.488445928469455559, 1.199719254218452935 ) ) ;
#197693 = PRODUCT_DEFINITION_CONTEXT ( 'detailed design', #115578, 'design' ) ;
#197694 = CARTESIAN_POINT ( 'NONE',  ( 6.522076087392383315, -1.544353836717025308, 0.7889432867928622972 ) ) ;
#197695 = COLOUR_RGB ( '', 0.31764706, 0.68627451, 0.89019608) ;
#197696 = B_SPLINE_CURVE_WITH_KNOTS ( 'NONE', 3,
 ( #124764, #157188, #42387, #92210, #205913, #191789 ),
 .UNSPECIFIED., .F., .F.,
 ( 4, 2, 4 ),
 ( 0.000000000000000000, 0.0003205138222656014457, 0.0006410276445312028913 ),
 .UNSPECIFIED. ) ;
#197697 = CARTESIAN_POINT ( 'NONE',  ( -9.815740026613960723, 11.51441345488021106, -1.082531754730539753 ) ) ;
#197698 = CARTESIAN_POINT ( 'NONE',  ( 4.487213805514509879, 0.09639557921744396074, 2.068113308821089902 ) ) ;
#197699 = CARTESIAN_POINT ( 'NONE',  ( 5.255504845270437819, 2.040225721616812482, -0.5655070190290175658 ) ) ;
#197700 = CARTESIAN_POINT ( 'NONE',  ( 6.908042961362778733, 8.018137195466769285, 1.199719254218462483 ) ) ;
#197701 = DIRECTION ( 'NONE',  ( 0.000000000000000000, -1.000000000000000000, 0.000000000000000000 ) ) ;
#197702 = CARTESIAN_POINT ( 'NONE',  ( 4.153143631030720151, 1.666095859335927187, -1.049822023992821984 ) ) ;
#197703 = CARTESIAN_POINT ( 'NONE',  ( 6.246038198481189241, 0.7129642902690846995, 2.178627299872720524 ) ) ;
#197704 = CARTESIAN_POINT ( 'NONE',  ( 2.771877994228102882, 0.9767612972278701955, 1.542236413651025151 ) ) ;
#197705 = CARTESIAN_POINT ( 'NONE',  ( 4.740510986633625024, 5.559626234941203116, -1.199719254218450271 ) ) ;
#197706 = CARTESIAN_POINT ( 'NONE',  ( 5.816084710138150093, 5.887779704690372817, -0.7216878364870257245 ) ) ;
#197707 = CARTESIAN_POINT ( 'NONE',  ( -6.018930129462987999, 9.109503353427070849, 1.199719254218452047 ) ) ;
#197708 = CARTESIAN_POINT ( 'NONE',  ( 5.071631979963703962, 8.074598522336444262, 1.199719254218451159 ) ) ;
#197709 = ORIENTED_EDGE ( 'NONE', *, *, #33285, .F. ) ;
#197710 = CARTESIAN_POINT ( 'NONE',  ( 3.990493469460140830, -1.155612956054508977, 1.648335472937176194 ) ) ;
#197711 = CARTESIAN_POINT ( 'NONE',  ( 0.1757712021154093640, -0.9832847084251387093, -2.074436467499872094 ) ) ;
#197712 = CARTESIAN_POINT ( 'NONE',  ( 4.715648799723409113, 0.4337510919622395988, -1.913030730064477769 ) ) ;
#197713 = CARTESIAN_POINT ( 'NONE',  ( -7.881367368245678406, 8.089350105908421185, 0.7998128361456602331 ) ) ;
#197714 = CARTESIAN_POINT ( 'NONE',  ( -5.610376637956639101, 5.439860920571172542, 0.000000000000000000 ) ) ;
#197715 = CARTESIAN_POINT ( 'NONE',  ( -4.261005416444848315, 8.193199762486115034, 0.7998128361456352531 ) ) ;
#197717 = CARTESIAN_POINT ( 'NONE',  ( 6.174623306383559829, -1.681873830149778648, -0.5512017132776861894 ) ) ;
#197716 = CARTESIAN_POINT ( 'NONE',  ( 0.9254645587078378366, -1.329342062510083355, -1.613690532076578199 ) ) ;
#197718 = CARTESIAN_POINT ( 'NONE',  ( 10.96562622554683664, -5.341077028191770104, -0.1833053738655282261 ) ) ;
#197719 = CARTESIAN_POINT ( 'NONE',  ( 1.693587955360946529, -0.7361150630936144079, 2.064250245950305374 ) ) ;
#197720 = CARTESIAN_POINT ( 'NONE',  ( 0.9072687458823289752, -0.7809752019604562223, -1.555474206689683836 ) ) ;
#197721 = STYLED_ITEM ( 'NONE', ( #151966 ), #172902 ) ;
#197722 = CARTESIAN_POINT ( 'NONE',  ( 5.452350330990040739, 9.512825819463730070, 0.7998128361456462443 ) ) ;
#197723 = CARTESIAN_POINT ( 'NONE',  ( 0.1333692844072802142, 2.017199222642913625, -2.468757726274827036 ) ) ;
#197724 = CARTESIAN_POINT ( 'NONE',  ( 1.857592325351750118, 1.720440678145126467, -0.1246472719800949674 ) ) ;
#197725 = CARTESIAN_POINT ( 'NONE',  ( 1.505704256594592838, -2.174480876681058827, 0.2726767719730335826 ) ) ;
#197726 = CARTESIAN_POINT ( 'NONE',  ( -0.01748474828899664046, -1.733701077801694579, -0.04590633323625636919 ) ) ;
#197727 = CARTESIAN_POINT ( 'NONE',  ( 3.563272299071856164, -1.946135509614330239, -1.040604674307284316 ) ) ;
#197728 = CARTESIAN_POINT ( 'NONE',  ( 1.516727516949545107, 0.8775410692131856427, 1.985969635014148915 ) ) ;
#197729 = CARTESIAN_POINT ( 'NONE',  ( 0.04711308451243316486, -1.408776630263553375, -1.161003007932148501 ) ) ;
#197730 = CARTESIAN_POINT ( 'NONE',  ( 2.114611820864919611, 2.055121497718506163, 0.5091636546959156240 ) ) ;
#197731 = CARTESIAN_POINT ( 'NONE',  ( 6.827182134110239886, 1.995248472151121444, 2.590158597942037844 ) ) ;
#197732 = ORIENTED_EDGE ( 'NONE', *, *, #83921, .F. ) ;
#197734 = CARTESIAN_POINT ( 'NONE',  ( 1.364683531249986537, 0.1760416670080860446, 0.7879004041258500513 ) ) ;
#197733 = CARTESIAN_POINT ( 'NONE',  ( 2.718655769491088225, 2.159526321510790492, 0.7694321526581606729 ) ) ;
#197735 = DIRECTION ( 'NONE',  ( 0.000000000000000000, 1.000000000000000000, 0.000000000000000000 ) ) ;
#197736 = CARTESIAN_POINT ( 'NONE',  ( 5.087333953625774008, 6.958308917361963886, 1.599625672291267398 ) ) ;
#197737 = TOROIDAL_SURFACE ( 'NONE', #208103, 11.92000000000000171, 0.08000000000000000167 ) ;
#197738 = CARTESIAN_POINT ( 'NONE',  ( 4.916739609850255377, -0.7473993280511237458, -2.091895594778249379 ) ) ;
#197739 = CARTESIAN_POINT ( 'NONE',  ( -6.534666852106790103, 10.56760239419251590, 0.7216878364870458196 ) ) ;
#197741 = ADVANCED_FACE ( 'NONE', ( #142891 ), #2378, .T. ) ;
#197740 = CARTESIAN_POINT ( 'NONE',  ( 5.527114335400765910, 5.971691288924419361, -0.7760601246002347686 ) ) ;
#197742 = CARTESIAN_POINT ( 'NONE',  ( 5.368665641331531013, 5.365790791082654998, -0.7216878364870207285 ) ) ;
#197743 = CARTESIAN_POINT ( 'NONE',  ( -6.629573926958124197, 9.717958100551031819, 1.082531754730548412 ) ) ;
#197744 = CARTESIAN_POINT ( 'NONE',  ( 5.397554552016228691, 5.469770863539975991, 0.7216878364870328300 ) ) ;
#197745 = ORIENTED_EDGE ( 'NONE', *, *, #81172, .T. ) ;
#197746 = CARTESIAN_POINT ( 'NONE',  ( 3.481092415823695774, -2.014232707597499505, -0.09613569647320965861 ) ) ;
#197748 = CARTESIAN_POINT ( 'NONE',  ( 0.9716179518045722219, -0.3065469058200780972, 2.039571770164672504 ) ) ;
#197747 = CARTESIAN_POINT ( 'NONE',  ( 6.100279051144945619, 9.204410428722734849, -1.199719254218440723 ) ) ;
#197749 = CARTESIAN_POINT ( 'NONE',  ( 4.411882113620712254, 5.024994294388632987, 0.9701603416667784474 ) ) ;
#197750 = CARTESIAN_POINT ( 'NONE',  ( 5.194182247366869731, 7.153241603385088965, 1.443375672974064550 ) ) ;
#197751 = CARTESIAN_POINT ( 'NONE',  ( 3.834746474454188013E-15, 8.593750000682796042, 1.500000000000001554 ) ) ;
#197752 = CARTESIAN_POINT ( 'NONE',  ( -1.364683531250012516, 3.280208333674756727, 0.7879004041258379498 ) ) ;
#197753 = CARTESIAN_POINT ( 'NONE',  ( 3.732539452256115275, 0.3211115598316104935, 2.167677955659273348 ) ) ;
#197754 = CARTESIAN_POINT ( 'NONE',  ( 1.371720446232262081, -0.2986288616722633793, -1.994071132515719658 ) ) ;
#197755 = CARTESIAN_POINT ( 'NONE',  ( 1.522747961674526085, -1.733470594775164075, 0.6210259959333885860 ) ) ;
#197756 = EDGE_CURVE ( 'NONE', #109478, #196234, #204622, .T. ) ;
#197757 = CARTESIAN_POINT ( 'NONE',  ( 8.796542737168120851, 9.157054702984622097, -0.7998128361456211532 ) ) ;
#197758 = CARTESIAN_POINT ( 'NONE',  ( 5.262654937129007671, -1.321179299781930938, 1.260103332352560779 ) ) ;
#197759 = CARTESIAN_POINT ( 'NONE',  ( 5.748672702226536479, 1.986101125435947301, -0.3474646712962395911 ) ) ;
#197760 = CARTESIAN_POINT ( 'NONE',  ( -9.027031348600448979, 9.425958082989001952, 1.040834085586084257E-14 ) ) ;
#197762 = CARTESIAN_POINT ( 'NONE',  ( -6.656127069666307072, 6.730179434224282886, 0.7998128361456341429 ) ) ;
#197761 = CARTESIAN_POINT ( 'NONE',  ( 4.083118212167598848, -0.2185186360062584821, -2.251932414709489905 ) ) ;
#197763 = CARTESIAN_POINT ( 'NONE',  ( 1.049603877184020373, -1.661282181752096410, -1.294363288650403732 ) ) ;
#197764 = CARTESIAN_POINT ( 'NONE',  ( -6.505933609711270549, 8.683618192786854095, -1.599625672291271394 ) ) ;
#197765 = CARTESIAN_POINT ( 'NONE',  ( 4.562978833902987752, 1.602482145440896399, -1.310924660355553106 ) ) ;
#197766 = CARTESIAN_POINT ( 'NONE',  ( 7.716561984472250835, 12.15440608185967086, 1.040834085586084257E-14 ) ) ;
#197767 = CARTESIAN_POINT ( 'NONE',  ( -0.6801582343750351978, 2.630208333674721732, -1.178068619123886718 ) ) ;
#197768 = PRODUCT_CONTEXT ( 'NONE', #90556, 'mechanical' ) ;
#197769 = CARTESIAN_POINT ( 'NONE',  ( -8.853638004923878313, 10.28799807962136548, 1.199719254218462483 ) ) ;
#197770 = CARTESIAN_POINT ( 'NONE',  ( 6.471393748265519719, 5.229711127717882491, -2.499999999999995115 ) ) ;
#197771 = CARTESIAN_POINT ( 'NONE',  ( 5.677832469072920496, 9.846164657218904992, 0.000000000000000000 ) ) ;
#197772 = CARTESIAN_POINT ( 'NONE',  ( 5.328689024754546644, 6.340921230984883472, -1.104828203510083373 ) ) ;
#197773 = CARTESIAN_POINT ( 'NONE',  ( -10.46653140006992899, 11.31330084294416771, -0.7216878364870267237 ) ) ;
#197775 = CARTESIAN_POINT ( 'NONE',  ( 1.617743263029525869, 1.850308847857740968, 1.228972131997711381 ) ) ;
#197774 = CARTESIAN_POINT ( 'NONE',  ( 0.2816890862925770511, 0.2015970107726860194, -2.110973810222869229 ) ) ;
#197776 = CARTESIAN_POINT ( 'NONE',  ( -5.608682343087995292, 5.618096023427380459, 0.4395498943386428881 ) ) ;
#197777 = CARTESIAN_POINT ( 'NONE',  ( -5.738844160334429567, 9.917344963690652548, 0.000000000000000000 ) ) ;
#197778 = CARTESIAN_POINT ( 'NONE',  ( 7.311924916471702396, 7.425000578838787391, -0.7998128361456281477 ) ) ;
#197779 = CARTESIAN_POINT ( 'NONE',  ( 3.139059813392345077, -0.1416510307416830594, -1.956792864499560691 ) ) ;
#197780 = CARTESIAN_POINT ( 'NONE',  ( 6.796715079152391148, 6.823922435299587974, 0.7998128361456341429 ) ) ;
#197781 = CARTESIAN_POINT ( 'NONE',  ( -4.021031317475609157, 7.616913651768732585, 0.1724795716798576684 ) ) ;
#197782 = CARTESIAN_POINT ( 'NONE',  ( 2.849184837166184536, 6.475799410002530898, 0.7998128361456362523 ) ) ;
#197783 = CARTESIAN_POINT ( 'NONE',  ( -5.478903473698255588, 7.485416367438324059, -1.443375672974066548 ) ) ;
#197784 = CARTESIAN_POINT ( 'NONE',  ( -8.839552966430023417, 9.415159337030921449, -0.7216878364870267237 ) ) ;
#197785 = COLOUR_RGB ( '', 0.72549020, 0.75294118, 0.79215686) ;
#197786 = CARTESIAN_POINT ( 'NONE',  ( 1.793382672576701919, -0.1090974814243403090, -2.117938670719583527 ) ) ;
#197787 = CARTESIAN_POINT ( 'NONE',  ( -6.557303570864871034, 7.679217583210999010, -1.199719254218452047 ) ) ;
#197788 = CARTESIAN_POINT ( 'NONE',  ( 3.965250677406896962, 1.681448970545707855, 1.010551734412237446 ) ) ;
#197789 = CARTESIAN_POINT ( 'NONE',  ( 2.817419395390472037, -0.2130390993498078311, 2.151187356804876050 ) ) ;
#197790 = CARTESIAN_POINT ( 'NONE',  ( 2.858754248528099229, 0.2676582106064147593, -1.821554178878769470 ) ) ;
#197791 = VECTOR ( 'NONE', #33810, 1000.000000000000000 ) ;
#197792 = CARTESIAN_POINT ( 'NONE',  ( -4.183908731771626144, 7.398323783528643283, -0.7858605482065593728 ) ) ;
#197793 = EDGE_CURVE ( 'NONE', #70421, #118245, #10150, .T. ) ;
#197794 = CARTESIAN_POINT ( 'NONE',  ( 1.364683531249986537, -0.5739583329919174526, 0.7879004041258500513 ) ) ;
#197795 = CARTESIAN_POINT ( 'NONE',  ( 4.857210178628561970, 1.720700030253617951, -0.2597475362437673407 ) ) ;
#197796 = CARTESIAN_POINT ( 'NONE',  ( 4.009043883868839586, 7.799745125292699477, 0.2347419505407536966 ) ) ;
#197797 = CARTESIAN_POINT ( 'NONE',  ( 4.582292731738905722, 5.408724944192588424, -1.082531754730548412 ) ) ;
#197798 = CARTESIAN_POINT ( 'NONE',  ( -10.45142682343936791, 5.144546645612242841, 5.216777551074719632 ) ) ;
#197799 = CARTESIAN_POINT ( 'NONE',  ( 7.736899214892750010, 12.17813285068358020, 1.040834085586084257E-14 ) ) ;
#197800 = CARTESIAN_POINT ( 'NONE',  ( 1.991316529349271836, 1.880942973025516940, -1.065213018539921563 ) ) ;
#197801 = CARTESIAN_POINT ( 'NONE',  ( 4.868517441940229951, -0.5404072756688071966, 1.942244311778835719 ) ) ;
#197802 = CARTESIAN_POINT ( 'NONE',  ( -9.286972035236630063, 10.89751746493999107, -1.082531754730537976 ) ) ;
#197803 = CARTESIAN_POINT ( 'NONE',  ( 1.094844843509492183, -0.5259716649698794599, -2.096624219460433647 ) ) ;
#197804 =( BOUNDED_CURVE ( )  B_SPLINE_CURVE ( 2, ( #20917, #87012, #134729, #200736, #3596, #52386, #137916, #118514, #85952 ),
 .UNSPECIFIED., .F., .T. ) 
 B_SPLINE_CURVE_WITH_KNOTS ( ( 3, 2, 2, 2, 3 ),
 ( 0.6875000000000000000, 0.6904761904761904656, 0.6964285714285713969, 0.7023809523809523281, 0.7053571428571427937 ),
 .UNSPECIFIED. ) 
 CURVE ( )  GEOMETRIC_REPRESENTATION_ITEM ( )  RATIONAL_B_SPLINE_CURVE ( ( 0.9330127018922194093, 0.9330127018922194093, 1.000000000000000000, 0.8660254037844387076, 1.000000000000000000, 0.8660254037844387076, 1.000000000000000000, 0.9330127018922206306, 0.9330127018922194093 ) ) 
 REPRESENTATION_ITEM ( '' )  );
#197805 = CARTESIAN_POINT ( 'NONE',  ( 2.794160851653566535, -1.965818266918018864, -0.1488234875552247316 ) ) ;
#197807 = EDGE_CURVE ( 'NONE', #94599, #108406, #108448, .T. ) ;
#197806 = CARTESIAN_POINT ( 'NONE',  ( 2.817592499383800853, -1.357869084745389809, -1.490969456672403881 ) ) ;
#197808 = CARTESIAN_POINT ( 'NONE',  ( 10.39230484541330313, 3.447199233515649386, 5.999999999999906741 ) ) ;
#197809 = CARTESIAN_POINT ( 'NONE',  ( 3.298316653532318732, 1.529317551288728483, -1.196868631420761053 ) ) ;
#197812 = ORIENTED_EDGE ( 'NONE', *, *, #100013, .T. ) ;
#197811 = CARTESIAN_POINT ( 'NONE',  ( -4.014622883422336308, 5.777089012116397804, -1.443375672974066548 ) ) ;
#197810 = CARTESIAN_POINT ( 'NONE',  ( -9.693716643646601128, 12.33242205571964512, 1.443375672974076540 ) ) ;
#197814 = EDGE_CURVE ( 'NONE', #54188, #35130, #147131, .T. ) ;
#197813 = CARTESIAN_POINT ( 'NONE',  ( -5.139949632912262700, 5.169231791251960750, 0.7216878364870257245 ) ) ;
#197815 = CARTESIAN_POINT ( 'NONE',  ( 3.790386463472274148, 6.579812086429759788, 1.199719254218452047 ) ) ;
#197817 = ORIENTED_EDGE ( 'NONE', *, *, #17110, .F. ) ;
#197816 = CARTESIAN_POINT ( 'NONE',  ( -4.471156797456668386, 8.438376373666578445, -0.7998128361456362523 ) ) ;
#197818 = CARTESIAN_POINT ( 'NONE',  ( -9.070041577417988776, 12.56517035942090388, 1.082531754730558626 ) ) ;
#197819 = CARTESIAN_POINT ( 'NONE',  ( 0.8509352111321017986, 0.6423128672003556305, 2.111239891224323983 ) ) ;
#197820 = CARTESIAN_POINT ( 'NONE',  ( 1.642778471875000035, -4.076041666188710444, -2.845375778867859751 ) ) ;
#197821 = CARTESIAN_POINT ( 'NONE',  ( 5.612146373276853950, 1.959670608579218376, -0.09257137562097839112 ) ) ;
#197822 = VERTEX_POINT ( 'NONE', #175369 ) ;
#197823 = CARTESIAN_POINT ( 'NONE',  ( 3.274719840360585721, -0.4174103159439371824, -2.075633323822536180 ) ) ;
#197824 = CARTESIAN_POINT ( 'NONE',  ( -1.201851678989727383E-14, 3.493750000682815493, 1.732050807568877637 ) ) ;
#197825 = CARTESIAN_POINT ( 'NONE',  ( 0.07459516483341446791, 5.726030365519781284, -2.349570391284861781 ) ) ;
#197826 = CARTESIAN_POINT ( 'NONE',  ( 4.242028835625204053, 0.4931972713904734795, 1.773778790588397491 ) ) ;
#197827 = ORIENTED_EDGE ( 'NONE', *, *, #141289, .F. ) ;
#197828 = CARTESIAN_POINT ( 'NONE',  ( -8.616370316684697883, 10.01118577667568132, -1.199719254218446718 ) ) ;
#197829 =( NAMED_UNIT ( * ) PLANE_ANGLE_UNIT ( ) SI_UNIT ( $, .RADIAN. ) );
#197830 = CARTESIAN_POINT ( 'NONE',  ( 5.414351406770180120, -2.120778210838507150, 0.002142078463891750485 ) ) ;
#197831 = CARTESIAN_POINT ( 'NONE',  ( -5.521155831633614675, 5.981593978145122392, -0.9474053820182636310 ) ) ;
#197832 = CARTESIAN_POINT ( 'NONE',  ( 5.392392409933256303, 7.314210449720692786, 1.599625672291267398 ) ) ;
#197833 = ORIENTED_EDGE ( 'NONE', *, *, #183770, .F. ) ;
#197834 = CARTESIAN_POINT ( 'NONE',  ( 5.624313186929686736, 1.231095119260311677, -1.652465237140358090 ) ) ;
#197837 = CARTESIAN_POINT ( 'NONE',  ( 3.087279721815265443, -0.7436087841871074078, 1.684586988852328160 ) ) ;
#197836 = CARTESIAN_POINT ( 'NONE',  ( 0.8009387066525032184, -1.599029608822761128, 0.9519043452789009985 ) ) ;
#197835 = CARTESIAN_POINT ( 'NONE',  ( -5.717785742877127042, 7.006476535625795421, -2.500000000000000444 ) ) ;
#197838 = CARTESIAN_POINT ( 'NONE',  ( 8.959240580532112475, 9.346868853575953651, -0.7998128361456221525 ) ) ;
#197839 = CARTESIAN_POINT ( 'NONE',  ( -11.88235317400313917, 9.843357602269703577, 0.9089793033029933689 ) ) ;
#197840 = CARTESIAN_POINT ( 'NONE',  ( -1.913131547260899179, 0.6205095947705763226, 0.2971265334020881110 ) ) ;
#197841 = CARTESIAN_POINT ( 'NONE',  ( 2.965657822035951963, 0.3232568108629539361, -2.182957019552448141 ) ) ;
#197842 = CARTESIAN_POINT ( 'NONE',  ( 4.429186382639688446, 0.1052742795825665628, 2.260063922926962121 ) ) ;
#197843 = CARTESIAN_POINT ( 'NONE',  ( -5.748293942514169252, 9.650167333001109071, -0.7216878364870207285 ) ) ;
#197844 = CARTESIAN_POINT ( 'NONE',  ( 5.009926431283926895, -0.6449355957302944642, 1.693101296380158383 ) ) ;
#197845 = B_SPLINE_CURVE_WITH_KNOTS ( 'NONE', 3,
 ( #165415, #132951, #65749, #111411 ),
 .UNSPECIFIED., .F., .F.,
 ( 4, 4 ),
 ( 0.001170373960510464294, 0.001235641208627022772 ),
 .UNSPECIFIED. ) ;
#197846 = CARTESIAN_POINT ( 'NONE',  ( 5.419116407314492179, -1.729028094342921706, 0.8252531017051125684 ) ) ;
#197847 = CARTESIAN_POINT ( 'NONE',  ( 6.827182134110198142, 0.003888933837258023996, 1.810856214465889069 ) ) ;
#197848 = CARTESIAN_POINT ( 'NONE',  ( 6.034044788248046132, 0.9204803733943857091, -1.628451883209979689 ) ) ;
#197849 = CARTESIAN_POINT ( 'NONE',  ( 6.215283151739675382, -1.596727646711604942, -0.9557930639402379969 ) ) ;
#197850 = CARTESIAN_POINT ( 'NONE',  ( 3.834746474454188013E-15, 13.06250000000000178, 1.500000000000001554 ) ) ;
#197851 = CIRCLE ( 'NONE', #21556, 0.04999999999999985706 ) ;
#197852 = CARTESIAN_POINT ( 'NONE',  ( 6.491055376221456008, 1.537463663300852490, -0.8764918771043300749 ) ) ;
#197853 = CARTESIAN_POINT ( 'NONE',  ( 0.4797043241997685503, -0.7212876333932433104, 1.883314553594167107 ) ) ;
#197855 = CARTESIAN_POINT ( 'NONE',  ( 2.684315897010148610, -1.081986827455215572, 1.806733699029156259 ) ) ;
#197854 = CARTESIAN_POINT ( 'NONE',  ( -3.429849674132942727, 5.984946472254969230, -1.082531754730549078 ) ) ;
#197856 = CARTESIAN_POINT ( 'NONE',  ( 2.372313692266983853, 5.711523707712699682, 0.7216878364870438212 ) ) ;
#197857 = CARTESIAN_POINT ( 'NONE',  ( -8.910733272679575379, 11.41894145625809820, -1.599625672291263179 ) ) ;
#197858 = CARTESIAN_POINT ( 'NONE',  ( 6.777182134110200096, 7.629137130509070275, 2.410944104600750038 ) ) ;
#197859 = CARTESIAN_POINT ( 'NONE',  ( 2.021745798758204149, -0.4384165714973499162, 1.971471537551409803 ) ) ;
#197860 = CARTESIAN_POINT ( 'NONE',  ( 1.364683531249988535, 1.863541667008086211, 0.7879004041258500513 ) ) ;
#197861 = CARTESIAN_POINT ( 'NONE',  ( 3.928111819657337911, 5.605883094398769195, 1.599625672291267398 ) ) ;
#197862 = CARTESIAN_POINT ( 'NONE',  ( 3.075615952314793233, 2.053625483174918553, -0.6748976972978243394 ) ) ;
#197863 = CARTESIAN_POINT ( 'NONE',  ( 6.890000000000044977, 2.990039200936049468, 2.173945303097582382 ) ) ;
#197866 = DIRECTION ( 'NONE',  ( 1.000000000000000000, -0.000000000000000000, -0.000000000000000000 ) ) ;
#197865 = CARTESIAN_POINT ( 'NONE',  ( 11.97929049433705373, 9.719999999999998863, -0.7046979865771821894 ) ) ;
#197864 = CARTESIAN_POINT ( 'NONE',  ( 3.562760505341037831, 7.378580699531681830, -1.734723475976807094E-15 ) ) ;
#197867 = CARTESIAN_POINT ( 'NONE',  ( 8.365017589507326434, 12.70301158782650397, -0.7216878364870338292 ) ) ;
#197868 = CARTESIAN_POINT ( 'NONE',  ( 11.89942855770814312, 9.799999999999998934, -0.7000000000000009548 ) ) ;
#197869 = CARTESIAN_POINT ( 'NONE',  ( -8.215877900201387973, 8.687538426430837291, 0.7216878364870578100 ) ) ;
#197870 = CARTESIAN_POINT ( 'NONE',  ( 1.364683531249986537, 0.6135416670080880985, 0.7879004041258500513 ) ) ;
#197871 = CARTESIAN_POINT ( 'NONE',  ( 0.9432342461353732110, -1.730868645791438842, -1.344178957308760802 ) ) ;
#197872 = CARTESIAN_POINT ( 'NONE',  ( -15.75000000000000000, 10.89999999999998259, 3.599999999999999201 ) ) ;
#197873 = CARTESIAN_POINT ( 'NONE',  ( 1.710245752144876619, -2.245277845785878412, 0.2781651023185549021 ) ) ;
#197874 = CARTESIAN_POINT ( 'NONE',  ( -8.694856585065634746, 9.038420858865048757, 0.7998128361456462443 ) ) ;
#197875 = ADVANCED_FACE ( 'NONE', ( #190517 ), #106138, .T. ) ;
#197876 = CARTESIAN_POINT ( 'NONE',  ( -3.416291520519271874, 6.929497840673697340, 1.040834085586084257E-14 ) ) ;
#197877 = CARTESIAN_POINT ( 'NONE',  ( -1.364683531249997417, 3.071875000341423245, 1.214306433183764966E-14 ) ) ;
#197878 = CARTESIAN_POINT ( 'NONE',  ( 4.633164669693822901, 8.325607986553848150, 0.3865003237762173471 ) ) ;
#197879 = CIRCLE ( 'NONE', #152907, 0.08000000000000025147 ) ;
#197880 = CARTESIAN_POINT ( 'NONE',  ( 1.499999999999993117, 11.60416666666666252, 0.8660254037844409281 ) ) ;
#197881 = CARTESIAN_POINT ( 'NONE',  ( 4.740510986633625024, 5.559626234941203116, -1.199719254218450271 ) ) ;
#197882 = CARTESIAN_POINT ( 'NONE',  ( 3.409201082634921498, -0.3482811000503453491, 1.734931447941751692 ) ) ;
#197883 =( BOUNDED_CURVE ( )  B_SPLINE_CURVE ( 2, ( #151273, #198916, #114569, #50562, #116683, #34303, #100376, #166446, #18038 ),
 .UNSPECIFIED., .F., .T. ) 
 B_SPLINE_CURVE_WITH_KNOTS ( ( 3, 2, 2, 2, 3 ),
 ( 0.2946428571428571508, 0.2976190476190476164, 0.3035714285714285476, 0.3095238095238095344, 0.3124999999999999445 ),
 .UNSPECIFIED. ) 
 CURVE ( )  GEOMETRIC_REPRESENTATION_ITEM ( )  RATIONAL_B_SPLINE_CURVE ( ( 0.9330127018922194093, 0.9330127018922194093, 1.000000000000000000, 0.8660254037844387076, 1.000000000000000000, 0.8660254037844387076, 1.000000000000000000, 0.9330127018922206306, 0.9330127018922194093 ) ) 
 REPRESENTATION_ITEM ( '' )  );
#197884 = CARTESIAN_POINT ( 'NONE',  ( 6.686557766011572923, -2.162873314485185272, -0.4371622687903350957 ) ) ;
#197885 = CARTESIAN_POINT ( 'NONE',  ( -1.402160292154681736E-14, 9.671875000341399797, 1.575800808251682339 ) ) ;
#197886 = VERTEX_POINT ( 'NONE', #155909 ) ;
#197887 = CARTESIAN_POINT ( 'NONE',  ( -4.586401103172829785, 8.572828063668767484, 0.7998128361456281477 ) ) ;
#197888 = CARTESIAN_POINT ( 'NONE',  ( 5.079703922733037835, -0.7231256174668048153, 1.882480835741196845 ) ) ;
#197889 = VERTEX_POINT ( 'NONE', #113614 ) ;
#197890 = CARTESIAN_POINT ( 'NONE',  ( 2.764352523130030548, -1.291370965961564421, 1.353630663414123969 ) ) ;
#197891 = CARTESIAN_POINT ( 'NONE',  ( 3.819242646454374057, -1.823515126939363462, -0.9802443236400714133 ) ) ;
#197892 = CARTESIAN_POINT ( 'NONE',  ( -8.054952659850432184, 8.570068656013202002, 0.000000000000000000 ) ) ;
#197893 = CARTESIAN_POINT ( 'NONE',  ( 2.461071540317420592, -1.587761714688111780, 1.065645112462119570 ) ) ;
#197894 = FACE_OUTER_BOUND ( 'NONE', #54157, .T. ) ;
#197895 = CARTESIAN_POINT ( 'NONE',  ( -9.505468521307150809, 5.017170101577987928, -6.783879874543660371 ) ) ;
#197896 = FACE_OUTER_BOUND ( 'NONE', #154112, .T. ) ;
#197897 = CARTESIAN_POINT ( 'NONE',  ( -0.6823417656249969321, 4.530208333674755394, -1.181850606188749264 ) ) ;
#197898 = CARTESIAN_POINT ( 'NONE',  ( 0.8965662283535699162, -1.866366896104875162, -0.4163465257057268332 ) ) ;
#197899 = CARTESIAN_POINT ( 'NONE',  ( 3.103904542773823660, 0.7086415210641981988, -1.829580771271981154 ) ) ;
#197900 = CARTESIAN_POINT ( 'NONE',  ( 7.037870247915942734, -8.233137084989836652, -6.381095703207974701 ) ) ;
#197901 = CARTESIAN_POINT ( 'NONE',  ( -4.125423880308188629, 8.035021303660014880, -0.7998128361456481317 ) ) ;
#197903 = SURFACE_SIDE_STYLE ('',( #149166 ) ) ;
#197902 = CARTESIAN_POINT ( 'NONE',  ( 8.778014389843965759, 12.32843499053828928, 1.199719254218450271 ) ) ;
#197904 = CARTESIAN_POINT ( 'NONE',  ( 0.2099203756031532975, -0.7936979409460078738, -1.692237190125941648 ) ) ;
#197905 = CARTESIAN_POINT ( 'NONE',  ( -1.402160292154681736E-14, 1.946875000341422579, -1.575800808251660134 ) ) ;
#197906 = CARTESIAN_POINT ( 'NONE',  ( 2.162360077456865870, 2.012843401649004882, 0.04526349954376075735 ) ) ;
#197908 = CARTESIAN_POINT ( 'NONE',  ( 2.460703409257146923, -2.027034307268358315, -0.6114533316685047959 ) ) ;
#197907 = CARTESIAN_POINT ( 'NONE',  ( -6.968527767744110868, 9.153035033833367251, 1.443375672974078761 ) ) ;
#197909 = B_SPLINE_CURVE_WITH_KNOTS ( 'NONE', 3,
 ( #49072, #131429, #113067, #198484, #179073, #30694 ),
 .UNSPECIFIED., .F., .F.,
 ( 4, 2, 4 ),
 ( 0.001877801214402442754, 0.002190719108449961511, 0.002503637002497480051 ),
 .UNSPECIFIED. ) ;
#197910 = CARTESIAN_POINT ( 'NONE',  ( 8.868211955184602147, 12.79485499900459367, -8.085349282452083841 ) ) ;
#197911 = CARTESIAN_POINT ( 'NONE',  ( 4.105968538015460467, 0.7004154448949986289, -1.948405661837959713 ) ) ;
#197912 = CARTESIAN_POINT ( 'NONE',  ( 3.874598038455354665, 7.742391154831717692, -0.7998128361456362523 ) ) ;
#197914 = CARTESIAN_POINT ( 'NONE',  ( 4.005544317833563461, 6.760553239859419250, -1.199719254218452047 ) ) ;
#197913 = CARTESIAN_POINT ( 'NONE',  ( 6.140588758375521650, -1.766823853066697536, 1.117321708369632516 ) ) ;
#197916 = VERTEX_POINT ( 'NONE', #65820 ) ;
#197915 = CARTESIAN_POINT ( 'NONE',  ( 4.594645031659345236, -0.4005623417570289280, -1.780931357837008733 ) ) ;
#197917 = CARTESIAN_POINT ( 'NONE',  ( 7.730120138085914583, 12.17022392774227768, 0.7998128361456462443 ) ) ;
#197918 =( LENGTH_UNIT ( ) NAMED_UNIT ( * ) SI_UNIT ( .MILLI., .METRE. ) );
#197919 = CARTESIAN_POINT ( 'NONE',  ( 10.20449125605852458, 13.21811437223454178, 7.146917523142401585 ) ) ;
#197920 = CARTESIAN_POINT ( 'NONE',  ( 5.069440727656137291, 0.2206807655098403653, -2.195719112144229879 ) ) ;
#197921 = CARTESIAN_POINT ( 'NONE',  ( 1.364683531249997417, 10.04687500034139802, 2.602085213965210642E-15 ) ) ;
#197922 = EDGE_LOOP ( 'NONE', ( #106047, #44211, #204939, #81517 ) ) ;
#197923 = CARTESIAN_POINT ( 'NONE',  ( 4.477155480220369910, -1.709698060584059043, -0.8567103784868701499 ) ) ;
#197924 = CARTESIAN_POINT ( 'NONE',  ( -10.32183501870554387, 10.93656236477829502, 0.7998128361456462443 ) ) ;
#197925 = CIRCLE ( 'NONE', #121965, 11.09999999999999964 ) ;
#197926 = CARTESIAN_POINT ( 'NONE',  ( 5.635385404774530649, 9.726366738878972740, 0.7998128361456462443 ) ) ;
#197927 =( GEOMETRIC_REPRESENTATION_CONTEXT ( 3 ) GLOBAL_UNCERTAINTY_ASSIGNED_CONTEXT ( ( #70949 ) ) GLOBAL_UNIT_ASSIGNED_CONTEXT ( ( #108005, #207555, #174032 ) ) REPRESENTATION_CONTEXT ( 'NONE', 'WORKASPACE' ) );
#197928 = CARTESIAN_POINT ( 'NONE',  ( -1.360316468750062624, 1.401041667008104730, -0.7853790794158941324 ) ) ;
#197929 = CARTESIAN_POINT ( 'NONE',  ( 3.646780131951580461, 7.198401220678078971, -0.7216878364870267237 ) ) ;
#197930 = CARTESIAN_POINT ( 'NONE',  ( 0.000000000000000000, 8.920000000000001705, 0.000000000000000000 ) ) ;
#197931 = CARTESIAN_POINT ( 'NONE',  ( 8.433462717895558569, 14.01452863678292715, -8.474055829133085638 ) ) ;
#197932 = CARTESIAN_POINT ( 'NONE',  ( 0.1339853816830008371, 0.3136495386693045062, 1.814181566856580607 ) ) ;
#197933 = ORIENTED_EDGE ( 'NONE', *, *, #194701, .T. ) ;
#197934 = ORIENTED_EDGE ( 'NONE', *, *, #49638, .T. ) ;
#197935 = CARTESIAN_POINT ( 'NONE',  ( 5.257115172742783393, 7.717454145000224308, 1.254163143712288653 ) ) ;
#197936 = ADVANCED_FACE ( 'NONE', ( #128806 ), #114679, .T. ) ;
#197937 = CARTESIAN_POINT ( 'NONE',  ( 4.428871017648271291, 0.08965458760558722706, 1.868499062828571367 ) ) ;
#197938 = CARTESIAN_POINT ( 'NONE',  ( 6.535912570239620578, 9.782925877658371405, 1.199719254218452047 ) ) ;
#197939 = CARTESIAN_POINT ( 'NONE',  ( -1.441115678601552652, 8.287243072884001194, -3.161846531485744460 ) ) ;
#197940 = CARTESIAN_POINT ( 'NONE',  ( -6.561783159334130922, 9.638868871656395498, -1.082531754730538864 ) ) ;
#197941 = CARTESIAN_POINT ( 'NONE',  ( 5.443762371086860341, 6.309809840144842141, 1.199719254218462483 ) ) ;
#197942 = CARTESIAN_POINT ( 'NONE',  ( 1.323035253951538426, -1.778235669024318177, -0.8468731209588018505 ) ) ;
#197943 = CARTESIAN_POINT ( 'NONE',  ( 2.091422941747251851, -0.4390073250180903663, 1.967893905867940996 ) ) ;
#197944 = CARTESIAN_POINT ( 'NONE',  ( -6.997979842947967377, 11.31606025008131233, -0.7998128361456291469 ) ) ;
#197946 = CARTESIAN_POINT ( 'NONE',  ( 7.503511670520385479, 7.718794801887437274, 0.7998128361456281477 ) ) ;
#197945 = B_SPLINE_CURVE_WITH_KNOTS ( 'NONE', 3,
 ( #55177, #118111, #69261, #133263, #37857, #135377, #168919 ),
 .UNSPECIFIED., .F., .F.,
 ( 4, 3, 4 ),
 ( 6.124194260411441496E-16, 2.761892602837239034E-05, 5.460426739246099117E-05 ),
 .UNSPECIFIED. ) ;
#197947 = FILL_AREA_STYLE ('',( #144986 ) ) ;
#197948 = CARTESIAN_POINT ( 'NONE',  ( 2.554835828347111093, -1.907293181126702653, -1.079063956894068754 ) ) ;
#197949 = DIRECTION ( 'NONE',  ( -5.551115123125764829E-17, 0.000000000000000000, 1.000000000000000000 ) ) ;
#197950 = CARTESIAN_POINT ( 'NONE',  ( -9.001723924469462901, 12.58942944760136484, -1.199719254218446718 ) ) ;
#197951 = CARTESIAN_POINT ( 'NONE',  ( 0.000000000000000000, 0.000000000000000000, 0.000000000000000000 ) ) ;
#197952 = CARTESIAN_POINT ( 'NONE',  ( 5.517805331081858888, 5.539787095791365523, 1.040834085586084257E-14 ) ) ;
#197953 = CARTESIAN_POINT ( 'NONE',  ( 5.126391479742934187, 6.113783160189109722, -1.082531754730548412 ) ) ;
#197954 = CARTESIAN_POINT ( 'NONE',  ( 9.447334110624092673, 9.916311305349925220, -0.7998128361456281477 ) ) ;
#197955 = CARTESIAN_POINT ( 'NONE',  ( 4.227444969362701421, 3.826440640544909400, 1.214306433183764966E-14 ) ) ;
#197956 = CARTESIAN_POINT ( 'NONE',  ( 7.512626515748113576, 7.937354821227203594, 0.7216878364870267237 ) ) ;
#197957 = EDGE_LOOP ( 'NONE', ( #139713, #113717, #1991, #89345 ) ) ;
#197959 = CARTESIAN_POINT ( 'NONE',  ( 1.277990700441207661, 1.982931799766519676, -0.3463461644656241623 ) ) ;
#197958 = CARTESIAN_POINT ( 'NONE',  ( 4.616662711240536510, -0.08544939198026380023, 1.839383977539174264 ) ) ;
#197960 = CARTESIAN_POINT ( 'NONE',  ( 3.532835791020246141, 2.243242391287715964, -0.4999081842005962395 ) ) ;
#197962 = CARTESIAN_POINT ( 'NONE',  ( 1.270090995528074362, -0.8302864195119415980, -1.665510012463662148 ) ) ;
#197961 = CARTESIAN_POINT ( 'NONE',  ( 2.236732156574683827, 5.553345249405011508, 1.040834085586084257E-14 ) ) ;
#197963 = CARTESIAN_POINT ( 'NONE',  ( -3.285556943749998737, -3.930208332855377407, 1.896917185911908499 ) ) ;
#197964 = CARTESIAN_POINT ( 'NONE',  ( 5.572493885891085519, 0.7809320506734825917, 1.745880147543739325 ) ) ;
#197965 = CARTESIAN_POINT ( 'NONE',  ( -7.645908563102897126, 11.00764485934031889, 1.199719254218453823 ) ) ;
#197966 = CARTESIAN_POINT ( 'NONE',  ( -5.126391479742927970, 8.994890803093138487, 0.7216878364870267237 ) ) ;
#197968 = CARTESIAN_POINT ( 'NONE',  ( 1.850267049257280139, 0.5840378008528935849, 1.777222254475477659 ) ) ;
#197967 = CARTESIAN_POINT ( 'NONE',  ( 3.386350598701783454, -0.4101191253191734387, -2.049945593880502681 ) ) ;
#197969 = CARTESIAN_POINT ( 'NONE',  ( 7.456621297836078632, 8.762108271306003004, 1.082531754730558626 ) ) ;
#197970 = DIRECTION ( 'NONE',  ( -0.000000000000000000, 1.000000000000000000, -0.000000000000000000 ) ) ;
#197971 = EDGE_CURVE ( 'NONE', #191521, #191009, #106367, .T. ) ;
#197972 = CARTESIAN_POINT ( 'NONE',  ( 6.163598723784101452, 0.9525508894225950263, 1.575581956637741587 ) ) ;
#197973 = TOROIDAL_SURFACE ( 'NONE', #180824, 10.92000000000000171, 0.08000000000000000167 ) ;
#197974 = CARTESIAN_POINT ( 'NONE',  ( 5.020596955762157698, 4.751784624677624080, 1.040834085586084257E-14 ) ) ;
#197975 = CARTESIAN_POINT ( 'NONE',  ( -2.440293211016301606E-15, 1.187499999999993117, -1.225000000000025624 ) ) ;
#197976 = CARTESIAN_POINT ( 'NONE',  ( 5.566962092400322248, -1.562093814453187735, -0.7318214103424671713 ) ) ;
#197977 = CARTESIAN_POINT ( 'NONE',  ( -6.714312387265696458, 8.856450423275211037, 1.599625672291283607 ) ) ;
#197978 = CARTESIAN_POINT ( 'NONE',  ( 0.4043864329151745651, -0.9253471945274373001, -1.466404024333650247 ) ) ;
#197979 = DIRECTION ( 'NONE',  ( 0.000000000000000000, 0.000000000000000000, -1.000000000000000000 ) ) ;
#197980 = CARTESIAN_POINT ( 'NONE',  ( 1.889772045536127765, 3.296949564223940143, 0.4024211290685025255 ) ) ;
#197981 = LINE ( 'NONE', #115734, #51668 ) ;
#197982 = CARTESIAN_POINT ( 'NONE',  ( 4.188457025382522403, 1.166365143183651920, -1.831003835250759604 ) ) ;
#197983 = CARTESIAN_POINT ( 'NONE',  ( 3.000428103051573814, -0.5303778429210231904, -1.746945217264872507 ) ) ;
#197984 = CARTESIAN_POINT ( 'NONE',  ( 1.287862062775881888, -1.240280065097350226, -1.519972987346601023 ) ) ;
#197985 = CARTESIAN_POINT ( 'NONE',  ( 5.489508092091861080, -0.5117143178510559220, 2.054485130609058796 ) ) ;
#197987 = CARTESIAN_POINT ( 'NONE',  ( -0.6823417656249969321, 4.030208333674754506, -1.181850606188749264 ) ) ;
#197986 = CARTESIAN_POINT ( 'NONE',  ( 6.392113680008942644, -0.6066422732131382389, -2.210563551359717938 ) ) ;
#197988 = CARTESIAN_POINT ( 'NONE',  ( 1.598423149420358458, 8.713846000021369775, 2.499999999999998668 ) ) ;
#197989 = CARTESIAN_POINT ( 'NONE',  ( 9.901532256681887745, 10.44620914241737530, 0.000000000000000000 ) ) ;
#197990 = CARTESIAN_POINT ( 'NONE',  ( 1.278162280329109279, 2.088516533416693743, -0.3659721813360562459 ) ) ;
#197991 = CARTESIAN_POINT ( 'NONE',  ( -2.657034918598338180, 6.043698471765932112, -0.7216878364870267237 ) ) ;
#197992 = DIRECTION ( 'NONE',  ( 0.000000000000000000, -0.000000000000000000, 1.000000000000000000 ) ) ;
#197993 = AXIS2_PLACEMENT_3D ( 'NONE', #39893, #103822, #106003 ) ;
#197994 = CARTESIAN_POINT ( 'NONE',  ( -4.189106276498259618, 6.870745841681152655, 1.082531754730560403 ) ) ;
#197995 = TOROIDAL_SURFACE ( 'NONE', #132352, 12.17999999982603576, 0.5000000000000008882 ) ;
#197996 = CARTESIAN_POINT ( 'NONE',  ( 6.631686460494314872, 2.080164978358085559, -0.6217935382996344629 ) ) ;
#197998 = CARTESIAN_POINT ( 'NONE',  ( -1.500000000000015099, 12.26041666734946212, -0.8660254037844309360 ) ) ;
#197997 = CARTESIAN_POINT ( 'NONE',  ( 6.983263157960363010, 6.034173670577698267, 2.748703042679788044 ) ) ;
#198000 = ORIENTED_EDGE ( 'NONE', *, *, #187251, .F. ) ;
#197999 = CARTESIAN_POINT ( 'NONE',  ( 2.649351634902767483, 0.2746262237617850821, 2.204210978092531192 ) ) ;
#198001 = CARTESIAN_POINT ( 'NONE',  ( 6.170546107226446253, 1.392543322632183722, 1.458558933167881211 ) ) ;
#198003 = CARTESIAN_POINT ( 'NONE',  ( 4.118078732422246979, 2.047561256575948452, -0.2476526470514497091 ) ) ;
#198002 = CARTESIAN_POINT ( 'NONE',  ( 5.020596955762157698, 4.751784624677624080, 1.040834085586084257E-14 ) ) ;
#198005 = CARTESIAN_POINT ( 'NONE',  ( -0.2408018239684642792, 0.2331886253038339407, -2.134526469895109635 ) ) ;
#198004 = CARTESIAN_POINT ( 'NONE',  ( 5.234329823327693809, 8.264412672927770487, 1.199719254218451159 ) ) ;
#198006 = CARTESIAN_POINT ( 'NONE',  ( 5.875479466675786355, 7.948088359245467416, -1.599625672291283607 ) ) ;
#198007 = CARTESIAN_POINT ( 'NONE',  ( 3.285556943750000514, -3.201041666188709112, 1.896917185911906500 ) ) ;
#198008 = FILL_AREA_STYLE ('',( #165518 ) ) ;
#198009 = CARTESIAN_POINT ( 'NONE',  ( 4.352959896991869471, 0.3989296284454147412, -1.797357466088687961 ) ) ;
#198010 = EDGE_CURVE ( 'NONE', #95626, #204176, #154709, .T. ) ;
#198011 = CARTESIAN_POINT ( 'NONE',  ( 6.179819089730593795, 6.104210447640811665, 1.040834085586084257E-14 ) ) ;
#198012 = CARTESIAN_POINT ( 'NONE',  ( -4.936726087586472467, 4.653935278472638437, -0.1487728517622861069 ) ) ;
#198013 = CARTESIAN_POINT ( 'NONE',  ( 2.344387759578896890, 0.3747227385639141373, 1.683394173241028913 ) ) ;
#198014 = LINE ( 'NONE', #166600, #9759 ) ;
#198015 = CARTESIAN_POINT ( 'NONE',  ( 2.022535828336795127, -2.051039051814534719, 1.038070753253451439 ) ) ;
#198016 = CARTESIAN_POINT ( 'NONE',  ( 0.6823417656249917140, 4.155208333674755394, 1.181850606188765695 ) ) ;
#198017 = CARTESIAN_POINT ( 'NONE',  ( 1.652057636490380732, 0.6571787646297929664, -2.164825341390004709 ) ) ;
#198018 = CARTESIAN_POINT ( 'NONE',  ( 4.653012138262506703, -1.691843218806210247, 1.254050867608807129 ) ) ;
#198019 = CARTESIAN_POINT ( 'NONE',  ( -5.966997003790217136, 9.975597247814986801, -0.7216878364870338292 ) ) ;
#198020 = CARTESIAN_POINT ( 'NONE',  ( 1.950134490391452369, 0.5496875458596857111, 1.682295776093334139 ) ) ;
#198021 = CARTESIAN_POINT ( 'NONE',  ( 6.474182045725470402, 7.511966127223233869, -1.199719254218446718 ) ) ;
#198022 = CARTESIAN_POINT ( 'NONE',  ( 6.034787771414195312, 6.213209619504250547, -0.7216878364870458196 ) ) ;
#198023 = CARTESIAN_POINT ( 'NONE',  ( -6.033542053281340856, 6.997886136038390603, -1.199719254218446718 ) ) ;
#198024 = CARTESIAN_POINT ( 'NONE',  ( -0.7500000000000006661, 2.108333333333357817, -1.299038105676652011 ) ) ;
#198025 = AXIS2_PLACEMENT_3D ( 'NONE', #52679, #153386, #170694 ) ;
#198026 = CARTESIAN_POINT ( 'NONE',  ( -3.262708522383007903, 6.958243709422141876, 1.040834085586084257E-14 ) ) ;
#198027 = CARTESIAN_POINT ( 'NONE',  ( 4.535507215201760367, -0.1075840215562298280, 2.218897223943790742 ) ) ;
#198028 = CARTESIAN_POINT ( 'NONE',  ( 3.644632398932126094, -1.791719913761843364, 1.261548167004488130 ) ) ;
#198029 = CARTESIAN_POINT ( 'NONE',  ( -4.303823697334223652, 7.108545849276850959, -1.199719254218452047 ) ) ;
#198030 = CARTESIAN_POINT ( 'NONE',  ( -5.483346782084204563, 5.361935765378481378, 0.000000000000000000 ) ) ;
#198031 = DIRECTION ( 'NONE',  ( -0.000000000000000000, 1.000000000000000000, 9.023263958591317418E-17 ) ) ;
#198032 = CARTESIAN_POINT ( 'NONE',  ( -0.6823417656250212460, 3.051041667008084879, 1.181850606188767472 ) ) ;
#198033 = CARTESIAN_POINT ( 'NONE',  ( 6.610000000000026077, 2.442988107647511509, 2.382821027452782570 ) ) ;
#198034 = CARTESIAN_POINT ( 'NONE',  ( -3.443407828190963915, 6.961133532957338943, 0.7216878364870317197 ) ) ;
#198035 = CARTESIAN_POINT ( 'NONE',  ( 5.713165544288242970, 1.732532623411761286, -1.222520872474173848 ) ) ;
#198036 = CARTESIAN_POINT ( 'NONE',  ( -5.614485009834902840, 9.564333254867113610, 0.7216878364870267237 ) ) ;
#198037 = ORIENTED_EDGE ( 'NONE', *, *, #118416, .T. ) ;
#198039 = CARTESIAN_POINT ( 'NONE',  ( 6.280167721515548251, -1.160692707240444710, 1.823489969145650313 ) ) ;
#198038 = CARTESIAN_POINT ( 'NONE',  ( -4.584065335196305213, 6.441438539186039591, 1.443375672974058777 ) ) ;
#198040 = CARTESIAN_POINT ( 'NONE',  ( 3.981290663907289140, 7.796589541200495965, -0.7998128361456221525 ) ) ;
#198041 = CARTESIAN_POINT ( 'NONE',  ( 6.515202330376022921, -1.784155196879381622, 0.4545711315065634195 ) ) ;
#198042 = SURFACE_SIDE_STYLE ('',( #50736 ) ) ;
#198043 = CARTESIAN_POINT ( 'NONE',  ( -0.6823417656250212460, 3.113541667008084879, 1.181850606188767472 ) ) ;
#198044 = CARTESIAN_POINT ( 'NONE',  ( 0.9776059304600862587, -1.697647217183468449, -0.3827929467696991050 ) ) ;
#198045 = CARTESIAN_POINT ( 'NONE',  ( 2.523789150438203510, 6.096171108819874007, 0.7998128361456462443 ) ) ;
#198046 = CARTESIAN_POINT ( 'NONE',  ( 0.6956633456795427994, -1.384754418207832405, -1.389998539416361645 ) ) ;
#198047 = CARTESIAN_POINT ( 'NONE',  ( -1.402160292154681736E-14, -0.1156249996585793222, 1.575800808251672791 ) ) ;
#198048 =( NAMED_UNIT ( * ) SI_UNIT ( $, .STERADIAN. ) SOLID_ANGLE_UNIT ( ) );
#198049 = CARTESIAN_POINT ( 'NONE',  ( 4.715790015261832835, -2.120648752638915724, 0.4184459369844309440 ) ) ;
#198050 = CARTESIAN_POINT ( 'NONE',  ( -4.634189577772691138, 4.300976017023221409, 1.214306433183764966E-14 ) ) ;
#198051 = CARTESIAN_POINT ( 'NONE',  ( -5.205967797523171292, 9.017453497178271604, 0.000000000000000000 ) ) ;
#198052 = CARTESIAN_POINT ( 'NONE',  ( 4.311504812833309330, -0.3723461477018601973, 2.129241309423899775 ) ) ;
#198053 = CARTESIAN_POINT ( 'NONE',  ( -2.823841133396259639, 6.516508098929413961, -0.7998128361456481317 ) ) ;
#198054 = CARTESIAN_POINT ( 'NONE',  ( -1.201851678989727383E-14, 3.321875000341421025, 1.575800808251672791 ) ) ;
#198055 = CARTESIAN_POINT ( 'NONE',  ( 6.011001170722232168, 1.737326539053269059, 0.9316862151012759163 ) ) ;
#198056 = CARTESIAN_POINT ( 'NONE',  ( 5.501237755103592697, 1.708535605516453115, 0.2940088878824585472 ) ) ;
#198057 = ADVANCED_FACE ( 'NONE', ( #49607 ), #194788, .T. ) ;
#198059 = CARTESIAN_POINT ( 'NONE',  ( 1.769323484426460480, 2.095969018468134770, -0.6401429536977767398 ) ) ;
#198058 = CARTESIAN_POINT ( 'NONE',  ( -0.6801582343750125492, -0.6510416663252707181, -1.178068619123848526 ) ) ;
#198060 = CARTESIAN_POINT ( 'NONE',  ( 3.294260915971382264, -0.9370450057796105847, 2.108945393182542372 ) ) ;
#198061 = CARTESIAN_POINT ( 'NONE',  ( 4.745419391729821967, -1.590323190411299770, -1.310567541734160457 ) ) ;
#198062 = CARTESIAN_POINT ( 'NONE',  ( 0.1462902992968219407, -1.560392365369901668, 1.155808223090015963 ) ) ;
#198063 = CARTESIAN_POINT ( 'NONE',  ( -6.765155463094763455, 8.915767345075790828, 1.443375672974078761 ) ) ;
#198065 = EDGE_CURVE ( 'NONE', #177076, #96508, #214193, .T. ) ;
#198064 = CARTESIAN_POINT ( 'NONE',  ( -3.806807270387036368, 7.663301925418665839, 0.000000000000000000 ) ) ;
#198066 = DIRECTION ( 'NONE',  ( 5.551115123125764213E-17, 0.000000000000000000, -1.000000000000000000 ) ) ;
#198067 = CARTESIAN_POINT ( 'NONE',  ( 3.533539421053989660, -0.1523460092780377639, 2.115156586662121363 ) ) ;
#198068 = DIRECTION ( 'NONE',  ( 0.000000000000000000, 0.000000000000000000, -1.000000000000000000 ) ) ;
#198069 = CARTESIAN_POINT ( 'NONE',  ( 1.406875202279284753, -1.122500148236497575, -1.674886495921081631 ) ) ;
#198070 = CARTESIAN_POINT ( 'NONE',  ( -7.185458225118419584, 7.485382138834033583, 1.040834085586084257E-14 ) ) ;
#198071 = CARTESIAN_POINT ( 'NONE',  ( 4.296070028909639404, -0.8476096858263427736, 2.037697185916572007 ) ) ;
#198072 = CARTESIAN_POINT ( 'NONE',  ( 3.285556943749998737, -1.042708332855377451, -1.896917185911906500 ) ) ;
#198073 =( BOUNDED_CURVE ( )  B_SPLINE_CURVE ( 2, ( #16570, #148737, #66376, #132524, #17632 ),
 .UNSPECIFIED., .F., .T. ) 
 B_SPLINE_CURVE_WITH_KNOTS ( ( 3, 2, 3 ),
 ( 0.2606479433802291745, 0.2625000000000000111, 0.2632879865674999098 ),
 .UNSPECIFIED. ) 
 CURVE ( )  GEOMETRIC_REPRESENTATION_ITEM ( )  RATIONAL_B_SPLINE_CURVE ( ( 0.9338382430890757036, 0.9404491509274826022, 1.000000000000000000, 0.9746631562710195151, 0.9589095569522538831 ) ) 
 REPRESENTATION_ITEM ( '' )  );
#198074 = CARTESIAN_POINT ( 'NONE',  ( 1.378881877344245277, 3.612814789602863730, 0.5904953584335879135 ) ) ;
#198075 = CARTESIAN_POINT ( 'NONE',  ( 2.876381804795541619, 6.437993120328354024, 0.3511878651327338674 ) ) ;
#198076 = CARTESIAN_POINT ( 'NONE',  ( 5.345847655232874196, 4.689681438633019894, -2.440353607042919926 ) ) ;
#198078 = CARTESIAN_POINT ( 'NONE',  ( -9.567965691386884686, -9.756398209953335510, 0.1670094623740840944 ) ) ;
#198077 = CARTESIAN_POINT ( 'NONE',  ( -4.624683998644739447, 8.449116153850892985, -0.4091045222319161234 ) ) ;
#198079 = CARTESIAN_POINT ( 'NONE',  ( 0.1100172516615156165, 7.047065462482140497, 3.945011421259203566 ) ) ;
#198080 = ORIENTED_EDGE ( 'NONE', *, *, #197691, .F. ) ;
#198081 = CARTESIAN_POINT ( 'NONE',  ( 4.241127833599818153, -1.794087422336073878, 1.013995622381487216 ) ) ;
#198082 = CARTESIAN_POINT ( 'NONE',  ( -0.6801582343750299797, 1.182291667008061875, 1.178068619123820771 ) ) ;
#198083 = CARTESIAN_POINT ( 'NONE',  ( -4.741601036477307574, 6.554953847355395880, 1.599625672291267398 ) ) ;
#198084 = CARTESIAN_POINT ( 'NONE',  ( 3.106122398345218638, -0.8164384046550461349, 1.847479848726358398 ) ) ;
#198085 = CARTESIAN_POINT ( 'NONE',  ( -0.7500000000000249800, -0.3083333333333132531, 1.299038105676659116 ) ) ;
#198086 = CARTESIAN_POINT ( 'NONE',  ( 2.333974999846879061, 5.874721266463329705, -0.7998128361456291469 ) ) ;
#198087 = CARTESIAN_POINT ( 'NONE',  ( 2.588805925060005730, -0.3509353788873382229, -2.030617818815634745 ) ) ;
#198088 = DIRECTION ( 'NONE',  ( -0.000000000000000000, -1.000000000000000000, -0.000000000000000000 ) ) ;
#198089 = CARTESIAN_POINT ( 'NONE',  ( 4.320244504248938355, 8.192035688265757898, 1.040834085586084257E-14 ) ) ;
#198090 = VECTOR ( 'NONE', #79200, 1000.000000000000000 ) ;
#198091 = CARTESIAN_POINT ( 'NONE',  ( -0.2409995289980003397, 4.087843961663322645, -2.555282842491034323 ) ) ;
#198092 = CARTESIAN_POINT ( 'NONE',  ( 1.780954670855667388, 1.268887097626215876, 1.334285251370644021 ) ) ;
#198093 = CARTESIAN_POINT ( 'NONE',  ( 6.305322857734435793, 1.832379230283949667, 1.229636283518860118 ) ) ;
#198094 = CARTESIAN_POINT ( 'NONE',  ( 6.119526231721748033, 8.232809585132461194, 1.599625672291269396 ) ) ;
#198095 = CARTESIAN_POINT ( 'NONE',  ( 1.774925396934714295, -2.051924176137665423, -0.6798970441593693570 ) ) ;
#198096 = CARTESIAN_POINT ( 'NONE',  ( -4.609409038966253647, 4.479991421656468908, -0.7216878364870207285 ) ) ;
#198097 = CARTESIAN_POINT ( 'NONE',  ( 1.481658059775035952, -0.6748446255696785023, 1.900416712880992343 ) ) ;
#198098 = CARTESIAN_POINT ( 'NONE',  ( 4.350813900535696277, 4.000456626940672500, 0.2320863031703649382 ) ) ;
#198099 = CARTESIAN_POINT ( 'NONE',  ( 0.5318453760667535279, 0.9654296485097979552, -1.602142582367314549 ) ) ;
#198100 = CARTESIAN_POINT ( 'NONE',  ( -4.827585214917754719, 7.789877296449459365, -1.199719254218453823 ) ) ;
#198101 = CARTESIAN_POINT ( 'NONE',  ( 4.926621433916460902, 1.886357061574754690, 0.5729670753305516895 ) ) ;
#198102 = CARTESIAN_POINT ( 'NONE',  ( 4.294157853547872605, -0.8666056138363428252, -1.820986994602634024 ) ) ;
#198104 = CARTESIAN_POINT ( 'NONE',  ( 8.703971429848968100, 13.09845773489176679, 0.000000000000000000 ) ) ;
#198103 = CARTESIAN_POINT ( 'NONE',  ( -0.6823417656250003738, 1.967708333674753174, -1.181850606188749264 ) ) ;
#198106 = CARTESIAN_POINT ( 'NONE',  ( 6.692010077984027916, -0.9030311967607449475, 1.901034507416640373 ) ) ;
#198105 = CARTESIAN_POINT ( 'NONE',  ( -7.552055258011950656, 8.769484874890757453, 1.199719254218462483 ) ) ;
#198107 = CARTESIAN_POINT ( 'NONE',  ( 5.283670394142272464, -1.967056725255760474, 0.6460906113585006549 ) ) ;
#198108 = CARTESIAN_POINT ( 'NONE',  ( 7.806797523370503811, 8.002351953554066810, 1.040834085586084257E-14 ) ) ;
#198109 = CARTESIAN_POINT ( 'NONE',  ( -5.876569516519495551, 8.943415971659659292, 1.199719254218452047 ) ) ;
#198110 = CARTESIAN_POINT ( 'NONE',  ( -1.512220381301933259, 8.756542408759468543, 2.494878041824271975 ) ) ;
#198111 = CARTESIAN_POINT ( 'NONE',  ( 5.625262229866254238, 1.783287769691415781, 0.9483128780355275511 ) ) ;
#198112 = CARTESIAN_POINT ( 'NONE',  ( -1.201851678989727383E-14, 5.696875000341416140, -1.575800808251660134 ) ) ;
#198113 = CARTESIAN_POINT ( 'NONE',  ( 3.651255599878608926, -1.887205614810626209, 1.327874790813722949 ) ) ;
#198114 = CARTESIAN_POINT ( 'NONE',  ( 0.9716179518045722219, -0.3065469058200780972, 2.039571770164672504 ) ) ;
#198115 = CARTESIAN_POINT ( 'NONE',  ( 8.609064354997688184, 9.146255957026539818, 1.040834085586084257E-14 ) ) ;
#198116 = CARTESIAN_POINT ( 'NONE',  ( 6.855582950365507244, 8.027210192628430718, -1.199719254218452047 ) ) ;
#198117 = CARTESIAN_POINT ( 'NONE',  ( 5.091969210384201361, 8.098325291160362482, 1.199719254218452047 ) ) ;
#198118 = CARTESIAN_POINT ( 'NONE',  ( 1.364683531249988757, 0.1968750003414204697, 0.000000000000000000 ) ) ;
#198119 = CARTESIAN_POINT ( 'NONE',  ( 3.528865121306874464, 7.339036084825155015, -0.7998128361456362523 ) ) ;
#198120 = CARTESIAN_POINT ( 'NONE',  ( 7.768458830506048685, 8.165549511786275971, -0.7216878364870267237 ) ) ;
#198122 = FACE_OUTER_BOUND ( 'NONE', #19970, .T. ) ;
#198121 = CARTESIAN_POINT ( 'NONE',  ( 4.369693832449129012, -0.3752608539947903665, 2.138364329090262306 ) ) ;
#198123 = CARTESIAN_POINT ( 'NONE',  ( -6.278834536460208504, 6.497930845391227450, 0.7216878364870173979 ) ) ;
#198125 = CARTESIAN_POINT ( 'NONE',  ( 2.788419073117563762, 1.577926727847511312, -0.9486480243563880643 ) ) ;
#198124 = CARTESIAN_POINT ( 'NONE',  ( -5.124618876285560454, 5.081069565195661220, 0.7216878364870317197 ) ) ;
#198126 = CARTESIAN_POINT ( 'NONE',  ( 1.364683531249990311, 4.613541667008083103, 0.7879004041258500513 ) ) ;
#198127 = CARTESIAN_POINT ( 'NONE',  ( 4.827760788416924242, 1.126602223531171898, -1.879657820484957664 ) ) ;
#198128 = CARTESIAN_POINT ( 'NONE',  ( 7.327176377373612048, 14.51562980571618056, 9.506369224037232613 ) ) ;
#198129 = CARTESIAN_POINT ( 'NONE',  ( 4.838899928913665605, 0.3820838354035635542, 2.229877907420589001 ) ) ;
#198130 = CARTESIAN_POINT ( 'NONE',  ( -5.249217764984337009, 6.599847349967512322, -1.403262209131036053 ) ) ;
#198131 = CARTESIAN_POINT ( 'NONE',  ( 5.088145468715395303, 7.830155539619080507, -1.136959649167136543 ) ) ;
#198132 = AXIS2_PLACEMENT_3D ( 'NONE', #21316, #5060, #137253 ) ;
#198133 = CARTESIAN_POINT ( 'NONE',  ( -5.438229012412890917, 8.398332043573416783, -1.082531754730549967 ) ) ;
#198134 = CARTESIAN_POINT ( 'NONE',  ( 3.933273961740296087, 6.642551151122080277, 1.082531754730549078 ) ) ;
#198135 = CARTESIAN_POINT ( 'NONE',  ( 6.573528787226094572, 1.692674132781073260, -0.5166258990680439034 ) ) ;
#198136 = CARTESIAN_POINT ( 'NONE',  ( 4.178388974671240597, 0.9510918172684652561, 1.774266679505158262 ) ) ;
#198137 = CARTESIAN_POINT ( 'NONE',  ( 5.960781091502512119, 10.10599504006161986, 0.7998128361456462443 ) ) ;
#198138 = CARTESIAN_POINT ( 'NONE',  ( 3.557739748072580088, 0.5135893094758836597, -2.042235538380641202 ) ) ;
#198139 = CARTESIAN_POINT ( 'NONE',  ( 0.5971114826688945776, -0.2799204757548044986, 1.894894164429518746 ) ) ;
#198140 = CARTESIAN_POINT ( 'NONE',  ( 2.488665619784910188, 1.909654154697162598, 0.4814545106021291265 ) ) ;
#198141 = CARTESIAN_POINT ( 'NONE',  ( 0.5670072068131201126, 0.1877032549213939472, -1.861219751863735672 ) ) ;
#198142 = CARTESIAN_POINT ( 'NONE',  ( 1.223018651738450480, -1.772137153356953432, -0.8420139538000551704 ) ) ;
#198144 = ORIENTED_EDGE ( 'NONE', *, *, #146212, .F. ) ;
#198143 = CARTESIAN_POINT ( 'NONE',  ( 0.1582721923853447621, 1.907395734848855051, 0.1385995803297388196 ) ) ;
#198145 = CARTESIAN_POINT ( 'NONE',  ( 4.012850279964918165, 7.625483060026979842, -0.7216878364870197293 ) ) ;
#198146 = CARTESIAN_POINT ( 'NONE',  ( -1.364683531250000748, 1.071875000341421247, 0.000000000000000000 ) ) ;
#198147 = CARTESIAN_POINT ( 'NONE',  ( 5.717618200960679964, -1.824738551054584157, 0.4112096411929695994 ) ) ;
#198148 = CARTESIAN_POINT ( 'NONE',  ( 9.083072846151447166, 12.68433652289702884, 1.199719254218450271 ) ) ;
#198149 = DIRECTION ( 'NONE',  ( 0.000000000000000000, 0.000000000000000000, 1.000000000000000000 ) ) ;
#198150 = CARTESIAN_POINT ( 'NONE',  ( 6.350451050988413115, -2.059726887988411637, -0.2088473404622398499 ) ) ;
#198151 = VECTOR ( 'NONE', #108301, 1000.000000000000000 ) ;
#198152 = CARTESIAN_POINT ( 'NONE',  ( 1.205626512970816355, -1.630946839658468983, -1.275175305487465049 ) ) ;
#198153 = CARTESIAN_POINT ( 'NONE',  ( -1.201851678989727383E-14, 1.962500000000020783, 1.732050807568877637 ) ) ;
#198154 = CARTESIAN_POINT ( 'NONE',  ( 8.098297826064319693, 8.342435640030188893, 0.7998128361456481317 ) ) ;
#198155 = CARTESIAN_POINT ( 'NONE',  ( -8.552495972122143186, 8.872333477097637200, 0.7998128361456462443 ) ) ;
#198156 = CARTESIAN_POINT ( 'NONE',  ( 4.692003678781083487, 7.631698837623355658, -1.199719254218450271 ) ) ;
#198157 = CARTESIAN_POINT ( 'NONE',  ( 5.074906250706387567, -1.535530725987072298, 1.462626433913247093 ) ) ;
#198158 = CARTESIAN_POINT ( 'NONE',  ( 5.110497557708379546, 4.926945003606695295, -0.7998128361456481317 ) ) ;
#198159 = CARTESIAN_POINT ( 'NONE',  ( 1.364683531249986537, 1.405208333674755838, -0.7879004041258239610 ) ) ;
#198160 = CARTESIAN_POINT ( 'NONE',  ( 0.7499999999999885647, 2.816666666666689522, -1.299038105676658228 ) ) ;
#198162 = CARTESIAN_POINT ( 'NONE',  ( 3.323720213644492993, 7.029424015893889433, 1.040834085586084257E-14 ) ) ;
#198161 = CARTESIAN_POINT ( 'NONE',  ( 6.127397123722368555, 0.1457569626216181913, -1.956525209266091192 ) ) ;
#198163 = CARTESIAN_POINT ( 'NONE',  ( 3.251327214347735417, -1.985796489957316613, -0.3474142817363469748 ) ) ;
#198164 = CARTESIAN_POINT ( 'NONE',  ( 3.854619899909034419, -1.789536248510626315, -0.6842995647342240417 ) ) ;
#198165 = CARTESIAN_POINT ( 'NONE',  ( -4.318600669050610463, 4.999583595936805125, 2.499999999999999556 ) ) ;
#198166 = AXIS2_PLACEMENT_3D ( 'NONE', #100775, #136499, #17374 ) ;
#198167 = CARTESIAN_POINT ( 'NONE',  ( 1.646283778714407342, 0.6915601415973006150, 2.079641132013386517 ) ) ;
#198168 = LINE ( 'NONE', #214383, #194610 ) ;
#198169 = CARTESIAN_POINT ( 'NONE',  ( 3.163207368312019430, 0.2779861718534247794, -1.849665920529340646 ) ) ;
#198170 = CARTESIAN_POINT ( 'NONE',  ( -0.7500000000000249800, -0.02708333265051543481, 1.299038105676659116 ) ) ;
#198171 = CARTESIAN_POINT ( 'NONE',  ( -7.019370843573183194, 9.212351955633947043, 1.599625672291283607 ) ) ;
#198173 = CARTESIAN_POINT ( 'NONE',  ( 6.099228927766127129, -0.2589519472634767006, 2.101251757753983984 ) ) ;
#198172 = CARTESIAN_POINT ( 'NONE',  ( -3.619663825168619731, 7.166765529431275539, 1.040834085586084257E-14 ) ) ;
#198174 = CARTESIAN_POINT ( 'NONE',  ( -1.364683531250014514, 8.651041667008065872, -0.7879004041258335089 ) ) ;
#198175 = CARTESIAN_POINT ( 'NONE',  ( 6.654741963219192868, -0.5482099483974657295, -1.996413779700876301 ) ) ;
#198177 = CARTESIAN_POINT ( 'NONE',  ( 6.620655732516625314, 7.629137130509059617, 2.773739711112707340 ) ) ;
#198176 = CARTESIAN_POINT ( 'NONE',  ( 2.191069407410517478, 1.617985365078830950, 1.324160459713573879 ) ) ;
#198179 = ORIENTED_EDGE ( 'NONE', *, *, #8087, .F. ) ;
#198178 = CARTESIAN_POINT ( 'NONE',  ( 0.3754632410046651048, 0.9867877818048297334, 1.414398233496700907 ) ) ;
#198180 = CARTESIAN_POINT ( 'NONE',  ( 7.287671262545424966, 8.461036880179857889, -1.199719254218451159 ) ) ;
#198182 = ADVANCED_FACE ( 'NONE', ( #81044 ), #82099, .F. ) ;
#198181 = CIRCLE ( 'NONE', #7854, 0.07999999999999982125 ) ;
#198183 = CARTESIAN_POINT ( 'NONE',  ( -0.09623479069434756616, -9.919835240146305466, -9.499512666137777117 ) ) ;
#198184 = CARTESIAN_POINT ( 'NONE',  ( 8.392133896734655707, 11.77427806529038357, 1.082531754730546636 ) ) ;
#198185 = CARTESIAN_POINT ( 'NONE',  ( 0.9398415344190423903, 7.435109595052201037, -4.383649807226275286 ) ) ;
#198187 = CARTESIAN_POINT ( 'NONE',  ( 1.365539917532717196, 0.5261944252722695614, -1.733370571883424693 ) ) ;
#198186 = CARTESIAN_POINT ( 'NONE',  ( 6.204791576909545192, 7.267953590263130259, -1.199719254218452047 ) ) ;
#198188 = CARTESIAN_POINT ( 'NONE',  ( -6.693975156845199059, 8.832723654451292816, 1.599625672291283607 ) ) ;
#198189 = CARTESIAN_POINT ( 'NONE',  ( 4.192495815123822744, 5.914331089109666983, -1.599625672291255185 ) ) ;
#198190 = CARTESIAN_POINT ( 'NONE',  ( -6.500216601102190239, 6.758717457939978246, 0.07576745652920421903 ) ) ;
#198191 = CARTESIAN_POINT ( 'NONE',  ( 6.550524494058025837, 7.671308660269694712, -1.199719254218452047 ) ) ;
#198192 = CARTESIAN_POINT ( 'NONE',  ( 6.539320575229274901, 7.629137130509072051, 2.496737603865983424 ) ) ;
#198193 = CARTESIAN_POINT ( 'NONE',  ( 6.773376349083131132, -7.473374494058229622, 6.661184041420955992 ) ) ;
#198194 = CARTESIAN_POINT ( 'NONE',  ( 9.734391104931955141, 10.45913716528321125, 0.7216878364870438212 ) ) ;
#198195 = ORIENTED_EDGE ( 'NONE', *, *, #180280, .F. ) ;
#198196 = EDGE_CURVE ( 'NONE', #93714, #135745, #72299, .T. ) ;
#198197 = CARTESIAN_POINT ( 'NONE',  ( 2.664321193032999524, -0.7092454343347885937, -1.720814620647417303 ) ) ;
#198198 = ADVANCED_FACE ( 'NONE', ( #78896 ), #95976, .T. ) ;
#198199 = CARTESIAN_POINT ( 'NONE',  ( -0.08845379458875551881, -1.178863245278682026, -1.510317944339079732 ) ) ;
#198200 = CARTESIAN_POINT ( 'NONE',  ( 6.106463915388694375, -0.6937866221692154944, -1.797298315204816310 ) ) ;
#198201 = CARTESIAN_POINT ( 'NONE',  ( 5.034901488060123498, 4.768473245691916773, 0.3558765841190755230 ) ) ;
#198202 = CARTESIAN_POINT ( 'NONE',  ( 4.812442952513422689, 8.115120723895499211, -0.8517184758452013282 ) ) ;
#198203 = CARTESIAN_POINT ( 'NONE',  ( -3.958617665510279160, 5.641473247893851628, -1.443375672974053447 ) ) ;
#198204 = CARTESIAN_POINT ( 'NONE',  ( 9.246297574839980271, 10.85006392781057905, 1.082531754730549967 ) ) ;
#198205 = CARTESIAN_POINT ( 'NONE',  ( 5.172688686914132639, 1.361056241693802349, -1.423677202773800721 ) ) ;
#198206 = CARTESIAN_POINT ( 'NONE',  ( 1.612141420133822223, -0.7113448269009944314, 1.997755531611951962 ) ) ;
#198207 = CARTESIAN_POINT ( 'NONE',  ( -6.417086777969760902, 6.381022750586497594, 0.7998128361456341429 ) ) ;
#198208 = DIRECTION ( 'NONE',  ( 1.000000000000000000, 0.000000000000000000, 0.000000000000000000 ) ) ;
#198209 = CARTESIAN_POINT ( 'NONE',  ( 9.495347311156807635, -6.857257212219900921, -1.861063089699362494E-15 ) ) ;
#198210 = CARTESIAN_POINT ( 'NONE',  ( 6.333935822332933618, 2.167035306593240840, 0.3253760364356065860 ) ) ;
#198211 = DIRECTION ( 'NONE',  ( 0.7592566023653016805, -0.6507913734559627184, 4.115938288792103177E-15 ) ) ;
#198212 = CARTESIAN_POINT ( 'NONE',  ( 4.524389607583827910, 1.185449959155547850, -1.518358881950541139 ) ) ;
#198213 = CARTESIAN_POINT ( 'NONE',  ( -7.230575994789712801, 7.330093503543126054, 0.7998128361456341429 ) ) ;
#198214 = CARTESIAN_POINT ( 'NONE',  ( 0.1822601575737579360, -1.769359155225664226, -0.4491840103194589817 ) ) ;
#198215 = CARTESIAN_POINT ( 'NONE',  ( 1.454063653991678473, 0.6380318336138122159, -2.112638918738508398 ) ) ;
#198216 = FACE_OUTER_BOUND ( 'NONE', #42796, .T. ) ;
#198217 = ORIENTED_EDGE ( 'NONE', *, *, #155093, .T. ) ;
#198218 = CARTESIAN_POINT ( 'NONE',  ( 0.4019237886466816012, 10.70758545099816672, -1.499999999999998668 ) ) ;
#198219 = EDGE_LOOP ( 'NONE', ( #176138, #186667, #85521, #142293 ) ) ;
#198220 = CARTESIAN_POINT ( 'NONE',  ( 6.139503339746209321, 1.821095124518475217, -0.7503768741054758218 ) ) ;
#198221 = CARTESIAN_POINT ( 'NONE',  ( 1.892034919678585281, -0.5197426219408564085, -1.871140422112322232 ) ) ;
#198222 = CARTESIAN_POINT ( 'NONE',  ( 6.643951024375948755, -0.1027215121673381443, -2.296211363497886460 ) ) ;
#198224 = CARTESIAN_POINT ( 'NONE',  ( 4.768306509995578146, -0.7929947328253506011, -1.683642203456004127 ) ) ;
#198223 = CARTESIAN_POINT ( 'NONE',  ( -6.526270840131767059, 8.707344961610770540, -1.599625672291271394 ) ) ;
#198225 = CARTESIAN_POINT ( 'NONE',  ( 7.062871678076271920, 7.204714810702593120, -0.7998128361456341429 ) ) ;
#198226 = CYLINDRICAL_SURFACE ( 'NONE', #1668, 0.3999999999999993006 ) ;
#198227 = DIRECTION ( 'NONE',  ( 0.1510067114093955887, 0.000000000000000000, -0.9885327375000383388 ) ) ;
#198228 = CARTESIAN_POINT ( 'NONE',  ( -5.850506979496850057, 6.784345216623154151, -1.199719254218446718 ) ) ;
#198229 = CARTESIAN_POINT ( 'NONE',  ( -3.011319516011047082, 6.527306845405913549, 0.7216878364870328300 ) ) ;
#198230 = CARTESIAN_POINT ( 'NONE',  ( 0.02921319935947005314, -2.001080581411585513, 0.8940957790435491992 ) ) ;
#198231 = CARTESIAN_POINT ( 'NONE',  ( 5.517805331081858888, 5.539787095791365523, 1.040834085586084257E-14 ) ) ;
#198232 = EDGE_LOOP ( 'NONE', ( #124301, #108120, #130130, #147110 ) ) ;
#198233 = CARTESIAN_POINT ( 'NONE',  ( 2.460826785407684181, 8.202405370174474797, 2.499999999999999112 ) ) ;
#198234 = DIRECTION ( 'NONE',  ( -0.8003905296791196111, 0.000000000000000000, -0.5994789404140719036 ) ) ;
#198235 = CARTESIAN_POINT ( 'NONE',  ( 1.207329354700342305, -0.4456725867950651621, 1.770335049871730071 ) ) ;
#198236 = CARTESIAN_POINT ( 'NONE',  ( -2.950870989268691957, 6.594433254122103349, -0.7998128361456281477 ) ) ;
#198237 = CARTESIAN_POINT ( 'NONE',  ( 3.762146167370096883, 1.631196324480500115, -0.5889743285819144525 ) ) ;
#198238 = CARTESIAN_POINT ( 'NONE',  ( -6.594145116354495961, 6.771750247812114765, -0.2697605348319087604 ) ) ;
#198239 = CARTESIAN_POINT ( 'NONE',  ( 6.609000000000015973, 2.967897204652646614, 2.453190122791535366 ) ) ;
#198240 = CARTESIAN_POINT ( 'NONE',  ( 8.530051201292206287, 13.10347683481629488, 0.000000000000000000 ) ) ;
#198241 = CARTESIAN_POINT ( 'NONE',  ( 0.02974079377688309753, -1.184178705181990532, -1.520296634558585547 ) ) ;
#198242 = CARTESIAN_POINT ( 'NONE',  ( 4.557442073745519018, 1.573120015848201492, 1.171846803954358363 ) ) ;
#198243 = CARTESIAN_POINT ( 'NONE',  ( -7.395082721250053837, 10.71501471051202614, -1.199719254218446718 ) ) ;
#198244 = CARTESIAN_POINT ( 'NONE',  ( 6.582647274634798151, 7.638508894284114170, 1.199719254218462483 ) ) ;
#198245 = CARTESIAN_POINT ( 'NONE',  ( 4.758503674095369007, 2.114844282287762667, 0.1552407789479764433 ) ) ;
#198246 = CARTESIAN_POINT ( 'NONE',  ( -7.483210719738908168, 10.81783070874899799, 1.199719254218453823 ) ) ;
#198247 = CARTESIAN_POINT ( 'NONE',  ( 5.431895982697334091, 6.433277491268158954, -1.247050338538328029 ) ) ;
#198248 = CARTESIAN_POINT ( 'NONE',  ( 2.395452669547156077, -1.851176756146424074, 0.9269567275110508486 ) ) ;
#198250 = CARTESIAN_POINT ( 'NONE',  ( 0.6823417656249864960, -0.5114583329919111243, -1.181850606188749264 ) ) ;
#198249 = DIRECTION ( 'NONE',  ( 1.000000000000000000, 0.000000000000000000, 0.000000000000000000 ) ) ;
#198251 = ORIENTED_EDGE ( 'NONE', *, *, #62562, .F. ) ;
#198252 = CARTESIAN_POINT ( 'NONE',  ( 2.479437202158024878, -2.292751561675594907, -0.1657748548101884711 ) ) ;
#198253 = CARTESIAN_POINT ( 'NONE',  ( 7.456621297836061757, 11.64321591421002644, 0.7216878364870438212 ) ) ;
#198255 = CARTESIAN_POINT ( 'NONE',  ( -3.285556943750000070, -2.909374999522040817, 0.000000000000000000 ) ) ;
#198254 = CARTESIAN_POINT ( 'NONE',  ( 5.370438244788902971, 9.279612028980123384, -0.7216878364870458196 ) ) ;
#198256 = CARTESIAN_POINT ( 'NONE',  ( -10.85951921430376288, 4.658322617273027433, 5.107420070442172388 ) ) ;
#198257 = EDGE_LOOP ( 'NONE', ( #25865, #28859, #102024, #196309 ) ) ;
#198258 = ADVANCED_FACE ( 'NONE', ( #104783 ), #176949, .T. ) ;
#198259 = CARTESIAN_POINT ( 'NONE',  ( 4.500206361630255003, -0.8965733778899236395, 1.689174240301967389 ) ) ;
#198260 = DIRECTION ( 'NONE',  ( 0.000000000000000000, -1.000000000000000000, -0.000000000000000000 ) ) ;
#198261 = CARTESIAN_POINT ( 'NONE',  ( 4.858271033065001632, 0.6623171007707692182, 1.592740567422048947 ) ) ;
#198262 = CARTESIAN_POINT ( 'NONE',  ( 3.503138892209650024, -0.1435209762444041581, 2.011451614702438828 ) ) ;
#198263 = CARTESIAN_POINT ( 'NONE',  ( 5.572921396849181974, -1.036564899910274784, 2.051751470549934453 ) ) ;
#198264 = CARTESIAN_POINT ( 'NONE',  ( 1.224999999999979217, 1.208333334016137739, -0.7072540797573078075 ) ) ;
#198265 = CARTESIAN_POINT ( 'NONE',  ( 0.5224629442122545875, -1.184049029929446828, -1.862174541895257995 ) ) ;
#198266 = CARTESIAN_POINT ( 'NONE',  ( -3.675669043080673770, 7.302381293653823491, 0.000000000000000000 ) ) ;
#198267 = CARTESIAN_POINT ( 'NONE',  ( 5.360532716240259177, -1.281408969121943464, 1.220901466008792235 ) ) ;
#198269 = CARTESIAN_POINT ( 'NONE',  ( 2.379227630831231011, 2.094957926495308875, -0.9307781363587577239 ) ) ;
#198268 = CARTESIAN_POINT ( 'NONE',  ( 5.013482942003290255, 9.071090208970993274, -0.7998128361456481317 ) ) ;
#198270 = CARTESIAN_POINT ( 'NONE',  ( 6.386648935047418263, 1.599332519906123462, -0.9119682274050244786 ) ) ;
#198271 = B_SPLINE_CURVE_WITH_KNOTS ( 'NONE', 3,
 ( #40773, #206441, #55936, #106876, #41848, #207512, #107958, #173986, #10370, #192315 ),
 .UNSPECIFIED., .F., .F.,
 ( 4, 2, 2, 2, 4 ),
 ( 0.000000000000000000, 0.0002021113321160286787, 0.0004042226642320573575, 0.0006063339963480859820, 0.0008084453284641139560 ),
 .UNSPECIFIED. ) ;
#198272 = CARTESIAN_POINT ( 'NONE',  ( -2.137381772448751605, 5.645362501165475777, -0.7998128361456281477 ) ) ;
#198273 = CARTESIAN_POINT ( 'NONE',  ( -1.500000000000039524, 7.750000000000000000, -10.86128356754322688 ) ) ;
#198274 = CARTESIAN_POINT ( 'NONE',  ( -4.679499295372141709, 5.488445928469455559, 1.199719254218452935 ) ) ;
#198275 = CARTESIAN_POINT ( 'NONE',  ( -0.6801582343750316451, -0.7864583329919294652, 1.178068619123805227 ) ) ;
#198276 = CARTESIAN_POINT ( 'NONE',  ( 3.982994815507484354, 7.308283119008860851, -0.9368446653362592080 ) ) ;
#198277 = EDGE_CURVE ( 'NONE', #176259, #132336, #40604, .T. ) ;
#198278 = CARTESIAN_POINT ( 'NONE',  ( 6.531696417657103737, 1.982406992490031383, -0.5971068152322634992 ) ) ;
#198279 = CARTESIAN_POINT ( 'NONE',  ( 2.430875351317234756, -1.673853735218135741, 1.124246214196801485 ) ) ;
#198280 = CARTESIAN_POINT ( 'NONE',  ( -1.500000000000001332, -0.06874999931718445145, 0.000000000000000000 ) ) ;
#198281 = CARTESIAN_POINT ( 'NONE',  ( 5.408790948643045660, 1.457530049539386141, -1.259864545333173158 ) ) ;
#198282 = CARTESIAN_POINT ( 'NONE',  ( -1.402160292154681736E-14, 11.17187500034139802, 1.575800808251682339 ) ) ;
#198283 = CARTESIAN_POINT ( 'NONE',  ( 2.689914112924804090, 2.107969469017998421, -0.7009301692152307695 ) ) ;
#198284 = ORIENTED_EDGE ( 'NONE', *, *, #48644, .F. ) ;
#198285 = CARTESIAN_POINT ( 'NONE',  ( -4.285785955251283141, 8.014184357852876417, 0.000000000000000000 ) ) ;
#198286 = CARTESIAN_POINT ( 'NONE',  ( 9.297140650669039275, 11.86975006391249643, 1.599625672291281386 ) ) ;
#198287 = DIRECTION ( 'NONE',  ( -0.007014632059889177630, -1.866992567669147331E-16, -0.9999753971658824625 ) ) ;
#198288 = CARTESIAN_POINT ( 'NONE',  ( 5.653775904655955920, 0.7130309894091393375, 1.587888939141286038 ) ) ;
#198289 = CARTESIAN_POINT ( 'NONE',  ( 4.000408739481801312, 1.952204270133122810, 0.1946113827649766925 ) ) ;
#198291 = CARTESIAN_POINT ( 'NONE',  ( -6.643132081016132062, 8.773406732650713025, 1.443375672974078761 ) ) ;
#198290 = CARTESIAN_POINT ( 'NONE',  ( 3.876741858503734761, 6.610283703974623393, 1.199719254218462483 ) ) ;
#198292 = CARTESIAN_POINT ( 'NONE',  ( -5.733986265252455361, 6.108121862465037744, 0.6873297539724126937 ) ) ;
#198293 = CARTESIAN_POINT ( 'NONE',  ( 4.974029133664690683, 1.296991790296280422, 1.853570637303619817 ) ) ;
#198294 = CIRCLE ( 'NONE', #52976, 3.475000000000000089 ) ;
#198295 = CARTESIAN_POINT ( 'NONE',  ( 1.434110160756268737, 1.226943730116908160, 1.657962230405624515 ) ) ;
#198296 = CARTESIAN_POINT ( 'NONE',  ( -8.518600588087975822, 8.832788862391110385, 1.040834085586084257E-14 ) ) ;
#198297 = CARTESIAN_POINT ( 'NONE',  ( -4.406036734316906234, 4.242723732898890709, -0.7216878364870207285 ) ) ;
#198298 = CARTESIAN_POINT ( 'NONE',  ( 2.641812911801244113, -1.676132216910112493, -1.519885475924544593 ) ) ;
#198299 = ORIENTED_EDGE ( 'NONE', *, *, #140470, .T. ) ;
#198300 = CARTESIAN_POINT ( 'NONE',  ( 1.499999999999987566, -0.6937499993171849511, 0.000000000000000000 ) ) ;
#198301 = CARTESIAN_POINT ( 'NONE',  ( 2.460033746253722065, 0.7958763861501785275, 1.692906160045657860 ) ) ;
#198302 = CARTESIAN_POINT ( 'NONE',  ( 1.283399958720226497, 1.417952419849175305, -0.9979722560638002449 ) ) ;
#198303 = EDGE_CURVE ( 'NONE', #29350, #21442, #160168, .T. ) ;
#198304 = CARTESIAN_POINT ( 'NONE',  ( 5.337503337980974649, 0.8888059580158399475, -2.003405333693850654 ) ) ;
#198305 = CARTESIAN_POINT ( 'NONE',  ( 6.282281253371452934, -1.241832687457484985, 1.944794379655417682 ) ) ;
#198306 = CARTESIAN_POINT ( 'NONE',  ( 1.727488365587977359, -1.940856233752264348, 0.6934696639643816996 ) ) ;
#198307 = CARTESIAN_POINT ( 'NONE',  ( 3.591681417399609888, -1.939766604489696622, -0.09448766823863874453 ) ) ;
#198308 = CARTESIAN_POINT ( 'NONE',  ( -3.429849674132942727, 5.984946472254969230, -1.082531754730549078 ) ) ;
#198309 = CARTESIAN_POINT ( 'NONE',  ( 5.325416506339426981, -1.776575524504428794, 0.5857008802128694791 ) ) ;
#198310 = CARTESIAN_POINT ( 'NONE',  ( 0.8125000000000005551, 1.451031289061154306, 1.451031289061088136 ) ) ;
#198311 = EDGE_CURVE ( 'NONE', #17249, #127447, #111138, .T. ) ;
#198312 = CARTESIAN_POINT ( 'NONE',  ( 3.996677956334552029, 7.600660605679141035, 0.1064861495668877750 ) ) ;
#198313 = CARTESIAN_POINT ( 'NONE',  ( 6.380232485702068246, -0.2495653932444163448, 2.000551205290925783 ) ) ;
#198314 = CARTESIAN_POINT ( 'NONE',  ( -1.360316468750004448, 1.640625000341400241, -2.602085213965210642E-14 ) ) ;
#198316 = CARTESIAN_POINT ( 'NONE',  ( 4.219375079941334761, 1.978050461189932552, 0.3905991720301109082 ) ) ;
#198315 = AXIS2_PLACEMENT_3D ( 'NONE', #69331, #120320, #52051 ) ;
#198317 = CARTESIAN_POINT ( 'NONE',  ( -3.755245360860939297, 4.443836344834937613, -1.082531754730548412 ) ) ;
#198318 = CARTESIAN_POINT ( 'NONE',  ( 7.771848369131631351, 10.09024240211882351, -1.599625672291262513 ) ) ;
#198319 = CARTESIAN_POINT ( 'NONE',  ( 4.095444919779759552, 6.935713618788495793, 1.199719254218451159 ) ) ;
#198321 = LINE ( 'NONE', #195155, #171350 ) ;
#198320 = CARTESIAN_POINT ( 'NONE',  ( 2.631258204695927194, -1.703542010001803275, 0.6570300758180421807 ) ) ;
#198322 = CARTESIAN_POINT ( 'NONE',  ( 10.98546216864998826, 11.25741378991010677, -1.592236800091192395 ) ) ;
#198323 = CARTESIAN_POINT ( 'NONE',  ( -9.470186914265017464, 4.005096909781187264, 6.837150237413082365 ) ) ;
#198324 = EDGE_LOOP ( 'NONE', ( #64461, #9340, #98812, #155191, #106051, #159853, #40309, #119952, #133503 ) ) ;
#198325 = CARTESIAN_POINT ( 'NONE',  ( -4.787437638956927977, 7.639075441208117212, -1.082531754730549967 ) ) ;
#198326 = DIRECTION ( 'NONE',  ( 0.000000000000000000, 1.000000000000000000, 0.000000000000000000 ) ) ;
#198327 = CARTESIAN_POINT ( 'NONE',  ( -7.621654909176601045, 12.04368116068139472, 0.7998128361456481317 ) ) ;
#198328 = CARTESIAN_POINT ( 'NONE',  ( 0.3694064801790334918, -1.708597689296184274, -1.076810303892479226 ) ) ;
#198329 = CARTESIAN_POINT ( 'NONE',  ( 6.393255305546848177, -0.1058262492604696708, -2.218914918540932035 ) ) ;
#198330 = VERTEX_POINT ( 'NONE', #15819 ) ;
#198331 = CARTESIAN_POINT ( 'NONE',  ( -6.934069218746458318, 7.054445274817795486, -0.7998128361456362523 ) ) ;
#198332 = CARTESIAN_POINT ( 'NONE',  ( 5.168682875307768931, 7.053215992657626110, -1.599625672291256295 ) ) ;
#198333 = CARTESIAN_POINT ( 'NONE',  ( 6.262583990076592499, -1.459235794176002132, 1.455568404382314718 ) ) ;
#198334 = CARTESIAN_POINT ( 'NONE',  ( 5.256482491209823138, 1.942542154241846619, -0.5404887192124521178 ) ) ;
#198335 = VERTEX_POINT ( 'NONE', #115534 ) ;
#198336 = ORIENTED_EDGE ( 'NONE', *, *, #9020, .F. ) ;
#198337 = ORIENTED_EDGE ( 'NONE', *, *, #47209, .T. ) ;
#198338 = CARTESIAN_POINT ( 'NONE',  ( 2.907691925098776942, 6.443576416979776234, 0.4208059576237854205 ) ) ;
#198339 = CARTESIAN_POINT ( 'NONE',  ( 3.475000000000000533, -1.210416665710750683, 2.006292185433948827 ) ) ;
#198342 = ORIENTED_EDGE ( 'NONE', *, *, #34638, .T. ) ;
#198341 = CARTESIAN_POINT ( 'NONE',  ( -1.150222622689971441, 3.222854968409793575, -0.7749999999993560929 ) ) ;
#198340 = CARTESIAN_POINT ( 'NONE',  ( -5.119085517611572378, 8.129960982925583224, 1.199719254218452935 ) ) ;
#198343 = CARTESIAN_POINT ( 'NONE',  ( 4.930145672075521013, 8.107674077938057167, 1.051636801887654293 ) ) ;
#198344 = CARTESIAN_POINT ( 'NONE',  ( 5.132185397524263060, 0.2004025303571632666, -2.006139158026089220 ) ) ;
#198345 = CARTESIAN_POINT ( 'NONE',  ( 4.839718430358881385, 1.836437689789902628, 0.1323948491315785347 ) ) ;
#198346 = CARTESIAN_POINT ( 'NONE',  ( -0.02338929933909209349, 2.063686797106215387, -2.128951798380565918 ) ) ;
#198347 = CARTESIAN_POINT ( 'NONE',  ( 3.053680222918000453, -1.886840229487633414, -1.328398743635789803 ) ) ;
#198348 = CARTESIAN_POINT ( 'NONE',  ( 6.912678218121202534, 9.158153569265168770, 1.599625672291268286 ) ) ;
#198349 = CARTESIAN_POINT ( 'NONE',  ( 4.323607124742586016, -2.069909602744592014, 0.6229453038564189971 ) ) ;
#198350 = CARTESIAN_POINT ( 'NONE',  ( 7.958799866421889746, 9.244020251369077457, -1.199719254218441611 ) ) ;
#198351 = CARTESIAN_POINT ( 'NONE',  ( 0.7494335824394976475, 1.939781244166354002, -0.09678450214786055161 ) ) ;
#198352 = CARTESIAN_POINT ( 'NONE',  ( -5.461236948206312114, 5.265864615862458464, 0.7998128361456341429 ) ) ;
#198353 = EDGE_CURVE ( 'NONE', #124142, #67541, #62460, .T. ) ;
#198354 = CARTESIAN_POINT ( 'NONE',  ( 11.89197369110779334, 9.799999999999998934, 0.8056055387119843703 ) ) ;
#198355 = CARTESIAN_POINT ( 'NONE',  ( -5.438755897737433287, 6.374245297895642537, -1.199719254218453823 ) ) ;
#198356 = CARTESIAN_POINT ( 'NONE',  ( 2.957714569337116295, 1.861795396119047208, -0.1817069356538636715 ) ) ;
#198359 = CARTESIAN_POINT ( 'NONE',  ( -5.315678745009726924, 8.359319748223434487, -1.199719254218453823 ) ) ;
#198358 = CARTESIAN_POINT ( 'NONE',  ( -1.201851678989727383E-14, 5.696875000341416140, -1.575800808251660134 ) ) ;
#198357 = CARTESIAN_POINT ( 'NONE',  ( 1.687617486097678476, 1.829050272730630144, -0.5582976189952293389 ) ) ;
#198360 = CARTESIAN_POINT ( 'NONE',  ( 3.071135375186518690, -2.039199700013223815, -0.8442704067812344393 ) ) ;
#198361 = CARTESIAN_POINT ( 'NONE',  ( -5.088463259863680754, 6.638951673345857785, 1.365981757201965907 ) ) ;
#198362 = CARTESIAN_POINT ( 'NONE',  ( 3.837121167867449945, 4.435395103055503441, 1.199719254218464037 ) ) ;
#198363 = CARTESIAN_POINT ( 'NONE',  ( 6.116136693096175136, 9.189224337703940648, -1.082531754730548412 ) ) ;
#198364 = CARTESIAN_POINT ( 'NONE',  ( -3.704402285031864306, 5.344888637335695414, -1.599625672291256295 ) ) ;
#198365 = CARTESIAN_POINT ( 'NONE',  ( -6.251718229232846369, 9.347402796530044355, -1.082531754730549967 ) ) ;
#198366 = CARTESIAN_POINT ( 'NONE',  ( 0.9308618464644430324, 0.1408870404581187008, 1.966361230860876441 ) ) ;
#198367 = CARTESIAN_POINT ( 'NONE',  ( 6.305331169356420240, 1.914788864002760160, 1.287784001537124468 ) ) ;
#198368 = CARTESIAN_POINT ( 'NONE',  ( 1.187862215860764126, -1.241893603568875903, -1.518774446641702580 ) ) ;
#198369 = CARTESIAN_POINT ( 'NONE',  ( 5.225460488781804358, 0.2076664479006613828, -2.052122333454815539 ) ) ;
#198370 = CARTESIAN_POINT ( 'NONE',  ( 5.395781948558860286, 6.357795697149212444, -1.082531754730542195 ) ) ;
#198371 = CARTESIAN_POINT ( 'NONE',  ( 6.703580607314123085, 6.785541894813420072, 0.000000000000000000 ) ) ;
#198372 = ORIENTED_EDGE ( 'NONE', *, *, #60772, .F. ) ;
#198373 = CARTESIAN_POINT ( 'NONE',  ( -1.001543065824772872E-14, 4.634375000341418804, 1.575800808251672791 ) ) ;
#198374 = CARTESIAN_POINT ( 'NONE',  ( 3.469446951953614189E-15, -6.938893903907228378E-15, -5.500000000000003553 ) ) ;
#198375 = CARTESIAN_POINT ( 'NONE',  ( 4.989037339704528229, 4.922891105851139315, 1.040834085586084257E-14 ) ) ;
#198376 = CARTESIAN_POINT ( 'NONE',  ( 0.5851434883720012525, 2.077150299251043553, 0.6315224188822368134 ) ) ;
#198378 = CARTESIAN_POINT ( 'NONE',  ( 6.409700764581637067, -0.8744420883355051854, -1.620376909479949390 ) ) ;
#198377 = CARTESIAN_POINT ( 'NONE',  ( 7.721398836998350390, -5.827195405469540290, -7.721398836998385917 ) ) ;
#198379 = CARTESIAN_POINT ( 'NONE',  ( 11.91294103507069302, 12.48539910043597345, 1.446263142085445041 ) ) ;
#198380 = CARTESIAN_POINT ( 'NONE',  ( -9.540655113774946017, 4.518459255872632419, 7.145788969735951568 ) ) ;
#198381 = CARTESIAN_POINT ( 'NONE',  ( 1.141631569582121752, 0.7634220068381202262, -1.707866752806507460 ) ) ;
#198382 = CARTESIAN_POINT ( 'NONE',  ( 5.887991582945824476, -0.9777203880148609416, 1.927937229880334113 ) ) ;
#198383 = CARTESIAN_POINT ( 'NONE',  ( -5.854914268151548917, 6.175991412503675448, 0.9282606102084377531 ) ) ;
#198384 = CARTESIAN_POINT ( 'NONE',  ( 0.07735805125223639556, 7.629137130509110243, -2.688903128390319530 ) ) ;
#198385 = CARTESIAN_POINT ( 'NONE',  ( 6.374094191309353619, 6.920300110170956032, -0.8184029421815092187 ) ) ;
#198386 = CARTESIAN_POINT ( 'NONE',  ( -1.201851678989727383E-14, 5.759375000341417028, -1.575800808251660801 ) ) ;
#198387 = CARTESIAN_POINT ( 'NONE',  ( 0.8031952904608251620, 1.686239601473665140, -0.9019194118903075541 ) ) ;
#198388 = AXIS2_PLACEMENT_3D ( 'NONE', #137767, #40259, #138834 ) ;
#198389 = CARTESIAN_POINT ( 'NONE',  ( 3.203702280051218931, -1.767899805609447261, 0.08541964596707474211 ) ) ;
#198390 = CARTESIAN_POINT ( 'NONE',  ( 1.207504981961624813, 1.448612403150219885, 1.248453992567559512 ) ) ;
#198391 = AXIS2_PLACEMENT_3D ( 'NONE', #207439, #210640, #173915 ) ;
#198393 = CARTESIAN_POINT ( 'NONE',  ( 5.853135685669797361, 0.1356727809044282473, -1.910850313501164743 ) ) ;
#198392 = CARTESIAN_POINT ( 'NONE',  ( -5.608135385276092677, 5.599224824533729716, 0.4022279080854191391 ) ) ;
#198394 = CARTESIAN_POINT ( 'NONE',  ( 6.004353349036935406, 1.967244357045078607, 0.09818725807526038074 ) ) ;
#198395 = CARTESIAN_POINT ( 'NONE',  ( -1.500000000000011324, 4.379166666666688634, -0.8660254037844313801 ) ) ;
#198396 = CARTESIAN_POINT ( 'NONE',  ( 0.9320672075895162223, -2.067649466203642206, 0.4702014512557165515 ) ) ;
#198397 = DIRECTION ( 'NONE',  ( -0.000000000000000000, 0.000000000000000000, -1.000000000000000000 ) ) ;
#198398 = CARTESIAN_POINT ( 'NONE',  ( 4.117926171558832671, -0.9613396577640184182, -1.604580606731422554 ) ) ;
#198400 = ORIENTED_EDGE ( 'NONE', *, *, #107183, .F. ) ;
#198399 = CARTESIAN_POINT ( 'NONE',  ( 0.9085097582094739943, 1.384192474337717194, -1.190531929384466281 ) ) ;
#198402 = CARTESIAN_POINT ( 'NONE',  ( 4.637820276784100137, 8.319831082953612622, -0.4078742439591088731 ) ) ;
#198401 = CARTESIAN_POINT ( 'NONE',  ( 3.106307083854151774, -2.204334110825040494, 0.1085914373066959593 ) ) ;
#198403 = CARTESIAN_POINT ( 'NONE',  ( 0.6823417656249899377, 4.488541667008086655, -1.181850606188754593 ) ) ;
#198404 = CARTESIAN_POINT ( 'NONE',  ( 1.627463713854758298, 0.1539993984382737602, -2.057001629134532550 ) ) ;
#198405 = CARTESIAN_POINT ( 'NONE',  ( 5.286789834324991055, 8.255339675766103724, -1.199719254218452935 ) ) ;
#198406 = CARTESIAN_POINT ( 'NONE',  ( -7.883176251342026042, 11.28445716228600126, -1.199719254218446718 ) ) ;
#198407 = DIRECTION ( 'NONE',  ( -1.000000000000000000, 0.000000000000000000, 0.000000000000000000 ) ) ;
#198408 = CARTESIAN_POINT ( 'NONE',  ( 11.94651559118242901, 11.15130655878981791, -1.135242698369562042 ) ) ;
#198409 = CIRCLE ( 'NONE', #174185, 3.971937515251341644 ) ;
#198410 = CARTESIAN_POINT ( 'NONE',  ( 6.451426615364327155, -1.705040744490589066, 0.8662930942644477827 ) ) ;
#198411 = EDGE_LOOP ( 'NONE', ( #95245, #70744, #66066, #103281, #185595 ) ) ;
#198412 = CARTESIAN_POINT ( 'NONE',  ( 4.387213907293201487, 0.09840592021137170575, 2.068135374880715638 ) ) ;
#198413 = CARTESIAN_POINT ( 'NONE',  ( -1.201851678989727383E-14, 5.837500000000023448, -1.732050807568863648 ) ) ;
#198414 = CARTESIAN_POINT ( 'NONE',  ( 1.722176697685766200, -1.199285583244277253, -1.798187405066300038 ) ) ;
#198415 = CARTESIAN_POINT ( 'NONE',  ( -5.638797120722775169, 7.366710520292286901, -1.234282198493292793 ) ) ;
#198416 = CARTESIAN_POINT ( 'NONE',  ( 2.385421078170113507, 0.09676420124534937384, -2.017471438767451275 ) ) ;
#198417 = CARTESIAN_POINT ( 'NONE',  ( 5.300874872818840622, 6.247070775452521652, 1.082531754730560403 ) ) ;
#198418 = ORIENTED_EDGE ( 'NONE', *, *, #157150, .F. ) ;
#198420 = CARTESIAN_POINT ( 'NONE',  ( 6.968527767744088663, 11.07377346243604599, 0.7216878364870438212 ) ) ;
#198419 = CARTESIAN_POINT ( 'NONE',  ( 0.000000000000000000, -3.937499999999998224, -4.012584370867899430 ) ) ;
#198421 = DIRECTION ( 'NONE',  ( 3.497202527569253358E-15, -0.000000000000000000, 1.000000000000000000 ) ) ;
#198422 = CARTESIAN_POINT ( 'NONE',  ( 0.09298292169932984019, 1.756857073293972116, 0.9896806593640145033 ) ) ;
#198423 = CARTESIAN_POINT ( 'NONE',  ( 6.639320575229257670, 3.688898292602959650, 2.617366112374151399 ) ) ;
#198424 = CARTESIAN_POINT ( 'NONE',  ( 4.476244563333130699, -2.125884358948509689, -0.5320566845071761364 ) ) ;
#198425 = CARTESIAN_POINT ( 'NONE',  ( 1.499999999999990896, 3.556250000682818602, 1.214306433183764966E-14 ) ) ;
#198426 = CARTESIAN_POINT ( 'NONE',  ( 3.814637755342592307, -0.6046605605216844870, -1.814329123173196834 ) ) ;
#198427 = CARTESIAN_POINT ( 'NONE',  ( -3.567766978690493307, 7.314145241780881435, 1.040834085586084257E-14 ) ) ;
#198428 = CARTESIAN_POINT ( 'NONE',  ( 3.511198595814926993, 6.079853547550633230, 1.082531754730558626 ) ) ;
#198430 = CARTESIAN_POINT ( 'NONE',  ( 1.669546221992053603, 1.392560760841387246, 1.458543886677300394 ) ) ;
#198429 = CARTESIAN_POINT ( 'NONE',  ( 0.4169036860909946518, 3.145283463680713432, 0.4342470185718878550 ) ) ;
#198431 = CARTESIAN_POINT ( 'NONE',  ( -0.6823417656250039265, 12.13020833367473017, -1.181850606188755259 ) ) ;
#198433 = CARTESIAN_POINT ( 'NONE',  ( -5.655686355556086120, 6.627330832017406692, 1.199719254218452935 ) ) ;
#198432 = CARTESIAN_POINT ( 'NONE',  ( 0.9961154782066735658, -2.292545471836278992, 0.006648471028786878678 ) ) ;
#198434 = CARTESIAN_POINT ( 'NONE',  ( 4.049579987339441800, 0.5806670320154716514, -1.624208954244592773 ) ) ;
#198435 = CARTESIAN_POINT ( 'NONE',  ( 7.014364370223726830, 9.276787413384745662, -1.599625672291269396 ) ) ;
#198436 = CARTESIAN_POINT ( 'NONE',  ( 4.090809663021327758, 5.795697244990093644, 1.599625672291267398 ) ) ;
#198437 = CARTESIAN_POINT ( 'NONE',  ( -1.123270288250315163, 2.985197346350006331, -0.7749999999993613109 ) ) ;
#198438 = CARTESIAN_POINT ( 'NONE',  ( 0.7308173252688826560, -1.846041318942293286, -0.6644482084196751126 ) ) ;
#198439 = CARTESIAN_POINT ( 'NONE',  ( 0.6021629784135495989, -0.6261829430146518272, -1.762877433595814614 ) ) ;
#198440 = CARTESIAN_POINT ( 'NONE',  ( 3.032219910950674890, 6.689340329417765574, 0.7998128361456321445 ) ) ;
#198441 = CARTESIAN_POINT ( 'NONE',  ( 0.1753634416057497925, 6.947017063990798214, -2.739087685391654148 ) ) ;
#198442 = VERTEX_POINT ( 'NONE', #129688 ) ;
#198443 = CARTESIAN_POINT ( 'NONE',  ( 0.2392000317489213768, -0.1454578200970526591, -2.037356452166842580 ) ) ;
#198444 = ORIENTED_EDGE ( 'NONE', *, *, #169231, .F. ) ;
#198445 = CARTESIAN_POINT ( 'NONE',  ( 4.775916358578648158, 1.790991888885495431, -0.2707881515907252234 ) ) ;
#198446 = ORIENTED_EDGE ( 'NONE', *, *, #157926, .T. ) ;
#198447 = CARTESIAN_POINT ( 'NONE',  ( 4.532168488718122390, 8.509556680138327778, 0.7998128361456271485 ) ) ;
#198448 = FACE_OUTER_BOUND ( 'NONE', #16420, .T. ) ;
#198449 = CARTESIAN_POINT ( 'NONE',  ( 5.795527448272657089, 1.671165027121311430, -0.6995385440057879656 ) ) ;
#198450 = CARTESIAN_POINT ( 'NONE',  ( 7.322812364712459221, 7.715904978352238430, 0.000000000000000000 ) ) ;
#198451 = CARTESIAN_POINT ( 'NONE',  ( 2.276812203907196075, 5.628006997859904104, -0.5575630420769552842 ) ) ;
#198452 = CARTESIAN_POINT ( 'NONE',  ( 4.952123820727618586, 6.619828698506379006, -1.244621138126526194 ) ) ;
#198453 = EDGE_CURVE ( 'NONE', #23324, #18526, #90357, .T. ) ;
#198455 = CARTESIAN_POINT ( 'NONE',  ( 9.890836756369282057, 11.49806328964105617, -1.199719254218440723 ) ) ;
#198454 = CARTESIAN_POINT ( 'NONE',  ( 6.074623017180313944, 1.249363044128497524, -1.379498876745478109 ) ) ;
#198456 = CARTESIAN_POINT ( 'NONE',  ( 3.708511580433976107, 1.820041504565768742, 0.5977543794245043784 ) ) ;
#198457 = CIRCLE ( 'NONE', #11684, 0.07999999999999984901 ) ;
#198458 = CARTESIAN_POINT ( 'NONE',  ( -6.717748655460328067, -7.473374494057241080, -6.717748655458897211 ) ) ;
#198459 = CYLINDRICAL_SURFACE ( 'NONE', #56633, 0.3999999999999997446 ) ;
#198460 = AXIS2_PLACEMENT_3D ( 'NONE', #118827, #4976, #184813 ) ;
#198461 = CARTESIAN_POINT ( 'NONE',  ( 4.690757960648213931, 8.416375354157496602, 0.7216878364870438212 ) ) ;
#198463 = CARTESIAN_POINT ( 'NONE',  ( 5.999228916948370127, -0.2569761400621084491, 2.101594505611179109 ) ) ;
#198462 = CARTESIAN_POINT ( 'NONE',  ( -8.161645285746702783, 12.46574390010577105, 0.7216878364870478180 ) ) ;
#198464 = CARTESIAN_POINT ( 'NONE',  ( 0.1984014031938194922, -2.161264429664040421, -0.05129915172277095536 ) ) ;
#198465 = CARTESIAN_POINT ( 'NONE',  ( -5.367048706163331850, 7.354919138647580290, -1.599625672291271394 ) ) ;
#198466 = CARTESIAN_POINT ( 'NONE',  ( 3.691562964670865199, 7.528850235416478576, -0.7998128361456362523 ) ) ;
#198467 = CARTESIAN_POINT ( 'NONE',  ( 1.272165501999738435, -1.161393580401563375, 1.408505525491813515 ) ) ;
#198468 = CARTESIAN_POINT ( 'NONE',  ( -5.264643720808155791, 5.036505850564608089, 0.000000000000000000 ) ) ;
#198469 = CARTESIAN_POINT ( 'NONE',  ( 3.539906422930443775, 0.8216601389946125433, -1.630302437610211763 ) ) ;
#198470 = EDGE_CURVE ( 'NONE', #136464, #22324, #161687, .T. ) ;
#198471 = CARTESIAN_POINT ( 'NONE',  ( 10.87630568456067692, 9.715185551068161729, 7.311958335779218388 ) ) ;
#198472 = ORIENTED_EDGE ( 'NONE', *, *, #178034, .F. ) ;
#198473 = CARTESIAN_POINT ( 'NONE',  ( 2.506254056688070886, 1.969067392671639771, 0.05118484259234063610 ) ) ;
#198474 = CARTESIAN_POINT ( 'NONE',  ( 4.616706917144582256, -0.09184519841067168011, 1.939997386343417896 ) ) ;
#198475 = CARTESIAN_POINT ( 'NONE',  ( -2.844178363816758814, 6.540234867753325076, -0.7998128361456481317 ) ) ;
#198477 = CARTESIAN_POINT ( 'NONE',  ( 4.957343421279006179, -1.817532610912236724, 1.092287347377165485 ) ) ;
#198476 = CARTESIAN_POINT ( 'NONE',  ( 5.936491157937257235, 8.019268665717216749, 1.599625672291268286 ) ) ;
#198478 = CARTESIAN_POINT ( 'NONE',  ( -5.765600714192150811, 7.067438534624118418, -2.440103264412639472 ) ) ;
#198479 = CARTESIAN_POINT ( 'NONE',  ( 6.113440106766272031, 6.016660024919275429, -0.07562458862005703997 ) ) ;
#198480 = CYLINDRICAL_SURFACE ( 'NONE', #204982, 1.250000000000000000 ) ;
#198481 = EDGE_LOOP ( 'NONE', ( #152396, #100216 ) ) ;
#198482 = CARTESIAN_POINT ( 'NONE',  ( -8.012344526598182026E-15, 13.29687500034139980, -1.575800808251669460 ) ) ;
#198483 = CARTESIAN_POINT ( 'NONE',  ( 4.878955176071345434, 6.785476686873604280, -1.599625672291269396 ) ) ;
#198485 =( BOUNDED_CURVE ( )  B_SPLINE_CURVE ( 2, ( #130755, #163196, #127581, #95008, #63551, #14779, #129707 ),
 .UNSPECIFIED., .F., .T. ) 
 B_SPLINE_CURVE_WITH_KNOTS ( ( 3, 2, 2, 3 ),
 ( 0.2857142857142859760, 0.2916666666666668517, 0.2976190476190477274, 0.3035714285714285476 ),
 .UNSPECIFIED. ) 
 CURVE ( )  GEOMETRIC_REPRESENTATION_ITEM ( )  RATIONAL_B_SPLINE_CURVE ( ( 0.9999999999999937828, 0.8660254037844449249, 1.000000000000000000, 0.8660254037844387076, 1.000000000000000000, 0.8660254037844387076, 1.000000000000000000 ) ) 
 REPRESENTATION_ITEM ( '' )  );
#198484 = CARTESIAN_POINT ( 'NONE',  ( 11.04986239659823433, 12.49060768514300079, -1.056426191432995765 ) ) ;
#198486 = CARTESIAN_POINT ( 'NONE',  ( 5.039593146249602640, -1.293522693445446015, -1.288650932716684849 ) ) ;
#198487 = CARTESIAN_POINT ( 'NONE',  ( 0.000000000000000000, 14.00000000000000533, 0.000000000000000000 ) ) ;
#198488 = CARTESIAN_POINT ( 'NONE',  ( -8.188761592974046266, 10.57664116326830595, -1.443375672974059665 ) ) ;
#198489 = CARTESIAN_POINT ( 'NONE',  ( -6.604009391672221341, 6.765323812321595298, -0.2039879123204788036 ) ) ;
#198490 = DIRECTION ( 'NONE',  ( -0.000000000000000000, -1.000000000000000000, -0.000000000000000000 ) ) ;
#198491 = CARTESIAN_POINT ( 'NONE',  ( 5.260568668178753349, -1.354309965608934352, 1.290672426560689035 ) ) ;
#198492 = CARTESIAN_POINT ( 'NONE',  ( 7.182068686937156166, 9.402166106225269715, 1.599625672291281386 ) ) ;
#198493 = CARTESIAN_POINT ( 'NONE',  ( -4.273844736805831879, 6.009238164405336313, 1.599625672291267175 ) ) ;
#198494 = CARTESIAN_POINT ( 'NONE',  ( -1.364683531250014514, 10.40104166700806765, -0.7879004041258335089 ) ) ;
#198495 = CARTESIAN_POINT ( 'NONE',  ( -4.564291269294938225, 8.476756914152748124, 1.040834085586084257E-14 ) ) ;
#198496 = CARTESIAN_POINT ( 'NONE',  ( 4.844340958784499662, 4.546152628203684820, 0.7998128361456341429 ) ) ;
#198497 = CARTESIAN_POINT ( 'NONE',  ( -3.458738584817664385, 7.049295759013638474, 0.7216878364870338292 ) ) ;
#198498 = CARTESIAN_POINT ( 'NONE',  ( -6.891622154448065807, 6.934647356477856128, 1.040834085586084257E-14 ) ) ;
#198499 = CARTESIAN_POINT ( 'NONE',  ( 6.526262532640958902, 1.108799689610693751, 1.866440817598405966 ) ) ;
#198500 = CARTESIAN_POINT ( 'NONE',  ( 2.724332569758937339, 2.101576450279537767, 0.2563457491038360070 ) ) ;
#198501 = CARTESIAN_POINT ( 'NONE',  ( 8.727698198895078363, 11.20540053684285553, -1.599625672291257406 ) ) ;
#198502 = FACE_OUTER_BOUND ( 'NONE', #41179, .T. ) ;
#198503 = CARTESIAN_POINT ( 'NONE',  ( 6.297728486381423352, -1.495382609916453998, -1.431936454106122358 ) ) ;
#198505 = B_SPLINE_CURVE_WITH_KNOTS ( 'NONE', 3,
 ( #7022, #187920, #170611, #39551, #82159, #200950, #21131, #89388, #68822, #22198 ),
 .UNSPECIFIED., .F., .F.,
 ( 4, 3, 3, 4 ),
 ( 0.000000000000000000, 8.893179197954836847E-05, 0.0001334007970840206305, 0.0001778705873658964021 ),
 .UNSPECIFIED. ) ;
#198504 = CARTESIAN_POINT ( 'NONE',  ( 4.439983357641082762, 7.074277023141499754, -1.114066652139956926 ) ) ;
#198506 = CARTESIAN_POINT ( 'NONE',  ( 4.677199807034550183, 8.400557508274889784, 1.040834085586084257E-14 ) ) ;
#198507 = CARTESIAN_POINT ( 'NONE',  ( 1.737500000000001155, -2.683333333333332682, 3.009438278150922130 ) ) ;
#198508 = CARTESIAN_POINT ( 'NONE',  ( 2.308868829589076022, 2.048438961056008090, 1.028902946192054912 ) ) ;
#198510 = PLANE ( 'NONE',  #150611 ) ;
#198509 = CARTESIAN_POINT ( 'NONE',  ( -9.499771308870727182, -7.644320505141722677, -0.06917019444584229793 ) ) ;
#198511 = CARTESIAN_POINT ( 'NONE',  ( 2.320441991784210067, -0.7354482596747033973, -1.765520077574176394 ) ) ;
#198512 = ORIENTED_EDGE ( 'NONE', *, *, #36673, .F. ) ;
#198513 = CARTESIAN_POINT ( 'NONE',  ( 8.554831740098663317, 9.082984572977682802, 0.7216878364870458196 ) ) ;
#198514 = EDGE_CURVE ( 'NONE', #49203, #7674, #199673, .T. ) ;
#198515 = CARTESIAN_POINT ( 'NONE',  ( 0.1584477454876299096, 2.008078640038186258, 0.1440931537372847071 ) ) ;
#198516 = CARTESIAN_POINT ( 'NONE',  ( 0.8308171121041010299, -1.845250773774274267, -0.6662997747023179373 ) ) ;
#198517 = CARTESIAN_POINT ( 'NONE',  ( -8.448702279610222021, 13.00856975952063088, 1.040834085586084257E-14 ) ) ;
#198518 = CARTESIAN_POINT ( 'NONE',  ( -7.660520486921249983, 8.896027641951645748, -1.199719254218446718 ) ) ;
#198519 = CARTESIAN_POINT ( 'NONE',  ( 3.285556943749998737, -0.6927083328553748087, -1.896917185911906500 ) ) ;
#198521 = CARTESIAN_POINT ( 'NONE',  ( 2.236828121427667071, -1.582394523617111970, 0.7928310554637070240 ) ) ;
#198520 = CARTESIAN_POINT ( 'NONE',  ( 4.224618542793646014, 0.1023655851960032920, 2.088258538514795593 ) ) ;
#198522 = DIRECTION ( 'NONE',  ( 0.000000000000000000, 1.000000000000000000, -8.546850786086437571E-32 ) ) ;
#198524 = CARTESIAN_POINT ( 'NONE',  ( 5.367208288505312730, 2.210367218987763671, -0.6069939957479841830 ) ) ;
#198523 = CARTESIAN_POINT ( 'NONE',  ( -0.3282377607281401488, 1.948664549684637315, -1.225000000000025846 ) ) ;
#198525 = CARTESIAN_POINT ( 'NONE',  ( 3.503586914695429488, -0.7067764301678289840, -1.590537823618918711 ) ) ;
#198526 = CARTESIAN_POINT ( 'NONE',  ( 4.552840656090682891, 4.206068941727564514, 1.214306433183764966E-14 ) ) ;
#198527 =( NAMED_UNIT ( * ) SI_UNIT ( $, .STERADIAN. ) SOLID_ANGLE_UNIT ( ) );
#198528 = CARTESIAN_POINT ( 'NONE',  ( 3.549848462767680068, 1.568450346167485243, -0.7392937452721718428 ) ) ;
#198529 = CARTESIAN_POINT ( 'NONE',  ( 3.279888855285200577, -2.093262694144955027, 0.5762538248230695270 ) ) ;
#198530 = CARTESIAN_POINT ( 'NONE',  ( 3.876741858503734761, 6.610283703974623393, 1.199719254218462483 ) ) ;
#198531 = CARTESIAN_POINT ( 'NONE',  ( 5.524625123954316486, 0.3981063221985549072, 1.976670730632006601 ) ) ;
#198532 = CARTESIAN_POINT ( 'NONE',  ( 6.593749840436431420, -1.895867669153237456, -0.7852924748296338242 ) ) ;
#198533 =( BOUNDED_SURFACE ( )  B_SPLINE_SURFACE ( 3, 2, ( 
 ( #35605, #19351, #86500 ),
 ( #122301, #51879, #38822 ),
 ( #136334, #201289, #135274 ),
 ( #88652, #36670, #20418 ),
 ( #85431, #102759, #119064 ),
 ( #188258, #121224, #168814 ) ),
 .UNSPECIFIED., .F., .F., .T. ) 
 B_SPLINE_SURFACE_WITH_KNOTS ( ( 4, 2, 4 ),
 ( 3, 3 ),
 ( 0.000000000000000000, 0.0003831327362561326704, 0.0007662654725122653408 ),
 ( 0.000000000000000000, 1.000000000000000000 ),
 .UNSPECIFIED. ) 
 GEOMETRIC_REPRESENTATION_ITEM ( )  RATIONAL_B_SPLINE_SURFACE ( (
 ( 1.000000000000000000, 0.5879095031487664436, 1.000000000000000000),
 ( 1.000000000000000000, 0.5873691247589374331, 1.000000000000000000),
 ( 1.000000000000000000, 0.6054349545483206363, 1.000000000000000000),
 ( 1.000000000000000000, 0.6533334602780871414, 1.000000000000000000),
 ( 1.000000000000000000, 0.6828746263140246242, 1.000000000000000000),
 ( 1.000000000000000000, 0.7071067811865475727, 1.000000000000000000) ) ) 
 REPRESENTATION_ITEM ( '' )  SURFACE ( )  );
#198534 = CARTESIAN_POINT ( 'NONE',  ( 1.499999999999987121, 3.577083334016152527, -0.8660254037844262731 ) ) ;
#198535 = CARTESIAN_POINT ( 'NONE',  ( 1.993070439633041424, 1.677129747370089019, -0.9476047394562473469 ) ) ;
#198536 = CARTESIAN_POINT ( 'NONE',  ( -1.500000000000015099, 10.01041666734946745, -0.8660254037844309360 ) ) ;
#198537 = CARTESIAN_POINT ( 'NONE',  ( 6.205373625529961856, 1.933303589146176948, -1.094015395867214080 ) ) ;
#198538 = VERTEX_POINT ( 'NONE', #79772 ) ;
#198539 = CARTESIAN_POINT ( 'NONE',  ( 6.983263157960372780, 1.247263239625576059, 2.158450195331083510 ) ) ;
#198540 = CARTESIAN_POINT ( 'NONE',  ( -1.402160292154681736E-14, 1.837500000000019895, -1.732050807568863648 ) ) ;
#198541 = CARTESIAN_POINT ( 'NONE',  ( 4.950698647284403009, 8.927565521807144577, 1.040834085586084257E-14 ) ) ;
#198542 = CARTESIAN_POINT ( 'NONE',  ( 3.673896439178918172, 6.269667698141953238, 1.082531754730558626 ) ) ;
#198543 = CARTESIAN_POINT ( 'NONE',  ( 1.454100989278300560, -1.612054358864203785, -1.528463602881096284 ) ) ;
#198544 = DIRECTION ( 'NONE',  ( -0.000000000000000000, 1.000000000000000000, -0.000000000000000000 ) ) ;
#198545 = CARTESIAN_POINT ( 'NONE',  ( 7.280365300858406385, 11.43758391773608984, 1.040834085586084257E-14 ) ) ;
#198546 = CARTESIAN_POINT ( 'NONE',  ( 0.3372878420078945783, 3.351185588117788328, 1.972345798854260090 ) ) ;
#198547 = CARTESIAN_POINT ( 'NONE',  ( 5.228604516725597229, 6.129068686715179126, -1.199719254218450271 ) ) ;
#198548 = CARTESIAN_POINT ( 'NONE',  ( -3.174017359375036929, 6.717120995997236221, 0.7216878364870338292 ) ) ;
#198549 = CARTESIAN_POINT ( 'NONE',  ( 4.123522620141695683, 0.2556129913668835907, -2.046733346555211330 ) ) ;
#198550 = CARTESIAN_POINT ( 'NONE',  ( -3.893162665418476109, 7.693773542963529444, 1.040834085586084257E-14 ) ) ;
#198551 = CARTESIAN_POINT ( 'NONE',  ( -1.500000000000011324, 4.202083334016156080, 0.8660254037844403729 ) ) ;
#198552 = CARTESIAN_POINT ( 'NONE',  ( 0.6823417656249882723, 0.09270833367475139752, 1.181850606188755259 ) ) ;
#198553 = CARTESIAN_POINT ( 'NONE',  ( 5.501189692264965458, 1.528658022856645315, 1.077728667985423661 ) ) ;
#198554 = CARTESIAN_POINT ( 'NONE',  ( 4.834428552630634535, 0.5376618173574229109, -1.648781088846348108 ) ) ;
#198555 = CARTESIAN_POINT ( 'NONE',  ( 3.966134247641060817, -1.625707123410979449, -0.6219663355369866586 ) ) ;
#198556 = CARTESIAN_POINT ( 'NONE',  ( 4.253507506385319381, 5.985511395581417204, 1.599625672291267398 ) ) ;
#198557 = EDGE_CURVE ( 'NONE', #97415, #131991, #20503, .T. ) ;
#198558 = CARTESIAN_POINT ( 'NONE',  ( 1.628911237561550873, 0.2300632485819526785, 2.280818132175948421 ) ) ;
#198559 = CARTESIAN_POINT ( 'NONE',  ( -1.364683531249997417, 5.321875000341417916, 1.214306433183764966E-14 ) ) ;
#198560 = CARTESIAN_POINT ( 'NONE',  ( 6.058164993413670096, -1.477959563288837375, 1.479067623735799586 ) ) ;
#198561 = CARTESIAN_POINT ( 'NONE',  ( 1.077780131904103156, -1.795810734350095750, -0.4053039038426772267 ) ) ;
#198562 = DIRECTION ( 'NONE',  ( 0.000000000000000000, 0.000000000000000000, 1.000000000000000000 ) ) ;
#198563 = CARTESIAN_POINT ( 'NONE',  ( 1.688125190044654556, 1.678006053171029688, 1.117831401076685660 ) ) ;
#198564 = DIRECTION ( 'NONE',  ( -0.000000000000000000, -0.000000000000000000, -1.000000000000000000 ) ) ;
#198565 = CARTESIAN_POINT ( 'NONE',  ( 9.082291402135501457, 13.43266975004936192, -9.116315574465707172 ) ) ;
#198566 = CARTESIAN_POINT ( 'NONE',  ( -8.362681821530818738, 8.650883634741092010, -0.7998128361456291469 ) ) ;
#198567 = CARTESIAN_POINT ( 'NONE',  ( 6.017121246366603060, 5.914396297049491658, 1.040834085586084257E-14 ) ) ;
#198568 = CARTESIAN_POINT ( 'NONE',  ( 1.360316468749981800, -0.4739583329918962695, 0.7853790794158760358 ) ) ;
#198569 = CARTESIAN_POINT ( 'NONE',  ( 3.035902975225315714, -2.043024508941180706, 0.5676086983019896781 ) ) ;
#198570 = CARTESIAN_POINT ( 'NONE',  ( -1.402160292154681736E-14, -1.178124999658576311, 1.575800808251672791 ) ) ;
#198572 = ADVANCED_FACE ( 'NONE', ( #47307 ), #31048, .T. ) ;
#198571 = CARTESIAN_POINT ( 'NONE',  ( 5.215394836314163562, -0.2642288504575221464, 1.806346989861665087 ) ) ;
#198573 = EDGE_LOOP ( 'NONE', ( #46841, #41883, #76882, #115028, #73792 ) ) ;
#198574 = CARTESIAN_POINT ( 'NONE',  ( -5.336015975430226099, 8.383046517047350932, -1.199719254218453823 ) ) ;
#198575 = CARTESIAN_POINT ( 'NONE',  ( -2.580963302752292243, 0.4788041664876945269, 0.000000000000000000 ) ) ;
#198576 = CARTESIAN_POINT ( 'NONE',  ( 5.655159470231527763, 9.611786791996525636, -0.7216878364870458196 ) ) ;
#198577 = CARTESIAN_POINT ( 'NONE',  ( -1.737499999999997824, -3.397916665710751349, 3.009438278150925683 ) ) ;
#198578 = CARTESIAN_POINT ( 'NONE',  ( -7.217017841176048165, 7.314275657660511243, 1.040834085586084257E-14 ) ) ;
#198579 = CARTESIAN_POINT ( 'NONE',  ( 3.515882793631277536, -0.5824337298786783634, 1.934013565619496999 ) ) ;
#198580 = CARTESIAN_POINT ( 'NONE',  ( 6.809632187368197087, -0.4906261968062891055, 2.159508175712351541 ) ) ;
#198581 = CARTESIAN_POINT ( 'NONE',  ( -5.550083779947821760, 7.568460058062819407, -1.599625672291271394 ) ) ;
#198582 = CARTESIAN_POINT ( 'NONE',  ( 8.353795204314554468, 12.89784483834236184, -0.7998128361456352531 ) ) ;
#198583 = CARTESIAN_POINT ( 'NONE',  ( 4.873795578896718439, -1.825537460381383870, 0.3603196638213671532 ) ) ;
#198584 = CARTESIAN_POINT ( 'NONE',  ( 9.901532256681887745, 10.44620914241737530, 0.000000000000000000 ) ) ;
#198585 = CARTESIAN_POINT ( 'NONE',  ( 11.91826848330681976, 13.50729645956968206, -1.400000080589506757 ) ) ;
#198586 = CARTESIAN_POINT ( 'NONE',  ( -2.279742385392243165, 5.811449882932888222, -0.7998128361456281477 ) ) ;
#198587 = CARTESIAN_POINT ( 'NONE',  ( -6.482770005628665011, 10.71498210654212002, 0.7998128361456481317 ) ) ;
#198588 = CARTESIAN_POINT ( 'NONE',  ( 6.262583990076592499, -1.459235794176002132, 1.455568404382314718 ) ) ;
#198590 = CARTESIAN_POINT ( 'NONE',  ( -5.328671718129330159, 6.540706332611327944, 1.372188321006672540 ) ) ;
#198589 = CARTESIAN_POINT ( 'NONE',  ( -6.261886844665283114, 8.398896966899865646, 1.599625672291269396 ) ) ;
#198591 = CARTESIAN_POINT ( 'NONE',  ( -1.402160292154681736E-14, -0.05312499965857903073, -1.575800808251665908 ) ) ;
#198592 = CARTESIAN_POINT ( 'NONE',  ( 1.932526292592825046, 0.8863411937694037901, 1.489983018702551787 ) ) ;
#198593 = CARTESIAN_POINT ( 'NONE',  ( 1.007268549873532981, -0.7791258169532075950, -1.556267712415648763 ) ) ;
#198595 = CARTESIAN_POINT ( 'NONE',  ( 8.758204044748005401, 10.28062147603659504, 1.082531754730549967 ) ) ;
#198594 = CARTESIAN_POINT ( 'NONE',  ( 0.1304780226794301778, -1.424241760892838382, -1.816604428824322159 ) ) ;
#198596 = CARTESIAN_POINT ( 'NONE',  ( 3.607351389687783794, 6.366271167014519783, 1.199719254218451159 ) ) ;
#198597 = CARTESIAN_POINT ( 'NONE',  ( 2.794271844819782302, -2.055044804604218456, -0.1548302833056774130 ) ) ;
#198598 = CARTESIAN_POINT ( 'NONE',  ( 4.547870462380197765, 7.393267075163835855, 1.199719254218462483 ) ) ;
#198599 = CARTESIAN_POINT ( 'NONE',  ( 1.264999722075825561, -2.016288307338756525, -0.002813990012486000669 ) ) ;
#198600 = CARTESIAN_POINT ( 'NONE',  ( -0.3282377607281340426, 1.051335450315359576, 1.224999999999977440 ) ) ;
#198602 = CIRCLE ( 'NONE', #84359, 2.500000000000000888 ) ;
#198601 = CARTESIAN_POINT ( 'NONE',  ( -6.635789839245807897, 6.706452665400368218, 0.7998128361456341429 ) ) ;
#198603 = ADVANCED_FACE ( 'NONE', ( #99238 ), #82962, .T. ) ;
#198604 = CARTESIAN_POINT ( 'NONE',  ( 6.385618529757402406, 1.291587659170100766, 1.353439767483602285 ) ) ;
#198605 = AXIS2_PLACEMENT_3D ( 'NONE', #94022, #11665, #24712 ) ;
#198607 = CARTESIAN_POINT ( 'NONE',  ( -7.485510208520816278, 8.866088343763324886, 1.082531754730549078 ) ) ;
#198606 = CARTESIAN_POINT ( 'NONE',  ( 4.922078805074791674, -1.902621863305080430, 0.1933406509087298719 ) ) ;
#198608 = CARTESIAN_POINT ( 'NONE',  ( 6.463508838306311510, 0.3818026259072569983, -2.173449913608487716 ) ) ;
#198609 = CARTESIAN_POINT ( 'NONE',  ( -6.956742217143487395, 8.249192353823097790, 1.082531754730549078 ) ) ;
#198610 = CARTESIAN_POINT ( 'NONE',  ( 8.011942431032855083, 8.311964022485323511, 0.7998128361456291469 ) ) ;
#198611 = CARTESIAN_POINT ( 'NONE',  ( -4.217995187182965289, 6.014356699837137832, 1.443375672974065660 ) ) ;
#198612 = CARTESIAN_POINT ( 'NONE',  ( 6.551439628692993900, -1.894445571042557619, 0.9528467149547341641 ) ) ;
#198613 = ORIENTED_EDGE ( 'NONE', *, *, #163343, .T. ) ;
#198614 = CARTESIAN_POINT ( 'NONE',  ( -1.500000000000008216, 12.78125000068279427, 3.469446951953614189E-15 ) ) ;
#198615 = CARTESIAN_POINT ( 'NONE',  ( 3.522812192065057690, 1.465757825172078865, -1.782263946013421974 ) ) ;
#198616 = CARTESIAN_POINT ( 'NONE',  ( 5.318788500806308051, -1.422220495204097546, 1.351624447685224162 ) ) ;
#198617 = CARTESIAN_POINT ( 'NONE',  ( 1.375751926856683127, -1.915142299924106339, 0.4244507266663796741 ) ) ;
#198618 = CARTESIAN_POINT ( 'NONE',  ( -4.702146809683723561, 5.356480858934594025, -2.420000000000000373 ) ) ;
#198619 = CARTESIAN_POINT ( 'NONE',  ( 0.07538891330674882263, -7.154544010627095219, -9.499700864329891914 ) ) ;
#198620 = VERTEX_POINT ( 'NONE', #177290 ) ;
#198621 = CARTESIAN_POINT ( 'NONE',  ( -0.1529269513586241080, -1.894431756695889923, -0.9458152384202949126 ) ) ;
#198622 = CARTESIAN_POINT ( 'NONE',  ( -4.680589345215810049, 6.483773540883647435, -1.599625672291256295 ) ) ;
#198623 = CARTESIAN_POINT ( 'NONE',  ( 0.5504183687293667804, -1.553892155338543191, -0.9872222399871023457 ) ) ;
#198624 = CARTESIAN_POINT ( 'NONE',  ( 4.786072553063510426, -1.330480670633835683, -1.715586834332043953 ) ) ;
#198625 = CARTESIAN_POINT ( 'NONE',  ( -0.2929755972075621662, 2.708422268617026951, 2.051080643833458783 ) ) ;
#198626 = CARTESIAN_POINT ( 'NONE',  ( 1.459403507577087700, -1.788631592985808538, 1.138920039206146928 ) ) ;
#198627 = CARTESIAN_POINT ( 'NONE',  ( 1.499999999999987121, 3.077083334016149863, -0.8660254037844262731 ) ) ;
#198628 = CARTESIAN_POINT ( 'NONE',  ( 8.052653171512838881, 11.48218023581863001, -1.199719254218446718 ) ) ;
#198629 = CARTESIAN_POINT ( 'NONE',  ( -4.911285141672522059, 4.693790260148114513, 0.3511878651327460243 ) ) ;
#198630 = CARTESIAN_POINT ( 'NONE',  ( 6.177100234330334061, 7.056796855232915888, 1.058592334412721936 ) ) ;
#198631 = CARTESIAN_POINT ( 'NONE',  ( 2.460294058246147664, 0.8780975587320086762, 1.864460488959890139 ) ) ;
#198633 = DIRECTION ( 'NONE',  ( 0.000000000000000000, 1.000000000000000000, 0.000000000000000000 ) ) ;
#198632 = CARTESIAN_POINT ( 'NONE',  ( -8.748035429315585532, 11.22912730566677553, -1.599625672291263179 ) ) ;
#198634 = CARTESIAN_POINT ( 'NONE',  ( 1.364683531249986537, 1.905208333674750287, -0.7879004041258239610 ) ) ;
#198635 = CARTESIAN_POINT ( 'NONE',  ( -0.4019237886467001974, 9.301335450315374231, 1.500000000000001998 ) ) ;
#198636 = CARTESIAN_POINT ( 'NONE',  ( 5.868043296107601670, 7.273814737382555684, -1.316550679767941157 ) ) ;
#198637 = ORIENTED_EDGE ( 'NONE', *, *, #124980, .F. ) ;
#198638 = CARTESIAN_POINT ( 'NONE',  ( 4.371672787583542608, 0.4156390277068115480, -1.866406306929219605 ) ) ;
#198639 = CARTESIAN_POINT ( 'NONE',  ( 0.7500000000000006661, 9.447916667349467446, -1.299038105676657340 ) ) ;
#198640 = CARTESIAN_POINT ( 'NONE',  ( 1.423510532338147394, -0.05571650319935492202, 2.261890015172054458 ) ) ;
#198641 = CARTESIAN_POINT ( 'NONE',  ( -10.48008955368359629, 11.32911868882677986, 1.040834085586084257E-14 ) ) ;
#198642 = CARTESIAN_POINT ( 'NONE',  ( 0.8436869049191192405, -1.150191864323051982, -1.399547552825676666 ) ) ;
#198643 = CARTESIAN_POINT ( 'NONE',  ( 1.973720722908858249, -0.8152147109428582450, 1.733722481544483163 ) ) ;
#198644 = CARTESIAN_POINT ( 'NONE',  ( 3.086448098943677998, 1.152334561581969785, -1.719836228861029603 ) ) ;
#198645 = CARTESIAN_POINT ( 'NONE',  ( -1.364683531250014514, 1.051041667008090208, -0.7879004041258289570 ) ) ;
#198646 = CARTESIAN_POINT ( 'NONE',  ( 0.8484322082523039210, 0.5699466304493487900, 1.887293252202123739 ) ) ;
#198647 = CARTESIAN_POINT ( 'NONE',  ( 5.338475953816137931, 1.898335173771143580, 0.3273637156304096130 ) ) ;
#198649 = CARTESIAN_POINT ( 'NONE',  ( 6.039396378094620488, 7.052381734106362821, -1.030794243266313082 ) ) ;
#198648 = CARTESIAN_POINT ( 'NONE',  ( 1.401454987343775382, 1.884297621475890416, -1.332007787593261883 ) ) ;
#198650 = CARTESIAN_POINT ( 'NONE',  ( -1.402160292154681736E-14, 1.196875000341419026, -1.575800808251659024 ) ) ;
#198651 = CARTESIAN_POINT ( 'NONE',  ( 5.775849841709651322, -2.013224797598807569, 0.4483296186361291902 ) ) ;
#198652 = CARTESIAN_POINT ( 'NONE',  ( -6.762819695118240659, 6.784377820593065600, 0.7998128361456341429 ) ) ;
#198653 = CARTESIAN_POINT ( 'NONE',  ( 8.372323551638698902, 9.726464550788689323, 1.199719254218462483 ) ) ;
#198654 = CARTESIAN_POINT ( 'NONE',  ( 0.9999999999999833467, 8.600000000000013856, 0.4000000000000014655 ) ) ;
#198656 = CARTESIAN_POINT ( 'NONE',  ( -0.7500000000000215383, 4.191666666666690411, 1.299038105676671107 ) ) ;
#198655 = CARTESIAN_POINT ( 'NONE',  ( 5.403390757083595730, 1.719820611593615656, 1.215146281773227921 ) ) ;
#198657 = CARTESIAN_POINT ( 'NONE',  ( 1.364683531249988535, 3.217708333674748289, -0.7879004041258239610 ) ) ;
#198658 = CARTESIAN_POINT ( 'NONE',  ( 4.429101881081805914, 0.1011787780425543737, 2.159334005894457231 ) ) ;
#198659 = CARTESIAN_POINT ( 'NONE',  ( 5.830724911194343996, 1.354916080449189764, -1.497948107757952174 ) ) ;
#198660 = CARTESIAN_POINT ( 'NONE',  ( 0.000000000000000000, 9.719999999999998863, 0.000000000000000000 ) ) ;
#198661 = CARTESIAN_POINT ( 'NONE',  ( -3.958617665510266725, 7.562211676496538360, -0.7216878364870267237 ) ) ;
#198662 = CIRCLE ( 'NONE', #25811, 1.250000000000000444 ) ;
#198665 = CARTESIAN_POINT ( 'NONE',  ( 4.663641653420880218, 8.384739662392275861, -0.7216878364870207285 ) ) ;
#198664 = CARTESIAN_POINT ( 'NONE',  ( -1.642778471875000035, -2.267708332855375541, -2.845375778867859751 ) ) ;
#198663 = CARTESIAN_POINT ( 'NONE',  ( 7.876360894896227371, 8.153785563659219804, -0.7998128361456341429 ) ) ;
#198666 =( BOUNDED_SURFACE ( )  B_SPLINE_SURFACE ( 1, 2, ( 
 ( #167780, #54032, #3109, #21491, #137429, #152591, #200253, #51905, #136362, #203447, #19376, #85456, #202382, #37780, #187220, #121250, #103854, #88679, #154738, #157952, #125518, #173134, #26853, #77742, #10597, #127660, #92957, #189360, #58300, #209856, #9544, #156881, #124456, #109260, #176325, #75619, #59361, #57236, #193623, #8468, #110318, #123396, #25785, #177388, #7390, #190415, #44198, #111385, #91896, #42072, #107111, #95089, #29002, #41000, #73470, #174212, #45265, #191479, #24715, #90818, #74554, #139571, #60424, #140655, #141729, #205598, #192545, #76673, #206669, #108186, #207737, #43147, #175268, #159004, #143863, #142788, #208794, #126584, #27932, #94025, #160064, #11668, #61494, #98270, #15918, #114581, #13795, #178459, #30068, #210928, #129785, #130832, #128717, #132921, #79869, #32194, #179525, #198926, #164328, #162209, #112446, #80943, #181623, #16978, #46331, #180572, #165385, #83059, #97219, #196824, #82001, #148088, #149135, #163271, #14853, #194689, #214093, #145978, #716, #211990, #66781, #50572, #63631, #64687, #65721, #115628, #116694, #182693, #31145, #34311, #131869, #161137, #197877, #12725, #78798, #147035, #96158, #195766, #213057, #47405, #144921, #48466, #113517, #49508, #33252, #99336, #62554, #152343, #150224, #6065, #35378, #203199, #1794, #118832, #55908, #100387, #68926, #137175, #204257, #184818, #135047, #200005, #188029, #122065, #67851, #166458, #52701, #138243, #3921, #133999, #51654, #101453, #18049, #153412, #117777, #36448, #84136, #71059, #103597, #183768, #167525, #19123, #85202, #151286, #2857, #170720, #201060, #102523, #168585, #20185, #86272, #38595, #69990, #136102, #37521, #169654, #53778, #202118, #119911, #185887, #21239, #87345, #4982, #54846, #72135, #120996, #186963, #104672, #22307, #154486, #88419, #9290, #110061, #8215, #74300, #26599, #205340, #92700, #189109, #56978, #10340, #42886, #123152, #40742, #176073, #191222, #108995, #207482, #106848, #172879, #24451, #89499, #140396, #75363, #7133, #11409, #90564, #125262, #58039, #158746, #93766, #156625, #141475, #27671, #206415, #124203, #76414, #190167, #142524, #41821, #107934, #208533, #175012, #173959, #25532, #159805, #77486, #60169, #91640, #157692, #59102, #126326, #143605, #139311, #192285, #43945, #209598, #61242, #127399, #39659, #105767, #171792, #23387, #155553, #73205, #196578, #194438, #197625, #46079, #115390, #49269, #112199, #96973, #212807, #147838, #16729, #82813, #211740, #181384, #31950, #33007, #180328, #99086, #463, #179272, #62311, #161959, #63378, #29822, #165138, #195515, #128470, #95906, #80700, #213855, #129534, #30896, #28746, #148890, #178205, #81756, #94830, #47151, #66532, #193371, #13549, #15669, #45016, #113268, #79621, #78552, #111126, #177129, #160882, #12477, #145740, #144669, #163021, #210682, #14603, #146791, #64444, #98034, #130588, #48220, #114333, #164088 ),
 ( #65476, #131626, #35119, #34064, #133744, #134798, #83875, #52455, #153153, #202943, #17788, #152093, #136916, #54587, #68675, #102264, #69741, #201869, #120734, #200804, #118580, #166197, #135846, #199752, #186707, #51397, #38335, #104412, #117517, #36188, #3664, #87083, #170461, #22046, #151037, #88157, #185635, #154225, #119651, #5797, #132674, #184568, #1536, #101190, #2606, #183510, #198680, #168339, #67598, #167279, #19934, #4728, #86020, #53517, #182437, #50325, #18864, #20986, #100135, #37268, #116443, #149967, #84948, #169400, #103338, #70803, #40487, #171531, #162501, #178750, #187773, #71874, #24195, #112739, #189917, #39405, #23124, #72953, #137984, #125010, #105499, #7952, #204001, #42633, #75109, #30363, #139055, #121806, #96450, #205082, #56724, #145211, #55650, #122892, #89241, #155292, #6875, #13016, #188851, #41562, #9035, #141220, #25279, #106591, #172619, #90298, #156368, #74044, #107675, #140134, #46618, #206160, #157441, #57788, #190967, #129005, #123948, #173704, #211217, #91381, #207230, #58854, #108742, #177679, #29291, #95383, #161435, #79093, #62844, #194982, #150512, #51936, #99613, #15145, #82281, #148374, #98553, #166748, #184045, #181908, #214375, #33540, #66005, #2073, #163560, #179808, #67075, #132155, #198160, #63912, #114857, #134280, #164614, #97504, #116985, #101742, #147313, #18343, #182985, #14071, #165679, #130068, #49794, #81231, #115919, #17267, #64963, #35663, #146266, #16199, #83343, #31427, #84423, #212278, #68146, #133210, #149428, #196063, #1010, #199215, #50863, #34602, #213340, #100670, #200285, #118060, #131116, #80160, #197104, #47693, #113807, #48744, #180857, #32478, #135331, #39955, #189388, #54065, #37809, #139602, #202409, #87628, #3143, #122357, #153699, #38878, #19410, #186175, #72421, #155834, #106062, #71345, #152622, #154767, #205625, #121275, #5268, #4209, #204546, #138523, #137462, #70277, #56194, #136393, #102814, #120200, #188313, #7418, #171003, #89788, #103884, #86560, #151574, #172085, #41030, #167810, #6350, #169933, #21517, #203477, #55130, #69212, #168869, #187250, #85488, #104962, #201345, #22601, #88708, #23677, #73500, #57264, #52985, #123426, #119121, #185101, #36727, #20472, #124483, #24745, #190441, #8498, #74581, #140684, #107140, #206700, #58327, #173166, #90846, #156910, #27908, #161115, #174190, #58279, #10577, #96136, #176305, #25762, #157930, #59341, #145959, #111362, #91874, #208771, #190393, #28981, #61473, #162188, #125495, #108163, #13775, #191458, #43123, #128697, #42051, #109237, #124435, #9523, #79850, #210908, #75595, #94005, #209836, #127638, #11648, #175247, #141707, #207718, #26833, #92936, #160044, #158980, #30046, #76651, #143842, #142766, #177367, #112426, #60401, #77720, #194665, #126563, #192523, #45245, #44177, #95067, #110297, #193603, #12702, #78779, #144900, #62535, #46310, #178440, #83039, #213038, #163252 ) ),
 .UNSPECIFIED., .F., .F., .T. ) 
 B_SPLINE_SURFACE_WITH_KNOTS ( ( 2, 2 ),
 ( 3, 2, 2, 2, 2, 2, 2, 2, 2, 2, 2, 2, 2, 2, 2, 2, 2, 2, 2, 2, 2, 2, 2, 2, 2, 2, 2, 2, 2, 2, 2, 2, 2, 2, 2, 2, 2, 2, 2, 2, 2, 2, 2, 2, 2, 2, 2, 2, 2, 2, 2, 2, 2, 2, 2, 2, 2, 2, 2, 2, 2, 2, 2, 2, 2, 2, 2, 2, 2, 2, 2, 2, 2, 2, 2, 2, 2, 2, 2, 2, 2, 2, 2, 2, 2, 2, 2, 2, 2, 2, 2, 2, 2, 2, 2, 2, 2, 2, 2, 2, 2, 2, 2, 2, 2, 2, 2, 2, 2, 2, 2, 2, 2, 2, 2, 2, 2, 2, 2, 2, 2, 2, 2, 2, 2, 2, 2, 2, 2, 2, 2, 2, 2, 2, 2, 2, 2, 2, 2, 2, 2, 2, 2, 2, 2, 2, 2, 2, 2, 2, 2, 2, 2, 2, 2, 2, 2, 2, 2, 2, 2, 2, 2, 2, 2, 2, 2, 2, 3 ),
 ( 0.000000000000000000, 1.000000000000000000 ),
 ( 0.000000000000000000, 0.005952380952380952051, 0.01190476190476190410, 0.01785714285714285615, 0.02380952380952380820, 0.02976190476190476025, 0.03571428571428571230, 0.04166666666666666435, 0.04761904761904761640, 0.05357142857142856845, 0.05952380952380952051, 0.06547619047619047949, 0.07142857142857142461, 0.07738095238095238360, 0.08333333333333332871, 0.08928571428571428770, 0.09523809523809523281, 0.1011904761904761918, 0.1071428571428571369, 0.1130952380952380959, 0.1190476190476190410, 0.1250000000000000000, 0.1309523809523809590, 0.1369047619047619180, 0.1428571428571428492, 0.1488095238095238082, 0.1547619047619047672, 0.1607142857142857262, 0.1666666666666666574, 0.1726190476190476164, 0.1785714285714285754, 0.1845238095238095344, 0.1904761904761904656, 0.1964285714285714246, 0.2023809523809523836, 0.2083333333333333426, 0.2142857142857142738, 0.2202380952380952328, 0.2261904761904761918, 0.2321428571428571508, 0.2380952380952380820, 0.2440476190476190410, 0.2500000000000000000, 0.2559523809523809312, 0.2619047619047619180, 0.2678571428571428492, 0.2738095238095238360, 0.2797619047619047672, 0.2857142857142856984, 0.2916666666666666852, 0.2976190476190476164, 0.3035714285714285476, 0.3095238095238095344, 0.3154761904761904656, 0.3214285714285714524, 0.3273809523809523836, 0.3333333333333333148, 0.3392857142857143016, 0.3452380952380952328, 0.3511904761904761640, 0.3571428571428571508, 0.3630952380952380820, 0.3690476190476190688, 0.3750000000000000000, 0.3809523809523809312, 0.3869047619047619180, 0.3928571428571428492, 0.3988095238095238360, 0.4047619047619047672, 0.4107142857142856984, 0.4166666666666666852, 0.4226190476190476164, 0.4285714285714285476, 0.4345238095238095344, 0.4404761904761904656, 0.4464285714285714524, 0.4523809523809523836, 0.4583333333333333148, 0.4642857142857143016, 0.4702380952380952328, 0.4761904761904761640, 0.4821428571428571508, 0.4880952380952380820, 0.4940476190476190688, 0.5000000000000000000, 0.5059523809523809312, 0.5119047619047618625, 0.5178571428571429047, 0.5238095238095238360, 0.5297619047619047672, 0.5357142857142856984, 0.5416666666666666297, 0.5476190476190476719, 0.5535714285714286031, 0.5595238095238095344, 0.5654761904761904656, 0.5714285714285713969, 0.5773809523809523281, 0.5833333333333333703, 0.5892857142857143016, 0.5952380952380952328, 0.6011904761904761640, 0.6071428571428570953, 0.6130952380952381375, 0.6190476190476190688, 0.6250000000000000000, 0.6309523809523809312, 0.6369047619047618625, 0.6428571428571429047, 0.6488095238095238360, 0.6547619047619047672, 0.6607142857142856984, 0.6666666666666666297, 0.6726190476190476719, 0.6785714285714286031, 0.6845238095238095344, 0.6904761904761904656, 0.6964285714285713969, 0.7023809523809523281, 0.7083333333333333703, 0.7142857142857143016, 0.7202380952380952328, 0.7261904761904761640, 0.7321428571428570953, 0.7380952380952381375, 0.7440476190476190688, 0.7500000000000000000, 0.7559523809523809312, 0.7619047619047618625, 0.7678571428571429047, 0.7738095238095238360, 0.7797619047619047672, 0.7857142857142856984, 0.7916666666666666297, 0.7976190476190476719, 0.8035714285714286031, 0.8095238095238095344, 0.8154761904761904656, 0.8214285714285713969, 0.8273809523809523281, 0.8333333333333333703, 0.8392857142857143016, 0.8452380952380952328, 0.8511904761904761640, 0.8571428571428570953, 0.8630952380952381375, 0.8690476190476190688, 0.8750000000000000000, 0.8809523809523809312, 0.8869047619047618625, 0.8928571428571429047, 0.8988095238095238360, 0.9047619047619047672, 0.9107142857142856984, 0.9166666666666666297, 0.9226190476190476719, 0.9285714285714286031, 0.9345238095238095344, 0.9404761904761904656, 0.9464285714285713969, 0.9523809523809523281, 0.9583333333333333703, 0.9642857142857143016, 0.9702380952380952328, 0.9761904761904761640, 0.9821428571428570953, 0.9880952380952381375, 0.9940476190476190688, 1.000000000000000000 ),
 .UNSPECIFIED. ) 
 GEOMETRIC_REPRESENTATION_ITEM ( )  RATIONAL_B_SPLINE_SURFACE ( (
 ( 1.000000000000000000, 0.8660254037844387076, 1.000000000000000000, 0.8660254037844387076, 1.000000000000000000, 0.8660254037844387076, 1.000000000000000000, 0.8660254037844387076, 1.000000000000000000, 0.8660254037844387076, 1.000000000000000000, 0.8660254037844387076, 1.000000000000000000, 0.8660254037844387076, 1.000000000000000000, 0.8660254037844387076, 1.000000000000000000, 0.8660254037844387076, 1.000000000000000000, 0.8660254037844387076, 1.000000000000000000, 0.8660254037844387076, 1.000000000000000000, 0.8660254037844387076, 1.000000000000000000, 0.8660254037844387076, 1.000000000000000000, 0.8660254037844387076, 1.000000000000000000, 0.8660254037844387076, 1.000000000000000000, 0.8660254037844387076, 1.000000000000000000, 0.8660254037844387076, 1.000000000000000000, 0.8660254037844387076, 1.000000000000000000, 0.8660254037844387076, 1.000000000000000000, 0.8660254037844387076, 1.000000000000000000, 0.8660254037844387076, 1.000000000000000000, 0.8660254037844387076, 1.000000000000000000, 0.8660254037844387076, 1.000000000000000000, 0.8660254037844387076, 1.000000000000000000, 0.8660254037844387076, 1.000000000000000000, 0.8660254037844387076, 1.000000000000000000, 0.8660254037844387076, 1.000000000000000000, 0.8660254037844387076, 1.000000000000000000, 0.8660254037844387076, 1.000000000000000000, 0.8660254037844387076, 1.000000000000000000, 0.8660254037844387076, 1.000000000000000000, 0.8660254037844387076, 1.000000000000000000, 0.8660254037844387076, 1.000000000000000000, 0.8660254037844387076, 1.000000000000000000, 0.8660254037844387076, 1.000000000000000000, 0.8660254037844387076, 1.000000000000000000, 0.8660254037844387076, 1.000000000000000000, 0.8660254037844387076, 1.000000000000000000, 0.8660254037844387076, 1.000000000000000000, 0.8660254037844387076, 1.000000000000000000, 0.8660254037844387076, 1.000000000000000000, 0.8660254037844387076, 1.000000000000000000, 0.8660254037844387076, 1.000000000000000000, 0.8660254037844387076, 1.000000000000000000, 0.8660254037844387076, 1.000000000000000000, 0.8660254037844387076, 1.000000000000000000, 0.8660254037844387076, 1.000000000000000000, 0.8660254037844387076, 1.000000000000000000, 0.8660254037844387076, 1.000000000000000000, 0.8660254037844387076, 1.000000000000000000, 0.8660254037844387076, 1.000000000000000000, 0.8660254037844387076, 1.000000000000000000, 0.8660254037844387076, 1.000000000000000000, 0.8660254037844387076, 1.000000000000000000, 0.8660254037844387076, 1.000000000000000000, 0.8660254037844387076, 1.000000000000000000, 0.8660254037844387076, 1.000000000000000000, 0.8660254037844387076, 1.000000000000000000, 0.8660254037844387076, 1.000000000000000000, 0.8660254037844387076, 1.000000000000000000, 0.8660254037844387076, 1.000000000000000000, 0.8660254037844387076, 1.000000000000000000, 0.8660254037844387076, 1.000000000000000000, 0.8660254037844387076, 1.000000000000000000, 0.8660254037844387076, 1.000000000000000000, 0.8660254037844387076, 1.000000000000000000, 0.8660254037844387076, 1.000000000000000000, 0.8660254037844387076, 1.000000000000000000, 0.8660254037844387076, 1.000000000000000000, 0.8660254037844387076, 1.000000000000000000, 0.8660254037844387076, 1.000000000000000000, 0.8660254037844387076, 1.000000000000000000, 0.8660254037844387076, 1.000000000000000000, 0.8660254037844387076, 1.000000000000000000, 0.8660254037844387076, 1.000000000000000000, 0.8660254037844387076, 1.000000000000000000, 0.8660254037844387076, 1.000000000000000000, 0.8660254037844387076, 1.000000000000000000, 0.8660254037844387076, 1.000000000000000000, 0.8660254037844387076, 1.000000000000000000, 0.8660254037844387076, 1.000000000000000000, 0.8660254037844387076, 1.000000000000000000, 0.8660254037844387076, 1.000000000000000000, 0.8660254037844387076, 1.000000000000000000, 0.8660254037844387076, 1.000000000000000000, 0.8660254037844387076, 1.000000000000000000, 0.8660254037844387076, 1.000000000000000000, 0.8660254037844387076, 1.000000000000000000, 0.8660254037844387076, 1.000000000000000000, 0.8660254037844387076, 1.000000000000000000, 0.8660254037844387076, 1.000000000000000000, 0.8660254037844387076, 1.000000000000000000, 0.8660254037844387076, 1.000000000000000000, 0.8660254037844387076, 1.000000000000000000, 0.8660254037844387076, 1.000000000000000000, 0.8660254037844387076, 1.000000000000000000, 0.8660254037844387076, 1.000000000000000000, 0.8660254037844387076, 1.000000000000000000, 0.8660254037844387076, 1.000000000000000000, 0.8660254037844387076, 1.000000000000000000, 0.8660254037844387076, 1.000000000000000000, 0.8660254037844387076, 1.000000000000000000, 0.8660254037844387076, 1.000000000000000000, 0.8660254037844387076, 1.000000000000000000, 0.8660254037844387076, 1.000000000000000000, 0.8660254037844387076, 1.000000000000000000, 0.8660254037844387076, 1.000000000000000000, 0.8660254037844387076, 1.000000000000000000, 0.8660254037844387076, 1.000000000000000000, 0.8660254037844387076, 1.000000000000000000, 0.8660254037844387076, 1.000000000000000000, 0.8660254037844387076, 1.000000000000000000, 0.8660254037844387076, 1.000000000000000000, 0.8660254037844387076, 1.000000000000000000, 0.8660254037844387076, 1.000000000000000000, 0.8660254037844387076, 1.000000000000000000, 0.8660254037844387076, 1.000000000000000000, 0.8660254037844387076, 1.000000000000000000, 0.8660254037844387076, 1.000000000000000000, 0.8660254037844387076, 1.000000000000000000, 0.8660254037844387076, 1.000000000000000000, 0.8660254037844387076, 1.000000000000000000, 0.8660254037844387076, 1.000000000000000000, 0.8660254037844387076, 1.000000000000000000, 0.8660254037844387076, 1.000000000000000000, 0.8660254037844387076, 1.000000000000000000, 0.8660254037844387076, 1.000000000000000000, 0.8660254037844387076, 1.000000000000000000, 0.8660254037844387076, 1.000000000000000000, 0.8660254037844387076, 1.000000000000000000, 0.8660254037844387076, 1.000000000000000000, 0.8660254037844387076, 1.000000000000000000, 0.8660254037844387076, 1.000000000000000000, 0.8660254037844387076, 1.000000000000000000, 0.8660254037844387076, 1.000000000000000000, 0.8660254037844387076, 1.000000000000000000, 0.8660254037844387076, 1.000000000000000000, 0.8660254037844387076, 1.000000000000000000, 0.8660254037844387076, 1.000000000000000000, 0.8660254037844387076, 1.000000000000000000, 0.8660254037844387076, 1.000000000000000000, 0.8660254037844387076, 1.000000000000000000, 0.8660254037844387076, 1.000000000000000000, 0.8660254037844387076, 1.000000000000000000, 0.8660254037844387076, 1.000000000000000000, 0.8660254037844387076, 1.000000000000000000, 0.8660254037844387076, 1.000000000000000000, 0.8660254037844387076, 1.000000000000000000, 0.8660254037844387076, 1.000000000000000000, 0.8660254037844387076, 1.000000000000000000, 0.8660254037844387076, 1.000000000000000000, 0.8660254037844387076, 1.000000000000000000, 0.8660254037844387076, 1.000000000000000000, 0.8660254037844387076, 1.000000000000000000, 0.8660254037844387076, 1.000000000000000000, 0.8660254037844387076, 1.000000000000000000, 0.8660254037844387076, 1.000000000000000000, 0.8660254037844387076, 1.000000000000000000, 0.8660254037844387076, 1.000000000000000000, 0.8660254037844387076, 1.000000000000000000, 0.8660254037844387076, 1.000000000000000000, 0.8660254037844387076, 1.000000000000000000, 0.8660254037844387076, 1.000000000000000000, 0.8660254037844387076, 1.000000000000000000, 0.8660254037844387076, 1.000000000000000000, 0.8660254037844387076, 1.000000000000000000, 0.8660254037844387076, 1.000000000000000000, 0.8660254037844387076, 1.000000000000000000),
 ( 1.000000000000000000, 0.8660254037844387076, 1.000000000000000000, 0.8660254037844387076, 1.000000000000000000, 0.8660254037844387076, 1.000000000000000000, 0.8660254037844387076, 1.000000000000000000, 0.8660254037844387076, 1.000000000000000000, 0.8660254037844387076, 1.000000000000000000, 0.8660254037844387076, 1.000000000000000000, 0.8660254037844387076, 1.000000000000000000, 0.8660254037844387076, 1.000000000000000000, 0.8660254037844387076, 1.000000000000000000, 0.8660254037844387076, 1.000000000000000000, 0.8660254037844387076, 1.000000000000000000, 0.8660254037844387076, 1.000000000000000000, 0.8660254037844387076, 1.000000000000000000, 0.8660254037844387076, 1.000000000000000000, 0.8660254037844387076, 1.000000000000000000, 0.8660254037844387076, 1.000000000000000000, 0.8660254037844387076, 1.000000000000000000, 0.8660254037844387076, 1.000000000000000000, 0.8660254037844387076, 1.000000000000000000, 0.8660254037844387076, 1.000000000000000000, 0.8660254037844387076, 1.000000000000000000, 0.8660254037844387076, 1.000000000000000000, 0.8660254037844387076, 1.000000000000000000, 0.8660254037844387076, 1.000000000000000000, 0.8660254037844387076, 1.000000000000000000, 0.8660254037844387076, 1.000000000000000000, 0.8660254037844387076, 1.000000000000000000, 0.8660254037844387076, 1.000000000000000000, 0.8660254037844387076, 1.000000000000000000, 0.8660254037844387076, 1.000000000000000000, 0.8660254037844387076, 1.000000000000000000, 0.8660254037844387076, 1.000000000000000000, 0.8660254037844387076, 1.000000000000000000, 0.8660254037844387076, 1.000000000000000000, 0.8660254037844387076, 1.000000000000000000, 0.8660254037844387076, 1.000000000000000000, 0.8660254037844387076, 1.000000000000000000, 0.8660254037844387076, 1.000000000000000000, 0.8660254037844387076, 1.000000000000000000, 0.8660254037844387076, 1.000000000000000000, 0.8660254037844387076, 1.000000000000000000, 0.8660254037844387076, 1.000000000000000000, 0.8660254037844387076, 1.000000000000000000, 0.8660254037844387076, 1.000000000000000000, 0.8660254037844387076, 1.000000000000000000, 0.8660254037844387076, 1.000000000000000000, 0.8660254037844387076, 1.000000000000000000, 0.8660254037844387076, 1.000000000000000000, 0.8660254037844387076, 1.000000000000000000, 0.8660254037844387076, 1.000000000000000000, 0.8660254037844387076, 1.000000000000000000, 0.8660254037844387076, 1.000000000000000000, 0.8660254037844387076, 1.000000000000000000, 0.8660254037844387076, 1.000000000000000000, 0.8660254037844387076, 1.000000000000000000, 0.8660254037844387076, 1.000000000000000000, 0.8660254037844387076, 1.000000000000000000, 0.8660254037844387076, 1.000000000000000000, 0.8660254037844387076, 1.000000000000000000, 0.8660254037844387076, 1.000000000000000000, 0.8660254037844387076, 1.000000000000000000, 0.8660254037844387076, 1.000000000000000000, 0.8660254037844387076, 1.000000000000000000, 0.8660254037844387076, 1.000000000000000000, 0.8660254037844387076, 1.000000000000000000, 0.8660254037844387076, 1.000000000000000000, 0.8660254037844387076, 1.000000000000000000, 0.8660254037844387076, 1.000000000000000000, 0.8660254037844387076, 1.000000000000000000, 0.8660254037844387076, 1.000000000000000000, 0.8660254037844387076, 1.000000000000000000, 0.8660254037844387076, 1.000000000000000000, 0.8660254037844387076, 1.000000000000000000, 0.8660254037844387076, 1.000000000000000000, 0.8660254037844387076, 1.000000000000000000, 0.8660254037844387076, 1.000000000000000000, 0.8660254037844387076, 1.000000000000000000, 0.8660254037844387076, 1.000000000000000000, 0.8660254037844387076, 1.000000000000000000, 0.8660254037844387076, 1.000000000000000000, 0.8660254037844387076, 1.000000000000000000, 0.8660254037844387076, 1.000000000000000000, 0.8660254037844387076, 1.000000000000000000, 0.8660254037844387076, 1.000000000000000000, 0.8660254037844387076, 1.000000000000000000, 0.8660254037844387076, 1.000000000000000000, 0.8660254037844387076, 1.000000000000000000, 0.8660254037844387076, 1.000000000000000000, 0.8660254037844387076, 1.000000000000000000, 0.8660254037844387076, 1.000000000000000000, 0.8660254037844387076, 1.000000000000000000, 0.8660254037844387076, 1.000000000000000000, 0.8660254037844387076, 1.000000000000000000, 0.8660254037844387076, 1.000000000000000000, 0.8660254037844387076, 1.000000000000000000, 0.8660254037844387076, 1.000000000000000000, 0.8660254037844387076, 1.000000000000000000, 0.8660254037844387076, 1.000000000000000000, 0.8660254037844387076, 1.000000000000000000, 0.8660254037844387076, 1.000000000000000000, 0.8660254037844387076, 1.000000000000000000, 0.8660254037844387076, 1.000000000000000000, 0.8660254037844387076, 1.000000000000000000, 0.8660254037844387076, 1.000000000000000000, 0.8660254037844387076, 1.000000000000000000, 0.8660254037844387076, 1.000000000000000000, 0.8660254037844387076, 1.000000000000000000, 0.8660254037844387076, 1.000000000000000000, 0.8660254037844387076, 1.000000000000000000, 0.8660254037844387076, 1.000000000000000000, 0.8660254037844387076, 1.000000000000000000, 0.8660254037844387076, 1.000000000000000000, 0.8660254037844387076, 1.000000000000000000, 0.8660254037844387076, 1.000000000000000000, 0.8660254037844387076, 1.000000000000000000, 0.8660254037844387076, 1.000000000000000000, 0.8660254037844387076, 1.000000000000000000, 0.8660254037844387076, 1.000000000000000000, 0.8660254037844387076, 1.000000000000000000, 0.8660254037844387076, 1.000000000000000000, 0.8660254037844387076, 1.000000000000000000, 0.8660254037844387076, 1.000000000000000000, 0.8660254037844387076, 1.000000000000000000, 0.8660254037844387076, 1.000000000000000000, 0.8660254037844387076, 1.000000000000000000, 0.8660254037844387076, 1.000000000000000000, 0.8660254037844387076, 1.000000000000000000, 0.8660254037844387076, 1.000000000000000000, 0.8660254037844387076, 1.000000000000000000, 0.8660254037844387076, 1.000000000000000000, 0.8660254037844387076, 1.000000000000000000, 0.8660254037844387076, 1.000000000000000000, 0.8660254037844387076, 1.000000000000000000, 0.8660254037844387076, 1.000000000000000000, 0.8660254037844387076, 1.000000000000000000, 0.8660254037844387076, 1.000000000000000000, 0.8660254037844387076, 1.000000000000000000, 0.8660254037844387076, 1.000000000000000000, 0.8660254037844387076, 1.000000000000000000, 0.8660254037844387076, 1.000000000000000000, 0.8660254037844387076, 1.000000000000000000, 0.8660254037844387076, 1.000000000000000000, 0.8660254037844387076, 1.000000000000000000, 0.8660254037844387076, 1.000000000000000000, 0.8660254037844387076, 1.000000000000000000, 0.8660254037844387076, 1.000000000000000000, 0.8660254037844387076, 1.000000000000000000, 0.8660254037844387076, 1.000000000000000000, 0.8660254037844387076, 1.000000000000000000, 0.8660254037844387076, 1.000000000000000000, 0.8660254037844387076, 1.000000000000000000, 0.8660254037844387076, 1.000000000000000000, 0.8660254037844387076, 1.000000000000000000, 0.8660254037844387076, 1.000000000000000000, 0.8660254037844387076, 1.000000000000000000, 0.8660254037844387076, 1.000000000000000000, 0.8660254037844387076, 1.000000000000000000, 0.8660254037844387076, 1.000000000000000000, 0.8660254037844387076, 1.000000000000000000, 0.8660254037844387076, 1.000000000000000000, 0.8660254037844387076, 1.000000000000000000, 0.8660254037844387076, 1.000000000000000000, 0.8660254037844387076, 1.000000000000000000, 0.8660254037844387076, 1.000000000000000000, 0.8660254037844387076, 1.000000000000000000, 0.8660254037844387076, 1.000000000000000000, 0.8660254037844387076, 1.000000000000000000) ) ) 
 REPRESENTATION_ITEM ( '' )  SURFACE ( )  );
#198667 = CARTESIAN_POINT ( 'NONE',  ( -5.655686355556086120, 6.627330832017406692, 1.199719254218452935 ) ) ;
#198668 = CARTESIAN_POINT ( 'NONE',  ( 3.889861467948489082, -2.010801299972611478, 0.1531677096566556595 ) ) ;
#198669 = CARTESIAN_POINT ( 'NONE',  ( -7.153898609505128015, 11.49796547773133604, 0.7998128361456481317 ) ) ;
#198671 = FACE_OUTER_BOUND ( 'NONE', #142317, .T. ) ;
#198670 = CARTESIAN_POINT ( 'NONE',  ( -2.103486388414573138, 5.605817886458954291, 1.040834085586084257E-14 ) ) ;
#198672 = APPLICATION_CONTEXT ( 'automotive_design' ) ;
#198673 = CARTESIAN_POINT ( 'NONE',  ( 0.6823417656249917140, 5.092708333674749177, 1.181850606188765695 ) ) ;
#198675 = CARTESIAN_POINT ( 'NONE',  ( -11.95360554405576714, 12.49555003497401451, -1.059413164304690680 ) ) ;
#198674 = CARTESIAN_POINT ( 'NONE',  ( 4.610339536224768331, -0.9213992672730475508, -1.955631277330005968 ) ) ;
#198676 = CARTESIAN_POINT ( 'NONE',  ( 1.274170411194398450E-16, 1.750000000000001554, 1.903066852858540603 ) ) ;
#198677 = CARTESIAN_POINT ( 'NONE',  ( -11.26733562030481473, 6.406227745073034718, -3.999921830493572195 ) ) ;
#198679 = CARTESIAN_POINT ( 'NONE',  ( 5.483999976877721672, -2.016598147233912730, 0.002826481282774962345 ) ) ;
#198678 = CARTESIAN_POINT ( 'NONE',  ( -7.551528372687420720, 8.872833191965849409, 1.082531754730558626 ) ) ;
#198680 = CARTESIAN_POINT ( 'NONE',  ( -0.7500000000000215383, 4.941666666666684193, 1.299038105676671107 ) ) ;
#198681 = CARTESIAN_POINT ( 'NONE',  ( 0.2227383504175127205, -0.09031333296150539924, 1.722639462886750517 ) ) ;
#198682 = CARTESIAN_POINT ( 'NONE',  ( 5.248941747146098180, 6.152795455539095570, -1.199719254218452047 ) ) ;
#198684 = CARTESIAN_POINT ( 'NONE',  ( 5.833751235630055376, 10.02806988486892514, 0.7998128361456331437 ) ) ;
#198683 = CARTESIAN_POINT ( 'NONE',  ( 6.968527767744093993, 10.11340424813470662, 1.082531754730558626 ) ) ;
#198685 = CARTESIAN_POINT ( 'NONE',  ( -10.66331579904126414, 5.901770781639986474, 5.511956274691907076 ) ) ;
#198686 = CARTESIAN_POINT ( 'NONE',  ( 6.450466390465378730, 0.5869013949594548141, 1.776180802621520005 ) ) ;
#198687 = CARTESIAN_POINT ( 'NONE',  ( 0.9088405895168538695, -0.4911093815175514021, -1.952142171939993842 ) ) ;
#198688 = SURFACE_STYLE_USAGE ( .BOTH. , #68683 ) ;
#198689 = CARTESIAN_POINT ( 'NONE',  ( 4.351804119862229037, 4.179452349368450115, -0.7216878364870188411 ) ) ;
#198690 = CARTESIAN_POINT ( 'NONE',  ( -7.715998819508785189, 8.174622508947939181, -0.7216878364870338292 ) ) ;
#198691 = ORIENTED_EDGE ( 'NONE', *, *, #161766, .T. ) ;
#198692 = CARTESIAN_POINT ( 'NONE',  ( 9.531018800282609504, 10.22186947652563305, 0.7216878364870458196 ) ) ;
#198694 = CARTESIAN_POINT ( 'NONE',  ( 1.546500145565052886, -1.423948579484592525, 1.427951870166991322 ) ) ;
#198693 = CARTESIAN_POINT ( 'NONE',  ( 2.438272501909013901, -1.223040458498025673, -1.732039452853536776 ) ) ;
#198695 = CARTESIAN_POINT ( 'NONE',  ( 2.794932832814459811, -0.1373201097526421111, -1.806460840857474937 ) ) ;
#198696 = CARTESIAN_POINT ( 'NONE',  ( 7.862802741282558294, 8.137967717776607657, 0.000000000000000000 ) ) ;
#198697 = CARTESIAN_POINT ( 'NONE',  ( 6.473507614529132148, 2.070149491355821159, -0.6224772505839873959 ) ) ;
#198698 = EDGE_CURVE ( 'NONE', #61933, #13808, #161776, .T. ) ;
#198699 = CARTESIAN_POINT ( 'NONE',  ( 6.693975156845185737, 8.832723654451292816, 1.599625672291281386 ) ) ;
#198701 = CARTESIAN_POINT ( 'NONE',  ( 0.3388992355649001476, -1.619940322034026270, -1.022281207937189684 ) ) ;
#198700 = CARTESIAN_POINT ( 'NONE',  ( -4.717347382551060342, 7.590990148696470818, 1.199719254218464037 ) ) ;
#198702 = DIRECTION ( 'NONE',  ( 0.6507913734559640506, -0.7592566023653003482, 0.000000000000000000 ) ) ;
#198703 = LINE ( 'NONE', #37289, #197580 ) ;
#198704 = CARTESIAN_POINT ( 'NONE',  ( 4.650083499362856365, 8.368921815991249957, 0.7216878364870438212 ) ) ;
#198705 = CARTESIAN_POINT ( 'NONE',  ( -1.402160292154681736E-14, 0.1343750003414218575, 1.575800808251672791 ) ) ;
#198706 = CARTESIAN_POINT ( 'NONE',  ( 4.528060117284244512, 4.385084346360807572, 0.7216878364870317197 ) ) ;
#198707 = CARTESIAN_POINT ( 'NONE',  ( -9.134442807305063639, 11.67993591332117376, 1.599625672291281386 ) ) ;
#198708 = CARTESIAN_POINT ( 'NONE',  ( 3.872077330825273389, 1.198917189070296541, 1.798566189592496034 ) ) ;
#198709 = CARTESIAN_POINT ( 'NONE',  ( -6.617788377246204945, 6.893376992974917350, -0.7216878364870338292 ) ) ;
#198710 = CARTESIAN_POINT ( 'NONE',  ( 4.082413651490639062, 7.776916670132135501, 0.000000000000000000 ) ) ;
#198711 = CARTESIAN_POINT ( 'NONE',  ( 1.600013431492643967, 1.466117565985028515, 1.532352819790145482 ) ) ;
#198712 = CARTESIAN_POINT ( 'NONE',  ( -2.091679895156829610E-15, 2.562499999999987121, 1.224999999999973888 ) ) ;
#198713 = CARTESIAN_POINT ( 'NONE',  ( 3.128153591792836252, 1.098079186366843985, -1.637025598404780791 ) ) ;
#198714 = VERTEX_POINT ( 'NONE', #61398 ) ;
#198715 = CARTESIAN_POINT ( 'NONE',  ( 9.473215147174835593, -6.532648913095251864, -0.3561222683123499433 ) ) ;
#198716 = CARTESIAN_POINT ( 'NONE',  ( 5.863713558449636487, -0.4802757262234845226, 1.909948281557447114 ) ) ;
#198717 = CARTESIAN_POINT ( 'NONE',  ( 2.097507970028670510, -1.941522886764552203, 0.04780177728339052301 ) ) ;
#198718 = ORIENTED_EDGE ( 'NONE', *, *, #74380, .F. ) ;
#198719 = CARTESIAN_POINT ( 'NONE',  ( -4.553559489343377287, 6.405848385690952718, -1.599625672291271394 ) ) ;
#198721 = CARTESIAN_POINT ( 'NONE',  ( 1.849802594915211928, 2.491750049492945429, -2.487615396287162994 ) ) ;
#198720 = CARTESIAN_POINT ( 'NONE',  ( -6.373741612200205076, 8.529394195690610303, 1.443375672974064550 ) ) ;
#198722 = CARTESIAN_POINT ( 'NONE',  ( 6.500244582748090139, 9.671036882259738121, 1.199719254218460707 ) ) ;
#198724 = CARTESIAN_POINT ( 'NONE',  ( 4.367134876933267407, 8.109091433148536865, 0.000000000000000000 ) ) ;
#198723 = CARTESIAN_POINT ( 'NONE',  ( 7.494959990256193194, 7.638541498254023843, -0.7998128361456281477 ) ) ;
#198726 = EDGE_LOOP ( 'NONE', ( #54960, #181075, #201828, #162245, #195305, #112991, #34424 ) ) ;
#198725 = CARTESIAN_POINT ( 'NONE',  ( 6.252599623108594074, 1.892168639490459325, 0.2757424028280440753 ) ) ;
#198727 = CARTESIAN_POINT ( 'NONE',  ( 4.283934280384479543, 1.440456688004333019, 1.672026782002330458 ) ) ;
#198728 = CARTESIAN_POINT ( 'NONE',  ( 2.098912041516465266, -0.5885267676426220174, -2.126790307141281033 ) ) ;
#198729 = LINE ( 'NONE', #152144, #75586 ) ;
#198730 = CARTESIAN_POINT ( 'NONE',  ( 1.049298088506251947, -1.728493729547801117, 0.8183166869351958805 ) ) ;
#198731 = DIRECTION ( 'NONE',  ( 1.000000000000000000, -7.771561172376097755E-16, -4.440892098500627148E-16 ) ) ;
#198732 = CARTESIAN_POINT ( 'NONE',  ( 10.40996301719436090, 11.03937836301526687, 0.000000000000000000 ) ) ;
#198733 = CARTESIAN_POINT ( 'NONE',  ( 4.721179655770254335, -1.847879960204744432, -0.9338546512941485744 ) ) ;
#198734 = CARTESIAN_POINT ( 'NONE',  ( -4.900382456335551140, 7.804531068111707270, 1.199719254218464037 ) ) ;
#198736 = CARTESIAN_POINT ( 'NONE',  ( 1.551884642779034262, 0.6273040060550126862, -2.068667048528524344 ) ) ;
#198735 = CARTESIAN_POINT ( 'NONE',  ( -4.925689880466507908, 4.641059703499347044, -0.7998128361456221525 ) ) ;
#198737 = CARTESIAN_POINT ( 'NONE',  ( 4.247736854543925133, 2.191053489037126045, -0.05455935714590579716 ) ) ;
#198738 = CARTESIAN_POINT ( 'NONE',  ( -5.558434366435592189, 6.905725166219703226, 1.208466946602093639 ) ) ;
#198739 = CARTESIAN_POINT ( 'NONE',  ( 4.936577329151614180, 4.931964103531220722, -0.7216878364870458196 ) ) ;
#198740 = CARTESIAN_POINT ( 'NONE',  ( 4.858757509019057785, 5.629766575900002401, -2.499999999999996891 ) ) ;
#198741 = CARTESIAN_POINT ( 'NONE',  ( -1.364683531250010295, 13.94270833367473195, 0.7879004041258445001 ) ) ;
#198742 = CARTESIAN_POINT ( 'NONE',  ( -4.167152111353897403, 5.955039778036558040, 1.599625672291270506 ) ) ;
#198744 = CARTESIAN_POINT ( 'NONE',  ( 5.607993946907785521, -0.03366334548273764576, 1.734015701317252134 ) ) ;
#198743 = AXIS2_PLACEMENT_3D ( 'NONE', #4537, #118391, #119459 ) ;
#198745 = CARTESIAN_POINT ( 'NONE',  ( -2.117044542028253318, 5.621635732341564662, -0.7998128361456281477 ) ) ;
#198746 = CARTESIAN_POINT ( 'NONE',  ( 3.327070777303439364, -1.911029926764183040, -0.7966718667702379353 ) ) ;
#198747 = CARTESIAN_POINT ( 'NONE',  ( 5.185217826725932788, 1.731529828693706641, 1.218147590116857026 ) ) ;
#198748 = STYLED_ITEM ( 'NONE', ( #49044 ), #186074 ) ;
#198749 = CARTESIAN_POINT ( 'NONE',  ( 6.205881626753210867, 8.263281202677319470, 1.599625672291281386 ) ) ;
#198750 = CARTESIAN_POINT ( 'NONE',  ( 0.6823417656249917140, 4.342708333674755394, 1.181850606188765695 ) ) ;
#198751 = CARTESIAN_POINT ( 'NONE',  ( 3.344544815957225747, -1.939504806627976752, -0.3411970713738179395 ) ) ;
#198752 = CARTESIAN_POINT ( 'NONE',  ( 6.105493113454719456, -2.275700256682281264, 0.2746985183333852110 ) ) ;
#198753 = CARTESIAN_POINT ( 'NONE',  ( 2.437895498511342574, 0.8609710149188253281, -1.609920059450341778 ) ) ;
#198754 = CARTESIAN_POINT ( 'NONE',  ( 5.239300017038202917, 5.077214539491492928, 0.000000000000000000 ) ) ;
#198755 = CARTESIAN_POINT ( 'NONE',  ( 5.138177029454847222, 6.057256624861201644, 1.082531754730560403 ) ) ;
#198756 = CARTESIAN_POINT ( 'NONE',  ( -8.016948904382338981, 8.247528564734524892, -0.7998128361456291469 ) ) ;
#198757 = ORIENTED_EDGE ( 'NONE', *, *, #102136, .F. ) ;
#198758 = ORIENTED_EDGE ( 'NONE', *, *, #173375, .F. ) ;
#198759 = CARTESIAN_POINT ( 'NONE',  ( 4.254156334807709605, 0.8570458487419434501, -1.821774543695050319 ) ) ;
#198760 = CARTESIAN_POINT ( 'NONE',  ( 4.241029431094700541, -0.1880360549168894613, -1.952691919460777026 ) ) ;
#198761 = CARTESIAN_POINT ( 'NONE',  ( -6.320072162264675164, 10.52516795595079557, 0.7998128361456481317 ) ) ;
#198762 = CARTESIAN_POINT ( 'NONE',  ( -3.574546055497324737, 7.322054164722185732, 0.7998128361456341429 ) ) ;
#198763 = CARTESIAN_POINT ( 'NONE',  ( 7.065207446497155708, 9.336104335703744539, 0.000000000000000000 ) ) ;
#198765 = CARTESIAN_POINT ( 'NONE',  ( 5.506658716161647149, 1.338116961444441921, -1.158480101542769036 ) ) ;
#198764 = CARTESIAN_POINT ( 'NONE',  ( 0.1520488688747126949, 0.8040222321012976403, 1.930173718738151578 ) ) ;
#198766 = FACE_OUTER_BOUND ( 'NONE', #205536, .T. ) ;
#198767 = CARTESIAN_POINT ( 'NONE',  ( 1.799034956846547795, 1.823213324544867397, 1.215573211712846158 ) ) ;
#198768 = CARTESIAN_POINT ( 'NONE',  ( 0.5557209801456406417, -1.262220463910254331, 1.198535436172887714 ) ) ;
#198769 = CARTESIAN_POINT ( 'NONE',  ( 4.937140493670735708, 8.911747675924535983, -0.7998128361456281477 ) ) ;
#198770 = CARTESIAN_POINT ( 'NONE',  ( 0.2333690889706925564, 2.018283468528142777, -2.468684669820114586 ) ) ;
#198771 = CARTESIAN_POINT ( 'NONE',  ( 0.8204219880046401681, 1.592052673282555286, 0.6642659308724234712 ) ) ;
#198772 = CARTESIAN_POINT ( 'NONE',  ( 1.230279809073684172, -2.078304686880276808, -0.9817359432500573080 ) ) ;
#198773 = CARTESIAN_POINT ( 'NONE',  ( 0.4686481397476391364, -2.065551408369214137, -0.7328327568804984260 ) ) ;
#198774 = CARTESIAN_POINT ( 'NONE',  ( 6.239525021605913047, -1.647457779603450634, -0.5405594386218066649 ) ) ;
#198775 = CARTESIAN_POINT ( 'NONE',  ( 3.018423772948013006, -1.088090592406821155, -1.919924466345590108 ) ) ;
#198776 = CARTESIAN_POINT ( 'NONE',  ( 1.903425830921786188, -1.835712436893768063, 1.158886079418340875 ) ) ;
#198777 = DIRECTION ( 'NONE',  ( 0.000000000000000000, 8.546850786086437571E-32, 1.000000000000000000 ) ) ;
#198778 = CARTESIAN_POINT ( 'NONE',  ( 1.850927149041701192, -1.938055702826226190, -0.8530577433697658085 ) ) ;
#198779 = CARTESIAN_POINT ( 'NONE',  ( 1.872871967411071648, 3.299999999999997158, 0.3999999999999958589 ) ) ;
#198780 = CARTESIAN_POINT ( 'NONE',  ( 5.631840744973369617, -1.222119163988559354, -1.489112003571291476 ) ) ;
#198781 = ORIENTED_EDGE ( 'NONE', *, *, #155989, .F. ) ;
#198783 = CARTESIAN_POINT ( 'NONE',  ( -1.499999999999997780, 5.650000000000023448, 1.214306433183764966E-14 ) ) ;
#198782 = CARTESIAN_POINT ( 'NONE',  ( 2.929518028021148357, -1.541346711875633435, -1.696969020646617476 ) ) ;
#198784 = CARTESIAN_POINT ( 'NONE',  ( 2.672928840188529609, 6.270167413528593414, 0.000000000000000000 ) ) ;
#198785 = CARTESIAN_POINT ( 'NONE',  ( 4.355193658487811703, 6.104145239700998538, -1.599625672291255185 ) ) ;
#198786 = CARTESIAN_POINT ( 'NONE',  ( 4.864059028628820336, 0.6975124644323873468, -2.109029365712757897 ) ) ;
#198787 = CARTESIAN_POINT ( 'NONE',  ( -8.053180056837398126, 8.497724275839514618, 0.7216878364870578100 ) ) ;
#198788 = FACE_OUTER_BOUND ( 'NONE', #13189, .T. ) ;
#198789 = CARTESIAN_POINT ( 'NONE',  ( 5.016153647376196290, 8.796003655340152605, 0.7216878364870438212 ) ) ;
#198790 = CARTESIAN_POINT ( 'NONE',  ( -7.768458830506062007, 11.04665715469030296, 1.082531754730549967 ) ) ;
#198791 = CARTESIAN_POINT ( 'NONE',  ( 4.855228407469603269, 7.718164671139588151, -1.082531754730548412 ) ) ;
#198792 = STYLED_ITEM ( 'NONE', ( #115824 ), #86509 ) ;
#198793 = VERTEX_POINT ( 'NONE', #146942 ) ;
#198794 = CARTESIAN_POINT ( 'NONE',  ( 3.059220373557011818, -1.198860207862334049, 1.621182619130703051 ) ) ;
#198796 = CARTESIAN_POINT ( 'NONE',  ( 1.041928790383022774, 1.382269897723470642, 1.531051681482889393 ) ) ;
#198795 = CARTESIAN_POINT ( 'NONE',  ( 7.610204295972345712, 7.772993188256215547, 0.7998128361456341429 ) ) ;
#198797 = SURFACE_STYLE_FILL_AREA ( #85068 ) ;
#198798 = EDGE_CURVE ( 'NONE', #210726, #193462, #71651, .T. ) ;
#198799 = CARTESIAN_POINT ( 'NONE',  ( 6.834718834620487016, 7.146462526578263308, 0.000000000000000000 ) ) ;
#198800 = DIRECTION ( 'NONE',  ( 0.000000000000000000, 1.000000000000000000, 0.000000000000000000 ) ) ;
#198801 = CARTESIAN_POINT ( 'NONE',  ( 0.6823417656249899377, 3.176041667008085323, -1.181850606188754593 ) ) ;
#198802 = CARTESIAN_POINT ( 'NONE',  ( 3.908297495596550597, 1.550167135825938569, -1.549264980215167231 ) ) ;
#198803 = CARTESIAN_POINT ( 'NONE',  ( 0.9498425221252141393, -1.824119990893595888, -0.8596288560165299408 ) ) ;
#198804 = CARTESIAN_POINT ( 'NONE',  ( 0.6437974683802077935, 0.5340323341261629109, 1.762076181610471526 ) ) ;
#198805 = CARTESIAN_POINT ( 'NONE',  ( 4.898102649693969468, -0.7706710736265044437, -2.159050251936722731 ) ) ;
#198806 = CARTESIAN_POINT ( 'NONE',  ( 4.382634408885896171, 1.643497958660003144, -0.8300281608688080404 ) ) ;
#198807 = AXIS2_PLACEMENT_3D ( 'NONE', #68215, #187315, #117055 ) ;
#198808 = CARTESIAN_POINT ( 'NONE',  ( 7.579171565239241737, 8.801120566655981747, 1.199719254218462483 ) ) ;
#198809 =( LENGTH_UNIT ( ) NAMED_UNIT ( * ) SI_UNIT ( .MILLI., .METRE. ) );
#198810 = CARTESIAN_POINT ( 'NONE',  ( 5.473610661177239933, 1.758888005172161373, -0.4887267171112125164 ) ) ;
#198811 = CARTESIAN_POINT ( 'NONE',  ( 4.729138786257041538, 2.011204126674607462, 0.1455352507326590494 ) ) ;
#198812 = CARTESIAN_POINT ( 'NONE',  ( -8.853638004923878313, 10.28799807962136548, 1.199719254218462483 ) ) ;
#198814 = CARTESIAN_POINT ( 'NONE',  ( -6.740338644649361832, 7.892758502626242567, -1.199719254218452047 ) ) ;
#198813 = CARTESIAN_POINT ( 'NONE',  ( 4.065478255348141445, 0.2803405965145295275, -2.245028738816820635 ) ) ;
#198815 = CARTESIAN_POINT ( 'NONE',  ( 6.528360061338796427, 1.215782546000489850, -1.719372923949607390 ) ) ;
#198816 = FILL_AREA_STYLE ('',( #66665 ) ) ;
#198817 = CARTESIAN_POINT ( 'NONE',  ( 5.020015195830264787, 2.048331326439792210, -0.3003445753073652469 ) ) ;
#198818 = CARTESIAN_POINT ( 'NONE',  ( 9.576136569953906275, 10.06658084123472641, 0.000000000000000000 ) ) ;
#198819 =( NAMED_UNIT ( * ) SI_UNIT ( $, .STERADIAN. ) SOLID_ANGLE_UNIT ( ) );
#198820 = PRODUCT_CONTEXT ( 'NONE', #168032, 'mechanical' ) ;
#198823 = ADVANCED_FACE ( 'NONE', ( #130736 ), #17418, .T. ) ;
#198822 = CARTESIAN_POINT ( 'NONE',  ( 1.928227594698066039, 1.109388971949121228, -1.574834034052971399 ) ) ;
#198821 = CARTESIAN_POINT ( 'NONE',  ( -9.352427035328430449, 9.805586384171650849, 1.040834085586084257E-14 ) ) ;
#198824 = CARTESIAN_POINT ( 'NONE',  ( 4.197870329852982252, 3.573279226090494198, -2.499999999999994671 ) ) ;
#198825 = CARTESIAN_POINT ( 'NONE',  ( 3.973948422136968084, 5.729635473950147606, -1.443375672974068769 ) ) ;
#198826 = CARTESIAN_POINT ( 'NONE',  ( 5.762717851902044330, 6.056246448182416309, -0.5943541797442238872 ) ) ;
#198827 = CARTESIAN_POINT ( 'NONE',  ( -2.981903720001798597, 5.566305875722335372, -1.199719254218446718 ) ) ;
#198829 = CARTESIAN_POINT ( 'NONE',  ( 1.336510806674645391, -1.239524924825789132, -1.843257696707498061 ) ) ;
#198828 = CARTESIAN_POINT ( 'NONE',  ( 0.6859744409541921328, 2.042103856186634925, -0.5713114342573709648 ) ) ;
#198830 = CARTESIAN_POINT ( 'NONE',  ( 3.276497419027382563, -1.255868110884267530, 1.690353172608966448 ) ) ;
#198831 = CARTESIAN_POINT ( 'NONE',  ( -5.803772275101700906, 8.928762199997411386, -1.199719254218452047 ) ) ;
#198832 = CARTESIAN_POINT ( 'NONE',  ( 8.098297826064319693, 8.342435640030188893, 0.7998128361456481317 ) ) ;
#198833 = CARTESIAN_POINT ( 'NONE',  ( 2.752341281506097470, -1.956419249932477955, -0.1471676765215298721 ) ) ;
#198834 = CARTESIAN_POINT ( 'NONE',  ( 4.123651276850781144, 7.962676922967908411, -0.7998128361456221525 ) ) ;
#198835 = CARTESIAN_POINT ( 'NONE',  ( -4.208837953572873047, 7.367755930811632936, 0.8315943877991900379 ) ) ;
#198836 = CARTESIAN_POINT ( 'NONE',  ( 4.416205349749311004, 6.175325546172740765, 1.599625672291267398 ) ) ;
#198837 = CARTESIAN_POINT ( 'NONE',  ( -5.478903473698247595, 8.445785581739666981, -1.082531754730549967 ) ) ;
#198838 = CARTESIAN_POINT ( 'NONE',  ( -6.724481002698120768, 9.828683022247721723, -1.082531754730538864 ) ) ;
#198839 = CARTESIAN_POINT ( 'NONE',  ( 2.724977724663907530, 1.532976055022855499, -1.465462182430438798 ) ) ;
#198840 = CARTESIAN_POINT ( 'NONE',  ( -6.123442655227560927, 7.173046514967467147, 1.199719254218452047 ) ) ;
#198841 = CARTESIAN_POINT ( 'NONE',  ( 4.475024536774164119, 1.792854848340214025, 0.7970393728587571447 ) ) ;
#198842 = CARTESIAN_POINT ( 'NONE',  ( 3.590839768554392908, -0.4196827604958653923, -2.120402733634827452 ) ) ;
#198843 = CARTESIAN_POINT ( 'NONE',  ( 3.192734241421916419, 1.453351889590439816, 1.130385295574042104 ) ) ;
#198844 = CARTESIAN_POINT ( 'NONE',  ( -4.124159483505494883, 7.474427186445510962, 0.6511861734826256409 ) ) ;
#198845 = CARTESIAN_POINT ( 'NONE',  ( -0.04151047742771058618, -7.963884727586691525, -9.500000000000145661 ) ) ;
#198846 = CARTESIAN_POINT ( 'NONE',  ( 4.294662974013852441, 1.399676235010495873, 1.034011069942197159 ) ) ;
#198847 = CARTESIAN_POINT ( 'NONE',  ( -8.065673753976707161, 15.99999996918363010, -8.613976771941846522 ) ) ;
#198848 = CARTESIAN_POINT ( 'NONE',  ( 5.178851490740207453, 5.144340948726102702, 0.7216878364870317197 ) ) ;
#198849 = CARTESIAN_POINT ( 'NONE',  ( -10.57232898948313604, 5.599354254162436817, 4.968808419985093039 ) ) ;
#198850 = CARTESIAN_POINT ( 'NONE',  ( 1.710078970767275885, -2.145365142986368934, 0.2646356489638818088 ) ) ;
#198851 = CARTESIAN_POINT ( 'NONE',  ( 3.972029700707707445, 1.727737986437705819, 1.038833660170018769 ) ) ;
#198852 = CARTESIAN_POINT ( 'NONE',  ( -2.788906526875773208E-15, 12.96875000068279782, -1.499999999999998446 ) ) ;
#198853 = CARTESIAN_POINT ( 'NONE',  ( 1.604591590977550108, -0.7782141685120853580, -2.016947388195994062 ) ) ;
#198854 = EDGE_CURVE ( 'NONE', #190376, #121012, #48467, .T. ) ;
#198855 = CARTESIAN_POINT ( 'NONE',  ( 3.291827724629258434, -0.8003651471039547882, 1.801871540228771273 ) ) ;
#198856 = CARTESIAN_POINT ( 'NONE',  ( 4.161989969715248705, 4.726297878971393196, -2.420000000000000373 ) ) ;
#198857 = CARTESIAN_POINT ( 'NONE',  ( 3.351055748958339908, 0.4689680007726776401, -1.884483806560928398 ) ) ;
#198860 = VERTEX_POINT ( 'NONE', #166459 ) ;
#198859 = CARTESIAN_POINT ( 'NONE',  ( 1.284279953904119864, 2.827889714876734129, -0.7749999999999910294 ) ) ;
#198858 = CARTESIAN_POINT ( 'NONE',  ( -9.829298179783291900, 11.53023130024440768, 1.082531754730558626 ) ) ;
#198861 = CARTESIAN_POINT ( 'NONE',  ( -5.582925393777276035, 9.735439736040634173, 0.7998128361456291469 ) ) ;
#198862 = CARTESIAN_POINT ( 'NONE',  ( 3.386504508363381571, 7.172948703057747011, -0.7998128361456362523 ) ) ;
#198863 = CARTESIAN_POINT ( 'NONE',  ( -6.143779885648060102, 7.196773283791382703, 1.199719254218452047 ) ) ;
#198864 = CARTESIAN_POINT ( 'NONE',  ( -10.29027540264791440, 11.10766884595181203, 0.7216878364870438212 ) ) ;
#198865 = CARTESIAN_POINT ( 'NONE',  ( 0.6752036787147744912, -2.078553970830565145, -0.7415856106591719454 ) ) ;
#198866 = CARTESIAN_POINT ( 'NONE',  ( 1.642778471875001811, -2.792708332855376785, 2.845375778867859751 ) ) ;
#198867 = CARTESIAN_POINT ( 'NONE',  ( 5.805508902378371694, -1.544246397408255866, -1.209716981170713357 ) ) ;
#198868 = CARTESIAN_POINT ( 'NONE',  ( 2.443982611291168006, -1.755769474653746665, -0.9913988478210812305 ) ) ;
#198869 = VERTEX_POINT ( 'NONE', #114582 ) ;
#198870 = CARTESIAN_POINT ( 'NONE',  ( 3.028621024253768113, 0.5188578782318100657, 2.052648472271414448 ) ) ;
#198871 = CARTESIAN_POINT ( 'NONE',  ( 1.499999999999989120, 2.306250000682817713, 1.214306433183764966E-14 ) ) ;
#198873 = CARTESIAN_POINT ( 'NONE',  ( -5.032047568966410367, 9.022472597102808578, 1.214306433183764966E-14 ) ) ;
#198872 = CARTESIAN_POINT ( 'NONE',  ( 9.500385102287568273, -7.162053774861992572, -0.01083140255524945791 ) ) ;
#198874 = CARTESIAN_POINT ( 'NONE',  ( 4.048646477676579813, -1.531818510360350327, -1.021117339664041834 ) ) ;
#198875 = EDGE_LOOP ( 'NONE', ( #7753, #171569, #181779, #33297 ) ) ;
#198876 = CARTESIAN_POINT ( 'NONE',  ( -7.971304249830880373, 11.38727316052296601, 1.199719254218453823 ) ) ;
#198877 = CARTESIAN_POINT ( 'NONE',  ( 5.607717026683647354, 1.607092460389969446, 1.383685132418293495 ) ) ;
#198878 = CARTESIAN_POINT ( 'NONE',  ( 1.772826578343093873, 3.949999999999995293, 0.3999999999999819811 ) ) ;
#198879 = CARTESIAN_POINT ( 'NONE',  ( 6.498435699651741615, 6.475929825882159818, -0.7998128361456281477 ) ) ;
#198880 = VERTEX_POINT ( 'NONE', #173960 ) ;
#198881 = CARTESIAN_POINT ( 'NONE',  ( 5.290332094886032621, -2.044729594613464041, -0.2563108835951214970 ) ) ;
#198884 = CARTESIAN_POINT ( 'NONE',  ( 2.841158510722852970, 0.6603703904487292498, -1.718939526767604420 ) ) ;
#198883 = CARTESIAN_POINT ( 'NONE',  ( 0.4318009167844725771, 1.066696818439222039, 1.524822319796947934 ) ) ;
#198882 = DIRECTION ( 'NONE',  ( 0.7592566023653016805, -0.6507913734559627184, 0.000000000000000000 ) ) ;
#198885 = CARTESIAN_POINT ( 'NONE',  ( 8.178592977541601527, 10.56477777859713463, 1.599625672291281386 ) ) ;
#198886 = CARTESIAN_POINT ( 'NONE',  ( 1.124100812432970948E-16, 3.500000000000003109, -2.025000000000006573 ) ) ;
#198887 = CARTESIAN_POINT ( 'NONE',  ( -8.106849506328558164, 8.422688943663599659, 0.000000000000000000 ) ) ;
#198888 = DIRECTION ( 'NONE',  ( -1.000000000000000000, -3.451266460341927087E-31, 0.000000000000000000 ) ) ;
#198889 = CARTESIAN_POINT ( 'NONE',  ( 2.578998426009218470, -2.112161100990978202, -0.6396139477699357423 ) ) ;
#198890 = CARTESIAN_POINT ( 'NONE',  ( 5.044316441076016844, 2.255832582719615065, 0.1735265121041371095 ) ) ;
#198891 = CARTESIAN_POINT ( 'NONE',  ( -7.375272376154093479, 9.627570410311676596, -1.443375672974059665 ) ) ;
#198892 = CARTESIAN_POINT ( 'NONE',  ( 4.693523411346745000, 1.687728755266065139, -0.6588045490927648684 ) ) ;
#198893 = CARTESIAN_POINT ( 'NONE',  ( 5.489432593909100433, -0.4588279098093718256, 1.859853701273159743 ) ) ;
#198894 = CARTESIAN_POINT ( 'NONE',  ( 1.364683531249992088, 5.446875000341417916, 1.214306433183764966E-14 ) ) ;
#198895 = CARTESIAN_POINT ( 'NONE',  ( 5.453920962983416665, 1.868457504587007545, -0.09292587778651077712 ) ) ;
#198896 = CARTESIAN_POINT ( 'NONE',  ( 4.826513810146395578, -1.216237885654298800, 1.408704720340781869 ) ) ;
#198897 = FACE_OUTER_BOUND ( 'NONE', #62900, .T. ) ;
#198898 = AXIS2_PLACEMENT_3D ( 'NONE', #205703, #174311, #57338 ) ;
#198899 = CARTESIAN_POINT ( 'NONE',  ( 6.332837517263664395, 0.1779433324526000226, 1.760853854254845530 ) ) ;
#198900 = CARTESIAN_POINT ( 'NONE',  ( -0.2058462039469660110, -0.8663896114125648751, -1.819200108291472606 ) ) ;
#198902 = CARTESIAN_POINT ( 'NONE',  ( 2.315183273126443009, 1.881732686034083724, 0.9459776246590365645 ) ) ;
#198901 = CARTESIAN_POINT ( 'NONE',  ( -3.673896439178936824, 5.309298483840612093, 1.443375672974064550 ) ) ;
#198903 = STYLED_ITEM ( 'NONE', ( #74626 ), #189681 ) ;
#198904 = CARTESIAN_POINT ( 'NONE',  ( 9.856941372335116469, 11.45851867493453291, 1.199719254218450271 ) ) ;
#198906 = CARTESIAN_POINT ( 'NONE',  ( -10.49131193887636826, 11.13428543831092909, 1.040834085586084257E-14 ) ) ;
#198905 = CARTESIAN_POINT ( 'NONE',  ( 1.499999999999822586, 7.240846818246208905, 4.154462424328221104 ) ) ;
#198907 = DIRECTION ( 'NONE',  ( 0.000000000000000000, 1.000000000000000000, 0.000000000000000000 ) ) ;
#198908 = CARTESIAN_POINT ( 'NONE',  ( 1.424088383587719386, -2.004042310577313302, 0.2513328237187910652 ) ) ;
#198909 = CARTESIAN_POINT ( 'NONE',  ( 0.6823417656249882723, 2.176041667008084435, -1.181850606188749264 ) ) ;
#198910 = CARTESIAN_POINT ( 'NONE',  ( 6.720655732516650716, 2.993363686233801779, 2.180545405541700177 ) ) ;
#198911 = CARTESIAN_POINT ( 'NONE',  ( 4.334856428067313416, 6.080418470877079429, -1.599625672291256295 ) ) ;
#198912 = ORIENTED_EDGE ( 'NONE', *, *, #61190, .F. ) ;
#198913 = CARTESIAN_POINT ( 'NONE',  ( 2.583474834239877449, 1.977432880963815309, -0.8734481387390122809 ) ) ;
#198914 = CARTESIAN_POINT ( 'NONE',  ( 6.890000000000029878, 7.629137130509094256, 2.600000000000001421 ) ) ;
#198917 = CARTESIAN_POINT ( 'NONE',  ( 3.667411383892732246, 3.520940564220482738, -2.447588313016641148 ) ) ;
#198916 = CARTESIAN_POINT ( 'NONE',  ( 0.4019237886466816012, 13.20758545099816672, -1.499999999999998668 ) ) ;
#198915 = CARTESIAN_POINT ( 'NONE',  ( 4.492547798081839794, 6.334668079219206049, 1.599625672291262513 ) ) ;
#198918 = CARTESIAN_POINT ( 'NONE',  ( 9.693716643646595799, 11.37205284141829686, 1.082531754730548412 ) ) ;
#198919 = CARTESIAN_POINT ( 'NONE',  ( 6.503150282362620160, -0.1410805869419759218, 1.984311032119711715 ) ) ;
#198920 = CARTESIAN_POINT ( 'NONE',  ( -6.399085315970137522, 9.449054721065074602, -1.082531754730538864 ) ) ;
#198921 = CARTESIAN_POINT ( 'NONE',  ( 0.7674258922165803076, 2.110627382301712540, -0.5898035449652739848 ) ) ;
#198922 = CARTESIAN_POINT ( 'NONE',  ( 0.5610452518370867558, 7.732119650022924340, 1.919700688223595408 ) ) ;
#198923 = CARTESIAN_POINT ( 'NONE',  ( 1.780510834742056847, -1.209543565243664798, 1.911899112700167880 ) ) ;
#198924 = CARTESIAN_POINT ( 'NONE',  ( -6.333630315878337136, 10.54098580183340772, 0.000000000000000000 ) ) ;
#198925 = CARTESIAN_POINT ( 'NONE',  ( -5.721177634842498527, 5.777054783512106440, 0.000000000000000000 ) ) ;
#198926 = CARTESIAN_POINT ( 'NONE',  ( -1.364683531250012516, 3.801041667008087099, -0.7879004041258300672 ) ) ;
#198927 = CARTESIAN_POINT ( 'NONE',  ( 4.851297196472967421, 8.072458764906237150, -0.9094135686919021522 ) ) ;
#198928 = CARTESIAN_POINT ( 'NONE',  ( -1.402160292154681736E-14, 10.81250000000000355, 1.732050807568881190 ) ) ;
#198929 = CARTESIAN_POINT ( 'NONE',  ( 5.401997860402196316, 5.267028690082820930, 0.000000000000000000 ) ) ;
#198930 = CARTESIAN_POINT ( 'NONE',  ( 2.776313302798124383, -1.692206278411222176, -0.5179841425143881795 ) ) ;
#198931 = CARTESIAN_POINT ( 'NONE',  ( 9.317477881089539338, 11.89347683273640932, 1.599625672291279388 ) ) ;
#198933 = AXIS2_PLACEMENT_3D ( 'NONE', #125829, #9851, #73789 ) ;
#198932 = CARTESIAN_POINT ( 'NONE',  ( 6.774453055690137226, -1.363307072557031985, 1.735998097611628932 ) ) ;
#198934 = CARTESIAN_POINT ( 'NONE',  ( 1.364683531250000303, 14.81770833367472839, -0.7879004041258355073 ) ) ;
#198935 = ORIENTED_EDGE ( 'NONE', *, *, #186335, .F. ) ;
#198936 = CARTESIAN_POINT ( 'NONE',  ( -5.074494633264801990, 9.142270515442742607, 0.7998128361456291469 ) ) ;
#198937 = CARTESIAN_POINT ( 'NONE',  ( 4.939077454563308933, -1.704950310733845065, -1.076300583479961048 ) ) ;
#198938 = ORIENTED_EDGE ( 'NONE', *, *, #16357, .F. ) ;
#198939 = EDGE_CURVE ( 'NONE', #153475, #5754, #16288, .T. ) ;
#198940 = CARTESIAN_POINT ( 'NONE',  ( 2.447944060942487621, 1.870205405844455049, 0.04815357881200743595 ) ) ;
#198941 = CARTESIAN_POINT ( 'NONE',  ( 2.131770371054972912, 1.982354287819853456, -0.5969549857752221023 ) ) ;
#198942 = CARTESIAN_POINT ( 'NONE',  ( -7.119440060507479018, 8.439006504414422238, 1.082531754730549078 ) ) ;
#198943 = CARTESIAN_POINT ( 'NONE',  ( 2.162237915172473546, 1.912057200688283665, 0.04323261116381121871 ) ) ;
#198944 = CARTESIAN_POINT ( 'NONE',  ( 8.499999999999980460, 6.280000000000042881, 2.873333333333345951 ) ) ;
#198945 = CARTESIAN_POINT ( 'NONE',  ( -9.917242840447775265, 4.174869238508773783, -6.172972641688763140 ) ) ;
#198946 = CARTESIAN_POINT ( 'NONE',  ( 0.4368516432692164941, -5.631911363926717762, 10.55905904256947636 ) ) ;
#198947 = CARTESIAN_POINT ( 'NONE',  ( 1.364683531249988535, 3.926041667008087543, 0.7879004041258500513 ) ) ;
#198948 = CARTESIAN_POINT ( 'NONE',  ( -0.03509584499547176162, -1.534781374734139670, 1.140672443274578729 ) ) ;
#198949 = EDGE_CURVE ( 'NONE', #69052, #162364, #4983, .T. ) ;
#198950 = CARTESIAN_POINT ( 'NONE',  ( 5.072158865288233898, 7.971250205261355859, 1.082531754730549078 ) ) ;
#198951 = CARTESIAN_POINT ( 'NONE',  ( 2.664445928352857429, -0.7481792696971515388, -1.813797970468238985 ) ) ;
#198952 = CARTESIAN_POINT ( 'NONE',  ( 1.651451222920913953, -0.8386022738108372954, 1.021479198850117287 ) ) ;
#198953 = CARTESIAN_POINT ( 'NONE',  ( -5.659602779061863487, 5.567567761852417085, 0.7998128361456281477 ) ) ;
#198954 = CARTESIAN_POINT ( 'NONE',  ( 5.801066647469003357, -0.3129311994157328303, -2.097281602037828208 ) ) ;
#198955 = CARTESIAN_POINT ( 'NONE',  ( 9.694243528971124846, 11.26870452434320491, 1.199719254218450271 ) ) ;
#198956 = CARTESIAN_POINT ( 'NONE',  ( 6.925078400183515726, -0.002206826874838820583, 1.955452213090567160 ) ) ;
#198957 = CARTESIAN_POINT ( 'NONE',  ( -1.201851678989727383E-14, 3.071875000341420137, 1.575800808251672791 ) ) ;
#198958 = CARTESIAN_POINT ( 'NONE',  ( 1.933841784273998332, -1.951746473714164321, 0.4931059669559466063 ) ) ;
#198960 = CARTESIAN_POINT ( 'NONE',  ( 0.5623061109219238407, -1.172325791230070857, 1.762859051686527012 ) ) ;
#198959 = CARTESIAN_POINT ( 'NONE',  ( -8.039621903223732602, 8.481906429956900695, 1.040834085586084257E-14 ) ) ;
#198961 = CARTESIAN_POINT ( 'NONE',  ( 9.967295635675853305, 9.878600899727834062, 6.621762730473949254 ) ) ;
#198962 = CARTESIAN_POINT ( 'NONE',  ( 2.189971326302230903, -1.350648006375281929, -1.569233719104834890 ) ) ;
#198963 = CARTESIAN_POINT ( 'NONE',  ( 4.740510986633625024, 5.559626234941203116, -1.199719254218450271 ) ) ;
#198964 = CARTESIAN_POINT ( 'NONE',  ( 3.413620815590684199, 7.204584394822967752, 0.7998128361456281477 ) ) ;
#198965 = ORIENTED_EDGE ( 'NONE', *, *, #134782, .F. ) ;
#198967 = CARTESIAN_POINT ( 'NONE',  ( 3.181359600701000989, 6.863336634126477875, 0.000000000000000000 ) ) ;
#198966 = CARTESIAN_POINT ( 'NONE',  ( 6.017543284830850325, -1.160447301756668104, -1.738784508216392855 ) ) ;
#198970 = ORIENTED_EDGE ( 'NONE', *, *, #6610, .F. ) ;
#198969 = CARTESIAN_POINT ( 'NONE',  ( 3.088311256162243446, -1.077087438943722164, 1.456314016777765286 ) ) ;
#198968 = CARTESIAN_POINT ( 'NONE',  ( 4.225493254642153751, -1.746956894163293361, 0.5300125199643389573 ) ) ;
#198971 = CARTESIAN_POINT ( 'NONE',  ( 7.716561984472250835, 12.15440608185967086, 1.040834085586084257E-14 ) ) ;
#198972 = CARTESIAN_POINT ( 'NONE',  ( 10.28861420900376089, 12.75941440320506004, 6.944769193408874663 ) ) ;
#198973 = CARTESIAN_POINT ( 'NONE',  ( 4.964015014492747291, 2.183396446337606989, -0.3195234977587738667 ) ) ;
#198974 = CARTESIAN_POINT ( 'NONE',  ( -1.364683531250000748, 10.42187500034139802, 0.000000000000000000 ) ) ;
#198975 = EDGE_LOOP ( 'NONE', ( #14234, #135417, #27042, #59794 ) ) ;
#198976 = CARTESIAN_POINT ( 'NONE',  ( 4.266199323752727146, 1.911794059647478949, -0.05023246155653331158 ) ) ;
#198977 = CARTESIAN_POINT ( 'NONE',  ( -3.216308754939891212, 4.775446185561722956, -1.599625672291262513 ) ) ;
#198978 = CARTESIAN_POINT ( 'NONE',  ( 6.500244582748090139, 9.671036882259738121, 1.199719254218460707 ) ) ;
#198979 = CARTESIAN_POINT ( 'NONE',  ( -0.6801582343750229853, 1.380208333674720622, -1.178068619123855409 ) ) ;
#198980 = CARTESIAN_POINT ( 'NONE',  ( 4.650083499362875017, 5.487814173087225633, 1.082531754730560403 ) ) ;
#198981 = EDGE_CURVE ( 'NONE', #179933, #111607, #14962, .T. ) ;
#198982 = CARTESIAN_POINT ( 'NONE',  ( 3.853720295264306372, 8.531188044730880549, -2.447541241191877770 ) ) ;
#198983 = CARTESIAN_POINT ( 'NONE',  ( 7.971049111166076173, 14.32663455170581379, -8.970823572502334642 ) ) ;
#198984 = CARTESIAN_POINT ( 'NONE',  ( 0.6789530235665336422, 1.236279375446739603, 1.364625092910062953 ) ) ;
#198985 = CARTESIAN_POINT ( 'NONE',  ( -6.042630808230841359E-15, -2.012500000000000178, 3.474999999999999645 ) ) ;
#198986 = CARTESIAN_POINT ( 'NONE',  ( 4.551927186349598031, 1.870183863439809357, -0.04390777100237578529 ) ) ;
#198987 = CARTESIAN_POINT ( 'NONE',  ( 11.78331023100045627, 11.29999999999999893, -1.800000000000001155 ) ) ;
#198988 = CARTESIAN_POINT ( 'NONE',  ( 0.01853509810217068496, 14.54321759157664395, 11.97163369463103599 ) ) ;
#198989 = CARTESIAN_POINT ( 'NONE',  ( -7.375272376154096143, 8.667201196010339004, -1.082531754730544860 ) ) ;
#198990 = CARTESIAN_POINT ( 'NONE',  ( 3.825371897350130723, 7.614684313550482031, 0.7998128361456321445 ) ) ;
#198991 = CARTESIAN_POINT ( 'NONE',  ( 1.410928143256191092, -1.555772830594209788, 1.207522851012821308 ) ) ;
#198992 = EDGE_CURVE ( 'NONE', #40394, #143545, #37033, .T. ) ;
#198993 = CARTESIAN_POINT ( 'NONE',  ( 1.985954055300429566, -2.015913623055834325, 0.05231662700833779323 ) ) ;
#198994 = CARTESIAN_POINT ( 'NONE',  ( -8.507905087775398556, 9.884643009614800135, 1.199719254218462483 ) ) ;
#198995 = CARTESIAN_POINT ( 'NONE',  ( 6.638652492546827766, 7.774124658506663010, 1.199719254218452047 ) ) ;
#198996 = CARTESIAN_POINT ( 'NONE',  ( -0.4626273691814692390, 3.108307088186299527, 0.4053073865229923078 ) ) ;
#198997 = CARTESIAN_POINT ( 'NONE',  ( 2.923975034273151419, 1.216836049711809586, -1.822369523680394066 ) ) ;
#198998 = CARTESIAN_POINT ( 'NONE',  ( 6.586557105272873969, -1.791547847876047594, -0.3505316570680468979 ) ) ;
#198999 = CARTESIAN_POINT ( 'NONE',  ( -3.867100128395853709, 5.534702787927018974, -1.599625672291256295 ) ) ;
#199000 = LINE ( 'NONE', #169464, #86450 ) ;
#199002 = DIRECTION ( 'NONE',  ( 1.000000000000000000, -0.000000000000000000, -0.000000000000000000 ) ) ;
#199001 = PRODUCT ( 'rubber 510 pin', 'rubber 510 pin', '', ( #67735 ) ) ;
#199003 = CARTESIAN_POINT ( 'NONE',  ( 5.736508392357904107, 5.865217010605237924, 0.000000000000000000 ) ) ;
#199004 = CARTESIAN_POINT ( 'NONE',  ( 9.260382613333817403, 10.76253345609967660, -1.199719254218446718 ) ) ;
#199005 = CARTESIAN_POINT ( 'NONE',  ( 3.785751206713845018, 5.439795712631356750, 1.599625672291267398 ) ) ;
#199006 = CARTESIAN_POINT ( 'NONE',  ( 5.234856708652215751, 9.121433570154021453, 0.7216878364870317197 ) ) ;
#199007 = ORIENTED_EDGE ( 'NONE', *, *, #67389, .F. ) ;
#199009 = CARTESIAN_POINT ( 'NONE',  ( 0.9615884438243198495, -1.588399402277500760, -1.236662224066273019 ) ) ;
#199008 = CARTESIAN_POINT ( 'NONE',  ( 3.684953445348177148, 1.336164438771630714, 1.267087564277062484 ) ) ;
#199010 = CARTESIAN_POINT ( 'NONE',  ( 2.706789001878449508, -1.702045039646230107, -1.544681222897727357 ) ) ;
#199012 = CARTESIAN_POINT ( 'NONE',  ( 0.8306204695724854759, -1.749664030167530138, -0.6342216345150762935 ) ) ;
#199011 = CARTESIAN_POINT ( 'NONE',  ( 6.539320575229281118, 7.629137130509070275, 2.703262396134015866 ) ) ;
#199013 = CARTESIAN_POINT ( 'NONE',  ( 3.475000000000000533, -0.2041666666666657748, 2.006292185433948827 ) ) ;
#199014 = CARTESIAN_POINT ( 'NONE',  ( -4.613852347352193739, 4.277249248199312071, 1.214306433183764966E-14 ) ) ;
#199015 = CARTESIAN_POINT ( 'NONE',  ( 4.781465250580236415, 0.1816826923375300662, -1.903719681147630016 ) ) ;
#199016 = CARTESIAN_POINT ( 'NONE',  ( -8.188234707649510113, 11.64035869464474082, -1.199719254218446718 ) ) ;
#199017 = CARTESIAN_POINT ( 'NONE',  ( -6.509323148336870091, 7.727203440215372865, 1.082531754730549078 ) ) ;
#199019 = CARTESIAN_POINT ( 'NONE',  ( 2.149089010626914931, -1.500894351328721621, -1.116326037436713881 ) ) ;
#199018 = CARTESIAN_POINT ( 'NONE',  ( 3.860945534362031140, 0.2537485593089708336, -2.075202752206976697 ) ) ;
#199020 = CARTESIAN_POINT ( 'NONE',  ( 5.978782553946477840, 9.919070713005490703, 1.040834085586084257E-14 ) ) ;
#199021 = CARTESIAN_POINT ( 'NONE',  ( -1.364683531250010740, 4.842708333674756283, 0.7879004041258379498 ) ) ;
#199022 = CARTESIAN_POINT ( 'NONE',  ( 6.356982874815331641, 0.3076174260261410054, -1.815216213958574132 ) ) ;
#199023 = CARTESIAN_POINT ( 'NONE',  ( 4.546061579283848353, 4.198160018786257552, -0.7998128361456211532 ) ) ;
#199024 = CARTESIAN_POINT ( 'NONE',  ( 4.260029445439558415, 7.236136616047151193, -2.420000000000000373 ) ) ;
#199025 = CARTESIAN_POINT ( 'NONE',  ( 3.756244407761480275, 0.6229016427463770489, 1.608663766957881824 ) ) ;
#199026 = CARTESIAN_POINT ( 'NONE',  ( -5.852315862593199469, 9.979452273000736895, 0.7998128361456481317 ) ) ;
#199027 = CARTESIAN_POINT ( 'NONE',  ( 6.586557750117827403, -2.163372447211810989, -0.4352210726449382006 ) ) ;
#199028 = CARTESIAN_POINT ( 'NONE',  ( -10.91033749632886973, 4.885617943545219610, -4.996452313011736202 ) ) ;
#199029 = CARTESIAN_POINT ( 'NONE',  ( 9.578206935422253210, -9.900000000000005684, -0.1671882239536598425 ) ) ;
#199030 = CARTESIAN_POINT ( 'NONE',  ( 5.137628997053973912, 2.028260002996465250, -0.7749071676581267276 ) ) ;
#199031 = CARTESIAN_POINT ( 'NONE',  ( 3.404746562951189937, 1.438594061741470753, -1.123979961188771304 ) ) ;
#199032 = CARTESIAN_POINT ( 'NONE',  ( 1.112071775475082402, 1.959765382314464732, -0.09068415226199526280 ) ) ;
#199033 = CARTESIAN_POINT ( 'NONE',  ( 5.647700563513772920, 2.085583167219496215, -0.3645771090082204902 ) ) ;
#199034 = ORIENTED_EDGE ( 'NONE', *, *, #195328, .F. ) ;
#199036 = CARTESIAN_POINT ( 'NONE',  ( -0.6823417656250212460, 3.863541667008085767, 1.181850606188767472 ) ) ;
#199035 = CARTESIAN_POINT ( 'NONE',  ( 5.952705545545641463, -1.964087939335951827, -1.181845259310390306 ) ) ;
#199037 = CARTESIAN_POINT ( 'NONE',  ( 10.06423010004587759, 10.63602329300870153, 0.000000000000000000 ) ) ;
#199038 = CARTESIAN_POINT ( 'NONE',  ( 1.453939175038564624, -1.538220317728825393, -1.459821603020584613 ) ) ;
#199039 = CARTESIAN_POINT ( 'NONE',  ( -3.633221978782283923, 7.182583375313884133, -0.7216878364870267237 ) ) ;
#199040 = AXIS2_PLACEMENT_3D ( 'NONE', #142114, #43535, #205997 ) ;
#199041 = CARTESIAN_POINT ( 'NONE',  ( 5.858531774436539052, 6.007577623030311287, 0.000000000000000000 ) ) ;
#199042 = CARTESIAN_POINT ( 'NONE',  ( -3.890826896997578999, 7.483122446565064756, 0.7216878364870317197 ) ) ;
#199043 =( BOUNDED_CURVE ( )  B_SPLINE_CURVE ( 2, ( #126443, #108048, #206529, #139427, #156743, #172994, #192406, #72249, #124319 ),
 .UNSPECIFIED., .F., .T. ) 
 B_SPLINE_CURVE_WITH_KNOTS ( ( 3, 2, 2, 2, 3 ),
 ( 0.07812500000000006939, 0.08333333333333332871, 0.09375000000000000000, 0.1041666666666666713, 0.1093749999999997641 ),
 .UNSPECIFIED. ) 
 CURVE ( )  GEOMETRIC_REPRESENTATION_ITEM ( )  RATIONAL_B_SPLINE_CURVE ( ( 0.9330127018922194093, 0.9330127018922202975, 1.000000000000000000, 0.8660254037844387076, 1.000000000000000000, 0.8660254037844387076, 1.000000000000000000, 0.9330127018922224069, 0.9330127018922194093 ) ) 
 REPRESENTATION_ITEM ( '' )  );
#199044 = CARTESIAN_POINT ( 'NONE',  ( 6.895391736652770831, -1.943277935985653349, 0.9682779983983346161 ) ) ;
#199046 = CARTESIAN_POINT ( 'NONE',  ( 1.499999999999997113, 12.92708333401612819, -0.8660254037844378194 ) ) ;
#199045 = CARTESIAN_POINT ( 'NONE',  ( 6.883263157960365142, -0.007059606330772279746, 2.153658854459541416 ) ) ;
#199049 = ORIENTED_EDGE ( 'NONE', *, *, #46016, .F. ) ;
#199048 = CARTESIAN_POINT ( 'NONE',  ( 2.315342353584739055, 1.782219222887641674, -1.325647956807120220 ) ) ;
#199047 = AXIS2_PLACEMENT_3D ( 'NONE', #25855, #10666, #192616 ) ;
#199050 = CARTESIAN_POINT ( 'NONE',  ( -0.08672817704761734414, -1.422268874607252043, -1.807091132531572608 ) ) ;
#199052 = CARTESIAN_POINT ( 'NONE',  ( 4.961816841544592904, -0.5550570666568316325, 1.986392505239948036 ) ) ;
#199051 = CARTESIAN_POINT ( 'NONE',  ( 3.337278367258157630, 7.045241861776501580, 0.7998128361456341429 ) ) ;
#199054 = CARTESIAN_POINT ( 'NONE',  ( 3.475000000000000533, -3.325000000000001510, 0.000000000000000000 ) ) ;
#199053 = CARTESIAN_POINT ( 'NONE',  ( 5.481239241674765950, 9.616805891921051952, -0.7998128361456481317 ) ) ;
#199055 = CARTESIAN_POINT ( 'NONE',  ( 4.701645408888975197, 8.707279753670952971, 0.000000000000000000 ) ) ;
#199056 = CARTESIAN_POINT ( 'NONE',  ( -3.285556943749998737, -3.317708332855375808, 1.896917185911908499 ) ) ;
#199057 = CARTESIAN_POINT ( 'NONE',  ( -0.4019237886466966447, 12.80133545031536890, 1.500000000000003997 ) ) ;
#199058 = CARTESIAN_POINT ( 'NONE',  ( 0.1465796939425691170, -1.677718324701961361, 1.247191284554289625 ) ) ;
#199059 = CARTESIAN_POINT ( 'NONE',  ( 4.236954046275762664, 2.015912997090345549, -0.05229627655192746472 ) ) ;
#199060 = CARTESIAN_POINT ( 'NONE',  ( 3.983814121021773680, -1.821778379405362136, -0.2661574599523569007 ) ) ;
#199061 = CARTESIAN_POINT ( 'NONE',  ( 6.342516933094585418, 6.294024598232139667, 1.040834085586084257E-14 ) ) ;
#199062 = CARTESIAN_POINT ( 'NONE',  ( 2.045521581634631048, 0.6637456736250256784, -1.592148833096140192 ) ) ;
#199063 = CARTESIAN_POINT ( 'NONE',  ( 0.6203277878081385754, 1.987498645412737908, 0.3399528957561820386 ) ) ;
#199064 = CARTESIAN_POINT ( 'NONE',  ( 2.321245813631057864, 1.080353426350823209, -2.028982405110477227 ) ) ;
#199065 = CARTESIAN_POINT ( 'NONE',  ( -4.564291269294938225, 8.476756914152748124, 1.040834085586084257E-14 ) ) ;
#199066 = CARTESIAN_POINT ( 'NONE',  ( 1.529016648559086811, 2.180303969971490563, 0.6036265194416541302 ) ) ;
#199067 = CARTESIAN_POINT ( 'NONE',  ( 3.721394855333003626, -0.1548319924524182156, 2.100431540652194062 ) ) ;
#199068 = CARTESIAN_POINT ( 'NONE',  ( -3.772911886352873445, 7.623757310712140800, 0.7998128361456352531 ) ) ;
#199069 = CARTESIAN_POINT ( 'NONE',  ( 7.772902139336337335, 7.962807338847539107, 0.7998128361456341429 ) ) ;
#199070 = CARTESIAN_POINT ( 'NONE',  ( 4.516274566683592617, 8.283087737857252719, -0.7216878364870357165 ) ) ;
#199071 = CARTESIAN_POINT ( 'NONE',  ( 6.718719045489192965, -0.7860540964614262105, 1.895863743164223347 ) ) ;
#199073 = EDGE_CURVE ( 'NONE', #96770, #203624, #30908, .T. ) ;
#199072 = CARTESIAN_POINT ( 'NONE',  ( -4.550733115681270036, 8.460939068270139529, 0.7998128361456481317 ) ) ;
#199074 = CARTESIAN_POINT ( 'NONE',  ( 1.499999999999989120, 2.754166666666688190, 0.8660254037844524744 ) ) ;
#199075 = CARTESIAN_POINT ( 'NONE',  ( -3.867100128395853709, 5.534702787927018974, -1.599625672291256295 ) ) ;
#199076 = CARTESIAN_POINT ( 'NONE',  ( 5.185853984360066171, 2.140751028750527141, -0.5928278168529849124 ) ) ;
#199077 = CARTESIAN_POINT ( 'NONE',  ( 3.504031732436951874, -0.8880451304637152488, -2.003635182500095535 ) ) ;
#199078 = CARTESIAN_POINT ( 'NONE',  ( -5.935772324684618795, 5.819489221753827657, 0.000000000000000000 ) ) ;
#199079 = CARTESIAN_POINT ( 'NONE',  ( -5.171509248969888617, 4.998125310078441075, 0.7998128361456281477 ) ) ;
#199080 = CARTESIAN_POINT ( 'NONE',  ( -1.364683531250012516, 2.988541667008091096, -0.7879004041258289570 ) ) ;
#199081 = CARTESIAN_POINT ( 'NONE',  ( 6.890000000000010338, 2.965158640989657979, 2.452917560796507246 ) ) ;
#199082 = CARTESIAN_POINT ( 'NONE',  ( -5.341549334104202629, 7.254893527920112994, 1.443375672974064550 ) ) ;
#199083 = CARTESIAN_POINT ( 'NONE',  ( 5.238584497427841491, 1.261362679698872169, -1.704546977916908457 ) ) ;
#199084 = CARTESIAN_POINT ( 'NONE',  ( -6.292392690518209264, 8.434487120394948079, -1.443375672974066548 ) ) ;
#199085 = ORIENTED_EDGE ( 'NONE', *, *, #17820, .F. ) ;
#199087 = CARTESIAN_POINT ( 'NONE',  ( -1.441119962213332828, 8.287674021641837641, -3.161270278916411769 ) ) ;
#199086 = CARTESIAN_POINT ( 'NONE',  ( -6.319508997745553636, 6.545384383557486530, 0.7216878364870257245 ) ) ;
#199088 = CARTESIAN_POINT ( 'NONE',  ( 5.843727902690005749, 6.776436293681846301, -1.199719254218445830 ) ) ;
#199089 = CARTESIAN_POINT ( 'NONE',  ( 5.882333747326812912, -0.2767177626767612919, -1.820229446528654371 ) ) ;
#199090 = SURFACE_STYLE_USAGE ( .BOTH. , #198042 ) ;
#199091 = CARTESIAN_POINT ( 'NONE',  ( -1.364683531250012516, 3.301041667008084879, -0.7879004041258289570 ) ) ;
#199092 = CARTESIAN_POINT ( 'NONE',  ( 0.9249085282522085949, -1.102964995092512890, -1.346285399390812598 ) ) ;
#199093 = CARTESIAN_POINT ( 'NONE',  ( 3.063252641683779753, 5.661212951017999373, 1.199719254218450271 ) ) ;
#199094 = CARTESIAN_POINT ( 'NONE',  ( 11.52483635780546045, 12.22000008642463165, 3.345866325258042284 ) ) ;
#199095 = CARTESIAN_POINT ( 'NONE',  ( -1.402160292154681736E-14, 0.1343750003414218575, 1.575800808251672791 ) ) ;
#199096 = CARTESIAN_POINT ( 'NONE',  ( 0.000000000000000000, 6.002124920821316323, 0.000000000000000000 ) ) ;
#199097 = CARTESIAN_POINT ( 'NONE',  ( 5.471600609837615536, 2.084441204114939161, -0.5725544205837928002 ) ) ;
#199098 = CARTESIAN_POINT ( 'NONE',  ( -3.164938793786285842, 5.779846795137578930, -1.199719254218452935 ) ) ;
#199099 = CARTESIAN_POINT ( 'NONE',  ( -5.680503174001480637, 9.571078103069643461, 0.7216878364870458196 ) ) ;
#199100 = VECTOR ( 'NONE', #147092, 1000.000000000000000 ) ;
#199101 = CARTESIAN_POINT ( 'NONE',  ( 5.172814640947125397, -2.034155943344346795, -0.7319064324283753864 ) ) ;
#199102 = ORIENTED_EDGE ( 'NONE', *, *, #71220, .T. ) ;
#199103 = CARTESIAN_POINT ( 'NONE',  ( 0.6823417656249899377, 2.842708333674753618, 1.181850606188765695 ) ) ;
#199104 = CARTESIAN_POINT ( 'NONE',  ( 6.380149230842863339, -1.056690401097816867, 1.664064485322758635 ) ) ;
#199105 = CARTESIAN_POINT ( 'NONE',  ( 4.798016402085652388, -1.585019518093808699, 0.7031974489903334291 ) ) ;
#199107 = CARTESIAN_POINT ( 'NONE',  ( 1.786939262935317130, 1.904797134731281538, -1.083727916527020607 ) ) ;
#199106 = CARTESIAN_POINT ( 'NONE',  ( -5.758872628492444169E-14, -0.1718749996585747786, -1.570758158831818241 ) ) ;
#199108 = CARTESIAN_POINT ( 'NONE',  ( 2.591229953566904776, -0.3941274307956154077, -2.273529888306951019 ) ) ;
#199109 = CARTESIAN_POINT ( 'NONE',  ( 4.675106833541732954, 0.004019643978107888781, -2.060967561157340810 ) ) ;
#199110 = CARTESIAN_POINT ( 'NONE',  ( 0.5505969416323712728, -1.640064848914600804, -1.039604180477508688 ) ) ;
#199111 = CARTESIAN_POINT ( 'NONE',  ( -6.683806541412768532, 8.820860269780128604, -1.443375672974058777 ) ) ;
#199113 = EDGE_CURVE ( 'NONE', #116857, #71330, #185846, .T. ) ;
#199112 = CARTESIAN_POINT ( 'NONE',  ( -3.654804927335652209, 6.421633627603656080, 1.199719254218452935 ) ) ;
#199114 = DIRECTION ( 'NONE',  ( 0.000000000000000000, 0.000000000000000000, -1.000000000000000000 ) ) ;
#199115 = CARTESIAN_POINT ( 'NONE',  ( 3.428091063814618700, -2.088597262255381448, 0.3661859999234198249 ) ) ;
#199116 = FACE_OUTER_BOUND ( 'NONE', #34620, .T. ) ;
#199117 = CARTESIAN_POINT ( 'NONE',  ( 1.529922885524274134, -1.701946718671920600, 1.081067414773040802 ) ) ;
#199118 = CARTESIAN_POINT ( 'NONE',  ( -6.114364089638801403, 8.156510742710487705, 1.443375672974078761 ) ) ;
#199119 = CARTESIAN_POINT ( 'NONE',  ( 4.647634198631804381, -1.703412986257560879, -1.402924735643434673 ) ) ;
#199120 = CARTESIAN_POINT ( 'NONE',  ( 1.001543065824772753E-15, -2.209374999522042859, 3.793834371823811669 ) ) ;
#199121 = CARTESIAN_POINT ( 'NONE',  ( 1.885388715806934679, -1.754394424870173719, 0.6211283009984622794 ) ) ;
#199122 = CARTESIAN_POINT ( 'NONE',  ( 0.000000000000000000, 1.000000000000000888, 0.000000000000000000 ) ) ;
#199123 = DIRECTION ( 'NONE',  ( 0.000000000000000000, 1.000000000000000000, 0.000000000000000000 ) ) ;
#199124 = CARTESIAN_POINT ( 'NONE',  ( 2.265485140597475855, 2.737013068702903063, -2.500000000000000444 ) ) ;
#199126 = CARTESIAN_POINT ( 'NONE',  ( 6.925078400183549476, 6.033022220673083247, 2.839235739982972184 ) ) ;
#199125 = CARTESIAN_POINT ( 'NONE',  ( -4.600441534204600558, 8.479163753367195966, -0.2584006677722027745 ) ) ;
#199127 =( NAMED_UNIT ( * ) SI_UNIT ( $, .STERADIAN. ) SOLID_ANGLE_UNIT ( ) );
#199128 = VERTEX_POINT ( 'NONE', #152344 ) ;
#199129 = CARTESIAN_POINT ( 'NONE',  ( 3.291920626085430346, -0.8366078139741841557, 1.883634853023412825 ) ) ;
#199130 = CARTESIAN_POINT ( 'NONE',  ( 1.360316468749949825, 1.994791667008131597, 0.7853790794158701516 ) ) ;
#199131 = CARTESIAN_POINT ( 'NONE',  ( -6.392833124043511894, 7.417059051927569868, 1.199719254218450271 ) ) ;
#199132 = CARTESIAN_POINT ( 'NONE',  ( 3.598311091834342612, -0.9934155151001385908, 1.758370388466141465 ) ) ;
#199133 = CARTESIAN_POINT ( 'NONE',  ( -0.7500000000000006661, -0.1416666666666441254, -1.299038105676652011 ) ) ;
#199134 = CARTESIAN_POINT ( 'NONE',  ( 3.277320446201373638, 4.846626492033466072, 1.599625672291267398 ) ) ;
#199135 = CARTESIAN_POINT ( 'NONE',  ( 1.868112839806375325, 1.058416689118582665, 1.768180007894581740 ) ) ;
#199137 = CARTESIAN_POINT ( 'NONE',  ( 1.364683531250000303, 13.25520833367472839, -0.7879004041258355073 ) ) ;
#199136 = CARTESIAN_POINT ( 'NONE',  ( -9.508795732819951496, 14.91378867702411171, -7.212928819065533403 ) ) ;
#199138 = CARTESIAN_POINT ( 'NONE',  ( 4.469384193999260901, 8.366031992974468423, -0.7998128361456231517 ) ) ;
#199139 =( BOUNDED_SURFACE ( )  B_SPLINE_SURFACE ( 3, 3, ( 
 ( #209019, #58532, #46561, #112681, #190645, #193850, #109491, #176552, #175498, #207966, #10826 ),
 ( #127899, #111616, #27086, #108420, #192775, #95328, #76900, #59592, #158182, #161377, #45500 ),
 ( #143024, #144097, #110550, #60655, #28162, #94258, #160297, #11900, #210092, #61731, #42305 ),
 ( #9774, #12961, #177628, #29236, #75847, #79038, #141954, #26018, #145153, #211159, #62783 ),
 ( #128946, #30305, #96390, #63858, #149375, #118007, #32430, #165626, #131064, #115867, #200234 ),
 ( #50806, #16145, #82230, #180804, #17214, #67024, #214320, #146207, #213289, #98496, #47640 ),
 ( #167757, #35610, #101688, #64915, #134224, #34549, #148321, #182933, #48690, #197052, #958 ) ),
 .UNSPECIFIED., .T., .F., .T. ) 
 B_SPLINE_SURFACE_WITH_KNOTS ( ( 4, 3, 4 ),
 ( 4, 1, 1, 1, 1, 1, 1, 1, 4 ),
 ( 0.000000000000000000, 0.5000000000000000000, 1.000000000000000000 ),
 ( 0.000000000000000000, 0.2256777920876190668, 0.3978457394851813711, 0.5256768607792676740, 0.6183602023682204241, 0.6850295134299612121, 0.7345374503969632762, 0.7752450576501028756, 1.000000000000000000 ),
 .UNSPECIFIED. ) 
 GEOMETRIC_REPRESENTATION_ITEM ( )  RATIONAL_B_SPLINE_SURFACE ( (
 ( 1.000000000000000000, 1.000000000000000000, 1.000000000000000000, 1.000000000000000222, 0.9999999999999997780, 1.000000000000000444, 0.9999999999999997780, 1.000000000000000222, 0.9999999999999996669, 1.000000000000000222, 1.000000000000000222),
 ( 0.3333333333333333703, 0.3333333333333334259, 0.3333333333333333703, 0.3333333333333334259, 0.3333333333333333703, 0.3333333333333334259, 0.3333333333333333703, 0.3333333333333334259, 0.3333333333333333148, 0.3333333333333334259, 0.3333333333333334259),
 ( 0.3333333333333333703, 0.3333333333333334259, 0.3333333333333333703, 0.3333333333333334259, 0.3333333333333333703, 0.3333333333333334259, 0.3333333333333333703, 0.3333333333333334259, 0.3333333333333333148, 0.3333333333333334259, 0.3333333333333334259),
 ( 1.000000000000000000, 1.000000000000000000, 1.000000000000000000, 1.000000000000000222, 0.9999999999999997780, 1.000000000000000444, 0.9999999999999997780, 1.000000000000000222, 0.9999999999999996669, 1.000000000000000222, 1.000000000000000222),
 ( 0.3333333333333333703, 0.3333333333333334259, 0.3333333333333333703, 0.3333333333333334259, 0.3333333333333333703, 0.3333333333333334259, 0.3333333333333333703, 0.3333333333333334259, 0.3333333333333333148, 0.3333333333333334259, 0.3333333333333334259),
 ( 0.3333333333333333703, 0.3333333333333334259, 0.3333333333333333703, 0.3333333333333334259, 0.3333333333333333703, 0.3333333333333334259, 0.3333333333333333703, 0.3333333333333334259, 0.3333333333333333148, 0.3333333333333334259, 0.3333333333333334259),
 ( 1.000000000000000000, 1.000000000000000000, 1.000000000000000000, 1.000000000000000222, 0.9999999999999997780, 1.000000000000000444, 0.9999999999999997780, 1.000000000000000222, 0.9999999999999996669, 1.000000000000000222, 1.000000000000000222) ) ) 
 REPRESENTATION_ITEM ( '' )  SURFACE ( )  );
#199140 = CARTESIAN_POINT ( 'NONE',  ( -0.2408018239684096284, -0.007136184528808932684, -2.100252307185761058 ) ) ;
#199141 = CARTESIAN_POINT ( 'NONE',  ( 1.235996726672627943, 0.3573974351761283752, 1.805938768738392319 ) ) ;
#199142 = CARTESIAN_POINT ( 'NONE',  ( 5.637410271038987730, -1.996576301129053377, 0.9405272304151901519 ) ) ;
#199143 = CARTESIAN_POINT ( 'NONE',  ( 6.713222337422018349, 7.861122810861019161, -1.199719254218452047 ) ) ;
#199144 = CARTESIAN_POINT ( 'NONE',  ( 1.933122032479916985, 0.2097677157741582865, 2.151362962771664833 ) ) ;
#199145 = CARTESIAN_POINT ( 'NONE',  ( -4.473827502829599290, 4.321812962830357208, 0.7216878364870317197 ) ) ;
#199146 = CARTESIAN_POINT ( 'NONE',  ( 2.114470590943520634, 1.957170936680457052, 0.4852650170619755565 ) ) ;
#199147 = EDGE_CURVE ( 'NONE', #191645, #90168, #53779, .T. ) ;
#199148 = CARTESIAN_POINT ( 'NONE',  ( 4.608569825152843968, 8.455154480611607681, 0.5018163687887734481 ) ) ;
#199149 = CARTESIAN_POINT ( 'NONE',  ( -0.1605634594619409494, 7.049300555817002767, 3.948520363690844359 ) ) ;
#199150 = B_SPLINE_CURVE_WITH_KNOTS ( 'NONE', 3,
 ( #130347, #127151, #12231, #209350 ),
 .UNSPECIFIED., .F., .F.,
 ( 4, 4 ),
 ( 0.001582017824277144819, 0.002341702326271049434 ),
 .UNSPECIFIED. ) ;
#199151 = CARTESIAN_POINT ( 'NONE',  ( 1.872868072690832220, 8.979822391611987698, -0.7749999999999996891 ) ) ;
#199152 = CARTESIAN_POINT ( 'NONE',  ( 4.082859939823464401, -0.1922352567787863620, -1.962060651276048118 ) ) ;
#199153 = CARTESIAN_POINT ( 'NONE',  ( 3.239470508323912146, 0.4852670486454255250, -1.957170429962351577 ) ) ;
#199155 = CARTESIAN_POINT ( 'NONE',  ( 8.215877899756996783, 12.52901528311778989, 1.040834085586084257E-14 ) ) ;
#199154 = CARTESIAN_POINT ( 'NONE',  ( -1.201851678989727383E-14, 1.821875000341421691, 1.575800808251672791 ) ) ;
#199157 = CARTESIAN_POINT ( 'NONE',  ( 6.252575686221216955, 0.6590897193336446858, 2.000345064990595390 ) ) ;
#199156 = CARTESIAN_POINT ( 'NONE',  ( -6.906989191158078079, 10.14557225873805812, -1.199719254218440723 ) ) ;
#199158 = CARTESIAN_POINT ( 'NONE',  ( 5.775854211382815073, -2.020734006234246927, 0.4499205674863211990 ) ) ;
#199159 = CARTESIAN_POINT ( 'NONE',  ( 7.657657833620182153, 7.828355648845348291, -0.7998128361456281477 ) ) ;
#199160 = CARTESIAN_POINT ( 'NONE',  ( -7.226659571283968297, 8.389856573708110332, 1.199719254218450271 ) ) ;
#199161 = CARTESIAN_POINT ( 'NONE',  ( -1.594690046439253273, 8.741643652401169362, 2.463706593913791210 ) ) ;
#199162 = CARTESIAN_POINT ( 'NONE',  ( 4.728773938389556619, 1.389870793851749164, -1.465793203850384030 ) ) ;
#199163 = CARTESIAN_POINT ( 'NONE',  ( -1.500000000000001332, -0.3187499993171846735, 0.000000000000000000 ) ) ;
#199164 = CARTESIAN_POINT ( 'NONE',  ( 0.5497677191402570163, 1.525909772416549126, 1.387868932477815065 ) ) ;
#199165 = CARTESIAN_POINT ( 'NONE',  ( 6.941411460516762943, 11.04213777067082702, -0.7216878364870267237 ) ) ;
#199166 = CARTESIAN_POINT ( 'NONE',  ( 5.668190738965027897, 8.770583741171307679, -1.199719254218452047 ) ) ;
#199167 = CARTESIAN_POINT ( 'NONE',  ( 4.712340909201580885, 7.655425606447271214, -1.199719254218452047 ) ) ;
#199168 = CARTESIAN_POINT ( 'NONE',  ( -1.402160292154681736E-14, 0.6343750003414162508, 1.575800808251672791 ) ) ;
#199170 = CARTESIAN_POINT ( 'NONE',  ( 3.432607057648175530, 6.331044601171339714, 1.095529308728976137 ) ) ;
#199169 = CARTESIAN_POINT ( 'NONE',  ( 4.041212305325117882, 6.872442235258051646, -1.199719254218448494 ) ) ;
#199171 = CARTESIAN_POINT ( 'NONE',  ( 7.090551149822744925, 7.374657217655760100, 0.7216878364870317197 ) ) ;
#199173 = DIRECTION ( 'NONE',  ( 0.8003905289055504024, -4.396526966619893387E-05, 0.5994789398347104559 ) ) ;
#199172 = CARTESIAN_POINT ( 'NONE',  ( 2.822911419172136949, -1.498817844263359067, 1.571052884911597003 ) ) ;
#199174 = CARTESIAN_POINT ( 'NONE',  ( -0.6744113354752461209, -0.8887487162305419686, -3.223033589173039282 ) ) ;
#199176 = CARTESIAN_POINT ( 'NONE',  ( 2.559893532628489954, -1.268187297466142338, 1.335118840784771166 ) ) ;
#199175 = CARTESIAN_POINT ( 'NONE',  ( -3.606105671554953318, 7.150947683548662503, 0.7216878364870317197 ) ) ;
#199177 = CARTESIAN_POINT ( 'NONE',  ( -0.6823417656250212460, 4.801041667008086655, 1.181850606188767472 ) ) ;
#199178 = CARTESIAN_POINT ( 'NONE',  ( 4.212563348414651188, 2.004022095860341413, 0.8874167208733558798 ) ) ;
#199179 = CARTESIAN_POINT ( 'NONE',  ( 7.860983254381821439, 14.39106760530863838, 9.010984000332380006 ) ) ;
#199180 = CARTESIAN_POINT ( 'NONE',  ( 4.294006694993548479, -0.8693707907260415091, 2.089011835857216948 ) ) ;
#199181 = CARTESIAN_POINT ( 'NONE',  ( -5.012244793233714191, 6.784968962630095746, -1.449178643049347848 ) ) ;
#199182 = CARTESIAN_POINT ( 'NONE',  ( 4.780342502845265074, 8.269896785439653897, -0.8296954209953393278 ) ) ;
#199183 = CARTESIAN_POINT ( 'NONE',  ( -6.089020385868867180, 7.236850217336030511, -1.082531754730549967 ) ) ;
#199184 = CARTESIAN_POINT ( 'NONE',  ( 4.258669648468278446, 7.022179452304728287, 1.082531754730549078 ) ) ;
#199185 = CARTESIAN_POINT ( 'NONE',  ( 6.784453145350711090, -1.736176628054094007, -0.3419908188336401311 ) ) ;
#199186 = CARTESIAN_POINT ( 'NONE',  ( 3.809243135778153100, 1.699416117590052622, -1.078869421455890709 ) ) ;
#199187 = CARTESIAN_POINT ( 'NONE',  ( 7.039708073993665494, 9.236078724457858158, 1.599625672291281386 ) ) ;
#199188 = CARTESIAN_POINT ( 'NONE',  ( 2.573382939595921570, 0.1044104795966259297, -2.103504788083962573 ) ) ;
#199189 = CARTESIAN_POINT ( 'NONE',  ( 1.265090914671564759, 1.769361140067410521, -0.7345930670351871195 ) ) ;
#199191 = CARTESIAN_POINT ( 'NONE',  ( -1.201851678989727383E-14, 2.837500000000024780, -1.732050807568863648 ) ) ;
#199190 = CARTESIAN_POINT ( 'NONE',  ( -0.6823417656250039265, 12.06770833367473017, -1.181850606188755259 ) ) ;
#199193 = EDGE_CURVE ( 'NONE', #106774, #22081, #102756, .T. ) ;
#199192 = CARTESIAN_POINT ( 'NONE',  ( 1.557020932125362078, 1.611981373198448253, -1.131376696270647075 ) ) ;
#199194 = CARTESIAN_POINT ( 'NONE',  ( 0.3209005354254980680, -0.09642172165634513292, 1.868300368337752815 ) ) ;
#199195 = CARTESIAN_POINT ( 'NONE',  ( 0.8538673084422104820, -0.7095216264049221122, 1.829241926910141203 ) ) ;
#199197 = ORIENTED_EDGE ( 'NONE', *, *, #31081, .F. ) ;
#199196 = CARTESIAN_POINT ( 'NONE',  ( -0.1757481403069499348, -0.8193859263425256056, -1.726394157293544840 ) ) ;
#199198 = CARTESIAN_POINT ( 'NONE',  ( 5.504247177468179153, 7.444707678511436555, 1.443375672974062551 ) ) ;
#199199 = CARTESIAN_POINT ( 'NONE',  ( -1.402160292154681736E-14, 0.2593750003414224681, -1.575800808251665908 ) ) ;
#199200 = EDGE_CURVE ( 'NONE', #137942, #78671, #37135, .T. ) ;
#199202 = CARTESIAN_POINT ( 'NONE',  ( 5.612129163471575310, -0.8422657237196762292, -1.670366365510121742 ) ) ;
#199201 = VECTOR ( 'NONE', #9530, 1000.000000000000000 ) ;
#199203 = CARTESIAN_POINT ( 'NONE',  ( 8.380911511541880188, 12.92948053010758258, 0.7998128361456462443 ) ) ;
#199204 = CARTESIAN_POINT ( 'NONE',  ( 0.000000000000000000, 0.5000000000000004441, 0.000000000000000000 ) ) ;
#199205 = CARTESIAN_POINT ( 'NONE',  ( 6.789897376884641567, -1.347643488625469121, -1.571692526165118009 ) ) ;
#199206 = CARTESIAN_POINT ( 'NONE',  ( -7.041790712887801895, 6.002124920821316323, -2.446252293856579829 ) ) ;
#199207 = CARTESIAN_POINT ( 'NONE',  ( 2.450243370979061641, 1.813773193624685254, -11.74719778151168015 ) ) ;
#199208 = CARTESIAN_POINT ( 'NONE',  ( -1.500000000000013101, 1.129166666666688634, -0.8660254037844313801 ) ) ;
#199209 = CARTESIAN_POINT ( 'NONE',  ( 7.962716289927667113, 8.184257181204083409, -0.7998128361456291469 ) ) ;
#199210 = CARTESIAN_POINT ( 'NONE',  ( -9.189729191964438826, 9.615772233580322848, 1.040834085586084257E-14 ) ) ;
#199211 = CARTESIAN_POINT ( 'NONE',  ( 5.342795052237045539, 8.390955439988655229, -1.199719254218450271 ) ) ;
#199212 = CARTESIAN_POINT ( 'NONE',  ( 4.934241560730721510, 4.721313007132757811, 0.000000000000000000 ) ) ;
#199213 = CARTESIAN_POINT ( 'NONE',  ( 1.364683531249986537, 0.9052083336747533959, -0.7879004041258239610 ) ) ;
#199214 = ORIENTED_EDGE ( 'NONE', *, *, #120681, .F. ) ;
#199216 = EDGE_CURVE ( 'NONE', #81519, #109478, #42864, .T. ) ;
#199215 = CARTESIAN_POINT ( 'NONE',  ( -1.500000000000013101, 2.170833333333357373, 0.8660254037844403729 ) ) ;
#199218 = CARTESIAN_POINT ( 'NONE',  ( 2.984766373302843778, 6.633977868828633717, -0.7998128361456291469 ) ) ;
#199217 = CARTESIAN_POINT ( 'NONE',  ( 5.951606347324345236, 1.484592722905058393, 1.282605414028796353 ) ) ;
#199219 = CARTESIAN_POINT ( 'NONE',  ( 3.567732365556259388, 1.591074578583807853, -1.238131541301431326 ) ) ;
#199220 = CARTESIAN_POINT ( 'NONE',  ( 4.065584057473277113, 1.255829935711678669, 1.446728075138058678 ) ) ;
#199221 = CARTESIAN_POINT ( 'NONE',  ( 11.87815913191726125, 9.796921793685850588, -1.708869976696599347 ) ) ;
#199222 = CARTESIAN_POINT ( 'NONE',  ( 1.382659466718983543, -0.3261178763579902773, -2.167053615394160637 ) ) ;
#199223 = FACE_OUTER_BOUND ( 'NONE', #116061, .T. ) ;
#199224 = CARTESIAN_POINT ( 'NONE',  ( 2.969827553264007047, 0.9974664638083343693, 1.582205488144486250 ) ) ;
#199225 = CARTESIAN_POINT ( 'NONE',  ( -0.7500000000000249800, -0.7770833326505161009, 1.299038105676659116 ) ) ;
#199226 = CARTESIAN_POINT ( 'NONE',  ( -6.832419346282942563, 10.05857410638369487, 1.199719254218453823 ) ) ;
#199228 = CARTESIAN_POINT ( 'NONE',  ( 4.323895160615763622, 0.9038210025188663232, -1.914733396627795958 ) ) ;
#199227 = CARTESIAN_POINT ( 'NONE',  ( -5.422898255786209099, 5.429062174613087599, -0.7216878364870207285 ) ) ;
#199229 = SURFACE_STYLE_FILL_AREA ( #133223 ) ;
#199230 = CARTESIAN_POINT ( 'NONE',  ( 5.846161131210033446, -0.9342735719010831774, 1.847668428805064655 ) ) ;
#199232 = CARTESIAN_POINT ( 'NONE',  ( 6.620655732516611103, 6.033324165176342291, 2.868629481857593255 ) ) ;
#199231 = CARTESIAN_POINT ( 'NONE',  ( 2.349268366499413840, 0.5549471352096692067, -2.015694315139557435 ) ) ;
#199234 = EDGE_LOOP ( 'NONE', ( #167954, #17839, #118239, #209217 ) ) ;
#199233 = CARTESIAN_POINT ( 'NONE',  ( 0.3227381541650706787, -0.09231566880639123507, 1.722440863776145692 ) ) ;
#199235 = CARTESIAN_POINT ( 'NONE',  ( 6.636879889089462026, 7.701780277814560982, -1.199719254218446718 ) ) ;
#199236 = CARTESIAN_POINT ( 'NONE',  ( 6.928203230275522095, 15.51887838114830132, 9.797958971132704420 ) ) ;
#199237 = CARTESIAN_POINT ( 'NONE',  ( -0.3000000000000033751, 3.950000000000001954, -1.007084189318394385 ) ) ;
#199238 = CARTESIAN_POINT ( 'NONE',  ( -9.587704862635016312, 4.026159954882873926, 6.671158199369250141 ) ) ;
#199240 = CARTESIAN_POINT ( 'NONE',  ( 7.009202228140744673, 9.200488570962775725, -1.443375672974058777 ) ) ;
#199239 = CARTESIAN_POINT ( 'NONE',  ( 7.969495366734495434, 8.192166104145387706, 1.040834085586084257E-14 ) ) ;
#199241 = CARTESIAN_POINT ( 'NONE',  ( 0.4652293495370784515, 7.465077128757543257, -4.424517295598819011 ) ) ;
#199243 = CARTESIAN_POINT ( 'NONE',  ( 0.2580964568148482741, 1.806467626183925423, 0.1351022710447576103 ) ) ;
#199242 = CARTESIAN_POINT ( 'NONE',  ( 6.587282531393223728, 8.778525268082516320, 1.599625672291268286 ) ) ;
#199244 = CARTESIAN_POINT ( 'NONE',  ( -8.206763054973658100, 8.468978407091068306, 0.7998128361456602331 ) ) ;
#199245 = CARTESIAN_POINT ( 'NONE',  ( 3.018661757337009810, 6.673522483535157868, 0.000000000000000000 ) ) ;
#199246 = CARTESIAN_POINT ( 'NONE',  ( -5.804269833667989431, 7.239147048582937671, 1.181955602297209751 ) ) ;
#199247 = CARTESIAN_POINT ( 'NONE',  ( 6.713222337422018349, 7.861122810861019161, -1.199719254218452047 ) ) ;
#199248 = DIRECTION ( 'NONE',  ( -7.387867266669436732E-31, -1.000000000000000000, 8.546850786086437571E-32 ) ) ;
#199249 = CARTESIAN_POINT ( 'NONE',  ( 1.123270288250311610, 3.172697346350006331, 0.7749999999993734123 ) ) ;
#199250 = CYLINDRICAL_SURFACE ( 'NONE', #175780, 0.08000000000000020983 ) ;
#199251 = CARTESIAN_POINT ( 'NONE',  ( 8.432808358020015049, 11.82173160345663376, 1.082531754730546636 ) ) ;
#199252 = VERTEX_POINT ( 'NONE', #139312 ) ;
#199253 = MECHANICAL_DESIGN_GEOMETRIC_PRESENTATION_REPRESENTATION (  '', ( #57967 ), #81775 ) ;
#199254 = CARTESIAN_POINT ( 'NONE',  ( 3.314761293198214887, -1.410806105172614178, 1.213857476866337937 ) ) ;
#199255 = CARTESIAN_POINT ( 'NONE',  ( 0.4564612863584472380, -1.804040949374663194, -0.6446129174930875783 ) ) ;
#199256 = CARTESIAN_POINT ( 'NONE',  ( 0.6629299983115041206, 0.6194173074674096391, 2.027988828570789437 ) ) ;
#199257 = SURFACE_STYLE_FILL_AREA ( #133252 ) ;
#199258 = AXIS2_PLACEMENT_3D ( 'NONE', #72487, #108277, #208879 ) ;
#199259 = CARTESIAN_POINT ( 'NONE',  ( -0.1399997263889559695, 7.629137130509076492, -2.600276787041354343 ) ) ;
#199260 = CARTESIAN_POINT ( 'NONE',  ( 1.844764736977719366, 2.494476015512113509, 2.491383360649020773 ) ) ;
#199261 = CARTESIAN_POINT ( 'NONE',  ( -5.111060722671894929, 5.065251719313053513, 0.000000000000000000 ) ) ;
#199262 = CARTESIAN_POINT ( 'NONE',  ( 8.595506201384008449, 11.05117653974661529, 1.443375672974076540 ) ) ;
#199263 = CARTESIAN_POINT ( 'NONE',  ( 4.416829296269289884, -1.462161721869711384, 1.319618631580289581 ) ) ;
#199264 = EDGE_CURVE ( 'NONE', #152613, #33663, #205342, .T. ) ;
#199265 = CARTESIAN_POINT ( 'NONE',  ( 1.629697543846151619, -0.2563088357964183883, 2.104862515383609800 ) ) ;
#199266 = CARTESIAN_POINT ( 'NONE',  ( -5.368138756007025947, 8.350246751061767725, 1.199719254218452047 ) ) ;
#199267 = CARTESIAN_POINT ( 'NONE',  ( -1.162044386198238935E-15, 0.3125000000000180411, 1.224999999999967004 ) ) ;
#199268 = CARTESIAN_POINT ( 'NONE',  ( -3.123065541208358997, 6.445821767598281404, -0.7606279415795504928 ) ) ;
#199269 = VECTOR ( 'NONE', #32876, 1000.000000000000000 ) ;
#199270 = CARTESIAN_POINT ( 'NONE',  ( 5.455090197064776270, 0.4301712223657681022, -2.148646160378755443 ) ) ;
#199271 = CARTESIAN_POINT ( 'NONE',  ( -1.416814887940473167, 7.999555336178689302, -9.899480522462164700 ) ) ;
#199272 = CARTESIAN_POINT ( 'NONE',  ( 4.454074118230034962, 1.925978650549282856, -0.04673309505795821689 ) ) ;
#199273 = CARTESIAN_POINT ( 'NONE',  ( -8.532158741701643123, 8.848606708273724308, 0.7998128361456462443 ) ) ;
#199274 = EDGE_CURVE ( 'NONE', #103298, #6442, #24452, .T. ) ;
#199275 = CARTESIAN_POINT ( 'NONE',  ( 0.6393319655835436599, -1.287349573739982933, -1.294668131371433661 ) ) ;
#199276 = CARTESIAN_POINT ( 'NONE',  ( 1.049787907720298286, -1.741764784136769162, -1.355102641770723704 ) ) ;
#199277 = CARTESIAN_POINT ( 'NONE',  ( -0.4956004317509503099, 7.799479031273152785, 1.990828115380108176 ) ) ;
#199278 = ORIENTED_EDGE ( 'NONE', *, *, #13474, .F. ) ;
#199279 = CARTESIAN_POINT ( 'NONE',  ( 4.773879485787624333, 4.742149952939897162, -0.7216878364870357165 ) ) ;
#199280 = ORIENTED_EDGE ( 'NONE', *, *, #185415, .T. ) ;
#199281 = CARTESIAN_POINT ( 'NONE',  ( 6.069198383140281372, 1.735254367832469891, 0.9315073086425088578 ) ) ;
#199282 = CARTESIAN_POINT ( 'NONE',  ( 1.821723684117615427, 1.116499850783551073, -1.588862189236692091 ) ) ;
#199283 = CARTESIAN_POINT ( 'NONE',  ( 6.661448219487969169, -0.6026422599177021500, -2.217949877449727047 ) ) ;
#199285 = CARTESIAN_POINT ( 'NONE',  ( 4.399146427517338864, -1.620787001191201560, 0.9142094169404291204 ) ) ;
#199284 = CARTESIAN_POINT ( 'NONE',  ( -6.770317605177755382, 8.992066187497757213, 1.599625672291269396 ) ) ;
#199286 = CARTESIAN_POINT ( 'NONE',  ( 7.876360894896227371, 8.153785563659219804, -0.7998128361456341429 ) ) ;
#199287 = DIRECTION ( 'NONE',  ( -0.05872483221476467591, -7.952201780260630618E-17, 0.9982742078614211811 ) ) ;
#199288 = CARTESIAN_POINT ( 'NONE',  ( -5.717788096661253761, 7.693838750903348789, 1.599625672291269396 ) ) ;
#199289 = CARTESIAN_POINT ( 'NONE',  ( 6.720655732516658709, 4.700665033810172311, 2.388972926809574737 ) ) ;
#199290 = CARTESIAN_POINT ( 'NONE',  ( -0.09381621004311831158, -0.9424329983100244723, -1.976553698157037076 ) ) ;
#199291 = CARTESIAN_POINT ( 'NONE',  ( 3.687454593236936251, 7.245854758844324728, -0.7216878364870267237 ) ) ;
#199292 = DIRECTION ( 'NONE',  ( -5.551115123125764829E-17, 0.000000000000000000, 1.000000000000000000 ) ) ;
#199293 = CYLINDRICAL_SURFACE ( 'NONE', #65138, 3.100000000000000089 ) ;
#199294 = CARTESIAN_POINT ( 'NONE',  ( 1.435882461153328515, 0.9014729512111450127, -1.587519582607027635 ) ) ;
#199295 = CARTESIAN_POINT ( 'NONE',  ( -4.948889764188092677, 5.732458465429559169, 1.199719254218462483 ) ) ;
#199296 = CARTESIAN_POINT ( 'NONE',  ( 3.181945575597402431, 1.368952998951804556, 1.064414454346799266 ) ) ;
#199297 = CARTESIAN_POINT ( 'NONE',  ( -0.2808621375647266660, 2.697699530669510626, -1.982805148454100275 ) ) ;
#199298 = CARTESIAN_POINT ( 'NONE',  ( -1.225000000000014300, 2.750000000000002665, -3.469446951953614189E-14 ) ) ;
#199299 = CARTESIAN_POINT ( 'NONE',  ( 1.313174662617409227, 8.310476012147654856, -10.86148356754324773 ) ) ;
#199300 = CARTESIAN_POINT ( 'NONE',  ( 0.1703666795057276195, -1.259402025324443564, 1.457936571737717735 ) ) ;
#199301 = CARTESIAN_POINT ( 'NONE',  ( 4.856279117655732058, -1.961245242753749674, -0.05215834203427943683 ) ) ;
#199302 = CARTESIAN_POINT ( 'NONE',  ( -7.527801604085656351, 9.805521176231838609, 1.599625672291295375 ) ) ;
#199303 = CARTESIAN_POINT ( 'NONE',  ( 5.099838337034727331, 9.101561826515851550, -0.7998128361456281477 ) ) ;
#199304 = CARTESIAN_POINT ( 'NONE',  ( 4.459710115430675081, -1.639780234044617035, -1.344486126324248465 ) ) ;
#199305 = CARTESIAN_POINT ( 'NONE',  ( 5.885121196783658526, 9.023669275293071834, 1.199719254218452047 ) ) ;
#199306 = CARTESIAN_POINT ( 'NONE',  ( -7.486073373039941359, 11.88550270185529278, -0.7998128361456291469 ) ) ;
#199307 = CARTESIAN_POINT ( 'NONE',  ( 5.497994985541524215, 6.373081223675282736, -1.199719254218445830 ) ) ;
#199308 = CARTESIAN_POINT ( 'NONE',  ( 2.694261129275489886, 0.9798316074655871732, -1.823736424811234658 ) ) ;
#199310 = CARTESIAN_POINT ( 'NONE',  ( -1.364683531250014514, 0.3010416670080866552, -0.7879004041258359514 ) ) ;
#199309 =( NAMED_UNIT ( * ) SI_UNIT ( $, .STERADIAN. ) SOLID_ANGLE_UNIT ( ) );
#199311 = VERTEX_POINT ( 'NONE', #186964 ) ;
#199312 = CARTESIAN_POINT ( 'NONE',  ( 2.708015267422092531, 2.165615165066101966, 0.7711511238016451886 ) ) ;
#199313 = CARTESIAN_POINT ( 'NONE',  ( 9.422553571817644524, 10.09532670998316384, 0.000000000000000000 ) ) ;
#199315 = CARTESIAN_POINT ( 'NONE',  ( 3.285556943750000070, -1.684374999522043836, 0.000000000000000000 ) ) ;
#199314 = CARTESIAN_POINT ( 'NONE',  ( 6.861835142292135536, 9.098836647464588978, 1.443375672974065660 ) ) ;
#199316 = SURFACE_SIDE_STYLE ('',( #70375 ) ) ;
#199317 = DIRECTION ( 'NONE',  ( 0.000000000000000000, 0.000000000000000000, -1.000000000000000000 ) ) ;
#199318 = EDGE_LOOP ( 'NONE', ( #196900, #117477, #58457, #78328 ) ) ;
#199319 = CARTESIAN_POINT ( 'NONE',  ( 0.000000000000000000, -0.4330127018922214077, 0.000000000000000000 ) ) ;
#199320 = CARTESIAN_POINT ( 'NONE',  ( 3.744317949583543470, 1.018843395500759197, -1.618198357137661469 ) ) ;
#199321 = LINE ( 'NONE', #1120, #158855 ) ;
#199322 = CARTESIAN_POINT ( 'NONE',  ( 5.666962058884261744, -1.561145826413099291, -0.7335915956277230254 ) ) ;
#199323 = CARTESIAN_POINT ( 'NONE',  ( 3.116422982138194353, 1.968445132739887748, 0.4370783100892047801 ) ) ;
#199324 =( BOUNDED_SURFACE ( )  B_SPLINE_SURFACE ( 3, 2, ( 
 ( #147632, #182233, #196376 ),
 ( #213650, #33857, #197422 ),
 ( #166000, #17585, #48016 ),
 ( #116244, #183306, #49064 ) ),
 .UNSPECIFIED., .F., .F., .T. ) 
 B_SPLINE_SURFACE_WITH_KNOTS ( ( 4, 4 ),
 ( 3, 3 ),
 ( -5.421010862427522170E-20, 9.170893477921754312E-05 ),
 ( 0.000000000000000000, 1.000000000000000000 ),
 .UNSPECIFIED. ) 
 GEOMETRIC_REPRESENTATION_ITEM ( )  RATIONAL_B_SPLINE_SURFACE ( (
 ( 1.000000000000000000, 0.6787756258918329344, 1.000000000000000000),
 ( 1.000000000000000000, 0.6894756946172844181, 1.000000000000000000),
 ( 1.000000000000000000, 0.6998898451712581847, 1.000000000000000000),
 ( 1.000000000000000000, 0.7100530722070645950, 1.000000000000000000) ) ) 
 REPRESENTATION_ITEM ( '' )  SURFACE ( )  );
#199325 = CARTESIAN_POINT ( 'NONE',  ( 5.151170688231202277, 1.131463054214848940, 2.000911673594136797 ) ) ;
#199326 = CARTESIAN_POINT ( 'NONE',  ( 0.000000000000000000, 4.446947634372835800, 0.000000000000000000 ) ) ;
#199327 = CARTESIAN_POINT ( 'NONE',  ( 0.4873205249028254027, -0.2742316277877173691, -2.189713876267186166 ) ) ;
#199328 = CARTESIAN_POINT ( 'NONE',  ( -5.668717624289589807, 5.786127781192186958, 0.7216878364870257245 ) ) ;
#199329 = CARTESIAN_POINT ( 'NONE',  ( 5.659369745216535463, 0.3440881560464129629, -1.735765479537496603 ) ) ;
#199330 = AXIS2_PLACEMENT_3D ( 'NONE', #79629, #28755, #145748 ) ;
#199332 = CARTESIAN_POINT ( 'NONE',  ( 1.623385997035782013, -2.157220310706788435, 0.7755101668525423708 ) ) ;
#199331 = CARTESIAN_POINT ( 'NONE',  ( 4.875038752565570732, 7.845239757038595663, -1.199719254218452047 ) ) ;
#199333 = CARTESIAN_POINT ( 'NONE',  ( 6.667912628260062036, -1.128459271250933149, 1.455361883854713767 ) ) ;
#199334 = CARTESIAN_POINT ( 'NONE',  ( 0.4153311931458959494, 3.850000000000006306, 0.5000000000000064393 ) ) ;
#199335 = CARTESIAN_POINT ( 'NONE',  ( 6.667925998804712151, -1.351855065013835455, 1.725503752137508284 ) ) ;
#199336 = CARTESIAN_POINT ( 'NONE',  ( -5.652823702255029836, 5.559658838911111900, -0.7998128361456362523 ) ) ;
#199337 = CARTESIAN_POINT ( 'NONE',  ( 0.6801582343749813520, 0.005208333674754095366, 1.178068619123793015 ) ) ;
#199338 = CARTESIAN_POINT ( 'NONE',  ( -11.86239285000045918, 13.88000000000000078, -1.812080536912752837 ) ) ;
#199339 = CARTESIAN_POINT ( 'NONE',  ( 6.461392557816405535, 1.719054114842766268, 1.153505076091146053 ) ) ;
#199340 = CARTESIAN_POINT ( 'NONE',  ( 0.8136858238772455287, -1.282993010278702606, -1.555696519147983459 ) ) ;
#199341 = CARTESIAN_POINT ( 'NONE',  ( -1.500000000000015099, -0.3395833326505143801, -0.8660254037844383745 ) ) ;
#199342 = CARTESIAN_POINT ( 'NONE',  ( 5.777940811437299651, 1.149350900142607879, 1.545952477797669200 ) ) ;
#199343 = CARTESIAN_POINT ( 'NONE',  ( 1.364683531249996529, 11.21354166700806232, 0.7879004041258405033 ) ) ;
#199344 = CARTESIAN_POINT ( 'NONE',  ( 1.846216761830053787, -1.455271069044868693, -1.678405531801461903 ) ) ;
#199345 = VERTEX_POINT ( 'NONE', #38596 ) ;
#199347 = LINE ( 'NONE', #149558, #201976 ) ;
#199346 = DIRECTION ( 'NONE',  ( 1.000000000000000000, -5.391474854832587087E-16, 0.000000000000000000 ) ) ;
#199348 = CARTESIAN_POINT ( 'NONE',  ( 7.183881110581282897E-16, 1.270118343195268951, -6.106226635438360972E-15 ) ) ;
#199349 = CARTESIAN_POINT ( 'NONE',  ( 9.511208455186636712, 11.05516360492796935, 1.199719254218453823 ) ) ;
#199350 = CARTESIAN_POINT ( 'NONE',  ( -11.33772463945036968, 13.40000000000000036, -3.600000000000002309 ) ) ;
#199351 = DIRECTION ( 'NONE',  ( -0.9999980456341538426, 0.000000000000000000, -0.001977050295967298574 ) ) ;
#199352 = CARTESIAN_POINT ( 'NONE',  ( 4.071615416877820692, -0.9979366678331093032, 1.425717084491331832 ) ) ;
#199353 = CARTESIAN_POINT ( 'NONE',  ( 2.277722772326017608, -1.903703133612335341, 0.4737097981617058862 ) ) ;
#199355 = CARTESIAN_POINT ( 'NONE',  ( -6.724481002698126098, 8.868313807946373473, -1.443375672974059665 ) ) ;
#199354 = CARTESIAN_POINT ( 'NONE',  ( 4.202137545231717120, 6.989912005157271402, 1.199719254218462483 ) ) ;
#199356 = PRESENTATION_STYLE_ASSIGNMENT (( #132287 ) ) ;
#199357 = CARTESIAN_POINT ( 'NONE',  ( 9.999301985278609806, 11.62460605670194447, 1.199719254218452047 ) ) ;
#199358 = AXIS2_PLACEMENT_3D ( 'NONE', #7671, #139851, #141998 ) ;
#199359 = CARTESIAN_POINT ( 'NONE',  ( 0.6079712386793578727, 0.6485803912554971573, -1.958102696269433673 ) ) ;
#199360 = CARTESIAN_POINT ( 'NONE',  ( -7.049349804101573191, 10.31165964050546258, -1.199719254218440723 ) ) ;
#199361 = CARTESIAN_POINT ( 'NONE',  ( -4.243338890952916387, 4.052909582307567149, -0.7216878364870207285 ) ) ;
#199362 = VECTOR ( 'NONE', #9123, 1000.000000000000000 ) ;
#199363 = CARTESIAN_POINT ( 'NONE',  ( 1.182923723612337774, -2.207873014618145113, -0.4935663919954368373 ) ) ;
#199364 = ORIENTED_EDGE ( 'NONE', *, *, #19444, .F. ) ;
#199365 = CARTESIAN_POINT ( 'NONE',  ( -1.402160292154681736E-14, 0.3687500006828169363, -1.732050807568870754 ) ) ;
#199366 = CARTESIAN_POINT ( 'NONE',  ( 2.266681450017640653, -1.708379500633325998, -0.7622673669660309237 ) ) ;
#199367 = CARTESIAN_POINT ( 'NONE',  ( 1.388881788488422586, -0.6239178774879328149, -1.618199924151533686 ) ) ;
#199368 = CARTESIAN_POINT ( 'NONE',  ( 5.407841436338867602, -0.9846607899807978681, -1.957994596084790206 ) ) ;
#199369 = CARTESIAN_POINT ( 'NONE',  ( 5.790114358714919973, -1.044397830967594976, 2.057800239056095659 ) ) ;
#199370 = CARTESIAN_POINT ( 'NONE',  ( 1.586866656640874451, -0.3012919939810917436, -2.038609575755165437 ) ) ;
#199371 = CARTESIAN_POINT ( 'NONE',  ( 3.943253339372253308, 0.6530871051511869529, -1.828966769512891277 ) ) ;
#199372 = CARTESIAN_POINT ( 'NONE',  ( -4.622967192135580383, 5.456178481322002227, 1.082531754730558626 ) ) ;
#199373 = CARTESIAN_POINT ( 'NONE',  ( 5.729731410239141454, -1.186140735684092284, -1.446405967604667886 ) ) ;
#199374 = CARTESIAN_POINT ( 'NONE',  ( 1.875000000000001776, 2.052068128417950721, -1.077215146005767577E-13 ) ) ;
#199375 = CARTESIAN_POINT ( 'NONE',  ( 4.143432174609324115, 7.404820066527033617, -0.7413545030366501809 ) ) ;
#199376 = CARTESIAN_POINT ( 'NONE',  ( 6.608749954595573683, 0.7741944705832277673, -1.861732896133998727 ) ) ;
#199377 = CARTESIAN_POINT ( 'NONE',  ( -1.360316468749990459, 1.890625000341386475, -2.428612866367529932E-14 ) ) ;
#199378 = CARTESIAN_POINT ( 'NONE',  ( 4.324842380567116784, 0.8596320953860696612, -1.824118450417112847 ) ) ;
#199379 = CARTESIAN_POINT ( 'NONE',  ( -3.104453987404963478, 5.605318171072321221, -1.082531754730549078 ) ) ;
#199380 = CARTESIAN_POINT ( 'NONE',  ( 9.921869487102386032, 10.46993591124128997, 0.000000000000000000 ) ) ;
#199381 = CARTESIAN_POINT ( 'NONE',  ( 3.054329744828568227, 6.785411478933790264, 0.000000000000000000 ) ) ;
#199383 = CARTESIAN_POINT ( 'NONE',  ( -4.171720451616118375, 7.856123832628136405, 0.2051403462137192935 ) ) ;
#199382 = CARTESIAN_POINT ( 'NONE',  ( 2.490611698265518648, -0.3118145247060916114, -1.798701865878708839 ) ) ;
#199384 = CARTESIAN_POINT ( 'NONE',  ( -6.120580001926503755, 6.105374521861167914, -0.7998128361456362523 ) ) ;
#199385 = CARTESIAN_POINT ( 'NONE',  ( -0.1296875068448159751, 0.001480089298542403009, -1.826395826379861864 ) ) ;
#199386 = CARTESIAN_POINT ( 'NONE',  ( -1.806654366501805775, 2.518449987798942136, 2.500000000000000444 ) ) ;
#199387 = ORIENTED_EDGE ( 'NONE', *, *, #133578, .F. ) ;
#199388 = CARTESIAN_POINT ( 'NONE',  ( -6.766928066552171828, 7.067373297165212342, 0.7216878364870317197 ) ) ;
#199389 = CARTESIAN_POINT ( 'NONE',  ( -2.442440228756222353, 6.001264033524212671, -0.7998128361456281477 ) ) ;
#199390 = CARTESIAN_POINT ( 'NONE',  ( -7.862839020921525091, 11.26073039346208660, -1.199719254218446718 ) ) ;
#199391 = CARTESIAN_POINT ( 'NONE',  ( 6.393224328948585722, -0.1011241736039915490, -2.017280362314947340 ) ) ;
#199393 = VERTEX_POINT ( 'NONE', #98825 ) ;
#199392 = CARTESIAN_POINT ( 'NONE',  ( 0.4344390223590781641, -1.137927343861804053, -1.789123301873453364 ) ) ;
#199394 = CARTESIAN_POINT ( 'NONE',  ( -5.237192476628793614, 9.332084666034067055, 0.7998128361456291469 ) ) ;
#199395 = CARTESIAN_POINT ( 'NONE',  ( 6.003563092752934871, 5.898578451166879510, 0.7998128361456341429 ) ) ;
#199396 = CARTESIAN_POINT ( 'NONE',  ( 5.682513945847499137, -2.010110750271485447, -0.4539000206328601683 ) ) ;
#199397 = CARTESIAN_POINT ( 'NONE',  ( 4.922500090287251773, -1.427935867408920645, -1.423962988533589158 ) ) ;
#199398 = ORIENTED_EDGE ( 'NONE', *, *, #31247, .F. ) ;
#199399 = CARTESIAN_POINT ( 'NONE',  ( -4.197870329853007121, 3.573279226090508409, 2.499999999999998224 ) ) ;
#199400 = CARTESIAN_POINT ( 'NONE',  ( -1.523611765266693174, 0.5000000000000001110, 1.789163823896770200 ) ) ;
#199401 = VECTOR ( 'NONE', #84706, 1000.000000000000000 ) ;
#199404 = ORIENTED_EDGE ( 'NONE', *, *, #156764, .T. ) ;
#199403 = CARTESIAN_POINT ( 'NONE',  ( -1.734723475976807094E-15, 2.999999999999988898, -6.938893903907228378E-15 ) ) ;
#199402 = CARTESIAN_POINT ( 'NONE',  ( -6.740338644649361832, 7.892758502626242567, -1.199719254218452047 ) ) ;
#199405 = CARTESIAN_POINT ( 'NONE',  ( 4.774898309648160755, 8.276035162536045320, 0.8191430224755236189 ) ) ;
#199406 = B_SPLINE_CURVE_WITH_KNOTS ( 'NONE', 3,
 ( #95391, #62850, #177686, #194989, #63919, #79100 ),
 .UNSPECIFIED., .F., .F.,
 ( 4, 2, 4 ),
 ( 0.001877801214402442754, 0.002190719108449961511, 0.002503637002497480051 ),
 .UNSPECIFIED. ) ;
#199407 = CARTESIAN_POINT ( 'NONE',  ( 5.114611164699836010, 0.6351010243071940620, -1.913510948406547563 ) ) ;
#199408 = CARTESIAN_POINT ( 'NONE',  ( 5.103375755629981469, -1.831930319445294719, 0.1838923505294575433 ) ) ;
#199409 = CARTESIAN_POINT ( 'NONE',  ( -0.02338929933911031503, 1.420967854922173368, -1.971839201816010911 ) ) ;
#199410 = CARTESIAN_POINT ( 'NONE',  ( 2.860362167425280600, 2.296499369387979606, -0.2270692390979132391 ) ) ;
#199411 = CARTESIAN_POINT ( 'NONE',  ( 6.964048179274811012, 8.153752959689313684, 1.199719254218452047 ) ) ;
#199412 = CARTESIAN_POINT ( 'NONE',  ( 5.167319818800252484, 0.2175342549677051207, -2.150644138106901693 ) ) ;
#199413 = CARTESIAN_POINT ( 'NONE',  ( 8.294891053462476904, 8.571794405328034827, 1.040834085586084257E-14 ) ) ;
#199414 = CARTESIAN_POINT ( 'NONE',  ( 0.3627036604622800864, 0.1893831815216796277, -1.932784825206189661 ) ) ;
#199415 = EDGE_CURVE ( 'NONE', #179126, #23953, #76415, .T. ) ;
#199416 = CARTESIAN_POINT ( 'NONE',  ( -4.517891501851816649, 6.293959390292322986, -1.599625672291256295 ) ) ;
#199417 = CONICAL_SURFACE ( 'NONE', #81925, 2.000000000000006217, 0.01725463330310792257 ) ;
#199418 = EDGE_CURVE ( 'NONE', #57689, #20233, #203865, .T. ) ;
#199419 = CARTESIAN_POINT ( 'NONE',  ( -9.393959922460844325, 15.45881633117845055, -7.466876303545585181 ) ) ;
#199420 = CARTESIAN_POINT ( 'NONE',  ( -5.061990249855848667, 6.999017606288844284, -1.599625672291271394 ) ) ;
#199421 = CARTESIAN_POINT ( 'NONE',  ( 3.836663719693265584, 0.2738035037005565053, 1.850374562403465983 ) ) ;
#199424 = CARTESIAN_POINT ( 'NONE',  ( -5.250750630242457362, 9.347902511916677426, 0.000000000000000000 ) ) ;
#199423 = CARTESIAN_POINT ( 'NONE',  ( 1.499999999999987121, -0.7145833326505161009, 0.8660254037844524744 ) ) ;
#199422 = CARTESIAN_POINT ( 'NONE',  ( 1.599720133015330337, 1.321132142916726204, 1.382909031182079307 ) ) ;
#199425 = CARTESIAN_POINT ( 'NONE',  ( 2.473496279428960776, 0.1070396533628548558, -2.204406164007084445 ) ) ;
#199426 = CARTESIAN_POINT ( 'NONE',  ( -11.94654170777226021, 9.948256738410641731, 1.134972293687618539 ) ) ;
#199427 = CARTESIAN_POINT ( 'NONE',  ( 5.542585869888291938, 5.360771691158120689, -0.7998128361456211532 ) ) ;
#199428 = CARTESIAN_POINT ( 'NONE',  ( 6.170369307550816806, 9.252495721234380355, 1.082531754730549967 ) ) ;
#199429 = CARTESIAN_POINT ( 'NONE',  ( -4.569261463005423352, 5.289558780716470565, -1.199719254218446718 ) ) ;
#199430 = MECHANICAL_DESIGN_GEOMETRIC_PRESENTATION_REPRESENTATION (  '', ( #140729 ), #189092 ) ;
#199431 = CARTESIAN_POINT ( 'NONE',  ( -6.089020385868856522, 9.157588645938716354, -1.082531754730549967 ) ) ;
#199432 = CARTESIAN_POINT ( 'NONE',  ( 0.2804619692761011751, -1.911105013696552168, -0.4832259537779006742 ) ) ;
#199433 = CARTESIAN_POINT ( 'NONE',  ( 6.727182134110239353, -0.007837387828812587484, 2.289081727344749684 ) ) ;
#199434 = CARTESIAN_POINT ( 'NONE',  ( 1.293326634533353170, -1.775083115552608559, 0.8357255594537355003 ) ) ;
#199435 = CARTESIAN_POINT ( 'NONE',  ( 4.346570391463054683, -2.039393746373055372, -0.3077390332135512829 ) ) ;
#199436 = CARTESIAN_POINT ( 'NONE',  ( 4.799223189557548785, 7.582548906917042864, -1.082531754730549078 ) ) ;
#199437 = CARTESIAN_POINT ( 'NONE',  ( 6.099189001301251523, 8.209082816308541197, 1.599625672291268286 ) ) ;
#199438 = ORIENTED_EDGE ( 'NONE', *, *, #155474, .F. ) ;
#199439 = CARTESIAN_POINT ( 'NONE',  ( 7.741342523278698096, 10.05465224862374285, 1.443375672974076540 ) ) ;
#199440 = CARTESIAN_POINT ( 'NONE',  ( -0.6823417656249969321, 4.530208333674755394, -1.181850606188749264 ) ) ;
#199441 = CARTESIAN_POINT ( 'NONE',  ( -4.948193499308641385, 4.885107685699183300, 0.5067794099899626259 ) ) ;
#199442 = CARTESIAN_POINT ( 'NONE',  ( 2.995988758495615745, 6.439144618312774959, -0.7216878364870267237 ) ) ;
#199443 = CARTESIAN_POINT ( 'NONE',  ( 6.637192348400761333, -0.09982221633967082453, -2.168999452382541993 ) ) ;
#199445 = CARTESIAN_POINT ( 'NONE',  ( 6.462460624273299814, -1.686435539877573220, -0.7394478613861471539 ) ) ;
#199444 = CARTESIAN_POINT ( 'NONE',  ( 9.496893780459336298, -9.200036371099118426, -0.2463816395386141112 ) ) ;
#199446 = CARTESIAN_POINT ( 'NONE',  ( 5.568382567296971786, 6.179660279684793700, -0.8958173718428998900 ) ) ;
#199447 = DIRECTION ( 'NONE',  ( 0.7592566023653044560, 0.6507913734559596097, 0.000000000000000000 ) ) ;
#199448 = CARTESIAN_POINT ( 'NONE',  ( 0.9834252619641962179, 1.251819791611600285, 1.390119989509101650 ) ) ;
#199449 = CARTESIAN_POINT ( 'NONE',  ( -6.098685391867989303, 6.020399689055939696, 0.3646554611961040360 ) ) ;
#199450 = CARTESIAN_POINT ( 'NONE',  ( -0.02244404828157658613, -0.004869073801674199918, -2.189079685368473527 ) ) ;
#199451 = CARTESIAN_POINT ( 'NONE',  ( 6.038137670975392446, 7.156622065392123311, -1.170913047369964710 ) ) ;
#199452 = CARTESIAN_POINT ( 'NONE',  ( 0.6823417656249917140, 4.905208333674755394, 1.181850606188765695 ) ) ;
#199453 = CARTESIAN_POINT ( 'NONE',  ( 1.031728963041964153, -1.865498905729731316, 0.4196304693004496156 ) ) ;
#199454 = CARTESIAN_POINT ( 'NONE',  ( 3.414700241993049001, 1.599697164860384380, 0.7574896018788888075 ) ) ;
#199455 = CARTESIAN_POINT ( 'NONE',  ( 0.8383554657987003500, 1.138622818284718008, -1.536203910471350298 ) ) ;
#199457 = CARTESIAN_POINT ( 'NONE',  ( 3.866719127221716512, -0.1911932653220274059, -1.906053554140298756 ) ) ;
#199456 = CARTESIAN_POINT ( 'NONE',  ( 2.194551752856947591, -3.163290167409173570, -2.543720345301475838 ) ) ;
#199458 = CARTESIAN_POINT ( 'NONE',  ( 0.7499999999999885647, -1.016666666666644847, 1.299038105676657340 ) ) ;
#199459 = CARTESIAN_POINT ( 'NONE',  ( 5.600048008112708864, 0.7998006467024108002, -1.800045223161725660 ) ) ;
#199460 = CARTESIAN_POINT ( 'NONE',  ( 1.178162429063234207, 2.088287186665960693, -0.3679680078583212333 ) ) ;
#199461 = CARTESIAN_POINT ( 'NONE',  ( 6.720655732516625847, 7.629137130509076492, 2.426260288887295058 ) ) ;
#199462 = CARTESIAN_POINT ( 'NONE',  ( 3.414787578387419309, 1.690673485743508619, 0.8009127983473337542 ) ) ;
#199464 = ORIENTED_EDGE ( 'NONE', *, *, #36958, .T. ) ;
#199463 = CARTESIAN_POINT ( 'NONE',  ( 0.8908993799596062191, 1.611356928563783208, -0.8583080905386344384 ) ) ;
#199466 = DIRECTION ( 'NONE',  ( 0.000000000000000000, 0.000000000000000000, -1.000000000000000000 ) ) ;
#199465 = CARTESIAN_POINT ( 'NONE',  ( 3.422699507934781060, 1.400174360247144589, -1.705827624971032686 ) ) ;
#199467 = CARTESIAN_POINT ( 'NONE',  ( -1.364683531250010295, 5.342708333674750953, 0.7879004041258379498 ) ) ;
#199468 = CARTESIAN_POINT ( 'NONE',  ( 0.4673242579315056155, 1.793762616230053508, 1.018268840648499207 ) ) ;
#199469 = CARTESIAN_POINT ( 'NONE',  ( 7.800018446563675489, 7.994443030612759848, -0.7998128361456281477 ) ) ;
#199470 = CARTESIAN_POINT ( 'NONE',  ( -7.641992139597101108, 12.06740792950531649, 0.7998128361456481317 ) ) ;
#199471 = CARTESIAN_POINT ( 'NONE',  ( -0.2226028112648442414, 15.44694767462292440, -11.95586206701304199 ) ) ;
#199472 = CARTESIAN_POINT ( 'NONE',  ( -3.469473121595833653, -0.004037186406451471338, -0.1333067274223260212 ) ) ;
#199473 = CARTESIAN_POINT ( 'NONE',  ( 8.018721507839716267, 8.319872945426633137, -0.7998128361456341429 ) ) ;
#199474 = ORIENTED_EDGE ( 'NONE', *, *, #137412, .F. ) ;
#199475 = CARTESIAN_POINT ( 'NONE',  ( 4.721179655770254335, -1.847879960204744432, -0.9338546512941485744 ) ) ;
#199476 = CARTESIAN_POINT ( 'NONE',  ( -0.7499999999999972244, 4.108333333333360038, -1.299038105676652011 ) ) ;
#199477 = CARTESIAN_POINT ( 'NONE',  ( 1.827627302340195437, -2.036028831988645926, 0.7264203155534704193 ) ) ;
#199478 = CARTESIAN_POINT ( 'NONE',  ( -5.122256578951685846, 7.813849795838854639, -1.152996464563345924 ) ) ;
#199479 = CARTESIAN_POINT ( 'NONE',  ( 2.244791279253912197, 1.959548689066059168, 0.4886446307589187854 ) ) ;
#199480 = DIRECTION ( 'NONE',  ( -0.000000000000000000, 1.000000000000000000, -0.000000000000000000 ) ) ;
#199481 = EDGE_CURVE ( 'NONE', #124676, #30003, #103396, .T. ) ;
#199483 = CARTESIAN_POINT ( 'NONE',  ( 7.104109303880752790, 11.23195192126214970, -0.7216878364870267237 ) ) ;
#199482 = CARTESIAN_POINT ( 'NONE',  ( 3.475000000000000533, -2.974999999999998312, 0.000000000000000000 ) ) ;
#199484 = CARTESIAN_POINT ( 'NONE',  ( 1.876272499184441500, -0.7121508056591638880, 0.8723429728170000175 ) ) ;
#199485 = CARTESIAN_POINT ( 'NONE',  ( 0.3039231887648624619, -1.082844287645868375, -1.700959134490941160 ) ) ;
#199486 = DIRECTION ( 'NONE',  ( -0.6507913734559640506, -0.7592566023653004592, 0.000000000000000000 ) ) ;
#199487 = CARTESIAN_POINT ( 'NONE',  ( 5.003566749295822014, -2.181051155298455058, 0.2145382695054529609 ) ) ;
#199489 = VECTOR ( 'NONE', #20387, 1000.000000000000114 ) ;
#199488 = CARTESIAN_POINT ( 'NONE',  ( 1.499999999999990896, 3.806250000682819046, 1.214306433183764966E-14 ) ) ;
#199490 = CARTESIAN_POINT ( 'NONE',  ( 3.638835171272115421, 1.817485770107383436, 0.5952672491930725007 ) ) ;
#199491 = CARTESIAN_POINT ( 'NONE',  ( -5.037017762676898158, 5.835274463666530131, -1.199719254218446718 ) ) ;
#199492 = CARTESIAN_POINT ( 'NONE',  ( 5.138177029454852551, 5.096887410559856946, 0.7216878364870317197 ) ) ;
#199494 = CARTESIAN_POINT ( 'NONE',  ( 1.616814774554303780, 0.2004563524992293566, 2.006445175307514095 ) ) ;
#199493 = DIRECTION ( 'NONE',  ( 0.000000000000000000, -1.000000000000000000, 0.000000000000000000 ) ) ;
#199495 = CARTESIAN_POINT ( 'NONE',  ( 1.364683531249997417, 11.79687500034139802, 2.602085213965210642E-15 ) ) ;
#199497 = CARTESIAN_POINT ( 'NONE',  ( -5.167592825464113915, 6.057888380243431570, 1.199719254218452935 ) ) ;
#199496 = CARTESIAN_POINT ( 'NONE',  ( 0.1524363970008953684, 0.8851206712186098224, 2.114804356544320640 ) ) ;
#199498 = CARTESIAN_POINT ( 'NONE',  ( 4.629763539376270387, -1.062658783613348534, -1.358442396976522248 ) ) ;
#199499 = CARTESIAN_POINT ( 'NONE',  ( -0.1405533004718495238, 2.888985375434447889, -2.209311699518405447 ) ) ;
#199500 = CARTESIAN_POINT ( 'NONE',  ( 3.161022370280501814, 6.839609865302569425, 0.000000000000000000 ) ) ;
#199501 = DIRECTION ( 'NONE',  ( 0.000000000000000000, 0.000000000000000000, -1.000000000000000000 ) ) ;
#199502 = CARTESIAN_POINT ( 'NONE',  ( 0.9066075625437097774, 0.5660373911110065936, 1.878450800843839419 ) ) ;
#199503 = EDGE_CURVE ( 'NONE', #63041, #213109, #179003, .T. ) ;
#199504 = CARTESIAN_POINT ( 'NONE',  ( 11.33772463945036790, 10.19999999999999929, -3.600000000000000977 ) ) ;
#199505 = CARTESIAN_POINT ( 'NONE',  ( 3.818592820543298405, 7.606775390609172405, -0.7998128361456221525 ) ) ;
#199506 = CARTESIAN_POINT ( 'NONE',  ( 0.07536363704233051131, 7.629137130509080045, -2.744199452819145790 ) ) ;
#199507 = ORIENTED_EDGE ( 'NONE', *, *, #25664, .F. ) ;
#199508 = CARTESIAN_POINT ( 'NONE',  ( 3.511198596259284876, 6.271927390929313617, -1.052294140492317842 ) ) ;
#199509 = ORIENTED_EDGE ( 'NONE', *, *, #183561, .T. ) ;
#199510 = CARTESIAN_POINT ( 'NONE',  ( 3.562975276761202181, -1.478990456472810910, 1.045639718295880094 ) ) ;
#199511 = VERTEX_POINT ( 'NONE', #26600 ) ;
#199512 = CARTESIAN_POINT ( 'NONE',  ( 7.517069824134078537, 7.734612647770044092, 0.000000000000000000 ) ) ;
#199513 = CARTESIAN_POINT ( 'NONE',  ( -5.414683845018970487, 6.133484104433280848, 1.108540189933695297 ) ) ;
#199514 = CARTESIAN_POINT ( 'NONE',  ( 4.371601898205011771, 0.3924986647133471007, -1.768265068870542800 ) ) ;
#199515 = CARTESIAN_POINT ( 'NONE',  ( 6.116136693096175136, 9.189224337703940648, -1.082531754730548412 ) ) ;
#199516 = FACE_OUTER_BOUND ( 'NONE', #26651, .T. ) ;
#199517 = CARTESIAN_POINT ( 'NONE',  ( 5.874728247277303694, 5.987702652136856152, -0.2291304890473921385 ) ) ;
#199518 = ORIENTED_EDGE ( 'NONE', *, *, #163609, .F. ) ;
#199519 = AXIS2_PLACEMENT_3D ( 'NONE', #40904, #92861, #107010 ) ;
#199521 = CARTESIAN_POINT ( 'NONE',  ( 8.866142388332804103, 12.43125098877526113, -1.199719254218446718 ) ) ;
#199520 = CARTESIAN_POINT ( 'NONE',  ( 6.109776933011930922, 0.5395433811187456685, -1.781096067677762962 ) ) ;
#199522 = CARTESIAN_POINT ( 'NONE',  ( 4.147977739690055898, 0.9062469702798245930, 1.687694244345463224 ) ) ;
#199523 = CARTESIAN_POINT ( 'NONE',  ( 1.500000000000039524, 7.193113254731344774, 10.88798745763943465 ) ) ;
#199524 = CARTESIAN_POINT ( 'NONE',  ( -11.58081452147585289, 6.132683923455591213, -5.154482061493088629 ) ) ;
#199525 = CARTESIAN_POINT ( 'NONE',  ( 9.499685679921592296, -9.917013740047293524, -0.07729799388535055216 ) ) ;
#199526 = SURFACE_STYLE_FILL_AREA ( #66314 ) ;
#199527 = CARTESIAN_POINT ( 'NONE',  ( 5.178851490740193242, 8.025448591630130579, 1.082531754730558626 ) ) ;
#199528 = EDGE_CURVE ( 'NONE', #111937, #29485, #9291, .T. ) ;
#199529 = CARTESIAN_POINT ( 'NONE',  ( -9.544576954340667996, 11.19805653722800365, 1.082531754730558626 ) ) ;
#199530 = CARTESIAN_POINT ( 'NONE',  ( 0.7784641540938312954, -1.199969256800371697, 1.797863220954009744 ) ) ;
#199531 = CARTESIAN_POINT ( 'NONE',  ( -4.288121723672178476, 8.224835454251337552, -0.7998128361456362523 ) ) ;
#199532 = CARTESIAN_POINT ( 'NONE',  ( 5.285699784481295183, 7.260012063351913625, 1.599625672291268286 ) ) ;
#199533 = CARTESIAN_POINT ( 'NONE',  ( 0.4986989427119004059, 1.520756344202650601, -1.009667857431728599 ) ) ;
#199534 = CARTESIAN_POINT ( 'NONE',  ( -3.684065054611367351, 5.321161868511784299, -1.599625672291256295 ) ) ;
#199535 = ADVANCED_FACE ( 'NONE', ( #142526 ), #210025, .T. ) ;
#199536 = CARTESIAN_POINT ( 'NONE',  ( 3.188313505853744179, -1.798300186086329688, -0.3134973320952222364 ) ) ;
#199537 = CARTESIAN_POINT ( 'NONE',  ( -3.642672431166784186, 3.097590952613293869, 2.447572309174936844 ) ) ;
#199538 = CARTESIAN_POINT ( 'NONE',  ( 1.705181254219298115, 1.662258477346746588, -0.9455041445245655485 ) ) ;
#199539 = ORIENTED_EDGE ( 'NONE', *, *, #174092, .T. ) ;
#199540 = CARTESIAN_POINT ( 'NONE',  ( 2.277737068081890914, -1.911112558508936354, 0.4757300241334978530 ) ) ;
#199541 = CARTESIAN_POINT ( 'NONE',  ( 5.319850173407331795, 1.153525655430783337, -1.562239502177962480 ) ) ;
#199542 = CARTESIAN_POINT ( 'NONE',  ( -8.100070429521727178, 8.414780020722290033, 0.7998128361456341429 ) ) ;
#199544 = CARTESIAN_POINT ( 'NONE',  ( 4.008146050417991546, -0.8085630067716749192, 1.960596031080278356 ) ) ;
#199543 = CARTESIAN_POINT ( 'NONE',  ( 2.898410978271408922, 6.603506251283770112, -0.7998128361456362523 ) ) ;
#199545 = CARTESIAN_POINT ( 'NONE',  ( -4.492294583947676223, 8.028511867738769681, -2.499999999999999556 ) ) ;
#199546 = CARTESIAN_POINT ( 'NONE',  ( 10.09812548408005384, 10.67556790771522124, -0.7998128361456281477 ) ) ;
#199547 = CARTESIAN_POINT ( 'NONE',  ( 5.728356146706021335, 6.265246534282280066, 1.050634566151719129 ) ) ;
#199548 = B_SPLINE_CURVE_WITH_KNOTS ( 'NONE', 3,
 ( #107610, #23063, #56664, #5732, #122828, #70740, #53451 ),
 .UNSPECIFIED., .F., .F.,
 ( 4, 3, 4 ),
 ( 0.0001126021370636924715, 0.0006031550062628982618, 0.002006790698585274747 ),
 .UNSPECIFIED. ) ;
#199549 = CARTESIAN_POINT ( 'NONE',  ( -7.439168848973998216, -6.893137084989842123, -8.103009739377998955 ) ) ;
#199550 = CARTESIAN_POINT ( 'NONE',  ( 1.364683531249997417, 13.23437500034139980, 2.602085213965210642E-15 ) ) ;
#199551 = CARTESIAN_POINT ( 'NONE',  ( 3.715816618597135523, 6.492813934075403637, -1.199719254218453823 ) ) ;
#199552 = CARTESIAN_POINT ( 'NONE',  ( 6.723917837734620484, 6.809268663637336516, 0.000000000000000000 ) ) ;
#199553 = CARTESIAN_POINT ( 'NONE',  ( 5.162654993523497993, -1.319871331358621669, 1.261628347558927166 ) ) ;
#199554 = FACE_OUTER_BOUND ( 'NONE', #213892, .T. ) ;
#199555 = CARTESIAN_POINT ( 'NONE',  ( -9.164948653158003111, 9.794787638213568570, -0.7216878364870267237 ) ) ;
#199556 = AXIS2_PLACEMENT_3D ( 'NONE', #50616, #116741, #66826 ) ;
#199557 = CARTESIAN_POINT ( 'NONE',  ( -5.889893629278568632, 7.264407438959931795, 1.268144897863663356 ) ) ;
#199558 = DIRECTION ( 'NONE',  ( -0.000000000000000000, -1.000000000000000000, -0.000000000000000000 ) ) ;
#199559 = CARTESIAN_POINT ( 'NONE',  ( 5.682452175617663137, -1.825344843996518529, -0.4084625512627630406 ) ) ;
#199560 = CARTESIAN_POINT ( 'NONE',  ( 8.125414133291656071, 8.374071331795406081, -0.7998128361456291469 ) ) ;
#199561 = CARTESIAN_POINT ( 'NONE',  ( -3.899941742225307983, 7.701682465904834629, 0.7998128361456341429 ) ) ;
#199562 = PRESENTATION_LAYER_ASSIGNMENT (  '', '', ( #50847 ) ) ;
#199563 = CARTESIAN_POINT ( 'NONE',  ( 4.192495815123822744, 5.914331089109666983, -1.599625672291255185 ) ) ;
#199564 = CARTESIAN_POINT ( 'NONE',  ( -1.364683531250014514, 10.65104166700806942, -0.7879004041258335089 ) ) ;
#199565 = CARTESIAN_POINT ( 'NONE',  ( -6.196239896645333367, 7.187700286629718605, -1.199719254218446718 ) ) ;
#199566 = CARTESIAN_POINT ( 'NONE',  ( 2.361091307074211887, 5.906356958228550447, 0.7998128361456462443 ) ) ;
#199567 = CARTESIAN_POINT ( 'NONE',  ( -4.624739795592948788, 5.528522862014106920, -1.082531754730549967 ) ) ;
#199568 = CARTESIAN_POINT ( 'NONE',  ( 6.438351068470751670, -1.168633322568404243, 1.829565972870864865 ) ) ;
#199569 = CARTESIAN_POINT ( 'NONE',  ( 0.6853559850922884555, 1.733544695350475395, 1.215283626663875793 ) ) ;
#199570 = CARTESIAN_POINT ( 'NONE',  ( 10.07778825365955733, 10.65184113889131012, -0.7998128361456281477 ) ) ;
#199571 = CARTESIAN_POINT ( 'NONE',  ( -4.046711340875996044, 3.801480273782240626, 2.499999999999999556 ) ) ;
#199572 = CARTESIAN_POINT ( 'NONE',  ( 6.174686067066745387, 1.394736081427111030, -1.530067588329916850 ) ) ;
#199574 = CARTESIAN_POINT ( 'NONE',  ( 4.002182886544830787, 7.824783036946191039, -0.1358892651178236766 ) ) ;
#199573 = CARTESIAN_POINT ( 'NONE',  ( 1.997363575765517485, -1.840834563946552649, 0.04656924640939614363 ) ) ;
#199575 = CARTESIAN_POINT ( 'NONE',  ( 4.189106276942576201, 7.831115056500907556, 1.040834085586084257E-14 ) ) ;
#199577 = CARTESIAN_POINT ( 'NONE',  ( 0.1100172516615156165, 7.047065462482140497, 3.945011421259203566 ) ) ;
#199576 = CARTESIAN_POINT ( 'NONE',  ( 1.737500000000001155, -3.033333333333332327, 3.009438278150922130 ) ) ;
#199578 = CARTESIAN_POINT ( 'NONE',  ( 1.500361222516993331, -0.8285058210528316591, -2.137470567302256708 ) ) ;
#199580 = DIRECTION ( 'NONE',  ( 0.1510067114093955887, 0.000000000000000000, -0.9885327375000383388 ) ) ;
#199579 = CARTESIAN_POINT ( 'NONE',  ( -5.763039058787667201, 7.049721345481766654, 2.499999999999999556 ) ) ;
#199581 = STYLED_ITEM ( 'NONE', ( #18182 ), #146262 ) ;
#199582 = ORIENTED_EDGE ( 'NONE', *, *, #188975, .T. ) ;
#199583 = CARTESIAN_POINT ( 'NONE',  ( 7.076992996209058973, 11.20031622897851165, 1.040834085586084257E-14 ) ) ;
#199584 = CARTESIAN_POINT ( 'NONE',  ( 0.9143154035033382865, -2.013376230895477903, 0.004183558276700528357 ) ) ;
#199585 = CARTESIAN_POINT ( 'NONE',  ( 1.498799732657706718, 0.3773721054241683248, 1.924948185394937283 ) ) ;
#199586 = CARTESIAN_POINT ( 'NONE',  ( 6.509000000000010999, 0.004788705324892603143, 2.000274819378269786 ) ) ;
#199588 = CARTESIAN_POINT ( 'NONE',  ( -10.19200560444942560, 4.477620260464512114, -5.707107691925500603 ) ) ;
#199587 = CARTESIAN_POINT ( 'NONE',  ( -8.040148788103921973, 9.338927326664741457, 1.199719254218462483 ) ) ;
#199589 = CARTESIAN_POINT ( 'NONE',  ( -9.367496996292747014, 15.51845925588232333, -7.500000001629758550 ) ) ;
#199591 = CARTESIAN_POINT ( 'NONE',  ( 1.902845806929494232, 1.469307612142495723, 0.9863148084752764166 ) ) ;
#199590 = CARTESIAN_POINT ( 'NONE',  ( 3.855486427358902013, 2.074851370404519280, -0.2558628111340756628 ) ) ;
#199592 = DIRECTION ( 'NONE',  ( -1.000000000000000000, 0.000000000000000000, 0.000000000000000000 ) ) ;
#199594 = CARTESIAN_POINT ( 'NONE',  ( 5.050848094970262991, -1.934468200101526758, -1.229489151810001735 ) ) ;
#199593 = CARTESIAN_POINT ( 'NONE',  ( -0.6125000000000140332, 2.041666666666650087, 1.060881119635936232 ) ) ;
#199595 = CARTESIAN_POINT ( 'NONE',  ( 3.626658729539467441, -1.607292185769314097, 0.6678421186538037180 ) ) ;
#199596 = CARTESIAN_POINT ( 'NONE',  ( 10.56588178375152864, 11.22128359066528169, -0.7998128361456281477 ) ) ;
#199597 = CARTESIAN_POINT ( 'NONE',  ( 4.980641328173811999, 6.904110530993182948, 1.599625672291269396 ) ) ;
#199598 = CARTESIAN_POINT ( 'NONE',  ( 3.831122626782780927, -1.165689738437695189, 1.283648893705439331 ) ) ;
#199599 = CARTESIAN_POINT ( 'NONE',  ( 3.192005314569335894, -1.456082124923337995, -1.610717807342199048 ) ) ;
#199600 = CARTESIAN_POINT ( 'NONE',  ( 5.671388329218120639, 5.511041227042920099, 1.040834085586084257E-14 ) ) ;
#199601 = ADVANCED_FACE ( 'NONE', ( #14342 ), #59281, .T. ) ;
#199602 = CARTESIAN_POINT ( 'NONE',  ( 4.909388789075159742, -1.913262893431907141, 0.6371506334161003426 ) ) ;
#199603 = CARTESIAN_POINT ( 'NONE',  ( 6.750000000000005329, 3.320568569168067974, 2.600000000000000533 ) ) ;
#199604 = CARTESIAN_POINT ( 'NONE',  ( -1.500000000000011324, 4.702083334016148974, 0.8660254037844403729 ) ) ;
#199605 = CARTESIAN_POINT ( 'NONE',  ( 2.379798427543390105, 1.183398162072072823, 1.519983715915488531 ) ) ;
#199606 = CARTESIAN_POINT ( 'NONE',  ( -6.009258394948636914E-15, 8.968750000682799595, -1.732050807568875195 ) ) ;
#199607 = CARTESIAN_POINT ( 'NONE',  ( 6.222901868277154414, 1.646860780578407013, -1.490944794436506626 ) ) ;
#199608 = ORIENTED_EDGE ( 'NONE', *, *, #58273, .T. ) ;
#199609 = CARTESIAN_POINT ( 'NONE',  ( -0.2106854629475425067, 4.089057744811007922, -2.552070079120628776 ) ) ;
#199610 = CARTESIAN_POINT ( 'NONE',  ( -1.500000000000001332, 1.400000000000019229, 0.000000000000000000 ) ) ;
#199611 = CARTESIAN_POINT ( 'NONE',  ( 5.276094334012385367, 9.307193822989793475, 1.040834085586084257E-14 ) ) ;
#199612 = CARTESIAN_POINT ( 'NONE',  ( 3.782361668088245921, 6.396210465202840645, -1.082531754730548412 ) ) ;
#199613 = CARTESIAN_POINT ( 'NONE',  ( 3.285556943750000514, -2.063541666188710266, 1.896917185911906722 ) ) ;
#199614 = CARTESIAN_POINT ( 'NONE',  ( -1.499999999999997780, 4.900000000000022560, 1.214306433183765124E-14 ) ) ;
#199615 = CARTESIAN_POINT ( 'NONE',  ( 7.619319141200051604, 11.83303006480134911, 0.7216878364870438212 ) ) ;
#199616 = DIRECTION ( 'NONE',  ( -0.000000000000000000, -1.000000000000000000, -0.000000000000000000 ) ) ;
#199617 = CARTESIAN_POINT ( 'NONE',  ( 6.749321564901560322, -1.811022791033944257, -1.355814775124731808 ) ) ;
#199618 = CARTESIAN_POINT ( 'NONE',  ( 6.052789233858158369, 6.026285292448116948, 0.000000000000000000 ) ) ;
#199619 = CARTESIAN_POINT ( 'NONE',  ( -2.875737979874388284, 6.369128386579808954, -0.7216878364870458196 ) ) ;
#199620 = CARTESIAN_POINT ( 'NONE',  ( 3.965324414628346172, 1.767556376804786611, 1.063002922270523953 ) ) ;
#199621 = CARTESIAN_POINT ( 'NONE',  ( -5.037017762676898158, 5.835274463666530131, -1.199719254218446718 ) ) ;
#199622 = CARTESIAN_POINT ( 'NONE',  ( -0.7499999999999972244, 4.389583334016150751, -1.299038105676652899 ) ) ;
#199623 = CARTESIAN_POINT ( 'NONE',  ( -1.364683531250014514, -0.01145833299191483488, -0.7879004041258359514 ) ) ;
#199624 = CARTESIAN_POINT ( 'NONE',  ( 5.378141472655761923, -1.040010688794581029, 1.554561134376866161 ) ) ;
#199625 = CARTESIAN_POINT ( 'NONE',  ( 4.518016650454199201, -1.583040169018738785, 0.7084668738900431473 ) ) ;
#199626 = CARTESIAN_POINT ( 'NONE',  ( 5.038483826543846078, -1.489082695810162837, 0.9007512145987550678 ) ) ;
#199627 = CARTESIAN_POINT ( 'NONE',  ( 4.521807925357579805, 5.234196320127330715, -1.199719254218452047 ) ) ;
#199628 = CARTESIAN_POINT ( 'NONE',  ( 1.505871038028598230, -2.274393761632488964, 0.2862045095256612326 ) ) ;
#199629 = CARTESIAN_POINT ( 'NONE',  ( -1.201851678989727383E-14, 4.759375000341419693, -1.575800808251660134 ) ) ;
#199630 = CARTESIAN_POINT ( 'NONE',  ( 6.146049400653379458, 0.6566722887273982456, 1.984991666494940743 ) ) ;
#199631 = CARTESIAN_POINT ( 'NONE',  ( 6.562452659285362699, -1.776534117310492711, -0.7846822752179910543 ) ) ;
#199632 = CARTESIAN_POINT ( 'NONE',  ( -6.735605996566196296E-15, -9.900000000000005684, 10.91970695577504458 ) ) ;
#199633 = FILL_AREA_STYLE ('',( #53399 ) ) ;
#199634 = CARTESIAN_POINT ( 'NONE',  ( 1.565077508395201988, -1.076315722900993643, 1.704939445326451475 ) ) ;
#199635 = CARTESIAN_POINT ( 'NONE',  ( 0.4983068789779531715, -0.7420642642406435341, -2.062120472104383317 ) ) ;
#199636 = CARTESIAN_POINT ( 'NONE',  ( 6.852217057538298128, 14.00000000000000000, -9.459770950306301884 ) ) ;
#199637 = CARTESIAN_POINT ( 'NONE',  ( -8.365544474831901667, 9.718555627847388578, 1.199719254218462483 ) ) ;
#199638 = CARTESIAN_POINT ( 'NONE',  ( 4.496500501226593727, 8.397667684739696270, 0.7998128361456462443 ) ) ;
#199639 = CARTESIAN_POINT ( 'NONE',  ( 3.651137946248568689, 0.3127203024623700367, 2.097190470537732221 ) ) ;
#199640 = CARTESIAN_POINT ( 'NONE',  ( 1.364683531249986537, -0.8447916663252468261, -0.7879004041258309554 ) ) ;
#199641 = CARTESIAN_POINT ( 'NONE',  ( 5.408770660633122063, 1.379882519126625295, -1.195542987486551301 ) ) ;
#199642 = ORIENTED_EDGE ( 'NONE', *, *, #10029, .T. ) ;
#199643 = CARTESIAN_POINT ( 'NONE',  ( -7.117104292530948229, 7.267986194233038155, -0.7998128361456362523 ) ) ;
#199644 = CARTESIAN_POINT ( 'NONE',  ( -2.449742653233043743, 3.299999999999976730, -0.4000000000000339950 ) ) ;
#199645 = CARTESIAN_POINT ( 'NONE',  ( -3.474999999999998312, -3.777083332377418223, 2.006292185433951047 ) ) ;
#199646 = CARTESIAN_POINT ( 'NONE',  ( -6.891622154448065807, 6.934647356477856128, 1.040834085586084257E-14 ) ) ;
#199647 = CARTESIAN_POINT ( 'NONE',  ( 2.883074275722704360, -1.867829236092366951, -0.7691044946091238899 ) ) ;
#199648 = CARTESIAN_POINT ( 'NONE',  ( 6.422910180798067969, 2.056742032306459578, 0.8002587082300142152 ) ) ;
#199649 = EDGE_CURVE ( 'NONE', #174147, #194519, #172833, .T. ) ;
#199650 = CARTESIAN_POINT ( 'NONE',  ( -5.008811405605897882, 4.808311159487113073, 0.7998128361456281477 ) ) ;
#199651 = CARTESIAN_POINT ( 'NONE',  ( 4.434314628233038569, -1.074157013132440275, 1.519412852752539678 ) ) ;
#199652 = CARTESIAN_POINT ( 'NONE',  ( 9.728138913005292210, 11.30824913904973705, -1.199719254218440723 ) ) ;
#199653 = CARTESIAN_POINT ( 'NONE',  ( 11.91826849282518275, 13.39999999999999858, -1.400000000000001465 ) ) ;
#199654 = EDGE_LOOP ( 'NONE', ( #209950, #90601, #192298, #44392 ) ) ;
#199655 = CARTESIAN_POINT ( 'NONE',  ( -2.578021764892882040, 6.159442492350315490, 0.7998128361456341429 ) ) ;
#199656 = CARTESIAN_POINT ( 'NONE',  ( -7.857113714319432063, 9.125386407249497012, 1.199719254218462483 ) ) ;
#199658 = CARTESIAN_POINT ( 'NONE',  ( -4.432018112209435756, 7.309502936831247411, 1.252451368452773384 ) ) ;
#199657 = CARTESIAN_POINT ( 'NONE',  ( -7.370792787684826486, 8.628288336167626582, -1.199719254218452047 ) ) ;
#199659 = CARTESIAN_POINT ( 'NONE',  ( -0.6823417656250003738, -0.7822916663252423852, -1.181850606188749264 ) ) ;
#199660 = CARTESIAN_POINT ( 'NONE',  ( 1.809482579268039126, -1.467825596939468902, 0.9224971444230285478 ) ) ;
#199661 = CARTESIAN_POINT ( 'NONE',  ( 1.745671189342316687, 0.5440799701325367277, 1.653152385070497887 ) ) ;
#199663 = CARTESIAN_POINT ( 'NONE',  ( 8.107412671292042461, 9.521364873671299023, 1.082531754730558626 ) ) ;
#199662 = CARTESIAN_POINT ( 'NONE',  ( 6.674459784896970227, -1.426286490538879903, 1.815071943837057500 ) ) ;
#199664 = CARTESIAN_POINT ( 'NONE',  ( 3.230585741806197841, 6.991043475407723307, 0.7998128361456271485 ) ) ;
#199665 = CARTESIAN_POINT ( 'NONE',  ( 1.177107960601676551, -0.04769765464058715876, -2.060389331245067179 ) ) ;
#199666 = CARTESIAN_POINT ( 'NONE',  ( 4.819033534653518025, 7.709623992816043270, -1.199719254218452047 ) ) ;
#199667 = ADVANCED_FACE ( 'NONE', ( #52194 ), #165943, .T. ) ;
#199668 = EDGE_CURVE ( 'NONE', #78277, #97632, #105717, .T. ) ;
#199669 = CARTESIAN_POINT ( 'NONE',  ( 6.626320313634256109, 0.4032262605214493312, -2.262638539848499164 ) ) ;
#199670 = DIRECTION ( 'NONE',  ( 0.000000000000000000, -1.000000000000000000, 0.000000000000000000 ) ) ;
#199671 = CARTESIAN_POINT ( 'NONE',  ( -4.664887371553763096, 7.600063145858131364, -1.199719254218453823 ) ) ;
#199672 = CARTESIAN_POINT ( 'NONE',  ( 0.2859245228041712439, -0.9316758688886862538, 1.737439158343912382 ) ) ;
#199673 = CIRCLE ( 'NONE', #47420, 11.09999999999999964 ) ;
#199675 = CARTESIAN_POINT ( 'NONE',  ( -5.804299160426224624, 9.785783097223662352, -0.7216878364870338292 ) ) ;
#199674 = CARTESIAN_POINT ( 'NONE',  ( 4.324404969281474109, -0.8226261416362996570, -1.726585468271451651 ) ) ;
#199676 = CARTESIAN_POINT ( 'NONE',  ( 6.094375512030342001, -2.195847865938059140, -0.2203403561373064590 ) ) ;
#199677 = CARTESIAN_POINT ( 'NONE',  ( -0.6125000000000244693, 1.520833334016126415, -1.060881119635955327 ) ) ;
#199678 = CARTESIAN_POINT ( 'NONE',  ( -6.075462232255183892, 10.10214001435745246, 0.000000000000000000 ) ) ;
#199679 = CARTESIAN_POINT ( 'NONE',  ( 3.553645660113312399, 7.160020680191912845, -1.734723475976807094E-15 ) ) ;
#199680 = CARTESIAN_POINT ( 'NONE',  ( -4.950135482320939140, 4.947781948895412008, -0.7216878364870338292 ) ) ;
#199681 = CARTESIAN_POINT ( 'NONE',  ( 0.2233145766990596859, 1.758413993963375610, 0.9933387185240820649 ) ) ;
#199682 = ORIENTED_EDGE ( 'NONE', *, *, #151247, .F. ) ;
#199683 = CARTESIAN_POINT ( 'NONE',  ( 2.942713080207468579, 2.290027058972336604, 0.2837140972290051466 ) ) ;
#199684 = CARTESIAN_POINT ( 'NONE',  ( 5.160583804383015227, -0.6592509027269661814, -1.847929681152965520 ) ) ;
#199685 = CARTESIAN_POINT ( 'NONE',  ( 0.7780835697005837881, -1.044612314895682292, -1.660310580060719188 ) ) ;
#199686 = CARTESIAN_POINT ( 'NONE',  ( 6.902720145097976712, 15.44736672593543148, 9.761920446463514978 ) ) ;
#199687 = LINE ( 'NONE', #150974, #161195 ) ;
#199688 = VERTEX_POINT ( 'NONE', #152371 ) ;
#199689 = CARTESIAN_POINT ( 'NONE',  ( 0.2865162857260491469, -0.7196341243457348158, -1.991407047551809750 ) ) ;
#199691 = CARTESIAN_POINT ( 'NONE',  ( -7.483210719738908168, 10.81783070874899799, 1.199719254218453823 ) ) ;
#199690 = CARTESIAN_POINT ( 'NONE',  ( -3.913499895838973508, 7.717500311787445000, 1.040834085586084257E-14 ) ) ;
#199692 = CARTESIAN_POINT ( 'NONE',  ( 0.1109373197970727476, -1.806229982939497436, 0.3559056038356380181 ) ) ;
#199693 = CARTESIAN_POINT ( 'NONE',  ( 3.889651762418313119, -2.008042162167834377, 0.8258804214429303903 ) ) ;
#199694 = CARTESIAN_POINT ( 'NONE',  ( 0.0008036159801554723387, 2.587196701860821957, 2.002358341361919702 ) ) ;
#199695 = CARTESIAN_POINT ( 'NONE',  ( 1.758217466200185042, 0.8068918862002281145, -1.961288232260410380 ) ) ;
#199696 = CARTESIAN_POINT ( 'NONE',  ( -1.500000000000013101, 3.410416667349487785, -0.8660254037844313801 ) ) ;
#199697 = CARTESIAN_POINT ( 'NONE',  ( 9.134442807305049428, 11.67993591332117376, 1.599625672291281386 ) ) ;
#199698 = CARTESIAN_POINT ( 'NONE',  ( 11.97185388258315264, 13.87999990720392596, -0.8311143155443057040 ) ) ;
#199699 = CARTESIAN_POINT ( 'NONE',  ( 6.374094191309353619, 6.920300110170956032, -0.8184029421815092187 ) ) ;
#199700 = ORIENTED_EDGE ( 'NONE', *, *, #176940, .F. ) ;
#199701 = CARTESIAN_POINT ( 'NONE',  ( 1.915377802959626230, -0.2551614870064948803, 2.044872660591416480 ) ) ;
#199703 = CARTESIAN_POINT ( 'NONE',  ( 0.000000000000000000, -3.600000000000005862, 0.000000000000000000 ) ) ;
#199702 = CARTESIAN_POINT ( 'NONE',  ( -7.641992139597101108, 12.06740792950531649, 0.7998128361456481317 ) ) ;
#199704 = CARTESIAN_POINT ( 'NONE',  ( 1.364683531249988757, 2.134375000341422357, 1.214306433183764966E-14 ) ) ;
#199705 = CARTESIAN_POINT ( 'NONE',  ( 0.07735805125223899070, 6.946777552644263665, -2.683974465663693021 ) ) ;
#199706 = CARTESIAN_POINT ( 'NONE',  ( -6.471393748265563239, 5.229711127717889596, 2.499999999999998668 ) ) ;
#199707 = ORIENTED_EDGE ( 'NONE', *, *, #130618, .T. ) ;
#199708 = CARTESIAN_POINT ( 'NONE',  ( 4.107995242876061326, -0.7289348763114507079, 1.768098669557085278 ) ) ;
#199709 = AXIS2_PLACEMENT_3D ( 'NONE', #43635, #109750, #27353 ) ;
#199710 = CARTESIAN_POINT ( 'NONE',  ( 3.022498986271242138, 2.800000000000017586, 2.500000000000000444 ) ) ;
#199711 = CARTESIAN_POINT ( 'NONE',  ( 1.898125948304218547, -0.7631055018291610370, 2.129926759817270199 ) ) ;
#199712 = CARTESIAN_POINT ( 'NONE',  ( -3.898132859128961236, 4.506575409527250997, -1.199719254218452047 ) ) ;
#199713 = CARTESIAN_POINT ( 'NONE',  ( 1.511653934090980034, -0.6084181080006717535, 1.706514628581125681 ) ) ;
#199714 = CARTESIAN_POINT ( 'NONE',  ( 1.217839795352684273, 0.9409426854420616104, -1.668592810110066438 ) ) ;
#199715 = CARTESIAN_POINT ( 'NONE',  ( 1.750525128138082254, -2.060206210462053988, -0.2049951091474821463 ) ) ;
#199716 = CARTESIAN_POINT ( 'NONE',  ( 1.364683531249986537, 1.176041667008082658, 0.7879004041258500513 ) ) ;
#199717 = CIRCLE ( 'NONE', #44212, 11.99999999999999112 ) ;
#199718 = CARTESIAN_POINT ( 'NONE',  ( 0.1453086613420169204, -1.522338971917249317, -1.252298935284136938 ) ) ;
#199719 = CARTESIAN_POINT ( 'NONE',  ( 4.969325399568108814, 0.1871947810346066554, -1.917384544105669386 ) ) ;
#199721 = CARTESIAN_POINT ( 'NONE',  ( 5.865087380380676230, 7.178575736046542310, -1.148900262672468475 ) ) ;
#199720 = CARTESIAN_POINT ( 'NONE',  ( 0.3820104410975051490, 2.150944695799131612, -0.8364647861166041309 ) ) ;
#199722 = CARTESIAN_POINT ( 'NONE',  ( 0.6823417656249899377, 1.842708333674752952, 1.181850606188755259 ) ) ;
#199723 = CARTESIAN_POINT ( 'NONE',  ( 4.773915743512389120, -2.023523412367009833, 0.3991901646795847913 ) ) ;
#199724 = CARTESIAN_POINT ( 'NONE',  ( -6.521635583373313061, 7.567328587812373719, -1.199719254218446718 ) ) ;
#199725 = CARTESIAN_POINT ( 'NONE',  ( 7.052212457402625922, 11.37933163361175382, -0.7998128361456291469 ) ) ;
#199726 = CARTESIAN_POINT ( 'NONE',  ( 3.181359600701000989, 6.863336634126477875, 0.000000000000000000 ) ) ;
#199727 = CARTESIAN_POINT ( 'NONE',  ( 3.981290663907289140, 7.796589541200495965, -0.7998128361456221525 ) ) ;
#199729 = CARTESIAN_POINT ( 'NONE',  ( -1.500000000000013101, 3.879166666666685970, -0.8660254037844313801 ) ) ;
#199728 = CARTESIAN_POINT ( 'NONE',  ( 5.245193717270952405, -1.807841653007141947, 1.079916013355223248 ) ) ;
#199730 = CARTESIAN_POINT ( 'NONE',  ( 0.9772844579341716242, 2.006041157791297991, 0.8309993691856133458 ) ) ;
#199731 = CARTESIAN_POINT ( 'NONE',  ( -1.364683531250012516, 2.092708333674750953, 0.7879004041258379498 ) ) ;
#199732 = CARTESIAN_POINT ( 'NONE',  ( 5.026735257907362531, 2.066873009482797841, 0.6328083787210944111 ) ) ;
#199733 = CARTESIAN_POINT ( 'NONE',  ( 5.180334445267184229, 0.9972254788270168424, 1.756242667785257172 ) ) ;
#199734 = CARTESIAN_POINT ( 'NONE',  ( -0.02900071798684483726, 7.629137130509101361, -2.773797386654376584 ) ) ;
#199735 = AXIS2_PLACEMENT_3D ( 'NONE', #51788, #180700, #32324 ) ;
#199736 = EDGE_CURVE ( 'NONE', #126275, #162523, #177803, .T. ) ;
#199739 = CARTESIAN_POINT ( 'NONE',  ( 5.883875478650832491, 6.927238148923188454, -1.082531754730543083 ) ) ;
#199738 = CARTESIAN_POINT ( 'NONE',  ( 3.285556943750000514, -2.063541666188710266, 1.896917185911906500 ) ) ;
#199737 = CARTESIAN_POINT ( 'NONE',  ( 5.854088466050551887, 10.05179665369283981, 0.7998128361456341429 ) ) ;
#199740 = CARTESIAN_POINT ( 'NONE',  ( -6.967964602780620353, 7.093989889524320525, 0.000000000000000000 ) ) ;
#199741 = CARTESIAN_POINT ( 'NONE',  ( 3.327361509216096191, -1.530157842762596143, -1.313544516083162028 ) ) ;
#199742 = CARTESIAN_POINT ( 'NONE',  ( -8.503988664269602538, 10.94440607977979063, 1.599625672291269396 ) ) ;
#199744 = CARTESIAN_POINT ( 'NONE',  ( -7.607533590599451223, 9.008448956188397361, 1.082531754730549078 ) ) ;
#199743 = CARTESIAN_POINT ( 'NONE',  ( -4.288456660624211381, 3.897620947016656956, 1.214306433183764966E-14 ) ) ;
#199746 = CARTESIAN_POINT ( 'NONE',  ( -1.364683531250010740, 8.380208333674730170, 0.7879004041258445001 ) ) ;
#199745 = CARTESIAN_POINT ( 'NONE',  ( 5.225516498768126183, -2.053876642077703707, 0.6744380372525200507 ) ) ;
#199747 = PRESENTATION_STYLE_ASSIGNMENT (( #49265 ) ) ;
#199749 = CARTESIAN_POINT ( 'NONE',  ( -10.84253909858433040, 4.919570308430903260, -5.035411995924087059 ) ) ;
#199748 = B_SPLINE_CURVE_WITH_KNOTS ( 'NONE', 3,
 ( #158813, #42952, #75427, #58108, #190225, #76481, #90628, #24519, #119164, #91705 ),
 .UNSPECIFIED., .F., .F.,
 ( 4, 2, 2, 2, 4 ),
 ( 0.000000000000000000, 0.0002334048330869030008, 0.0004668096661738060016, 0.0007002144992607089481, 0.0009336193323476120031 ),
 .UNSPECIFIED. ) ;
#199751 = CARTESIAN_POINT ( 'NONE',  ( 5.009388752257521560, -1.913799287717246500, 0.6352160319311253023 ) ) ;
#199750 = CARTESIAN_POINT ( 'NONE',  ( -6.358410854684777291, 10.36197039720016022, -0.7216878364870267237 ) ) ;
#199752 = CARTESIAN_POINT ( 'NONE',  ( -1.500000000000011324, 5.420833333333356485, 0.8660254037844403729 ) ) ;
#199753 = CARTESIAN_POINT ( 'NONE',  ( 0.3809451599157384627, 1.611386624718774918, -0.6158283211408090985 ) ) ;
#199754 = CARTESIAN_POINT ( 'NONE',  ( 4.923546060418115822, 5.773167154356443120, -1.199719254218452047 ) ) ;
#199756 = CARTESIAN_POINT ( 'NONE',  ( 6.156284269057003655, 9.340026192945279249, -1.199719254218452047 ) ) ;
#199755 = CARTESIAN_POINT ( 'NONE',  ( 6.805829924380097040, 10.88395931184472154, 0.7216878364870438212 ) ) ;
#199757 = CARTESIAN_POINT ( 'NONE',  ( -11.55895101287907067, 8.210663139309525960, 3.234169276427452111 ) ) ;
#199758 = CARTESIAN_POINT ( 'NONE',  ( 5.835183367072669824, -1.691281831231405963, 0.7993005984755219284 ) ) ;
#199759 =( BOUNDED_CURVE ( )  B_SPLINE_CURVE ( 2, ( #53191, #164024, #31889, #70474, #136590, #119320, #20666 ),
 .UNSPECIFIED., .F., .T. ) 
 B_SPLINE_CURVE_WITH_KNOTS ( ( 3, 2, 2, 3 ),
 ( 0.1999999999999998446, 0.2041666666666665519, 0.2083333333333333148, 0.2125000000000000222 ),
 .UNSPECIFIED. ) 
 CURVE ( )  GEOMETRIC_REPRESENTATION_ITEM ( )  RATIONAL_B_SPLINE_CURVE ( ( 1.000000000000005329, 0.8660254037844333785, 1.000000000000000000, 0.8660254037844387076, 1.000000000000000000, 0.8660254037844378194, 1.000000000000000888 ) ) 
 REPRESENTATION_ITEM ( '' )  );
#199760 = CARTESIAN_POINT ( 'NONE',  ( 6.345953593097265255, -1.318148336383131669, -1.521719194605136494 ) ) ;
#199761 = CARTESIAN_POINT ( 'NONE',  ( -4.222251700817149178, 3.978710388688374788, 0.5243367479217392324 ) ) ;
#199762 = CARTESIAN_POINT ( 'NONE',  ( -5.099275172071237705, 8.963255110809500437, 0.000000000000000000 ) ) ;
#199763 = ORIENTED_EDGE ( 'NONE', *, *, #97288, .T. ) ;
#199765 = CARTESIAN_POINT ( 'NONE',  ( 1.968375273883906429, -1.978056371059619511, -0.3905749819678172585 ) ) ;
#199764 = CARTESIAN_POINT ( 'NONE',  ( 2.051582899450168362, -1.892833867889589960, 0.9560217657286762538 ) ) ;
#199766 = CARTESIAN_POINT ( 'NONE',  ( 1.529274006537587161, -0.2194501901080987971, 1.798134050542072870 ) ) ;
#199767 = CARTESIAN_POINT ( 'NONE',  ( 7.686546744304875389, 7.932335721302671949, 0.7998128361456291469 ) ) ;
#199768 = CARTESIAN_POINT ( 'NONE',  ( 6.702040708066514085, -2.161345696851162845, 0.04751196314212167288 ) ) ;
#199769 = CARTESIAN_POINT ( 'NONE',  ( 7.623762449586013901, 7.788811034138823253, 1.040834085586084257E-14 ) ) ;
#199771 = CARTESIAN_POINT ( 'NONE',  ( 0.004910489962322779275, -0.09121751714964576596, 1.913643331117439672 ) ) ;
#199770 = CARTESIAN_POINT ( 'NONE',  ( -4.229253852459088137, 7.021547696922494808, 1.199719254218464037 ) ) ;
#199772 = DIRECTION ( 'NONE',  ( -0.000000000000000000, -8.546850786086437571E-32, -1.000000000000000000 ) ) ;
#199773 = DIRECTION ( 'NONE',  ( -8.638326563840814399E-31, 0.000000000000000000, -1.000000000000000000 ) ) ;
#199774 = CARTESIAN_POINT ( 'NONE',  ( 5.083944415000174466, 7.914723669933440675, -1.082531754730549078 ) ) ;
#199775 = CARTESIAN_POINT ( 'NONE',  ( 1.364683531249986981, -1.053124999658580752, 0.000000000000000000 ) ) ;
#199776 = CARTESIAN_POINT ( 'NONE',  ( 4.555176424511575561, 4.416720038126027426, -0.7216878364870188411 ) ) ;
#199777 = CARTESIAN_POINT ( 'NONE',  ( -3.704402285031864306, 5.344888637335695414, -1.599625672291256295 ) ) ;
#199778 = ADVANCED_FACE ( 'NONE', ( #101480 ), #178839, .T. ) ;
#199779 = CARTESIAN_POINT ( 'NONE',  ( 4.522454563201145028, 1.332364063043835811, -1.702191164408660029 ) ) ;
#199780 = CARTESIAN_POINT ( 'NONE',  ( -6.672020991700860826, 7.917017590806697314, 1.082531754730549078 ) ) ;
#199781 = CARTESIAN_POINT ( 'NONE',  ( 4.584065335196252811, 8.362176967788721882, 0.7216878364870328300 ) ) ;
#199782 = CARTESIAN_POINT ( 'NONE',  ( 1.775790443353560732, 0.3575140072833471461, -2.090081039791711337 ) ) ;
#199783 = CARTESIAN_POINT ( 'NONE',  ( 6.475623784153278883, 1.746001614453606576, -0.5331787911772439825 ) ) ;
#199784 = CARTESIAN_POINT ( 'NONE',  ( 3.022686310138736676, 1.855048300136890482, 0.6674203052531629821 ) ) ;
#199785 = CARTESIAN_POINT ( 'NONE',  ( 4.763870730211980487, 0.5944114921396548290, -1.817767169311027997 ) ) ;
#199786 = ORIENTED_EDGE ( 'NONE', *, *, #22230, .T. ) ;
#199788 = ADVANCED_FACE ( 'NONE', ( #200028 ), #53809, .F. ) ;
#199787 = LINE ( 'NONE', #86055, #166929 ) ;
#199789 = CARTESIAN_POINT ( 'NONE',  ( 5.687944394218412469, -1.248225810400976465, -1.523521433493113308 ) ) ;
#199790 = CARTESIAN_POINT ( 'NONE',  ( 1.781094086345108130, 1.339032250488644937, 1.406688339355038009 ) ) ;
#199791 = ORIENTED_EDGE ( 'NONE', *, *, #11694, .F. ) ;
#199792 = CARTESIAN_POINT ( 'NONE',  ( -3.135678666510573365, 6.880318554229450712, 0.000000000000000000 ) ) ;
#199794 = CARTESIAN_POINT ( 'NONE',  ( 5.691390622686558487, 9.861982503101517139, 0.7998128361456341429 ) ) ;
#199793 = CARTESIAN_POINT ( 'NONE',  ( -6.536439455564198475, 8.719208346281938304, 1.443375672974064550 ) ) ;
#199795 = CARTESIAN_POINT ( 'NONE',  ( 6.608709811657416999, 9.797579649320619311, -1.199719254218440723 ) ) ;
#199797 = CARTESIAN_POINT ( 'NONE',  ( 4.706088717274896638, 7.544168365912456764, 1.082531754730548412 ) ) ;
#199796 = CARTESIAN_POINT ( 'NONE',  ( 7.308008492965924141, 8.484763649003774333, -1.199719254218451159 ) ) ;
#199799 = ORIENTED_EDGE ( 'NONE', *, *, #61767, .T. ) ;
#199798 = CARTESIAN_POINT ( 'NONE',  ( 6.410809557875646547, -0.5148348048229570706, -1.841598127471068658 ) ) ;
#199800 = CARTESIAN_POINT ( 'NONE',  ( 3.440233207309027375, 0.9924059104887033023, -1.971224004288201881 ) ) ;
#199801 = CARTESIAN_POINT ( 'NONE',  ( 2.450463542074859280, 2.206263077450395738, 0.05474276496272853509 ) ) ;
#199802 = DIRECTION ( 'NONE',  ( 0.9885327375000381167, 0.000000000000000000, -0.1510067114093955609 ) ) ;
#199803 = CARTESIAN_POINT ( 'NONE',  ( 0.9789966485893276671, -1.729064073676725544, -0.8170501332188941923 ) ) ;
#199804 = CARTESIAN_POINT ( 'NONE',  ( -0.4366703603831086355, -8.283751815806034813, 10.40709768291845094 ) ) ;
#199805 = CARTESIAN_POINT ( 'NONE',  ( -5.204170427930421283E-15, 3.467171072964057910, -11.99762841690768234 ) ) ;
#199806 = CARTESIAN_POINT ( 'NONE',  ( 3.561042923925850978, 1.633862107263984065, -1.271492733312264090 ) ) ;
#199807 = CARTESIAN_POINT ( 'NONE',  ( -4.415151579544611238, 8.302760609444034046, -0.7998128361456281477 ) ) ;
#199808 = CIRCLE ( 'NONE', #78763, 0.07999999999999998779 ) ;
#199809 = CARTESIAN_POINT ( 'NONE',  ( -5.244114872543307548, 7.700386654371578210, 1.209007019071134170 ) ) ;
#199811 = CARTESIAN_POINT ( 'NONE',  ( 1.499129196564863209, 1.767075381950654611, -1.244890797856931686 ) ) ;
#199810 = CARTESIAN_POINT ( 'NONE',  ( -3.765413976293358278, 5.416068943807445635, 1.599625672291267398 ) ) ;
#199812 = CARTESIAN_POINT ( 'NONE',  ( 3.614928802375876771, -0.1595779646587774658, 2.185787688459623901 ) ) ;
#199813 = CARTESIAN_POINT ( 'NONE',  ( -0.3282377607281289911, 0.6986645496846380921, -1.225000000000010747 ) ) ;
#199814 = CARTESIAN_POINT ( 'NONE',  ( 3.268924434670684498, 6.827845917175511481, -1.734723475976807094E-15 ) ) ;
#199815 = CARTESIAN_POINT ( 'NONE',  ( -0.3282377607281401488, 1.011164550367433579, -1.225000000000022959 ) ) ;
#199816 = CARTESIAN_POINT ( 'NONE',  ( -8.012344526598182026E-15, 13.85937500034139447, -1.575800808251669460 ) ) ;
#199817 = CARTESIAN_POINT ( 'NONE',  ( -4.796552484184649856, 8.818004674849227342, -0.7998128361456362523 ) ) ;
#199818 = PRODUCT_DEFINITION_CONTEXT ( 'detailed design', #29814, 'design' ) ;
#199819 = CARTESIAN_POINT ( 'NONE',  ( 5.502511934227880097, -1.689919030931926969, 0.3883318411201929776 ) ) ;
#199820 = ADVANCED_FACE ( 'NONE', ( #202147 ), #182719, .F. ) ;
#199821 = CARTESIAN_POINT ( 'NONE',  ( -10.48008955368359629, 11.32911868882677986, 1.040834085586084257E-14 ) ) ;
#199822 = PRESENTATION_LAYER_ASSIGNMENT (  '', '', ( #33791 ) ) ;
#199823 = CARTESIAN_POINT ( 'NONE',  ( 4.030184149050713316, 1.145922430192683805, 1.723988044715178081 ) ) ;
#199824 = CARTESIAN_POINT ( 'NONE',  ( 4.323895160615763622, 0.9038210025188663232, -1.914733396627795958 ) ) ;
#199825 = CARTESIAN_POINT ( 'NONE',  ( 6.474182045725470402, 7.511966127223233869, -1.199719254218446718 ) ) ;
#199826 = CARTESIAN_POINT ( 'NONE',  ( -1.001543065824772872E-14, 4.571875000341418804, 1.575800808251672791 ) ) ;
#199827 = CARTESIAN_POINT ( 'NONE',  ( 3.045709290742618425, 1.389371873615535602, 1.396104611999344769 ) ) ;
#199828 = CARTESIAN_POINT ( 'NONE',  ( 0.4746845637013075159, -1.383529810647101455, 1.320479256824915071 ) ) ;
#199829 = CARTESIAN_POINT ( 'NONE',  ( 4.593851424282248352, -2.291655481657675519, -0.05911330884650690953 ) ) ;
#199830 = CARTESIAN_POINT ( 'NONE',  ( 2.930095790256614929, 1.013914413367119627, -1.518051517300327502 ) ) ;
#199831 = CARTESIAN_POINT ( 'NONE',  ( 3.902768115887398803, 5.646591783325653147, -1.599625672291269396 ) ) ;
#199832 = CARTESIAN_POINT ( 'NONE',  ( 4.975479186090857375, 5.867442474269873642, 1.082531754730560403 ) ) ;
#199833 = CARTESIAN_POINT ( 'NONE',  ( -6.561256274009600986, 9.742217188731485678, -1.199719254218440723 ) ) ;
#199834 = ORIENTED_EDGE ( 'NONE', *, *, #174601, .T. ) ;
#199835 = ORIENTED_EDGE ( 'NONE', *, *, #213029, .F. ) ;
#199836 = CARTESIAN_POINT ( 'NONE',  ( 4.465094144989894431, -1.614439531090381408, 1.202519638469838226 ) ) ;
#199837 = CARTESIAN_POINT ( 'NONE',  ( 4.680490258543752446, 1.210089798712219222, -1.543956201849092658 ) ) ;
#199838 = CARTESIAN_POINT ( 'NONE',  ( -7.019370843573183194, 9.212351955633947043, 1.599625672291283607 ) ) ;
#199839 = CARTESIAN_POINT ( 'NONE',  ( -4.401593425930945713, 8.286942763561420122, 1.040834085586084257E-14 ) ) ;
#199840 = CARTESIAN_POINT ( 'NONE',  ( 0.1751657365761703222, 0.2353161675953834020, -2.077853038718394885 ) ) ;
#199842 = CARTESIAN_POINT ( 'NONE',  ( 6.139478286200317214, -1.284810642169451622, -1.217457132491184035 ) ) ;
#199841 = CARTESIAN_POINT ( 'NONE',  ( 0.9078953525096540300, -0.9432727566685695786, -1.865958795489220723 ) ) ;
#199843 = CARTESIAN_POINT ( 'NONE',  ( -1.420000000000021911, 6.280000000000042881, 2.580000000000011173 ) ) ;
#199844 = CARTESIAN_POINT ( 'NONE',  ( 2.291216553123593958, 1.694975396412688351, 1.389067552005143424 ) ) ;
#199845 = CARTESIAN_POINT ( 'NONE',  ( 6.298757997817161502, 1.451094931915532404, 0.9604431249435537721 ) ) ;
#199846 = CARTESIAN_POINT ( 'NONE',  ( 6.751070424600909448, 9.963667031088037973, -1.199719254218441611 ) ) ;
#199847 =( NAMED_UNIT ( * ) PLANE_ANGLE_UNIT ( ) SI_UNIT ( $, .RADIAN. ) );
#199848 = CARTESIAN_POINT ( 'NONE',  ( 0.4688601960516668443, 0.1741500657085493509, -1.716052735907805937 ) ) ;
#199849 = CARTESIAN_POINT ( 'NONE',  ( 0.7030180566853957425, -1.627119059678893587, -1.623510667393740725 ) ) ;
#199850 = CARTESIAN_POINT ( 'NONE',  ( 0.7850416839378616674, 1.930235501049954339, -1.037882601892345713 ) ) ;
#199851 = CARTESIAN_POINT ( 'NONE',  ( 3.299657469156279888, 1.739734091921738557, 1.357710657151039779 ) ) ;
#199852 = AXIS2_PLACEMENT_3D ( 'NONE', #127914, #57485, #44449 ) ;
#199853 = CARTESIAN_POINT ( 'NONE',  ( 0.7608744453060071189, -0.7297706024342350828, -2.044895412143563185 ) ) ;
#199854 = CARTESIAN_POINT ( 'NONE',  ( 1.673838217086941410E-16, 3.900000000000000799, 2.500000000000000000 ) ) ;
#199855 = CARTESIAN_POINT ( 'NONE',  ( 2.800141503465008341, -1.047918259751862147, -1.839804015593812458 ) ) ;
#199856 = CARTESIAN_POINT ( 'NONE',  ( 5.104483318454627216, -0.6487533354903095573, -1.814000550502705922 ) ) ;
#199857 = ORIENTED_EDGE ( 'NONE', *, *, #125435, .T. ) ;
#199859 = CARTESIAN_POINT ( 'NONE',  ( -0.6823417656250003738, -0.9697916663252494907, -1.181850606188749264 ) ) ;
#199858 = CARTESIAN_POINT ( 'NONE',  ( 2.665910428807946708, 1.228978066529669899, 1.934933738419620575 ) ) ;
#199860 = CARTESIAN_POINT ( 'NONE',  ( 3.334415713957098681, 5.977569868670206787, -1.199719254218446718 ) ) ;
#199861 = CARTESIAN_POINT ( 'NONE',  ( 6.602984505055297326, 7.662235663108029726, 1.199719254218462483 ) ) ;
#199862 = CIRCLE ( 'NONE', #61507, 10.97656854249491687 ) ;
#199863 = CARTESIAN_POINT ( 'NONE',  ( 4.354274701107041956, 0.9498992632326860308, -2.008065553403962422 ) ) ;
#199864 = CARTESIAN_POINT ( 'NONE',  ( -6.548225005720456515, 10.58342024007512983, 0.000000000000000000 ) ) ;
#199865 = CARTESIAN_POINT ( 'NONE',  ( -0.1749484593404703747, -5.350147675656129032, -10.96499746917716678 ) ) ;
#199866 = CARTESIAN_POINT ( 'NONE',  ( 4.799223189557548785, 7.582548906917042864, -1.082531754730549078 ) ) ;
#199867 = CARTESIAN_POINT ( 'NONE',  ( -7.659993601596713830, 9.959745173328078849, -1.443375672974058777 ) ) ;
#199868 = CARTESIAN_POINT ( 'NONE',  ( 5.939880696562888751, 7.062853913145737295, -1.082531754730548412 ) ) ;
#199869 = ORIENTED_EDGE ( 'NONE', *, *, #89552, .T. ) ;
#199870 = CARTESIAN_POINT ( 'NONE',  ( 2.953750172290268150, -1.864168560446223033, -0.7691209412190866956 ) ) ;
#199872 = CARTESIAN_POINT ( 'NONE',  ( 1.059521212928912881, 1.683986000210126788, 1.190688086201870499 ) ) ;
#199871 = CARTESIAN_POINT ( 'NONE',  ( 6.238723240582662477, 10.43026088065513513, -0.7998128361456291469 ) ) ;
#199873 = CARTESIAN_POINT ( 'NONE',  ( -10.91970695577495398, -6.134628647623513231, 8.483881999699072196E-15 ) ) ;
#199874 = CARTESIAN_POINT ( 'NONE',  ( 6.495764994278809823, 6.751016379513001375, 0.7216878364870328300 ) ) ;
#199875 = PRESENTATION_STYLE_ASSIGNMENT (( #166324 ) ) ;
#199876 = CARTESIAN_POINT ( 'NONE',  ( -1.364683531249997417, 4.009375000341424133, 1.214306433183764966E-14 ) ) ;
#199877 = CARTESIAN_POINT ( 'NONE',  ( 4.295009486468337023, 1.759388067201245187, 1.306329983072423984 ) ) ;
#199878 = CARTESIAN_POINT ( 'NONE',  ( 1.055314813143366726, -1.277040974352643854, 1.560502084637045650 ) ) ;
#199879 = CARTESIAN_POINT ( 'NONE',  ( 1.329379181053941483, 0.9071106928158387817, -1.602193565413398968 ) ) ;
#199880 = CARTESIAN_POINT ( 'NONE',  ( 5.671479170183292950, 1.362789248821870025, 1.843150307845689229 ) ) ;
#199881 = CARTESIAN_POINT ( 'NONE',  ( 3.714658492009088153, -0.1339090230784936997, 1.836323816731308067 ) ) ;
#199882 = CARTESIAN_POINT ( 'NONE',  ( 8.555358625423188812, 9.940005470203933768, 1.199719254218462483 ) ) ;
#199883 = CARTESIAN_POINT ( 'NONE',  ( 4.155160913615768337, -1.517764731708035386, -1.014145119915064841 ) ) ;
#199884 = CARTESIAN_POINT ( 'NONE',  ( 5.449842333688053486, -1.824117940560719298, -0.8596331684956670660 ) ) ;
#199885 = CARTESIAN_POINT ( 'NONE',  ( -8.259941899223614215, 10.65968485389279508, -1.599625672291263179 ) ) ;
#199887 = CARTESIAN_POINT ( 'NONE',  ( 0.000000000000000000, 5.999999999999998224, 0.000000000000000000 ) ) ;
#199886 = CARTESIAN_POINT ( 'NONE',  ( 5.102513680054168610, -0.7571875712604788644, -2.132187818420825831 ) ) ;
#199888 = CARTESIAN_POINT ( 'NONE',  ( 6.774446309029529267, -1.298820955785205955, 1.658247839749617869 ) ) ;
#199889 = CARTESIAN_POINT ( 'NONE',  ( 3.578635096964689843, 1.315621898185691974, -1.598582974826658010 ) ) ;
#199890 = CARTESIAN_POINT ( 'NONE',  ( 9.077347539549325717, 10.54899253668443393, -1.199719254218446718 ) ) ;
#199891 = CARTESIAN_POINT ( 'NONE',  ( -6.760415694317216410E-14, 2.234375000341476625, 1.570758158831744078 ) ) ;
#199892 = SHAPE_DEFINITION_REPRESENTATION ( #41899, #189584 ) ;
#199894 = CARTESIAN_POINT ( 'NONE',  ( 1.875490933414716288, 1.843686865663298091, -0.5587569667290130937 ) ) ;
#199893 = CARTESIAN_POINT ( 'NONE',  ( -7.330154606482786050, 11.70359747420527619, 0.000000000000000000 ) ) ;
#199895 = CARTESIAN_POINT ( 'NONE',  ( -4.516801452008150086, 5.298631777878131111, 1.199719254218452935 ) ) ;
#199896 = CARTESIAN_POINT ( 'NONE',  ( 6.332857179708399009, -1.868906791504289844, -0.6213115537570863545 ) ) ;
#199897 = CARTESIAN_POINT ( 'NONE',  ( 5.370438244344566847, 5.438135171256338829, 0.000000000000000000 ) ) ;
#199898 = CARTESIAN_POINT ( 'NONE',  ( 5.827790676886797527, 6.016211147664318304, -0.4261259532085531765 ) ) ;
#199899 = VECTOR ( 'NONE', #40981, 1000.000000000000227 ) ;
#199900 = CARTESIAN_POINT ( 'NONE',  ( -9.002250809793991948, 12.48608113052627289, -1.082531754730543971 ) ) ;
#199902 = CARTESIAN_POINT ( 'NONE',  ( 1.986886853112525442, -1.362214788617806649, 1.754679387841934002 ) ) ;
#199901 = CARTESIAN_POINT ( 'NONE',  ( 1.002369745560643510, -0.9483682245385971488, 1.896766750748935415 ) ) ;
#199903 = CARTESIAN_POINT ( 'NONE',  ( 3.030406611367501224, 1.171151514522270398, -1.750062178063223506 ) ) ;
#199904 = CARTESIAN_POINT ( 'NONE',  ( -5.413448473606448985, 9.537716662508005427, 0.000000000000000000 ) ) ;
#199905 = CARTESIAN_POINT ( 'NONE',  ( 7.786460292950004636, 7.978625184730144149, 1.040834085586084257E-14 ) ) ;
#199906 = CARTESIAN_POINT ( 'NONE',  ( 0.8712809235682484887, -0.2783187086575014679, 1.840006102165496982 ) ) ;
#199907 = CARTESIAN_POINT ( 'NONE',  ( 6.582647274634798151, 7.638508894284114170, 1.199719254218462483 ) ) ;
#199908 = CARTESIAN_POINT ( 'NONE',  ( -4.245996903372413200, 7.323364108789364835, -0.8915694317389293300 ) ) ;
#199909 = CARTESIAN_POINT ( 'NONE',  ( 3.161022370280501814, 6.839609865302569425, 0.000000000000000000 ) ) ;
#199910 = CARTESIAN_POINT ( 'NONE',  ( -4.502716413514296079, 8.267269892493059658, -0.7216878364870338292 ) ) ;
#199911 = CARTESIAN_POINT ( 'NONE',  ( -6.534666852106790103, 10.56760239419251590, 0.7216878364870458196 ) ) ;
#199912 = CARTESIAN_POINT ( 'NONE',  ( 1.283610819548046011, 0.1505422781087061845, -2.115291873224629082 ) ) ;
#199913 = CARTESIAN_POINT ( 'NONE',  ( -4.925354943514475003, 8.968274210734028529, 0.000000000000000000 ) ) ;
#199915 = CARTESIAN_POINT ( 'NONE',  ( 4.088298575758734898, 1.051444423028622399, -1.656135347060924135 ) ) ;
#199914 = CARTESIAN_POINT ( 'NONE',  ( -1.225000000000028066, 0.5000000000000143219, -5.030698080332740574E-14 ) ) ;
#199916 = CARTESIAN_POINT ( 'NONE',  ( 3.801785103514757846, -0.6297183656660889639, 2.067937956787009757 ) ) ;
#199917 = CARTESIAN_POINT ( 'NONE',  ( 1.979791773625012352, -1.805961398883266344, -0.3578489297004632808 ) ) ;
#199918 = CARTESIAN_POINT ( 'NONE',  ( -4.021031317475609157, 7.616913651768732585, 0.1724795716798576684 ) ) ;
#199919 = CARTESIAN_POINT ( 'NONE',  ( 1.364683531249984538, -1.032291666325247714, -0.7879004041258309554 ) ) ;
#199920 = CARTESIAN_POINT ( 'NONE',  ( 4.206796582046585797, -0.2943472477981134428, 1.715077512146965688 ) ) ;
#199922 = AXIS2_PLACEMENT_3D ( 'NONE', #62013, #47924, #161656 ) ;
#199921 = CARTESIAN_POINT ( 'NONE',  ( -3.796053574490474869, 15.00000000000207656, -12.24940615670125510 ) ) ;
#199923 = CARTESIAN_POINT ( 'NONE',  ( 6.155038550924155416, 6.283225852274053835, 0.7216878364870317197 ) ) ;
#199924 = CARTESIAN_POINT ( 'NONE',  ( -10.99931038725301846, 6.873658557531565627, -3.960823121322395224 ) ) ;
#199925 = EDGE_CURVE ( 'NONE', #13744, #141934, #162470, .T. ) ;
#199926 = CARTESIAN_POINT ( 'NONE',  ( 2.448304249002517974, 2.161202317112873139, 0.05382173394478938222 ) ) ;
#199927 = CARTESIAN_POINT ( 'NONE',  ( 3.128279665134887644, 0.2985813455266342342, -1.993766061640166232 ) ) ;
#199928 = CARTESIAN_POINT ( 'NONE',  ( -10.43941509239824228, 11.28166515066052966, 1.040834085586084257E-14 ) ) ;
#199929 = CARTESIAN_POINT ( 'NONE',  ( 1.024558638192473170, 1.287004556549703693, -1.736669753874709343 ) ) ;
#199930 = CARTESIAN_POINT ( 'NONE',  ( 3.625814716899962153, -1.173175478197308053, -1.584272814160747833 ) ) ;
#199931 = CARTESIAN_POINT ( 'NONE',  ( 3.228005407155889461, 1.895358990768666096, 0.4226955006484037214 ) ) ;
#199934 = ORIENTED_EDGE ( 'NONE', *, *, #126711, .T. ) ;
#199933 = CARTESIAN_POINT ( 'NONE',  ( -3.526529353330355221, 6.168015774643768268, -1.082531754730546636 ) ) ;
#199932 = CARTESIAN_POINT ( 'NONE',  ( -9.070041577417988776, 12.56517035942090388, 1.082531754730558626 ) ) ;
#199935 = CARTESIAN_POINT ( 'NONE',  ( -3.946832114909637479, 7.618738210787614484, 0.7216878364870338292 ) ) ;
#199936 = CARTESIAN_POINT ( 'NONE',  ( 4.167152111353856547, 5.955039778036558040, 1.599625672291262513 ) ) ;
#199937 = CARTESIAN_POINT ( 'NONE',  ( -4.305596300791617814, 7.180890229968955651, 1.199719254218452935 ) ) ;
#199938 = CARTESIAN_POINT ( 'NONE',  ( -4.945692173934974178, 8.992000979557944973, 0.000000000000000000 ) ) ;
#199939 = CARTESIAN_POINT ( 'NONE',  ( -8.907343734053998929, 12.37535620882957588, 1.082531754730558626 ) ) ;
#199940 = CARTESIAN_POINT ( 'NONE',  ( 0.3236265600991515834, -0.1057403636935544400, 2.204373366691187108 ) ) ;
#199941 = CARTESIAN_POINT ( 'NONE',  ( -3.285556943750000514, -3.988541666188710089, -1.896917185911906500 ) ) ;
#199942 = ADVANCED_FACE ( 'NONE', ( #166481 ), #119938, .T. ) ;
#199943 = CARTESIAN_POINT ( 'NONE',  ( 4.838696733575553743, -1.901848327180942766, -0.4805237247276354928 ) ) ;
#199944 =( BOUNDED_SURFACE ( )  B_SPLINE_SURFACE ( 3, 3, ( 
 ( #99189, #2705, #564, #69838, #50428, #53622, #119754, #116547, #35222, #85051, #86122 ),
 ( #169502, #150068, #185733, #184669, #21084, #200904, #87187, #213958, #101298, #82916, #182539 ),
 ( #34166, #151138, #115489, #68779, #100237, #134898, #102367, #197731, #1640, #67698, #165240 ),
 ( #131726, #133845, #49371, #16833, #148989, #73054, #203044, #107780, #139153, #24299, #4827 ),
 ( #57888, #141325, #74148, #89342, #55751, #75214, #125115, #106696, #205183, #138085, #190017 ),
 ( #56824, #204099, #23230, #120835, #121907, #124051, #70907, #186811, #172721, #173805, #105602 ),
 ( #137017, #41669, #26451, #54685, #170564, #122994, #187876, #39503, #171633, #38439, #154329 ) ),
 .UNSPECIFIED., .T., .F., .T. ) 
 B_SPLINE_SURFACE_WITH_KNOTS ( ( 4, 3, 4 ),
 ( 4, 1, 1, 1, 1, 1, 1, 1, 4 ),
 ( 0.000000000000000000, 0.5000000000000000000, 1.000000000000000000 ),
 ( 0.000000000000000000, 0.2256926809922864541, 0.3979886288388991278, 0.5260859906349554249, 0.6192013483571605637, 0.6864504996671639825, 0.7364865548622955282, 0.7772638159577213157, 1.000000000000000000 ),
 .UNSPECIFIED. ) 
 GEOMETRIC_REPRESENTATION_ITEM ( )  RATIONAL_B_SPLINE_SURFACE ( (
 ( 1.000000000000000222, 1.000000000000000222, 0.9999999999999997780, 1.000000000000000222, 0.9999999999999996669, 1.000000000000000000, 1.000000000000000222, 0.9999999999999996669, 1.000000000000000444, 1.000000000000000222, 1.000000000000000222),
 ( 0.3333333333333334259, 0.3333333333333334259, 0.3333333333333333148, 0.3333333333333333703, 0.3333333333333333703, 0.3333333333333332593, 0.3333333333333334814, 0.3333333333333332038, 0.3333333333333335924, 0.3333333333333334259, 0.3333333333333334259),
 ( 0.3333333333333334259, 0.3333333333333334259, 0.3333333333333333148, 0.3333333333333333703, 0.3333333333333333703, 0.3333333333333332593, 0.3333333333333334814, 0.3333333333333332038, 0.3333333333333335924, 0.3333333333333334259, 0.3333333333333334259),
 ( 1.000000000000000222, 1.000000000000000222, 0.9999999999999997780, 1.000000000000000222, 0.9999999999999996669, 1.000000000000000000, 1.000000000000000222, 0.9999999999999996669, 1.000000000000000444, 1.000000000000000222, 1.000000000000000222),
 ( 0.3333333333333334259, 0.3333333333333334259, 0.3333333333333333148, 0.3333333333333333703, 0.3333333333333333703, 0.3333333333333332593, 0.3333333333333334814, 0.3333333333333332038, 0.3333333333333335924, 0.3333333333333334259, 0.3333333333333334259),
 ( 0.3333333333333334259, 0.3333333333333334259, 0.3333333333333333148, 0.3333333333333333703, 0.3333333333333333703, 0.3333333333333332593, 0.3333333333333334814, 0.3333333333333332038, 0.3333333333333335924, 0.3333333333333334259, 0.3333333333333334259),
 ( 1.000000000000000222, 1.000000000000000222, 0.9999999999999997780, 1.000000000000000222, 0.9999999999999996669, 1.000000000000000000, 1.000000000000000222, 0.9999999999999996669, 1.000000000000000444, 1.000000000000000222, 1.000000000000000222) ) ) 
 REPRESENTATION_ITEM ( '' )  SURFACE ( )  );
#199945 = CARTESIAN_POINT ( 'NONE',  ( 2.285779929129946098, 1.617817622347239803, -1.203354541732377658 ) ) ;
#199946 = ORIENTED_EDGE ( 'NONE', *, *, #38172, .T. ) ;
#199947 = CARTESIAN_POINT ( 'NONE',  ( 2.923186261301851996, -1.865062457072470536, 1.002408848433397726 ) ) ;
#199948 = CARTESIAN_POINT ( 'NONE',  ( 0.7499999999999885647, 3.097916667349487341, -1.299038105676658228 ) ) ;
#199950 = CARTESIAN_POINT ( 'NONE',  ( -4.232116505760120440, 8.089219690028791376, -0.7998128361456281477 ) ) ;
#199949 = CARTESIAN_POINT ( 'NONE',  ( 0.1747926744264677035, 1.388892567315727744, -2.112808070315982167 ) ) ;
#199951 = CARTESIAN_POINT ( 'NONE',  ( 2.800538183361205302, 1.555518290611109800, 0.9846574483025126723 ) ) ;
#199952 = ORIENTED_EDGE ( 'NONE', *, *, #97607, .F. ) ;
#199953 = UNCERTAINTY_MEASURE_WITH_UNIT (LENGTH_MEASURE( 1.000000000000000082E-05 ), #135717, 'distance_accuracy_value', 'NONE');
#199954 = CARTESIAN_POINT ( 'NONE',  ( -7.995557903757128493, 10.35123685918189729, 1.599625672291295375 ) ) ;
#199955 = FACE_OUTER_BOUND ( 'NONE', #182807, .T. ) ;
#199956 = CARTESIAN_POINT ( 'NONE',  ( 5.080389167821143026, 1.047295930500062866, 1.843893106414703054 ) ) ;
#199957 = CARTESIAN_POINT ( 'NONE',  ( -0.2104748580754166598, -0.006608320950483163522, -2.103482951484026753 ) ) ;
#199958 = CARTESIAN_POINT ( 'NONE',  ( 7.447506452608354088, 7.583179037664891098, 0.7998128361456341429 ) ) ;
#199959 = CARTESIAN_POINT ( 'NONE',  ( 5.518845395222173877, 1.902436629287082237, 0.7926794616768815249 ) ) ;
#199961 = CARTESIAN_POINT ( 'NONE',  ( 2.208333698829296310, 1.645431377724184463, 0.8263914577605266931 ) ) ;
#199960 = CARTESIAN_POINT ( 'NONE',  ( 1.029495724655055344, 1.794938190532389788, -0.4914328765713778524 ) ) ;
#199962 = CARTESIAN_POINT ( 'NONE',  ( 9.921869487102386032, 10.46993591124128997, 0.000000000000000000 ) ) ;
#199963 = CARTESIAN_POINT ( 'NONE',  ( 3.179715765502636682, 5.975770656120749535, 2.499999999999999556 ) ) ;
#199964 = DIRECTION ( 'NONE',  ( 8.638326563840814399E-31, -0.000000000000000000, 1.000000000000000000 ) ) ;
#199965 = VECTOR ( 'NONE', #185441, 1000.000000000000000 ) ;
#199966 = CARTESIAN_POINT ( 'NONE',  ( 2.297764732281985633, 1.706874461811638044, 1.398895601573101111 ) ) ;
#199967 = CARTESIAN_POINT ( 'NONE',  ( 4.499490165225078719, 1.813563011714003803, 1.352382200441957227 ) ) ;
#199968 = CARTESIAN_POINT ( 'NONE',  ( -8.039621903223732602, 8.481906429956900695, 1.040834085586084257E-14 ) ) ;
#199969 = CARTESIAN_POINT ( 'NONE',  ( 4.166123871162411341, 1.811061351045451850, -0.05074819156030555695 ) ) ;
#199970 = CARTESIAN_POINT ( 'NONE',  ( 5.085127819360848456, 1.569905733240322343, 1.097627489654330990 ) ) ;
#199971 = CARTESIAN_POINT ( 'NONE',  ( 11.33772463945036790, 19.00000000000000000, -3.680000000000002824 ) ) ;
#199972 = CARTESIAN_POINT ( 'NONE',  ( 3.625814716899962153, -1.173175478197308053, -1.584272814160747833 ) ) ;
#199973 = CARTESIAN_POINT ( 'NONE',  ( 4.821099876132087125, -0.09137817997613774390, 1.868553921495450965 ) ) ;
#199974 = CARTESIAN_POINT ( 'NONE',  ( 5.336322170104328855, -1.033901835001526104, 1.547212704913742520 ) ) ;
#199975 = CARTESIAN_POINT ( 'NONE',  ( -0.6823417656250212460, 5.301041667008086655, 1.181850606188767472 ) ) ;
#199976 = B_SPLINE_CURVE_WITH_KNOTS ( 'NONE', 3,
 ( #113314, #213899, #33052, #65522, #133786, #150008, #131667, #82857, #99130, #198721, #50367, #67639, #49314, #100179, #51439, #29867 ),
 .UNSPECIFIED., .F., .F.,
 ( 4, 3, 3, 3, 3, 4 ),
 ( 0.000000000000000000, 1.583418202669895186E-05, 3.180857839710038795E-05, 4.638200804740730851E-05, 6.757612010261591353E-05, 9.484161822725196631E-05 ),
 .UNSPECIFIED. ) ;
#199977 = AXIS2_PLACEMENT_3D ( 'NONE', #2171, #151674, #134381 ) ;
#199978 = CARTESIAN_POINT ( 'NONE',  ( 0.6027503803631119039, 1.865048444749048739, 0.7672877736318934883 ) ) ;
#199980 = CARTESIAN_POINT ( 'NONE',  ( 1.330846195043289493, 2.030104276556158549, 0.5602782565924493419 ) ) ;
#199979 = CARTESIAN_POINT ( 'NONE',  ( -9.130526383799315582, 12.73969898348616070, 1.199719254218462483 ) ) ;
#199981 = CARTESIAN_POINT ( 'NONE',  ( 10.01963921569910632, 11.64833282552586091, 1.199719254218450271 ) ) ;
#199983 = CARTESIAN_POINT ( 'NONE',  ( 0.07479286986305369589, 0.2526433113205875935, -1.890777245541554796 ) ) ;
#199982 = DIRECTION ( 'NONE',  ( -1.276756478318932585E-15, 1.000000000000000000, -1.665334536937738262E-16 ) ) ;
#199984 = CARTESIAN_POINT ( 'NONE',  ( 3.428091063814618700, -2.088597262255381448, 0.3661859999234198249 ) ) ;
#199985 = CYLINDRICAL_SURFACE ( 'NONE', #162056, 0.08000000000000020983 ) ;
#199986 = CARTESIAN_POINT ( 'NONE',  ( 1.793229165239007994, -0.1032543025433537293, -2.017296481459893709 ) ) ;
#199987 = CARTESIAN_POINT ( 'NONE',  ( -1.402160292154681736E-14, 2.446875000341416584, -1.575800808251660134 ) ) ;
#199988 = DIRECTION ( 'NONE',  ( 1.039099362110107450E-15, 1.000000000000000000, -4.583713267641621330E-32 ) ) ;
#199989 = CARTESIAN_POINT ( 'NONE',  ( 3.985207087413062066, 6.736826471035503694, -1.199719254218452047 ) ) ;
#199990 = ORIENTED_EDGE ( 'NONE', *, *, #158684, .F. ) ;
#199991 = CARTESIAN_POINT ( 'NONE',  ( 2.530746307392011563, 2.096003997654236173, 0.5278882200696957128 ) ) ;
#199994 = DIRECTION ( 'NONE',  ( 1.000000000000000000, 0.000000000000000000, 0.000000000000000000 ) ) ;
#199993 = CARTESIAN_POINT ( 'NONE',  ( 11.89197816957260478, 9.799999999999998934, -0.8055420615339534685 ) ) ;
#199992 = CARTESIAN_POINT ( 'NONE',  ( 3.549202351727371862, 7.362762853649070571, -0.7998128361456362523 ) ) ;
#199995 = DIRECTION ( 'NONE',  ( 0.000000000000000000, -0.000000000000000000, 1.000000000000000000 ) ) ;
#199996 = FACE_OUTER_BOUND ( 'NONE', #38374, .T. ) ;
#199997 = CARTESIAN_POINT ( 'NONE',  ( -7.754900677336769022, 9.110100880723427608, 1.082531754730558626 ) ) ;
#199998 = CARTESIAN_POINT ( 'NONE',  ( 1.171705676731093604, 1.309414992938146893, 1.757219779060022580 ) ) ;
#199999 = CARTESIAN_POINT ( 'NONE',  ( -0.4655726814510630640, -8.186910006429405584, -9.501690549794776786 ) ) ;
#200001 = CARTESIAN_POINT ( 'NONE',  ( -1.364683531250000748, 12.35937500034139980, 0.000000000000000000 ) ) ;
#200000 = CARTESIAN_POINT ( 'NONE',  ( 1.376233744030544104, 1.349093794351564624, 1.816168808025316661 ) ) ;
#200002 = CARTESIAN_POINT ( 'NONE',  ( -7.486073373039941359, 11.88550270185529278, -0.7998128361456291469 ) ) ;
#200003 = CARTESIAN_POINT ( 'NONE',  ( 4.382046175016578005, -2.016188710442788246, -0.04465648322755921829 ) ) ;
#200004 = CARTESIAN_POINT ( 'NONE',  ( -4.812781342726871969, 6.637997537979888563, 1.443375672974064550 ) ) ;
#200005 = CARTESIAN_POINT ( 'NONE',  ( 1.364683531249986537, 2.467708333674753174, -0.7879004041258239610 ) ) ;
#200006 = CARTESIAN_POINT ( 'NONE',  ( 4.637309883081485395, 8.320457421531981979, 0.4059539251603030974 ) ) ;
#200007 = CARTESIAN_POINT ( 'NONE',  ( 0.7500000000000006661, 9.333333333333332149, 1.299038105676657340 ) ) ;
#200008 = CARTESIAN_POINT ( 'NONE',  ( 4.283650633623343751, 1.129305773815322711, 1.303882612223838500 ) ) ;
#200009 = CARTESIAN_POINT ( 'NONE',  ( 2.878073747850912412, 6.579779482459851003, -0.7998128361456362523 ) ) ;
#200010 = CARTESIAN_POINT ( 'NONE',  ( 2.336827959689928846, -1.583187595272864900, 0.7909824253358921364 ) ) ;
#200011 = CARTESIAN_POINT ( 'NONE',  ( 5.069440727656137291, 0.2206807655098403653, -2.195719112144229879 ) ) ;
#200012 = ORIENTED_EDGE ( 'NONE', *, *, #100151, .T. ) ;
#200013 = CARTESIAN_POINT ( 'NONE',  ( 4.640881595473839383, 1.934004784890541062, 0.5824627899903914718 ) ) ;
#200014 = CARTESIAN_POINT ( 'NONE',  ( -4.827585214917754719, 7.789877296449459365, -1.199719254218453823 ) ) ;
#200015 = CARTESIAN_POINT ( 'NONE',  ( 4.851185501729457172, 0.1948232160459452411, -2.006962824030594561 ) ) ;
#200016 = VERTEX_POINT ( 'NONE', #197900 ) ;
#200017 = MECHANICAL_DESIGN_GEOMETRIC_PRESENTATION_REPRESENTATION (  '', ( #175935 ), #117071 ) ;
#200018 = CARTESIAN_POINT ( 'NONE',  ( 2.272138710904994863, -1.152746988206950096, 1.473173409640892384 ) ) ;
#200019 = FACE_OUTER_BOUND ( 'NONE', #113455, .T. ) ;
#200020 = CARTESIAN_POINT ( 'NONE',  ( 2.074333847954575205, 0.8209984392052707136, 1.727357542596375861 ) ) ;
#200021 = CYLINDRICAL_SURFACE ( 'NONE', #102036, 0.08000000000000020983 ) ;
#200022 = CARTESIAN_POINT ( 'NONE',  ( -10.55260481140867235, 5.124873218919925755, -7.009574331923702495 ) ) ;
#200023 = CARTESIAN_POINT ( 'NONE',  ( 4.950135482320912494, 6.868520377498098739, -1.443375672974068769 ) ) ;
#200024 = CARTESIAN_POINT ( 'NONE',  ( -1.001543065824772872E-14, 4.884375000341420581, 1.575800808251672791 ) ) ;
#200025 = CARTESIAN_POINT ( 'NONE',  ( 0.6680393924826667496, 1.910109291395128972, -0.09634788558426229943 ) ) ;
#200026 = CARTESIAN_POINT ( 'NONE',  ( 6.699137298928158124, 6.988284068270579574, 0.7216878364870328300 ) ) ;
#200027 = CARTESIAN_POINT ( 'NONE',  ( 2.137090596337941406, -0.09316805448006218460, -1.959763546484971197 ) ) ;
#200028 = FACE_OUTER_BOUND ( 'NONE', #104599, .T. ) ;
#200029 = CARTESIAN_POINT ( 'NONE',  ( -5.041653019435350380, 6.975290837464928728, -1.599625672291271394 ) ) ;
#200030 = CARTESIAN_POINT ( 'NONE',  ( 5.537388447972660721, -0.05000006065614125139, 2.120159173171487055 ) ) ;
#200032 = DIRECTION ( 'NONE',  ( -1.000000000000000000, 5.578564026256504688E-16, 0.000000000000000000 ) ) ;
#200031 = CARTESIAN_POINT ( 'NONE',  ( 9.368847842243145152, 10.88907622316056312, 1.199719254218453823 ) ) ;
#200033 = CARTESIAN_POINT ( 'NONE',  ( 6.766873944267649321, -1.801439555086775002, -0.8010921537245048185 ) ) ;
#200034 = CARTESIAN_POINT ( 'NONE',  ( 1.364683531249988757, 2.134375000341422357, 1.214306433183764966E-14 ) ) ;
#200035 = CARTESIAN_POINT ( 'NONE',  ( 1.793228464370033581, -0.1031022715946017104, -2.010704963445380411 ) ) ;
#200036 = VERTEX_POINT ( 'NONE', #134021 ) ;
#200038 = CARTESIAN_POINT ( 'NONE',  ( 1.300578652796330115, 1.418844934001600944, -1.571659118156268908 ) ) ;
#200037 = CARTESIAN_POINT ( 'NONE',  ( -6.995644074971465010, 10.14503993989993091, 1.082531754730549967 ) ) ;
#200040 = EDGE_CURVE ( 'NONE', #80409, #138814, #96129, .T. ) ;
#200039 = CARTESIAN_POINT ( 'NONE',  ( 9.280199541404417829, 11.48923774938119635, 7.537149123760571889 ) ) ;
#200041 = CARTESIAN_POINT ( 'NONE',  ( 3.156751980976373329, -0.5984545454679365273, -1.982000093670479135 ) ) ;
#200042 = CARTESIAN_POINT ( 'NONE',  ( 5.890091390494168522, 5.836471141856793388, 0.000000000000000000 ) ) ;
#200043 = CARTESIAN_POINT ( 'NONE',  ( 5.435893244436359240, 5.306573304789342416, -0.7998128361456481317 ) ) ;
#200044 = VERTEX_POINT ( 'NONE', #68952 ) ;
#200046 = CARTESIAN_POINT ( 'NONE',  ( 4.891794496432329886, 4.601515088792824670, -0.7998128361456211532 ) ) ;
#200045 = CARTESIAN_POINT ( 'NONE',  ( 5.068349447220681370, -1.968310418947304408, -0.7050240649949056637 ) ) ;
#200049 = ORIENTED_EDGE ( 'NONE', *, *, #161384, .F. ) ;
#200048 = CARTESIAN_POINT ( 'NONE',  ( 2.367557981294612812, 0.4819373766774863177, -1.746117998840409191 ) ) ;
#200047 = CARTESIAN_POINT ( 'NONE',  ( 2.977373796215293300, 1.734057503958493118, -0.5710112477543202170 ) ) ;
#200050 = CARTESIAN_POINT ( 'NONE',  ( 6.621690180768193379, -2.141820631849135292, 0.5315211216728524812 ) ) ;
#200051 = CIRCLE ( 'NONE', #41001, 3.970406073902761790 ) ;
#200052 = CARTESIAN_POINT ( 'NONE',  ( 0.7499999999999885647, 2.816666666666689522, -1.299038105676658228 ) ) ;
#200053 = CARTESIAN_POINT ( 'NONE',  ( 9.267535596873369030, 13.53505500093428893, -6.807038118641733249 ) ) ;
#200054 = CARTESIAN_POINT ( 'NONE',  ( 5.684669477433477169, -2.151827843693389308, -0.4886931181809702207 ) ) ;
#200055 = CARTESIAN_POINT ( 'NONE',  ( -1.364683531250014514, 9.651041667008064096, -0.7879004041258335089 ) ) ;
#200056 = EDGE_LOOP ( 'NONE', ( #176289, #107237, #26137, #85317 ) ) ;
#200057 = CARTESIAN_POINT ( 'NONE',  ( 3.914637684252043393, -0.6027250981219151038, -1.814865640613130271 ) ) ;
#200058 = CARTESIAN_POINT ( 'NONE',  ( -4.460796234096120472, 5.163016013655583158, 1.199719254218462483 ) ) ;
#200059 = CARTESIAN_POINT ( 'NONE',  ( 7.793239369756836510, 7.986534107671458216, 0.7998128361456341429 ) ) ;
#200060 = CARTESIAN_POINT ( 'NONE',  ( -1.360316468750032204, 0.6718750003414097893, -2.081668171172168513E-14 ) ) ;
#200061 = CARTESIAN_POINT ( 'NONE',  ( 4.270455198180219902, 6.965652916976816655, -1.082531754730548412 ) ) ;
#200062 = CARTESIAN_POINT ( 'NONE',  ( -11.94105721237523277, 19.00000000000000000, -1.187919463087249827 ) ) ;
#200063 = CARTESIAN_POINT ( 'NONE',  ( 8.381179344826065858, 14.06946724413340100, -8.588858344356935959 ) ) ;
#200064 = CARTESIAN_POINT ( 'NONE',  ( -9.483257663143223937, -6.709848117146014701, 0.3912817730721166454 ) ) ;
#200065 = AXIS2_PLACEMENT_3D ( 'NONE', #126023, #142227, #57744 ) ;
#200066 = DIRECTION ( 'NONE',  ( 0.000000000000000000, 0.000000000000000000, 1.000000000000000000 ) ) ;
#200067 = CARTESIAN_POINT ( 'NONE',  ( 4.006994748872731549, 1.602975652146242380, 0.9638501484771769823 ) ) ;
#200068 = CARTESIAN_POINT ( 'NONE',  ( 7.614839552730775729, 8.913009562054615031, 1.199719254218452047 ) ) ;
#200069 = CARTESIAN_POINT ( 'NONE',  ( 10.50000000000000178, 10.19999999999998153, 3.599999999999999201 ) ) ;
#200070 = EDGE_CURVE ( 'NONE', #191630, #122458, #85224, .T. ) ;
#200071 = CARTESIAN_POINT ( 'NONE',  ( -6.941411460516810017, 8.161030127766803588, 1.082531754730549967 ) ) ;
#200072 = CARTESIAN_POINT ( 'NONE',  ( 4.137209430464448445, 7.978494768850520558, 1.040834085586084257E-14 ) ) ;
#200073 = CARTESIAN_POINT ( 'NONE',  ( 0.3386328343033001564, -1.908876393446774955, -0.4841592594212947298 ) ) ;
#200074 = CARTESIAN_POINT ( 'NONE',  ( 1.722280025409760329, 1.994874335020242695, 0.2930476355553628953 ) ) ;
#200075 = CARTESIAN_POINT ( 'NONE',  ( -9.671043645249580933, 10.17730576241299900, 0.7998128361456462443 ) ) ;
#200076 = CARTESIAN_POINT ( 'NONE',  ( 4.844006021832467646, 8.873367135438366304, 0.000000000000000000 ) ) ;
#200077 = LINE ( 'NONE', #185964, #80652 ) ;
#200078 = CARTESIAN_POINT ( 'NONE',  ( 3.064592470464472473, -2.024993410009158890, -0.8382372354380845936 ) ) ;
#200079 = CARTESIAN_POINT ( 'NONE',  ( 6.059193749186201572, -1.568369423792463024, -0.9343120793870243190 ) ) ;
#200080 = CARTESIAN_POINT ( 'NONE',  ( -2.923754682041362241, 6.562797562356882608, 0.7998128361456341429 ) ) ;
#200081 = CARTESIAN_POINT ( 'NONE',  ( 5.912764389335563919, 6.070849007079172743, -0.7216878364870458196 ) ) ;
#200082 = CARTESIAN_POINT ( 'NONE',  ( 7.584896871841365851, 10.93646455286856956, -1.199719254218446718 ) ) ;
#200083 = CARTESIAN_POINT ( 'NONE',  ( 7.051649292883499953, 7.399548061218447437, -0.7216878364870317197 ) ) ;
#200084 = ORIENTED_EDGE ( 'NONE', *, *, #121881, .T. ) ;
#200086 = CARTESIAN_POINT ( 'NONE',  ( 0.5924399621960573237, -1.116526876179738226, 1.674895298907061569 ) ) ;
#200085 = CARTESIAN_POINT ( 'NONE',  ( 3.966218424140379728, -1.719484690100345325, -0.6589542199007536460 ) ) ;
#200087 = CARTESIAN_POINT ( 'NONE',  ( 3.304404366906594337, -2.028264134497267168, 1.081039266028597234 ) ) ;
#200089 = CARTESIAN_POINT ( 'NONE',  ( 1.111883761159220496, 1.859168010044176311, -0.08395930885315286418 ) ) ;
#200088 = CARTESIAN_POINT ( 'NONE',  ( 2.399429999938675007, 5.743159399996332404, 0.000000000000000000 ) ) ;
#200090 = CARTESIAN_POINT ( 'NONE',  ( -1.642778471874998480, -3.201041666188710000, 2.845375778867863303 ) ) ;
#200091 = CARTESIAN_POINT ( 'NONE',  ( -4.042302355168801320, 7.867769847672247074, 0.7998128361456341429 ) ) ;
#200092 =( NAMED_UNIT ( * ) PLANE_ANGLE_UNIT ( ) SI_UNIT ( $, .RADIAN. ) );
#200093 = CARTESIAN_POINT ( 'NONE',  ( 4.482611839828003930, -1.244964735940889522, 1.451779576051547282 ) ) ;
#200094 = CARTESIAN_POINT ( 'NONE',  ( -8.109748439268576803, 12.61312361245537517, 0.7998128361456481317 ) ) ;
#200095 = CARTESIAN_POINT ( 'NONE',  ( 6.119462805442048570, 6.996221746119736018, -0.9567421715909133484 ) ) ;
#200096 = CARTESIAN_POINT ( 'NONE',  ( -6.672020991700860826, 7.917017590806697314, 1.082531754730549078 ) ) ;
#200098 = CARTESIAN_POINT ( 'NONE',  ( 2.236979667955760309, -1.672073921526989748, 0.8388852543278202401 ) ) ;
#200097 = CARTESIAN_POINT ( 'NONE',  ( 4.300388110500093397, 1.614917507917512207, -1.327843252744983049 ) ) ;
#200099 = CARTESIAN_POINT ( 'NONE',  ( 8.107412671292042461, 9.521364873671299023, 1.082531754730558626 ) ) ;
#200100 = CARTESIAN_POINT ( 'NONE',  ( 3.177206141917392923, 8.963489737286291614, 2.500000000000000888 ) ) ;
#200101 = CARTESIAN_POINT ( 'NONE',  ( 3.052039328023182119, -1.315916573227500219, 1.139148930295554862 ) ) ;
#200102 = CARTESIAN_POINT ( 'NONE',  ( 5.657830175604453338, 5.495223381160312393, 0.7998128361456341429 ) ) ;
#200103 = CARTESIAN_POINT ( 'NONE',  ( -1.115562610750309283E-14, 11.59375000068279604, 1.500000000000001554 ) ) ;
#200104 = CARTESIAN_POINT ( 'NONE',  ( 4.090264520950432470, -1.706510830129988499, -0.2501320830878352997 ) ) ;
#200105 = CARTESIAN_POINT ( 'NONE',  ( -7.039708073993679704, 9.236078724457858158, 1.599625672291283607 ) ) ;
#200106 = CARTESIAN_POINT ( 'NONE',  ( 6.322910218073367616, 2.057572540570989261, 0.7984293639632376038 ) ) ;
#200107 = CARTESIAN_POINT ( 'NONE',  ( -1.387358672534977355, 7.315968950353621381, -4.254625267138091971 ) ) ;
#200108 = VECTOR ( 'NONE', #103959, 1000.000000000000000 ) ;
#200109 = CARTESIAN_POINT ( 'NONE',  ( 9.578284150245949036, -9.932867526282002757, -0.1622940087187645097 ) ) ;
#200110 = CARTESIAN_POINT ( 'NONE',  ( 3.063509990063197019, 1.831722579244631666, 1.165231348177008242 ) ) ;
#200111 = CARTESIAN_POINT ( 'NONE',  ( 1.928079105319381314, 1.052063804484974385, -1.491885150056403431 ) ) ;
#200112 = CARTESIAN_POINT ( 'NONE',  ( 0.4792544977638459880, -0.1021076105021078151, 1.959249876678282209 ) ) ;
#200113 = CARTESIAN_POINT ( 'NONE',  ( 5.173117096678320870, 1.865890646727845326, -1.000864459693462383 ) ) ;
#200114 = VERTEX_POINT ( 'NONE', #135073 ) ;
#200116 = CARTESIAN_POINT ( 'NONE',  ( 1.364683531249988535, 2.926041667008082658, 0.7879004041258500513 ) ) ;
#200115 = CARTESIAN_POINT ( 'NONE',  ( 5.530919501969752794, -2.073650524585127997, 0.9775372349926645388 ) ) ;
#200117 = CARTESIAN_POINT ( 'NONE',  ( 8.055515824813896941, 12.54985222892493368, 0.7998128361456462443 ) ) ;
#200118 = CARTESIAN_POINT ( 'NONE',  ( 1.067215373428985092, -1.669322716927954753, 1.307481345630675529 ) ) ;
#200119 = CARTESIAN_POINT ( 'NONE',  ( -4.392478581147607031, 7.108013530438723748, 1.082531754730560403 ) ) ;
#200120 = CARTESIAN_POINT ( 'NONE',  ( 3.145128448690309053, 4.692402494937224056, -1.443375672974057666 ) ) ;
#200121 = CARTESIAN_POINT ( 'NONE',  ( -6.710922848640111127, 6.931757532942661726, 0.7216878364870317197 ) ) ;
#200122 = VECTOR ( 'NONE', #132774, 1000.000000000000000 ) ;
#200123 = CARTESIAN_POINT ( 'NONE',  ( 6.420782495146515778, -1.541274310347956922, 1.529322475779694601 ) ) ;
#200125 = CARTESIAN_POINT ( 'NONE',  ( -0.7500000000000006661, 12.23958333401613174, -1.299038105676657340 ) ) ;
#200124 = CARTESIAN_POINT ( 'NONE',  ( -1.420000000000021911, 7.176846818246207960, 4.202462424328227364 ) ) ;
#200127 = ORIENTED_EDGE ( 'NONE', *, *, #107456, .T. ) ;
#200126 = CARTESIAN_POINT ( 'NONE',  ( 1.594693315975799441, -1.184698573716694847, 1.878835628132907054 ) ) ;
#200128 = CARTESIAN_POINT ( 'NONE',  ( 6.592432824109000222, -0.4393352932590722792, 1.975308225066509049 ) ) ;
#200130 = CARTESIAN_POINT ( 'NONE',  ( 4.698127260392297444, 0.8867148737545665904, -1.862399597460895784 ) ) ;
#200129 = CARTESIAN_POINT ( 'NONE',  ( 4.847203612085560387, 5.613824621309978724, -1.199719254218452047 ) ) ;
#200132 = CARTESIAN_POINT ( 'NONE',  ( -6.251718229232856139, 6.466295153626024472, -0.7216878364870422669 ) ) ;
#200131 = CARTESIAN_POINT ( 'NONE',  ( 6.692885107001518286, 7.837396042037102717, -1.199719254218452047 ) ) ;
#200133 = CARTESIAN_POINT ( 'NONE',  ( 7.713663051532233972, 7.963971413067895355, -0.7998128361456341429 ) ) ;
#200134 = CARTESIAN_POINT ( 'NONE',  ( -3.285556943750000070, -0.4593749995220435256, 0.000000000000000000 ) ) ;
#200135 = CARTESIAN_POINT ( 'NONE',  ( -9.579665964935227151, -7.246166700194470067, 0.000000000000000000 ) ) ;
#200136 = CARTESIAN_POINT ( 'NONE',  ( 1.025464405625675646, -1.327728713622891688, -1.614889332886438655 ) ) ;
#200137 = CARTESIAN_POINT ( 'NONE',  ( 4.641250102003463773, 0.7743139518727223392, 1.862017545363145565 ) ) ;
#200138 = CARTESIAN_POINT ( 'NONE',  ( 4.757273854911123756, 1.820453720981948242, -0.2752165127944474210 ) ) ;
#200139 = CARTESIAN_POINT ( 'NONE',  ( 4.168242161197552420, 6.950367390450747251, -1.199719254218452047 ) ) ;
#200140 = CARTESIAN_POINT ( 'NONE',  ( 0.7094338256347174632, -1.717145877019264022, 0.1620263704987124354 ) ) ;
#200141 = CARTESIAN_POINT ( 'NONE',  ( 0.2903707658989269080, -5.254568858751053284, 10.97058181929407894 ) ) ;
#200142 = CARTESIAN_POINT ( 'NONE',  ( -6.600121851754250812, 6.594563670001734046, 0.7998128361456341429 ) ) ;
#200143 = CARTESIAN_POINT ( 'NONE',  ( 1.669569175971203023, 0.1671416771932125456, -2.256311322606067371 ) ) ;
#200144 = CARTESIAN_POINT ( 'NONE',  ( 3.176497522518567873, -1.254329069944852382, 1.691643483388256985 ) ) ;
#200145 = CARTESIAN_POINT ( 'NONE',  ( -5.285699784481336927, 7.260012063351913625, 1.599625672291263179 ) ) ;
#200146 = CARTESIAN_POINT ( 'NONE',  ( 4.964256800898067645, 8.943383367689749619, 0.7998128361456462443 ) ) ;
#200147 = CARTESIAN_POINT ( 'NONE',  ( 5.329763783503544516, 9.232158490813878515, -0.7216878364870458196 ) ) ;
#200148 = CARTESIAN_POINT ( 'NONE',  ( 5.937500000000004441, 1.451031289060873863, -1.451031289061349927 ) ) ;
#200149 = CARTESIAN_POINT ( 'NONE',  ( -5.250031796989778066, 7.148123067953287446, 1.599625672291267398 ) ) ;
#200150 = CARTESIAN_POINT ( 'NONE',  ( 4.799223189113185128, 8.542918120699967588, 1.040834085586084257E-14 ) ) ;
#200151 = CARTESIAN_POINT ( 'NONE',  ( -1.499999999999997780, 2.150000000000019895, 1.214306433183764966E-14 ) ) ;
#200152 = CARTESIAN_POINT ( 'NONE',  ( -4.298098390732130625, 4.973201863064262263, 1.199719254218462483 ) ) ;
#200153 = CARTESIAN_POINT ( 'NONE',  ( 4.957398421247804166, -1.904820672624758515, 1.142771788014641743 ) ) ;
#200154 = CARTESIAN_POINT ( 'NONE',  ( 3.416156609664961152, 1.390242785425911620, -1.694013327489252152 ) ) ;
#200155 = CARTESIAN_POINT ( 'NONE',  ( -5.005985031943793295, 6.863401842066301661, -1.599625672291256295 ) ) ;
#200157 = TOROIDAL_SURFACE ( 'NONE', #68725, 1.811274280335456677, 0.2000000000000000111 ) ;
#200156 = CARTESIAN_POINT ( 'NONE',  ( -2.986538976760251263, 6.706322249520737522, -0.7998128361456481317 ) ) ;
#200158 = CARTESIAN_POINT ( 'NONE',  ( -1.364683531249997417, 2.759375000341422801, 1.214306433183764966E-14 ) ) ;
#200159 = CARTESIAN_POINT ( 'NONE',  ( 6.609999999999968345, 7.051749200714771959, 2.878153929105996323 ) ) ;
#200160 = CARTESIAN_POINT ( 'NONE',  ( -4.446711195602245148, 7.171284913969171448, -1.082531754730549967 ) ) ;
#200161 = CARTESIAN_POINT ( 'NONE',  ( 4.377262645480927361, -1.895543854172193399, -0.9507902649282941043 ) ) ;
#200162 = CARTESIAN_POINT ( 'NONE',  ( -7.444835747679825033, 7.858265591814152629, 0.000000000000000000 ) ) ;
#200163 = ORIENTED_EDGE ( 'NONE', *, *, #171579, .T. ) ;
#200165 = DIRECTION ( 'NONE',  ( 8.881784197001252323E-16, 0.000000000000000000, -1.000000000000000000 ) ) ;
#200164 = CARTESIAN_POINT ( 'NONE',  ( -4.814553946628611136, 8.631080347793099961, 0.000000000000000000 ) ) ;
#200166 = CARTESIAN_POINT ( 'NONE',  ( 3.669453130792974971, 7.432779085900453886, 1.040834085586084257E-14 ) ) ;
#200167 = CARTESIAN_POINT ( 'NONE',  ( 4.616662711240536510, -0.08544939198026380023, 1.839383977539174264 ) ) ;
#200168 = UNCERTAINTY_MEASURE_WITH_UNIT (LENGTH_MEASURE( 1.000000000000000082E-05 ), #60805, 'distance_accuracy_value', 'NONE');
#200169 = CARTESIAN_POINT ( 'NONE',  ( 1.364683531249988535, 2.926041667008082658, 0.7879004041258500513 ) ) ;
#200170 = CARTESIAN_POINT ( 'NONE',  ( 1.206182128890446403, 1.534490571913693868, 0.8211921505957423539 ) ) ;
#200171 = LINE ( 'NONE', #101626, #142937 ) ;
#200172 = CARTESIAN_POINT ( 'NONE',  ( -0.2981862293453914625, 7.114787932596419395, 1.978802099905853984 ) ) ;
#200173 = CARTESIAN_POINT ( 'NONE',  ( -0.6125000000000089262, 1.791666666666677621, 1.060881119635936232 ) ) ;
#200174 = EDGE_CURVE ( 'NONE', #200016, #182623, #175594, .T. ) ;
#200175 = CARTESIAN_POINT ( 'NONE',  ( 5.383715653711652394, 1.448795075966866852, 1.604530791579752202 ) ) ;
#200176 = CARTESIAN_POINT ( 'NONE',  ( -3.216308754939891212, 4.775446185561722956, -1.599625672291262513 ) ) ;
#200177 = CARTESIAN_POINT ( 'NONE',  ( -8.324343128666356506, 8.814081192973304724, 1.040834085586084257E-14 ) ) ;
#200178 = CARTESIAN_POINT ( 'NONE',  ( 4.188458007013862172, -2.137797052781073237, -0.3198388112101158143 ) ) ;
#200179 = CARTESIAN_POINT ( 'NONE',  ( 0.6823417656249917140, 3.592708333674754506, 1.181850606188765695 ) ) ;
#200180 = CARTESIAN_POINT ( 'NONE',  ( 6.450460791689297757, 0.6159929566152704261, 1.872736359496610659 ) ) ;
#200181 = CARTESIAN_POINT ( 'NONE',  ( 4.587041898695760622, 1.066698363585473652, -1.366732696162711314 ) ) ;
#200182 = CARTESIAN_POINT ( 'NONE',  ( 2.208753784402537335, 1.959192758111829136, 0.9821998110004714899 ) ) ;
#200183 = CARTESIAN_POINT ( 'NONE',  ( 1.975998049093165232, 2.207973392102855925, -0.6707195784038646469 ) ) ;
#200184 = CARTESIAN_POINT ( 'NONE',  ( 5.096976104305405819, 1.715636550957209794, -1.141348886549067077 ) ) ;
#200185 = CARTESIAN_POINT ( 'NONE',  ( 0.2517628464389579102, 0.7423079377118102506, 1.794666626680625932 ) ) ;
#200186 = CARTESIAN_POINT ( 'NONE',  ( -6.602457619730773608, 8.725953194484466380, 1.443375672974078761 ) ) ;
#200187 = CARTESIAN_POINT ( 'NONE',  ( -3.709037541790315640, 6.484905011134099340, -1.199719254218450271 ) ) ;
#200188 = CARTESIAN_POINT ( 'NONE',  ( -5.608113461897637819, 5.663683967803710750, -0.3064300721642960190 ) ) ;
#200189 = DIRECTION ( 'NONE',  ( -0.000000000000000000, -1.000000000000000000, -0.000000000000000000 ) ) ;
#200190 = CARTESIAN_POINT ( 'NONE',  ( 1.020157974382044364, -1.821741137083273010, 0.8647263380179845971 ) ) ;
#200191 = CARTESIAN_POINT ( 'NONE',  ( -5.382223794500827552, 9.223085493652217082, -0.7216878364870207285 ) ) ;
#200192 = CARTESIAN_POINT ( 'NONE',  ( 2.942613154609276638, 2.189964478704994555, 0.2713889102748042736 ) ) ;
#200193 = CARTESIAN_POINT ( 'NONE',  ( 3.285556943750000514, -1.801041666188707424, 1.896917185911906500 ) ) ;
#200194 = CARTESIAN_POINT ( 'NONE',  ( 2.359995855038379720, -1.860683555027684788, 0.03984664071272727565 ) ) ;
#200195 = CARTESIAN_POINT ( 'NONE',  ( 3.475000000000000533, -1.910416665710751749, 2.006292185433948827 ) ) ;
#200196 = CARTESIAN_POINT ( 'NONE',  ( 1.499999999999968914, 4.827083334016150751, -0.8660254037844440367 ) ) ;
#200197 = CARTESIAN_POINT ( 'NONE',  ( -9.500232605408747588, -7.619382996155716015, -0.01181297548859716086 ) ) ;
#200199 = CARTESIAN_POINT ( 'NONE',  ( 6.925078400183531713, -0.004750840071900476122, 2.044148492825672569 ) ) ;
#200198 = CARTESIAN_POINT ( 'NONE',  ( -4.612885993627734216, 8.463679738117141582, -0.3448095128447264957 ) ) ;
#200200 = DIRECTION ( 'NONE',  ( 0.7592566023653005702, 0.6507913734559639396, 0.000000000000000000 ) ) ;
#200201 = VERTEX_POINT ( 'NONE', #86301 ) ;
#200202 = CARTESIAN_POINT ( 'NONE',  ( 3.344654342685839499, 0.4992920947068257842, 1.999368073990233308 ) ) ;
#200203 = CARTESIAN_POINT ( 'NONE',  ( -1.360316468749998675, 2.411458333674741716, 0.7853790794158941324 ) ) ;
#200204 = CARTESIAN_POINT ( 'NONE',  ( -6.891622154448065807, 6.934647356477856128, 1.040834085586084257E-14 ) ) ;
#200205 = CARTESIAN_POINT ( 'NONE',  ( 1.910812834059022469, -0.5409473409442880909, -1.945794739053583466 ) ) ;
#200206 = CARTESIAN_POINT ( 'NONE',  ( 0.7499999999999867883, 0.06666666666668707997, -1.299038105676652899 ) ) ;
#200207 = CIRCLE ( 'NONE', #41149, 6.200000000000000178 ) ;
#200208 = CARTESIAN_POINT ( 'NONE',  ( 2.900554798319789906, 5.471398800426671372, 1.199719254218452047 ) ) ;
#200209 = CARTESIAN_POINT ( 'NONE',  ( 2.149359023125880341, -1.654445155856735905, -1.228624528962230400 ) ) ;
#200211 = CARTESIAN_POINT ( 'NONE',  ( -0.6823417656250039265, 13.81770833367473195, -1.181850606188755259 ) ) ;
#200210 = CARTESIAN_POINT ( 'NONE',  ( 1.252085211431714251, 3.300000000000025135, 0.7750000000000100142 ) ) ;
#200212 = CARTESIAN_POINT ( 'NONE',  ( 4.984594031318565932, 8.967110136513669616, 0.7998128361456462443 ) ) ;
#200213 = CARTESIAN_POINT ( 'NONE',  ( -0.2411972340276204718, 2.032951786628557134, -2.316127775276015655 ) ) ;
#200214 = CARTESIAN_POINT ( 'NONE',  ( 0.2515690823673248921, 0.7017594223384625574, 1.702352774230586618 ) ) ;
#200215 = CARTESIAN_POINT ( 'NONE',  ( 5.848300530743933301, 2.204158087718602221, 0.1119919437090263481 ) ) ;
#200216 = CARTESIAN_POINT ( 'NONE',  ( 5.875479466675786355, 7.948088359245467416, -1.599625672291283607 ) ) ;
#200217 = CARTESIAN_POINT ( 'NONE',  ( 1.212450271513715094, -0.9707322288472041150, -1.931405299116681018 ) ) ;
#200218 = VECTOR ( 'NONE', #16220, 1000.000000000000000 ) ;
#200219 = CARTESIAN_POINT ( 'NONE',  ( -4.853455804012230423, 6.685451076146141425, 1.443375672974064550 ) ) ;
#200220 = CARTESIAN_POINT ( 'NONE',  ( 1.815639016007553730, -1.320828798922760949, -1.523793687088881299 ) ) ;
#200221 = CARTESIAN_POINT ( 'NONE',  ( 1.950936211155746447, 1.584691988697755960, 1.664941613344946836 ) ) ;
#200222 = FILL_AREA_STYLE_COLOUR ( '', #139280 ) ;
#200223 = CARTESIAN_POINT ( 'NONE',  ( 0.1450994221751950586, -1.442925249786636943, -1.190247126510869613 ) ) ;
#200224 = DIRECTION ( 'NONE',  ( -1.224646799147355426E-16, 0.000000000000000000, -1.000000000000000000 ) ) ;
#200225 = CARTESIAN_POINT ( 'NONE',  ( 2.043623373375623942, 0.7184291972081280342, -1.727395513401897453 ) ) ;
#200226 = CARTESIAN_POINT ( 'NONE',  ( 3.731657894805060938, 0.6748485617756972976, -1.900415309456899182 ) ) ;
#200229 = ADVANCED_FACE ( 'NONE', ( #140431 ), #88389, .T. ) ;
#200228 = CARTESIAN_POINT ( 'NONE',  ( 10.18181017373857600, 10.98112607889092907, 0.7216878364870438212 ) ) ;
#200227 = CARTESIAN_POINT ( 'NONE',  ( 0.6823417656249882723, 1.926041667008083991, -1.181850606188749264 ) ) ;
#200231 = CARTESIAN_POINT ( 'NONE',  ( 5.320966398826527666, 1.945490409060679049, 0.8070863781705228668 ) ) ;
#200230 = CARTESIAN_POINT ( 'NONE',  ( -6.028571859570855729, 10.18508426947466816, 0.000000000000000000 ) ) ;
#200232 = CARTESIAN_POINT ( 'NONE',  ( 7.793239369756836510, 7.986534107671458216, 0.7998128361456341429 ) ) ;
#200233 = CARTESIAN_POINT ( 'NONE',  ( -5.865874016206865882, 9.995270118883347266, 0.000000000000000000 ) ) ;
#200234 = CARTESIAN_POINT ( 'NONE',  ( 6.639320575229294086, 0.002105643433562148347, 2.003388605011639179 ) ) ;
#200235 = CARTESIAN_POINT ( 'NONE',  ( 5.537369811128121988, -0.04535447194144863470, 2.019437878860441238 ) ) ;
#200236 = CARTESIAN_POINT ( 'NONE',  ( 1.499999999999987121, -1.214583332650518432, 0.8660254037844524744 ) ) ;
#200237 = CARTESIAN_POINT ( 'NONE',  ( 0.6200784347700560861, 2.040642744413103671, -0.2990284185609564105 ) ) ;
#200238 = CARTESIAN_POINT ( 'NONE',  ( 8.514157279702022407, 10.95626946445095307, -1.443375672974063439 ) ) ;
#200239 = CARTESIAN_POINT ( 'NONE',  ( 5.508355548902068577, 9.648441583686274470, 0.7998128361456331437 ) ) ;
#200240 = CARTESIAN_POINT ( 'NONE',  ( 4.552505719138623341, 8.533283448962240669, 0.7998128361456341429 ) ) ;
#200241 = CARTESIAN_POINT ( 'NONE',  ( -0.6823417656250003738, 0.2802083336747515641, -1.181850606188749264 ) ) ;
#200243 = CARTESIAN_POINT ( 'NONE',  ( -6.326802395788107880, 6.950450678040672514, 0.9045734915664763731 ) ) ;
#200242 = CARTESIAN_POINT ( 'NONE',  ( 5.903649544107831382, 5.852288987739402870, -0.7998128361456481317 ) ) ;
#200244 = CARTESIAN_POINT ( 'NONE',  ( 7.415946836550722843, 8.714654733139752807, 1.082531754730558626 ) ) ;
#200245 = CARTESIAN_POINT ( 'NONE',  ( 2.559224761666531567, 1.745036862030847624, -1.291676481929154408 ) ) ;
#200247 = CARTESIAN_POINT ( 'NONE',  ( 2.454439063956286304, -1.602943312447857593, -0.9057913635923324769 ) ) ;
#200246 = CARTESIAN_POINT ( 'NONE',  ( -5.016153647376219382, 6.875265226737464985, 1.443375672974064550 ) ) ;
#200248 = CARTESIAN_POINT ( 'NONE',  ( -1.201851678989727383E-14, 3.446875000341421469, -1.575800808251660134 ) ) ;
#200249 = CARTESIAN_POINT ( 'NONE',  ( 3.984055765753656164, -2.167877601896048390, -0.3204034371554059235 ) ) ;
#200250 = CARTESIAN_POINT ( 'NONE',  ( 7.704529957180471733, 14.43789495343931506, 9.203201968345597450 ) ) ;
#200251 = CARTESIAN_POINT ( 'NONE',  ( 5.172873261720807747, -2.128565284095069288, -0.7672878325792488186 ) ) ;
#200252 = CARTESIAN_POINT ( 'NONE',  ( -6.880926654135487652, 7.986501503701545879, 1.199719254218450271 ) ) ;
#200253 = CARTESIAN_POINT ( 'NONE',  ( 1.364683531249992088, 5.696875000341418804, 1.214306433183764966E-14 ) ) ;
#200254 = CARTESIAN_POINT ( 'NONE',  ( 5.599868899865946936, 7.382462344760764239, -1.240035354157904779 ) ) ;
#200255 = CARTESIAN_POINT ( 'NONE',  ( -7.065207446052822249, 7.415365906582643163, -0.7216878364870338292 ) ) ;
#200256 = CARTESIAN_POINT ( 'NONE',  ( 5.072158865288243668, 6.050511776658669127, 1.082531754730549078 ) ) ;
#200257 = CARTESIAN_POINT ( 'NONE',  ( 6.520749347316099787, 1.652272609716086249, 0.6344386834381664508 ) ) ;
#200259 = CARTESIAN_POINT ( 'NONE',  ( 4.090493406365951934, -1.157184705539246794, 1.647087716845529126 ) ) ;
#200258 = COLOUR_RGB ( '', 0.66274510, 0.83137255, 0.94901961) ;
#200260 = CARTESIAN_POINT ( 'NONE',  ( 6.500244582748090139, 9.671036882259738121, 1.199719254218460707 ) ) ;
#200261 = CARTESIAN_POINT ( 'NONE',  ( 2.503073473877976518, 1.692030140557040152, -1.253631523096561784 ) ) ;
#200262 = CARTESIAN_POINT ( 'NONE',  ( 0.4388990752801218975, -1.618778001572194647, -1.023919763412997286 ) ) ;
#200264 = CARTESIAN_POINT ( 'NONE',  ( 0.7499999999999885647, 2.816666666666689522, -1.299038105676658228 ) ) ;
#200263 = CARTESIAN_POINT ( 'NONE',  ( 0.6823417656249934904, 11.69270833367473017, 1.181850606188764807 ) ) ;
#200265 = CARTESIAN_POINT ( 'NONE',  ( 2.330458462945466547, -1.214122947426389709, 1.550707797581540204 ) ) ;
#200266 = CARTESIAN_POINT ( 'NONE',  ( 0.7252172114964609007, -1.777616610744123804, 0.5828384007960025759 ) ) ;
#200267 = CARTESIAN_POINT ( 'NONE',  ( 1.398799877119625501, 0.3793605821263335565, 1.924665094374561791 ) ) ;
#200269 = ORIENTED_EDGE ( 'NONE', *, *, #184597, .F. ) ;
#200268 = CARTESIAN_POINT ( 'NONE',  ( -0.08783152977152529350, -1.912005390248720627, -0.04503566501021933483 ) ) ;
#200270 = CARTESIAN_POINT ( 'NONE',  ( 5.666945020832170776, 7.634521829102760115, 1.443375672974062551 ) ) ;
#200271 = CARTESIAN_POINT ( 'NONE',  ( -1.201851678989727383E-14, 0.8843750003414173610, 1.575800808251672791 ) ) ;
#200272 = CARTESIAN_POINT ( 'NONE',  ( 5.453920962983416665, 1.868457504587007545, -0.09292587778651076325 ) ) ;
#200273 = CARTESIAN_POINT ( 'NONE',  ( 9.890836756369282057, 11.49806328964105617, -1.199719254218440723 ) ) ;
#200274 = DIRECTION ( 'NONE',  ( -1.000000000000000000, 0.000000000000000000, 0.000000000000000000 ) ) ;
#200275 = CARTESIAN_POINT ( 'NONE',  ( 5.278213287142951238, -1.102824678039602269, -1.751873656341627505 ) ) ;
#200276 = CIRCLE ( 'NONE', #89620, 0.08000000000000020983 ) ;
#200277 = CARTESIAN_POINT ( 'NONE',  ( 10.00198841338951716, 1.970899860167793616, 6.221464951635504725 ) ) ;
#200278 = CARTESIAN_POINT ( 'NONE',  ( -5.438229012412911345, 5.517224400669388018, -0.7216878364870338292 ) ) ;
#200279 = CARTESIAN_POINT ( 'NONE',  ( 0.1392002015415672034, -0.1474423581745692435, -2.037351525059682977 ) ) ;
#200280 = CARTESIAN_POINT ( 'NONE',  ( 1.499999999999985123, 0.04583333333335545129, -0.8660254037844323793 ) ) ;
#200281 = CARTESIAN_POINT ( 'NONE',  ( 6.726816770674637347, 10.99970333242910669, -0.7998128361456291469 ) ) ;
#200282 = CARTESIAN_POINT ( 'NONE',  ( -9.338868881714763148, 9.789768538289042255, -0.7998128361456291469 ) ) ;
#200283 = CARTESIAN_POINT ( 'NONE',  ( 6.367489420273535039, 7.457767740854454708, -1.199719254218452047 ) ) ;
#200284 = CARTESIAN_POINT ( 'NONE',  ( -1.402160292154681736E-14, 0.9468750003414176941, -1.575800808251659024 ) ) ;
#200285 = CARTESIAN_POINT ( 'NONE',  ( 0.7499999999999885647, 2.066666666666688634, -1.299038105676652899 ) ) ;
#200287 = CARTESIAN_POINT ( 'NONE',  ( 3.497113557321089861, 6.167384019261527683, -1.199719254218446718 ) ) ;
#200286 = CARTESIAN_POINT ( 'NONE',  ( 5.617619635959271385, 0.3843197845415853853, -1.923678648292715732 ) ) ;
#200288 = CARTESIAN_POINT ( 'NONE',  ( 2.688827190807027367, -1.158510681541668141, -1.649829502315000251 ) ) ;
#200289 = CARTESIAN_POINT ( 'NONE',  ( 2.096773827148257219, 1.713186613203399489, 0.8573791853930428086 ) ) ;
#200290 = CARTESIAN_POINT ( 'NONE',  ( -1.907713928855368168, 3.283019769909846897, -0.4154771360143861836 ) ) ;
#200291 = CARTESIAN_POINT ( 'NONE',  ( -0.09381621004311831158, -0.9424329983100244723, -1.976553698157037298 ) ) ;
#200292 = CARTESIAN_POINT ( 'NONE',  ( 0.1333692844072801587, 4.087911462428309051, -2.608372271572469092 ) ) ;
#200293 = CARTESIAN_POINT ( 'NONE',  ( 3.391731324245280010, -0.7611128710301139355, 1.708892184765831157 ) ) ;
#200294 = CARTESIAN_POINT ( 'NONE',  ( 1.499999999999985123, -0.4229166659838508036, -0.8660254037844323793 ) ) ;
#200295 = CARTESIAN_POINT ( 'NONE',  ( -7.965578943228732278, 9.251929174310385307, -1.199719254218446718 ) ) ;
#200297 = CARTESIAN_POINT ( 'NONE',  ( 4.236029508982094072, 2.116713919566749702, -0.05380437090627546853 ) ) ;
#200296 = CARTESIAN_POINT ( 'NONE',  ( -4.338245966692955591, 5.124003718305597310, 1.082531754730560403 ) ) ;
#200299 = EDGE_CURVE ( 'NONE', #116857, #208229, #168605, .T. ) ;
#200298 = DIRECTION ( 'NONE',  ( 0.000000000000000000, -1.000000000000000000, 0.000000000000000000 ) ) ;
#200300 = CARTESIAN_POINT ( 'NONE',  ( 6.109843426155951107, 0.6047356833836557977, -1.980059631771100781 ) ) ;
#200302 = CARTESIAN_POINT ( 'NONE',  ( 6.620655732516610215, 1.221631503675042030, 2.386181433960798071 ) ) ;
#200301 = CARTESIAN_POINT ( 'NONE',  ( 2.032869862874300271, -1.866249813966861515, 0.9426962998228316515 ) ) ;
#200304 = ORIENTED_EDGE ( 'NONE', *, *, #212491, .T. ) ;
#200303 = CARTESIAN_POINT ( 'NONE',  ( 0.6040130627208201153, -0.5744563726430768069, -1.626443300898507305 ) ) ;
#200305 = CARTESIAN_POINT ( 'NONE',  ( 6.287230548435207567, 8.358188277972981695, -1.599625672291262513 ) ) ;
#200306 = PRESENTATION_STYLE_ASSIGNMENT (( #68167 ) ) ;
#200307 = CARTESIAN_POINT ( 'NONE',  ( -0.08676667164122778275, -9.915770458193639669, -9.499603944220581297 ) ) ;
#200308 = CIRCLE ( 'NONE', #127759, 2.650000000000000799 ) ;
#200309 = CARTESIAN_POINT ( 'NONE',  ( 0.000000000000000000, 6.999999999999999112, -11.00000000000000000 ) ) ;
#200310 = CARTESIAN_POINT ( 'NONE',  ( 7.741342523278707866, 8.133913820021057006, 0.7216878364870458196 ) ) ;
#200311 = LINE ( 'NONE', #69237, #151507 ) ;
#200313 = CARTESIAN_POINT ( 'NONE',  ( 0.2053161149570548183, 1.340855080820763545, 1.218213988936674763 ) ) ;
#200312 = CARTESIAN_POINT ( 'NONE',  ( 5.318541398310776103, 9.426991741329731056, -0.7998128361456481317 ) ) ;
#200314 = CARTESIAN_POINT ( 'NONE',  ( -6.645467848992654858, 10.90479625713344625, 0.7998128361456481317 ) ) ;
#200315 = CARTESIAN_POINT ( 'NONE',  ( 4.680589345215795838, 6.483773540883647435, -1.599625672291256295 ) ) ;
#200316 = CARTESIAN_POINT ( 'NONE',  ( -5.333877144031607287, 7.620261487198364492, 1.234409035313356107 ) ) ;
#200317 = CARTESIAN_POINT ( 'NONE',  ( 6.339319342841494453, 9.553567112360518365, -1.199719254218452047 ) ) ;
#200318 = CARTESIAN_POINT ( 'NONE',  ( -9.492660725451591119, -6.771447601804276850, 0.03895569783345646103 ) ) ;
#200319 = CARTESIAN_POINT ( 'NONE',  ( 9.499679989893813570, -7.184999792974224420, 0.07801928546529238173 ) ) ;
#200320 = CARTESIAN_POINT ( 'NONE',  ( 8.215877900201359552, 11.56864606933486606, -1.082531754730543083 ) ) ;
#200321 = EDGE_LOOP ( 'NONE', ( #60637, #79355, #82344, #61408, #62389, #67558, #114028, #140702, #60579, #69339, #187541, #22475, #155054, #68365, #58871, #4926, #121023 ) ) ;
#200322 = AXIS2_PLACEMENT_3D ( 'NONE', #73176, #9264, #23360 ) ;
#200323 = CARTESIAN_POINT ( 'NONE',  ( 0.5267775621587212909, -1.642505510697172655, 0.9855279480080190169 ) ) ;
#200324 = CARTESIAN_POINT ( 'NONE',  ( -0.1046615654881309365, -0.1561857951268459388, -2.086345279447648693 ) ) ;
#200325 = CARTESIAN_POINT ( 'NONE',  ( -0.1399997263889612154, 1.357298622859518078, -2.254419820505838334 ) ) ;
#200326 = CARTESIAN_POINT ( 'NONE',  ( -1.504932104232262091, 8.664796307965627165, -2.552344783041797793 ) ) ;
#200327 =( BOUNDED_SURFACE ( )  B_SPLINE_SURFACE ( 3, 2, ( 
 ( #183825, #82052, #113570 ),
 ( #49557, #101513, #115684 ),
 ( #147085, #100444, #31193 ),
 ( #66837, #64739, #117834 ),
 ( #167584, #18106, #116753 ),
 ( #33304, #132980, #165441 ),
 ( #130882, #198983, #35437 ),
 ( #114633, #179574, #85258 ),
 ( #34370, #97267, #131921 ),
 ( #80997, #200063, #135106 ),
 ( #197931, #151347, #148145 ),
 ( #14903, #17038, #68988 ),
 ( #214147, #150280, #2915 ),
 ( #83115, #166515, #149196 ) ),
 .UNSPECIFIED., .F., .F., .T. ) 
 B_SPLINE_SURFACE_WITH_KNOTS ( ( 4, 2, 2, 2, 2, 2, 4 ),
 ( 3, 3 ),
 ( 0.000000000000000000, 0.0007244816566593680670, 0.001086722484989051992, 0.001448963313318736134, 0.001811204141648420059, 0.002173444969978103984, 0.002897926626637472268 ),
 ( 0.000000000000000000, 1.000000000000000000 ),
 .UNSPECIFIED. ) 
 GEOMETRIC_REPRESENTATION_ITEM ( )  RATIONAL_B_SPLINE_SURFACE ( (
 ( 1.000000000000000000, 0.8509629433967720313, 1.000000000000000000),
 ( 1.000000000000000000, 0.8509409660886558813, 1.000000000000000000),
 ( 1.000000000000000000, 0.8506801742508753872, 1.000000000000000000),
 ( 1.000000000000000000, 0.8504573418716681044, 1.000000000000000000),
 ( 1.000000000000000000, 0.8503421207546283389, 1.000000000000000000),
 ( 1.000000000000000000, 0.8502290005389957495, 1.000000000000000000),
 ( 1.000000000000000000, 0.8502658874624668961, 1.000000000000000000),
 ( 1.000000000000000000, 0.8500987576256546774, 1.000000000000000000),
 ( 1.000000000000000000, 0.8497013267704406347, 1.000000000000000000),
 ( 1.000000000000000000, 0.8485069977425411247, 1.000000000000000000),
 ( 1.000000000000000000, 0.8477706576622060508, 1.000000000000000000),
 ( 1.000000000000000000, 0.8457454946330462686, 1.000000000000000000),
 ( 1.000000000000000000, 0.8445998729257416793, 1.000000000000000000),
 ( 1.000000000000000000, 0.8434733505592222347, 1.000000000000000000) ) ) 
 REPRESENTATION_ITEM ( '' )  SURFACE ( )  );
#200328 = CARTESIAN_POINT ( 'NONE',  ( -5.436456409399874623, 5.444880020495701523, 0.000000000000000000 ) ) ;
#200329 = CARTESIAN_POINT ( 'NONE',  ( 9.463228032658635769, 11.10314946193233965, -1.082531754730543083 ) ) ;
#200330 = CARTESIAN_POINT ( 'NONE',  ( 3.450015926008513478, -0.8023341227383492535, 1.798807795796441678 ) ) ;
#200331 = CARTESIAN_POINT ( 'NONE',  ( 1.084817099560590803, -1.342388549496125627, 1.641497191572589776 ) ) ;
#200332 = CARTESIAN_POINT ( 'NONE',  ( -5.961834861707238531, 7.978559976790334574, -1.599625672291263179 ) ) ;
#200333 = CARTESIAN_POINT ( 'NONE',  ( 6.727182134110196721, 7.051813866762763006, 2.787205683092201181 ) ) ;
#200334 = CARTESIAN_POINT ( 'NONE',  ( 5.929655999079199269, 1.083026401007038952, -1.905042663481799403 ) ) ;
#200335 = CARTESIAN_POINT ( 'NONE',  ( 3.763755302173072081, 3.180306474485404600, 2.446972558850332824 ) ) ;
#200336 = CARTESIAN_POINT ( 'NONE',  ( 3.715773558573881363, -1.898061356504710639, 0.3282749975898023309 ) ) ;
#200337 = CARTESIAN_POINT ( 'NONE',  ( -8.830438121202295321, 9.196599317691152464, -0.7998128361456291469 ) ) ;
#200338 = CARTESIAN_POINT ( 'NONE',  ( 0.3580656308817786737, 0.6935259069400133702, 1.688922952486398454 ) ) ;
#200339 = CARTESIAN_POINT ( 'NONE',  ( 0.9970219447392356660, -0.5395372827587068265, -2.139793933917451874 ) ) ;
#200340 = CARTESIAN_POINT ( 'NONE',  ( 5.523117969621105239, 6.371578878345163233, -1.187916293638406895 ) ) ;
#200341 = ORIENTED_EDGE ( 'NONE', *, *, #81383, .F. ) ;
#200343 =( BOUNDED_SURFACE ( )  B_SPLINE_SURFACE ( 3, 3, ( 
 ( #70665, #4591, #200666, #166065, #17651, #53376, #119511, #170319, #168198, #52315 ),
 ( #54453, #68535, #120596, #71736, #121670, #186573, #199609, #83735, #133604, #118445 ),
 ( #69601, #37122, #103201, #169263, #149827, #20849, #38201, #19797, #187637, #1397 ),
 ( #51252, #167140, #101050, #21907, #67458, #184432, #85881, #151957, #36049, #88017 ),
 ( #150898, #5656, #135709, #201735, #137850, #117377, #203871, #183374, #34979, #18725 ),
 ( #2459, #24066, #208149, #74968, #43557, #125937, #171395, #76032, #60846, #105358 ),
 ( #6740, #42491, #139998, #157299, #107534, #123814, #142135, #141078, #77089, #26204 ) ),
 .UNSPECIFIED., .T., .F., .F. ) 
 B_SPLINE_SURFACE_WITH_KNOTS ( ( 4, 3, 4 ),
 ( 4, 1, 1, 1, 1, 1, 1, 4 ),
 ( 0.000000000000000000, 0.5000000000000000000, 1.000000000000000000 ),
 ( 0.000000000000000000, 0.09705918685507786137, 0.1907419858981972138, 0.2602182418918835838, 0.3625179829595637226, 0.5215049497019805802, 0.7338397267804015467, 1.000000000000000000 ),
 .UNSPECIFIED. ) 
 GEOMETRIC_REPRESENTATION_ITEM ( )  RATIONAL_B_SPLINE_SURFACE ( (
 ( 1.000000000000000000, 1.000000000000000000, 1.000000000000000000, 1.000000000000000222, 1.000000000000000222, 0.9999999999999994449, 1.000000000000000444, 0.9999999999999997780, 1.000000000000000000, 1.000000000000000000),
 ( 0.3333333333333333703, 0.3333333333333333703, 0.3333333333333333703, 0.3333333333333334259, 0.3333333333333333703, 0.3333333333333332038, 0.3333333333333335369, 0.3333333333333332038, 0.3333333333333333703, 0.3333333333333333703),
 ( 0.3333333333333333703, 0.3333333333333333703, 0.3333333333333333703, 0.3333333333333334259, 0.3333333333333333703, 0.3333333333333332038, 0.3333333333333335369, 0.3333333333333332038, 0.3333333333333333703, 0.3333333333333333703),
 ( 1.000000000000000000, 1.000000000000000000, 1.000000000000000000, 1.000000000000000222, 1.000000000000000222, 0.9999999999999994449, 1.000000000000000444, 0.9999999999999997780, 1.000000000000000000, 1.000000000000000000),
 ( 0.3333333333333333703, 0.3333333333333333703, 0.3333333333333333703, 0.3333333333333334259, 0.3333333333333333703, 0.3333333333333332038, 0.3333333333333335369, 0.3333333333333332038, 0.3333333333333333703, 0.3333333333333333703),
 ( 0.3333333333333333703, 0.3333333333333333703, 0.3333333333333333703, 0.3333333333333334259, 0.3333333333333333703, 0.3333333333333332038, 0.3333333333333335369, 0.3333333333333332038, 0.3333333333333333703, 0.3333333333333333703),
 ( 1.000000000000000000, 1.000000000000000000, 1.000000000000000000, 1.000000000000000222, 1.000000000000000222, 0.9999999999999994449, 1.000000000000000444, 0.9999999999999997780, 1.000000000000000000, 1.000000000000000000) ) ) 
 REPRESENTATION_ITEM ( '' )  SURFACE ( )  );
#200342 = CARTESIAN_POINT ( 'NONE',  ( 4.909461021924256485, 4.900328411765999981, 0.7216878364870338292 ) ) ;
#200344 = CARTESIAN_POINT ( 'NONE',  ( 6.649268376821393822, 1.715264285883275397, -0.9675598167100638580 ) ) ;
#200345 = CARTESIAN_POINT ( 'NONE',  ( 0.8373251867893832801, 0.7858318893144546902, -1.776134337346139125 ) ) ;
#200346 = CARTESIAN_POINT ( 'NONE',  ( 6.485746271079104730, 2.140961846981633609, 0.8364165754714718570 ) ) ;
#200348 = CARTESIAN_POINT ( 'NONE',  ( 4.838624485402447384, -1.804320056961044694, -0.4549315660777561443 ) ) ;
#200347 = CARTESIAN_POINT ( 'NONE',  ( -7.930593509350902792, 8.217056947189661287, -0.7998128361456362523 ) ) ;
#200349 = CARTESIAN_POINT ( 'NONE',  ( 5.664274315459256748, 9.830346811336296398, -0.7998128361456481317 ) ) ;
#200350 = DIRECTION ( 'NONE',  ( -5.578564026256490882E-16, -1.000000000000000000, -9.066213480720158442E-32 ) ) ;
#200351 = CARTESIAN_POINT ( 'NONE',  ( -6.175902666224832416, 7.163973517805802160, -1.199719254218446718 ) ) ;
#200352 = CARTESIAN_POINT ( 'NONE',  ( 6.720655732516652492, 7.053303974100803231, 2.424416723604695179 ) ) ;
#200353 = CARTESIAN_POINT ( 'NONE',  ( 6.614806893291146572, -0.1579704184760947761, 2.055781730312715272 ) ) ;
#200354 = CARTESIAN_POINT ( 'NONE',  ( 4.853455804012222430, 5.725081861844796727, 1.082531754730560403 ) ) ;
#200355 = VERTEX_POINT ( 'NONE', #110376 ) ;
#200356 = CIRCLE ( 'NONE', #68927, 0.08000000000000025147 ) ;
#200357 = FACE_OUTER_BOUND ( 'NONE', #173195, .T. ) ;
#200359 =( BOUNDED_CURVE ( )  B_SPLINE_CURVE ( 2, ( #71516, #70442, #105131, #2240, #201511, #35833, #104052, #136558, #202579, #186344, #151741, #101911, #53159, #19582, #54231, #154931, #85654, #120369, #138693, #170098, #21684, #204710, #87794, #6516, #119288, #153868, #185274, #56360, #203645, #169037, #121446, #187415, #122523, #40116, #102979, #42263, #59548, #192735, #125707, #94217, #124648, #173329, #190605, #28123, #106227, #27040, #210052, #176511, #108376, #208981, #8664, #191666, #43331, #175456, #109449, #93149, #76862, #7585, #159186, #10787, #24907 ),
 .UNSPECIFIED., .F., .T. ) 
 B_SPLINE_CURVE_WITH_KNOTS ( ( 3, 2, 2, 2, 2, 2, 2, 2, 2, 2, 2, 2, 2, 2, 2, 2, 2, 2, 2, 2, 2, 2, 2, 2, 2, 2, 2, 2, 2, 2, 3 ),
 ( 0.2689266445891022039, 0.2750000000000000222, 0.2833333333333333259, 0.2916666666666666852, 0.2999999999999999889, 0.3083333333333333481, 0.3166666666666666519, 0.3250000000000000111, 0.3333333333333333148, 0.3416666666666666741, 0.3499999999999999778, 0.3583333333333333370, 0.3666666666666666408, 0.3750000000000000000, 0.3833333333333333592, 0.3916666666666666630, 0.4000000000000000222, 0.4083333333333333259, 0.4166666666666667407, 0.4249999999999999889, 0.4333333333333333481, 0.4416666666666666519, 0.4500000000000000111, 0.4583333333333333148, 0.4666666666666666741, 0.4749999999999999778, 0.4833333333333333370, 0.4916666666666666408, 0.5000000000000000000, 0.5083333333333333037, 0.5088011391770072001 ),
 .UNSPECIFIED. ) 
 CURVE ( )  GEOMETRIC_REPRESENTATION_ITEM ( )  RATIONAL_B_SPLINE_CURVE ( ( 0.9470400169073494023, 0.9023589593381649010, 1.000000000000000000, 0.8660254037844387076, 1.000000000000000000, 0.8660254037844387076, 1.000000000000000000, 0.8660254037844387076, 1.000000000000000000, 0.8660254037844387076, 1.000000000000000000, 0.8660254037844387076, 1.000000000000000000, 0.8660254037844387076, 1.000000000000000000, 0.8660254037844387076, 1.000000000000000000, 0.8660254037844387076, 1.000000000000000000, 0.8660254037844387076, 1.000000000000000000, 0.8660254037844387076, 1.000000000000000000, 0.8660254037844387076, 1.000000000000000000, 0.8660254037844387076, 1.000000000000000000, 0.8660254037844387076, 1.000000000000000000, 0.8660254037844387076, 1.000000000000000000, 0.8660254037844387076, 1.000000000000000000, 0.8660254037844387076, 1.000000000000000000, 0.8660254037844387076, 1.000000000000000000, 0.8660254037844387076, 1.000000000000000000, 0.8660254037844387076, 1.000000000000000000, 0.8660254037844387076, 1.000000000000000000, 0.8660254037844387076, 1.000000000000000000, 0.8660254037844387076, 1.000000000000000000, 0.8660254037844387076, 1.000000000000000000, 0.8660254037844387076, 1.000000000000000000, 0.8660254037844387076, 1.000000000000000000, 0.8660254037844387076, 1.000000000000000000, 0.8660254037844387076, 1.000000000000000000, 0.8660254037844387076, 1.000000000000000000, 0.9924791081183812480, 0.9858026123580090339 ) ) 
 REPRESENTATION_ITEM ( '' )  );
#200358 = CARTESIAN_POINT ( 'NONE',  ( -11.89942855770814134, 12.30000000000000071, -0.7000000000000009548 ) ) ;
#200360 = CARTESIAN_POINT ( 'NONE',  ( 0.1526014871912773629, -1.468541917219987836, 1.084465738218153064 ) ) ;
#200361 = CARTESIAN_POINT ( 'NONE',  ( -3.100010679019018500, 6.768429558830820980, 1.040834085586084257E-14 ) ) ;
#200362 = CARTESIAN_POINT ( 'NONE',  ( 2.039351246016813501, -1.339629256360101106, 1.101148611782216014 ) ) ;
#200363 = CARTESIAN_POINT ( 'NONE',  ( 10.39230484541318589, 4.000000000000003553, -6.000000000000107470 ) ) ;
#200364 = CARTESIAN_POINT ( 'NONE',  ( -1.225000000000040279, 0.2500000000000002220, -4.857225732735059864E-14 ) ) ;
#200365 = CARTESIAN_POINT ( 'NONE',  ( 0.3813102713988948955, 1.798072043455358981, -0.6920631024385316410 ) ) ;
#200366 = CARTESIAN_POINT ( 'NONE',  ( 3.660947809037872425, 1.549288415169544963, -1.203348422379519667 ) ) ;
#200367 = CIRCLE ( 'NONE', #20554, 3.100000000000000089 ) ;
#200368 = CARTESIAN_POINT ( 'NONE',  ( 1.224999999999992983, -0.04166666598383617082, -0.7072540797572937077 ) ) ;
#200369 = CARTESIAN_POINT ( 'NONE',  ( -9.287498920561160887, 10.79416914786490089, -1.199719254218441611 ) ) ;
#200370 = CARTESIAN_POINT ( 'NONE',  ( 6.043183783389218355, 8.073467052085995022, 1.599625672291267398 ) ) ;
#200371 =( GEOMETRIC_REPRESENTATION_CONTEXT ( 3 ) GLOBAL_UNCERTAINTY_ASSIGNED_CONTEXT ( ( #16116 ) ) GLOBAL_UNIT_ASSIGNED_CONTEXT ( ( #64787, #177125, #64440 ) ) REPRESENTATION_CONTEXT ( 'NONE', 'WORKASPACE' ) );
#200372 = CARTESIAN_POINT ( 'NONE',  ( 5.022192282182047940, -2.110239842997441606, 0.2083548542347323507 ) ) ;
#200373 = CARTESIAN_POINT ( 'NONE',  ( 7.343676480457483002, 8.596652644402405841, -1.199719254218452047 ) ) ;
#200374 = CARTESIAN_POINT ( 'NONE',  ( -9.917953063596627317, 11.52969898140628047, -1.199719254218441611 ) ) ;
#200375 = CARTESIAN_POINT ( 'NONE',  ( 3.432542862244458703, -1.236986750340131946, 1.659893174209552624 ) ) ;
#200377 = CARTESIAN_POINT ( 'NONE',  ( -1.364683531250014514, 0.5510416670080878765, -0.7879004041258289570 ) ) ;
#200376 = DIRECTION ( 'NONE',  ( 0.000000000000000000, -1.000000000000000000, -9.023263958591317418E-17 ) ) ;
#200379 = EDGE_LOOP ( 'NONE', ( #94338, #90913, #66441, #21032 ) ) ;
#200378 = CARTESIAN_POINT ( 'NONE',  ( 4.758541215226599341, 2.215266761731282674, 0.1642064029221591559 ) ) ;
#200380 = CARTESIAN_POINT ( 'NONE',  ( 2.795839995030196423, 1.662961046791612940, -1.587192879829945946 ) ) ;
#200381 = CARTESIAN_POINT ( 'NONE',  ( 7.782016984564054773, 10.10210578678999482, 1.443375672974076540 ) ) ;
#200383 = CARTESIAN_POINT ( 'NONE',  ( -1.642778471875000035, -1.567708332855376252, -2.845375778867859751 ) ) ;
#200382 = CARTESIAN_POINT ( 'NONE',  ( 5.722950238744187956, 9.690876021928001904, 0.7216878364870317197 ) ) ;
#200384 = FILL_AREA_STYLE_COLOUR ( '', #161587 ) ;
#200385 = CARTESIAN_POINT ( 'NONE',  ( -10.17810690056512613, 3.623929045899029866, 6.361496871862332370 ) ) ;
#200386 = PLANE ( 'NONE',  #45992 ) ;
#200387 = CARTESIAN_POINT ( 'NONE',  ( 3.972844611716894736, -1.413603510852480927, 1.288168406687495215 ) ) ;
#200388 = CARTESIAN_POINT ( 'NONE',  ( 7.204675194429079505E-15, -1.137499999999999512, -3.475000000000000089 ) ) ;
#200389 = CARTESIAN_POINT ( 'NONE',  ( 3.838627834895870450, 0.2530714650476103555, 1.705954220825799617 ) ) ;
#200390 = CARTESIAN_POINT ( 'NONE',  ( 2.940638933469359895, -1.523795050681177710, 1.320827213682006285 ) ) ;
#200391 = CARTESIAN_POINT ( 'NONE',  ( 4.395370282159323239, -0.9827166871091972400, -2.078181120130776272 ) ) ;
#200392 = CARTESIAN_POINT ( 'NONE',  ( -1.499999999999966693, 7.750000000000000000, 9.886859966642596476 ) ) ;
#200393 = CARTESIAN_POINT ( 'NONE',  ( 6.621705515693503408, -2.043321748007483674, 0.5098342655636013410 ) ) ;
#200394 = CARTESIAN_POINT ( 'NONE',  ( -6.143253000767895600, 6.339752387083549934, 0.000000000000000000 ) ) ;
#200395 = CARTESIAN_POINT ( 'NONE',  ( 5.835142003873758476, -1.599326089537930873, 0.7579421051841316315 ) ) ;
#200397 = CARTESIAN_POINT ( 'NONE',  ( 1.412523707164672127, 1.536465969362065476, -1.701261851757162269 ) ) ;
#200396 = CARTESIAN_POINT ( 'NONE',  ( 5.712781623311797397, 7.758274208654143855, -1.599625672291283607 ) ) ;
#200398 = CARTESIAN_POINT ( 'NONE',  ( 0.1459185412583801633, -1.400943258209320863, 1.032289493613134823 ) ) ;
#200399 = CARTESIAN_POINT ( 'NONE',  ( 0.5993518605652721210, 4.282474605821112057, -0.2595036419143193496 ) ) ;
#200400 = CARTESIAN_POINT ( 'NONE',  ( 0.000000000000000000, 12.22000000000000064, 0.000000000000000000 ) ) ;
#200401 = CARTESIAN_POINT ( 'NONE',  ( -3.318713740295064163, 7.093859473644694269, 0.000000000000000000 ) ) ;
#200402 = CARTESIAN_POINT ( 'NONE',  ( 0.6801582343749900117, -0.6614583329919085930, -1.178068619123883165 ) ) ;
#200403 = LINE ( 'NONE', #19529, #4419 ) ;
#200404 = CARTESIAN_POINT ( 'NONE',  ( 0.6608746330511162670, -0.7316962540516893654, -2.044312434917434640 ) ) ;
#200405 = CARTESIAN_POINT ( 'NONE',  ( 1.376185782568883020, -2.007256511855738612, -0.1928315418098166534 ) ) ;
#200406 =( BOUNDED_CURVE ( )  B_SPLINE_CURVE ( 2, ( #188358, #23722, #134328, #71392, #102860, #152671, #135375, #137504, #168917 ),
 .UNSPECIFIED., .F., .T. ) 
 B_SPLINE_CURVE_WITH_KNOTS ( ( 3, 2, 2, 2, 3 ),
 ( 0.7410714285714286031, 0.7440476190476190688, 0.7500000000000000000, 0.7559523809523809312, 0.7589285714285713969 ),
 .UNSPECIFIED. ) 
 CURVE ( )  GEOMETRIC_REPRESENTATION_ITEM ( )  RATIONAL_B_SPLINE_CURVE ( ( 0.9330127018922194093, 0.9330127018922194093, 1.000000000000000000, 0.8660254037844387076, 1.000000000000000000, 0.8660254037844387076, 1.000000000000000000, 0.9330127018922194093, 0.9330127018922194093 ) ) 
 REPRESENTATION_ITEM ( '' )  );
#200407 = AXIS2_PLACEMENT_3D ( 'NONE', #95216, #132002, #161266 ) ;
#200408 = CARTESIAN_POINT ( 'NONE',  ( -1.500000000000013101, -0.2979166659838501929, 0.8660254037844403729 ) ) ;
#200409 = CARTESIAN_POINT ( 'NONE',  ( 5.690048631714204497, -0.8642791622572744137, 1.721823430457876780 ) ) ;
#200410 = CARTESIAN_POINT ( 'NONE',  ( 1.364683531249996529, 11.71354166700806587, 0.7879004041258405033 ) ) ;
#200411 = CARTESIAN_POINT ( 'NONE',  ( 2.707538781118669302, 1.902989223989959067, -1.145821276547890122 ) ) ;
#200412 = ORIENTED_EDGE ( 'NONE', *, *, #129984, .F. ) ;
#200414 = CARTESIAN_POINT ( 'NONE',  ( 0.4417779905600578982, 7.383047307301190187, -2.041823008714561460 ) ) ;
#200413 = CARTESIAN_POINT ( 'NONE',  ( 1.244150428498992600, 3.027476754118171964, -0.7749999999999874767 ) ) ;
#200415 = CARTESIAN_POINT ( 'NONE',  ( 3.791513125430877373, 7.352524219418101303, -0.3677586026353037996 ) ) ;
#200416 = CARTESIAN_POINT ( 'NONE',  ( 10.05067194643221207, 10.62020544712608938, 0.7998128361456462443 ) ) ;
#200417 = DIRECTION ( 'NONE',  ( 0.000000000000000000, 1.000000000000000000, 0.000000000000000000 ) ) ;
#200418 = DIRECTION ( 'NONE',  ( -0.03984146075563036599, -3.484297484818016589E-16, -0.9992060137953822085 ) ) ;
#200419 = CARTESIAN_POINT ( 'NONE',  ( 3.983749006537410153, -1.722186279587777369, -0.2504274415035238621 ) ) ;
#200420 = CARTESIAN_POINT ( 'NONE',  ( 2.154674626568295892, -0.5202524484802829585, -1.891573884155263396 ) ) ;
#200422 = CARTESIAN_POINT ( 'NONE',  ( -0.6823417656250212460, 3.113541667008084879, 1.181850606188767472 ) ) ;
#200421 = CARTESIAN_POINT ( 'NONE',  ( 4.521807925357579805, 5.234196320127330715, -1.199719254218452047 ) ) ;
#200423 = EDGE_CURVE ( 'NONE', #118779, #89507, #65776, .T. ) ;
#200424 = CARTESIAN_POINT ( 'NONE',  ( 4.350813900535696277, 4.000456626940672500, 0.2320863031703649382 ) ) ;
#200425 = CARTESIAN_POINT ( 'NONE',  ( 0.9067701044400799937, 0.5968461685175918685, 1.974459182335401186 ) ) ;
#200426 = CARTESIAN_POINT ( 'NONE',  ( -8.345207244411405156, 9.694828859023472134, 1.199719254218462483 ) ) ;
#200427 = CARTESIAN_POINT ( 'NONE',  ( -3.917943204224914933, 6.554388924028945240, -1.082531754730548412 ) ) ;
#200428 = CARTESIAN_POINT ( 'NONE',  ( 1.604739632818411144, -0.8155265934593752819, -2.110601385940619412 ) ) ;
#200429 = EDGE_LOOP ( 'NONE', ( #108680, #165176, #158535, #146874, #122543 ) ) ;
#200430 = CARTESIAN_POINT ( 'NONE',  ( -1.500000000000013101, 0.2020833340161521663, 0.8660254037844403729 ) ) ;
#200431 = CARTESIAN_POINT ( 'NONE',  ( 2.407302635362520427, -0.4140892318466664057, 1.823965488845371796 ) ) ;
#200432 = CARTESIAN_POINT ( 'NONE',  ( 0.8614527929159084829, -0.04078779759817893064, -1.733857029152048757 ) ) ;
#200433 = CARTESIAN_POINT ( 'NONE',  ( 5.003566749295822014, -2.181051155298455058, 0.2145382695054529609 ) ) ;
#200434 = CARTESIAN_POINT ( 'NONE',  ( 5.544061457994609476, 0.9416624597364110505, -2.106895457712253616 ) ) ;
#200435 = CARTESIAN_POINT ( 'NONE',  ( 1.411086320874027855, 1.817183042272657145, 0.9721812696896633410 ) ) ;
#200436 = CARTESIAN_POINT ( 'NONE',  ( 3.644416830925560014, -1.587075459539259992, 1.118831915631451013 ) ) ;
#200437 = CARTESIAN_POINT ( 'NONE',  ( -3.416291520519271874, 6.929497840673697340, 1.040834085586084257E-14 ) ) ;
#200438 = EDGE_CURVE ( 'NONE', #113976, #183546, #127267, .T. ) ;
#200439 = CARTESIAN_POINT ( 'NONE',  ( 6.081297793977560318, 1.728434112010367674, -0.7156336962577531935 ) ) ;
#200440 = CARTESIAN_POINT ( 'NONE',  ( 1.371478227464764998, 13.33154996480476484, -0.3356224383821780899 ) ) ;
#200441 = CARTESIAN_POINT ( 'NONE',  ( 6.696638777208028692, -1.314797947003863543, -1.528504179509587280 ) ) ;
#200442 = CARTESIAN_POINT ( 'NONE',  ( 3.282482588284323821, 6.843663763058119187, 0.7216878364870257245 ) ) ;
#200443 = CARTESIAN_POINT ( 'NONE',  ( 0.6801582343749917881, 0.7239583336747443809, 1.178068619123793015 ) ) ;
#200444 = CARTESIAN_POINT ( 'NONE',  ( 4.061172775696818782, -1.158689426361030561, 1.650081270007992318 ) ) ;
#200445 = CARTESIAN_POINT ( 'NONE',  ( -4.243338890952911058, 5.013278796608906518, -1.082531754730543971 ) ) ;
#200446 = CARTESIAN_POINT ( 'NONE',  ( 7.801827329660018684, 11.18955008699033726, 1.199719254218460707 ) ) ;
#200447 = CARTESIAN_POINT ( 'NONE',  ( 3.230585741806197841, 6.991043475407723307, 0.7998128361456271485 ) ) ;
#200449 = CARTESIAN_POINT ( 'NONE',  ( 0.5773502691896124084, -4.295408888568413630, -0.9999999999999991118 ) ) ;
#200448 = CARTESIAN_POINT ( 'NONE',  ( 1.734698295210383767, 0.1775668987445792879, 1.817036636966688823 ) ) ;
#200450 = CARTESIAN_POINT ( 'NONE',  ( -5.808742468812186033, 5.741564066561132940, 0.000000000000000000 ) ) ;
#200451 = CARTESIAN_POINT ( 'NONE',  ( 6.928203230275524760, 14.48154074412737202, -9.797958971132702644 ) ) ;
#200452 = CARTESIAN_POINT ( 'NONE',  ( -9.505648412044632067, 5.017053549588888828, 6.783778555801666776 ) ) ;
#200453 = ORIENTED_EDGE ( 'NONE', *, *, #137597, .T. ) ;
#200454 = CARTESIAN_POINT ( 'NONE',  ( -5.600926855776888758, 7.627776979863398310, -1.443375672974066548 ) ) ;
#200455 = CARTESIAN_POINT ( 'NONE',  ( 0.3999999999999758193, 2.999999999999999112, 7.500000000000000000 ) ) ;
#200456 = CARTESIAN_POINT ( 'NONE',  ( -8.402302512167102222, 10.82577223566020841, -1.599625672291263179 ) ) ;
#200457 = CARTESIAN_POINT ( 'NONE',  ( 6.041667287826984811, -1.900962894602696185, 0.6825640075473203838 ) ) ;
#200459 = ORIENTED_EDGE ( 'NONE', *, *, #125621, .T. ) ;
#200458 = CARTESIAN_POINT ( 'NONE',  ( -0.09290056220616692284, -0.4702265987995763452, -2.075310686570643437 ) ) ;
#200460 = CARTESIAN_POINT ( 'NONE',  ( -6.394605727500880299, 7.489403432619674561, -1.199719254218452047 ) ) ;
#200461 = CARTESIAN_POINT ( 'NONE',  ( 5.464099601507359516, 6.333536608968757697, 1.199719254218462483 ) ) ;
#200462 = CIRCLE ( 'NONE', #89810, 1.219999999999999751 ) ;
#200463 = CARTESIAN_POINT ( 'NONE',  ( 4.803620198249330286, -0.5517947341296326469, 1.985563166520041278 ) ) ;
#200464 = CARTESIAN_POINT ( 'NONE',  ( 5.467422714486909641, -1.967887220244109558, -0.4390321945699494632 ) ) ;
#200465 = VERTEX_POINT ( 'NONE', #13847 ) ;
#200466 = EDGE_LOOP ( 'NONE', ( #196250, #187047, #128261, #135, #198757 ) ) ;
#200467 = CARTESIAN_POINT ( 'NONE',  ( 3.583694962331215095, 7.343521886800600029, 0.3257169618917153397 ) ) ;
#200468 = CARTESIAN_POINT ( 'NONE',  ( 1.902435570468863135, -0.6170404364503377925, 0.9487424039605132364 ) ) ;
#200470 = ORIENTED_EDGE ( 'NONE', *, *, #113945, .T. ) ;
#200469 = CARTESIAN_POINT ( 'NONE',  ( -4.633854640820660009, 8.628190524257904670, -0.7998128361456362523 ) ) ;
#200471 = CARTESIAN_POINT ( 'NONE',  ( 4.802592184731321545, 8.245026257381830703, 0.8702854636597904259 ) ) ;
#200472 = CARTESIAN_POINT ( 'NONE',  ( 4.622422610786712127, 0.4444332032229811325, -1.966343831704894907 ) ) ;
#200473 = CARTESIAN_POINT ( 'NONE',  ( 4.259580805731934205, 0.8699401392010926992, 1.622648742527862620 ) ) ;
#200474 = EDGE_CURVE ( 'NONE', #155330, #172991, #185906, .T. ) ;
#200475 = CARTESIAN_POINT ( 'NONE',  ( 0.07661050522434449672, 6.948789054712463553, -2.305832378935098514 ) ) ;
#200476 = CARTESIAN_POINT ( 'NONE',  ( 2.086955060466778811, -2.263696646927360501, -0.4477047476570076290 ) ) ;
#200477 = CARTESIAN_POINT ( 'NONE',  ( 5.722423353419669567, 8.833855124701747386, 1.199719254218451159 ) ) ;
#200478 = CARTESIAN_POINT ( 'NONE',  ( 5.044278900083454253, 2.155409826167026477, 0.1645634770654491874 ) ) ;
#200479 = CARTESIAN_POINT ( 'NONE',  ( 9.420217803396747414, 9.884675613584706255, 0.7998128361456462443 ) ) ;
#200480 = CARTESIAN_POINT ( 'NONE',  ( 0.2044968316872765035, 1.690132753820037692, 0.9564217018903762302 ) ) ;
#200481 = CARTESIAN_POINT ( 'NONE',  ( -4.249591082879585535, 7.045274465746411252, 1.199719254218464037 ) ) ;
#200482 = MECHANICAL_DESIGN_GEOMETRIC_PRESENTATION_REPRESENTATION (  '', ( #203879 ), #155517 ) ;
#200483 = CARTESIAN_POINT ( 'NONE',  ( -0.9486429539237204445, 2.975839070649075158, -1.028101543438967980 ) ) ;
#200484 = CARTESIAN_POINT ( 'NONE',  ( -5.276058054373441664, 6.184431147304315424, -1.199719254218453823 ) ) ;
#200485 = CARTESIAN_POINT ( 'NONE',  ( 3.537841792810627606, 0.8420186812403904764, -1.670516725672297031 ) ) ;
#200488 = EDGE_CURVE ( 'NONE', #112565, #164262, #64857, .T. ) ;
#200487 = CARTESIAN_POINT ( 'NONE',  ( -5.264308783856126439, 9.363720357799287797, -0.7998128361456362523 ) ) ;
#200486 = CARTESIAN_POINT ( 'NONE',  ( -0.6823417656250212460, 5.551041667008087543, 1.181850606188767472 ) ) ;
#200489 = CARTESIAN_POINT ( 'NONE',  ( 2.948105999307056635, 0.7938017206191756436, -2.059354589195587337 ) ) ;
#200490 = CARTESIAN_POINT ( 'NONE',  ( 5.438229012412886476, 7.437962829272074750, -1.443375672974078316 ) ) ;
#200491 = CARTESIAN_POINT ( 'NONE',  ( 3.005103603723342953, 6.657704637652544832, -0.7998128361456291469 ) ) ;
#200492 = CARTESIAN_POINT ( 'NONE',  ( 6.007671464186812749, 10.02305078494439883, 0.7216878364870317197 ) ) ;
#200493 = CARTESIAN_POINT ( 'NONE',  ( -4.086893239515592136, 6.855460315155083251, 1.199719254218464037 ) ) ;
#200494 = CARTESIAN_POINT ( 'NONE',  ( -6.821160681006823268, 9.051383109298335228, 1.443375672974064550 ) ) ;
#200495 = CARTESIAN_POINT ( 'NONE',  ( 0.4738186427182951577, 1.131346554974651086, 1.614239802345132757 ) ) ;
#200496 = ADVANCED_FACE ( 'NONE', ( #212040 ), #210977, .F. ) ;
#200497 = CARTESIAN_POINT ( 'NONE',  ( 6.393248246410252911, 2.011339380631727458, -1.131280203180404342 ) ) ;
#200498 = CARTESIAN_POINT ( 'NONE',  ( 1.433958818539453395, 1.165882187713672247, 1.577721859592796205 ) ) ;
#200499 = CARTESIAN_POINT ( 'NONE',  ( 4.539923930118438200, 1.343280314546798637, 1.565306332949261803 ) ) ;
#200500 = CARTESIAN_POINT ( 'NONE',  ( 4.528060117284222308, 8.226561203566173930, 0.7216878364870438212 ) ) ;
#200501 = CARTESIAN_POINT ( 'NONE',  ( 7.191674137406095291, 7.354984346587396082, 0.000000000000000000 ) ) ;
#200502 = ORIENTED_EDGE ( 'NONE', *, *, #194169, .F. ) ;
#200503 = CARTESIAN_POINT ( 'NONE',  ( 7.090551149822728938, 10.25576486055978442, 1.082531754730558626 ) ) ;
#200504 = CARTESIAN_POINT ( 'NONE',  ( 0.6823417656249899377, 4.738541667008086655, -1.181850606188754593 ) ) ;
#200505 = CARTESIAN_POINT ( 'NONE',  ( -10.77716609946257620, 4.490170579428209408, -5.280790421213856334 ) ) ;
#200506 = CARTESIAN_POINT ( 'NONE',  ( 4.839897649954202130, 4.748894801142428790, -0.7216878364870197293 ) ) ;
#200507 = CARTESIAN_POINT ( 'NONE',  ( 6.145025799957537060, -0.3124719705198654718, -2.148460482323500731 ) ) ;
#200508 = CARTESIAN_POINT ( 'NONE',  ( 9.486534023829911177, -9.006863021369365896, -0.5123739589067538569 ) ) ;
#200509 = CARTESIAN_POINT ( 'NONE',  ( 2.750000000000003109, 8.900000000000023448, 1.214306433183764966E-14 ) ) ;
#200510 = CARTESIAN_POINT ( 'NONE',  ( -2.428612866367529932E-14, 8.999999999999998224, 2.420000000000000373 ) ) ;
#200511 = CARTESIAN_POINT ( 'NONE',  ( 1.704156511045151978, -0.6684128243485131238, -1.747238085743174185 ) ) ;
#200512 = CARTESIAN_POINT ( 'NONE',  ( -5.903366504444580443, 6.144480293219754863, 0.8539384941207116553 ) ) ;
#200513 = DIRECTION ( 'NONE',  ( 0.000000000000000000, 0.000000000000000000, 1.000000000000000000 ) ) ;
#200514 = CARTESIAN_POINT ( 'NONE',  ( 6.533654944624902150, 6.813559398729744032, -0.4760831665120857648 ) ) ;
#200515 = CARTESIAN_POINT ( 'NONE',  ( 0.6823417656249917140, 4.655208333674755394, 1.181850606188765695 ) ) ;
#200516 = CARTESIAN_POINT ( 'NONE',  ( 0.6449871831117167664, 0.1410837285014763798, 1.907147727228817535 ) ) ;
#200517 = CARTESIAN_POINT ( 'NONE',  ( 3.309201167148849265, -0.3463371335676104223, 1.735430568453823374 ) ) ;
#200518 = CARTESIAN_POINT ( 'NONE',  ( 0.1703706300211875746, 0.7318840393725855042, 1.766877091004593225 ) ) ;
#200520 = CARTESIAN_POINT ( 'NONE',  ( 4.868704338522531039, -0.2386889102116992178, -1.900620109961237203 ) ) ;
#200519 = CARTESIAN_POINT ( 'NONE',  ( 2.148112680227530102, -3.224741275562422960, 2.502858284989965210 ) ) ;
#200521 = CARTESIAN_POINT ( 'NONE',  ( 0.000000000000000000, -9.999999999999994671, 0.000000000000000000 ) ) ;
#200522 = CARTESIAN_POINT ( 'NONE',  ( 4.896905686981484429, 0.3346149513497528871, 1.940740247813901087 ) ) ;
#200523 = CARTESIAN_POINT ( 'NONE',  ( 0.4398875993102538962, -2.011672884243600024, 0.6710486789910232730 ) ) ;
#200524 = CARTESIAN_POINT ( 'NONE',  ( 0.000000000000000000, -0.2000000000000057288, 0.000000000000000000 ) ) ;
#200525 = CARTESIAN_POINT ( 'NONE',  ( 3.502682687546424312, 1.475339254275360279, -1.149998991230333223 ) ) ;
#200527 = ORIENTED_EDGE ( 'NONE', *, *, #7456, .T. ) ;
#200526 = CARTESIAN_POINT ( 'NONE',  ( 0.3108172448005979138, 1.586703044182024458, 0.9029097728878652251 ) ) ;
#200529 = CARTESIAN_POINT ( 'NONE',  ( 2.887523530030648988, 6.312601851770308414, 0.000000000000000000 ) ) ;
#200528 = CARTESIAN_POINT ( 'NONE',  ( 3.879664727460280904, 2.078262106501146622, -0.7427522710690689367 ) ) ;
#200530 = AXIS2_PLACEMENT_3D ( 'NONE', #30930, #28782, #61276 ) ;
#200531 = CARTESIAN_POINT ( 'NONE',  ( -1.364683531249997417, 4.571875000341417028, 1.214306433183764966E-14 ) ) ;
#200532 = CARTESIAN_POINT ( 'NONE',  ( 0.5024796060203519099, 2.057031790779086045, 0.1535979213492833784 ) ) ;
#200533 = CARTESIAN_POINT ( 'NONE',  ( 8.098297826064319693, 8.342435640030188893, 0.7998128361456481317 ) ) ;
#200534 = CARTESIAN_POINT ( 'NONE',  ( -8.208571938070008400, 11.66408546346865016, -1.199719254218446718 ) ) ;
#200535 = CARTESIAN_POINT ( 'NONE',  ( 5.899206235721897507, 6.055031161196562373, 0.000000000000000000 ) ) ;
#200536 = CARTESIAN_POINT ( 'NONE',  ( -3.446831259402118430, -0.01219589716538043052, -0.3300872410877821461 ) ) ;
#200537 = FACE_OUTER_BOUND ( 'NONE', #60219, .T. ) ;
#200538 = ORIENTED_EDGE ( 'NONE', *, *, #160015, .F. ) ;
#200539 = CARTESIAN_POINT ( 'NONE',  ( 3.016144355299533952, 2.060630728401948275, -0.2003171163396169074 ) ) ;
#200540 = CARTESIAN_POINT ( 'NONE',  ( 1.499999999999989120, 4.254166666666687746, 0.8660254037844524744 ) ) ;
#200541 = CARTESIAN_POINT ( 'NONE',  ( 1.142116303652768172, 0.8771353898661786719, -1.975824051420910221 ) ) ;
#200542 = CARTESIAN_POINT ( 'NONE',  ( -6.604009391672221341, 6.765323812321595298, -0.2039879123204788036 ) ) ;
#200543 = CARTESIAN_POINT ( 'NONE',  ( 0.6276103948988649428, -0.2939658443398012744, 1.998026100167526575 ) ) ;
#200544 = CARTESIAN_POINT ( 'NONE',  ( 1.499999999999990896, 8.266799604814890401, 3.162088779278453998 ) ) ;
#200545 = ORIENTED_EDGE ( 'NONE', *, *, #93956, .T. ) ;
#200547 = CARTESIAN_POINT ( 'NONE',  ( 9.408995418203975447, 10.07950886410055524, 0.7216878364870438212 ) ) ;
#200546 = CARTESIAN_POINT ( 'NONE',  ( -1.737499999999997824, -2.391666666666667052, 3.009438278150925683 ) ) ;
#200548 = CARTESIAN_POINT ( 'NONE',  ( 6.538435458278026857, 1.930121188254026787, -0.5825698962980339068 ) ) ;
#200549 = CARTESIAN_POINT ( 'NONE',  ( 5.735529463276822781, 0.5494309942872098729, -1.835271804430014919 ) ) ;
#200550 = CARTESIAN_POINT ( 'NONE',  ( 4.318054327947466575, 1.347776305887092185, -1.728067674571641898 ) ) ;
#200551 = CARTESIAN_POINT ( 'NONE',  ( -1.500000000000013101, 3.160416667349486008, -0.8660254037844313801 ) ) ;
#200552 = CARTESIAN_POINT ( 'NONE',  ( 3.515784362865181478, -0.5505564139345071606, 1.831456330389509501 ) ) ;
#200553 = CARTESIAN_POINT ( 'NONE',  ( -3.716906668440817185, 7.488141546489591072, 0.7998128361456341429 ) ) ;
#200554 = CARTESIAN_POINT ( 'NONE',  ( 3.484082288587588838, 7.008587070086755411, -0.7216878364870267237 ) ) ;
#200556 = CARTESIAN_POINT ( 'NONE',  ( 1.564077599769473803, -1.076297475396456704, 1.704952281334138675 ) ) ;
#200555 = CYLINDRICAL_SURFACE ( 'NONE', #125369, 0.08000000000000020983 ) ;
#200558 = EDGE_CURVE ( 'NONE', #160319, #78710, #17798, .T. ) ;
#200557 = CARTESIAN_POINT ( 'NONE',  ( 0.6823417656249969321, 11.58854166700806765, -1.181850606188757036 ) ) ;
#200560 = CARTESIAN_POINT ( 'NONE',  ( -3.806807270387036368, 7.663301925418665839, 0.000000000000000000 ) ) ;
#200559 = CARTESIAN_POINT ( 'NONE',  ( 0.9434182766495626815, -1.811351811004081158, -1.404917595322150659 ) ) ;
#200561 = CARTESIAN_POINT ( 'NONE',  ( 4.260587326446613865, -1.277293937326873019, 1.159233799866489889 ) ) ;
#200562 = CARTESIAN_POINT ( 'NONE',  ( 0.1399997263886020860, 0.7221123407896400392, -2.083281383436136558 ) ) ;
#200563 = CARTESIAN_POINT ( 'NONE',  ( 6.934105498385400246, 10.17720795050327354, -1.199719254218441611 ) ) ;
#200564 = CARTESIAN_POINT ( 'NONE',  ( 3.497113557321089861, 6.167384019261527683, -1.199719254218446718 ) ) ;
#200565 = LINE ( 'NONE', #197383, #199401 ) ;
#200566 = CARTESIAN_POINT ( 'NONE',  ( 1.170277241841523264, -0.8789641444944886750, -1.754005360843587047 ) ) ;
#200567 = CARTESIAN_POINT ( 'NONE',  ( 5.518332215962025167, 6.396807992499198292, -1.199719254218445830 ) ) ;
#200568 = CARTESIAN_POINT ( 'NONE',  ( 0.07516593201269992919, 2.015085533825950126, -2.458757630349134082 ) ) ;
#200569 = ORIENTED_EDGE ( 'NONE', *, *, #167712, .T. ) ;
#200570 = SURFACE_SIDE_STYLE ('',( #134569 ) ) ;
#200571 = ORIENTED_EDGE ( 'NONE', *, *, #175529, .F. ) ;
#200572 = CARTESIAN_POINT ( 'NONE',  ( 4.318897000252651885, 1.397372457865418083, -1.152701029936139099 ) ) ;
#200573 = ORIENTED_EDGE ( 'NONE', *, *, #176483, .T. ) ;
#200574 = CARTESIAN_POINT ( 'NONE',  ( 6.855582950365507244, 8.027210192628430718, -1.199719254218452047 ) ) ;
#200575 = CARTESIAN_POINT ( 'NONE',  ( 3.061108821635398769, 6.793320401875094561, -0.7998128361456362523 ) ) ;
#200576 = CARTESIAN_POINT ( 'NONE',  ( 4.846265894328573687, 0.9266178045349574566, -1.556377301703376625 ) ) ;
#200577 = CARTESIAN_POINT ( 'NONE',  ( 6.333067150914816423, 7.521571443223021625, 1.082531754730549967 ) ) ;
#200578 = CARTESIAN_POINT ( 'NONE',  ( 7.874499448206170094, -5.294771359305315173, -7.680942717881076298 ) ) ;
#200579 = CARTESIAN_POINT ( 'NONE',  ( 5.112599315731837457, 6.496590726105775815, -1.208607640439966158 ) ) ;
#200581 = CARTESIAN_POINT ( 'NONE',  ( 9.378489572351044856, 11.96465713920816043, -1.599625672291262513 ) ) ;
#200580 = CARTESIAN_POINT ( 'NONE',  ( 5.723074792265875566, -1.682715607417185399, -0.7953119777529999990 ) ) ;
#200582 = CARTESIAN_POINT ( 'NONE',  ( 3.884325381594720739, -0.6044542036256529416, -1.817792542802825428 ) ) ;
#200583 = DIRECTION ( 'NONE',  ( 0.000000000000000000, 1.000000000000000000, 0.000000000000000000 ) ) ;
#200584 = CARTESIAN_POINT ( 'NONE',  ( -11.31088518949709965, 5.182344123437907513, 5.726584094856639773 ) ) ;
#200585 = CARTESIAN_POINT ( 'NONE',  ( -10.99952653502856137, -9.917017194762472343, 0.1020740558599455700 ) ) ;
#200586 = CARTESIAN_POINT ( 'NONE',  ( -1.602468905319636405E-14, -1.053124999658583638, -1.575800808251665908 ) ) ;
#200587 = CARTESIAN_POINT ( 'NONE',  ( 6.155038550924144758, 8.203964280876741455, 1.443375672974076540 ) ) ;
#200588 = CARTESIAN_POINT ( 'NONE',  ( -2.266184231778562541, 5.795632037050281404, 1.040834085586084257E-14 ) ) ;
#200589 = CARTESIAN_POINT ( 'NONE',  ( 0.4269344243218140544, 2.069031678568326704, 0.6260965431626740463 ) ) ;
#200590 = CARTESIAN_POINT ( 'NONE',  ( -6.231907884136888676, 7.299589282028351001, -1.199719254218453823 ) ) ;
#200591 = CARTESIAN_POINT ( 'NONE',  ( 6.052789233858158369, 6.026285292448116948, 0.000000000000000000 ) ) ;
#200592 = CARTESIAN_POINT ( 'NONE',  ( 0.7975364289293709330, -0.6616875547802402169, 1.701626729119443127 ) ) ;
#200593 = CARTESIAN_POINT ( 'NONE',  ( -4.055860508782465068, 7.883587693554856557, 1.040834085586084257E-14 ) ) ;
#200594 = EDGE_CURVE ( 'NONE', #101274, #201966, #87106, .T. ) ;
#200595 = CARTESIAN_POINT ( 'NONE',  ( 3.469579810302122702, 1.781292651720441711, -0.3989491859636914994 ) ) ;
#200596 = CARTESIAN_POINT ( 'NONE',  ( 9.686381629184177555, 13.40773330361598248, 8.159561931930056744 ) ) ;
#200597 =( BOUNDED_CURVE ( )  B_SPLINE_CURVE ( 2, ( #19664, #134529, #150763, #183238, #151825, #202665, #200535 ),
 .UNSPECIFIED., .F., .T. ) 
 B_SPLINE_CURVE_WITH_KNOTS ( ( 3, 2, 2, 3 ),
 ( 0.3250000000000001776, 0.3333333333333334814, 0.3416666666666667851, 0.3500000000000000888 ),
 .UNSPECIFIED. ) 
 CURVE ( )  GEOMETRIC_REPRESENTATION_ITEM ( )  RATIONAL_B_SPLINE_CURVE ( ( 0.9999999999999973355, 0.8660254037844413721, 1.000000000000000000, 0.8660254037844387076, 1.000000000000000000, 0.8660254037844369313, 1.000000000000001776 ) ) 
 REPRESENTATION_ITEM ( '' )  );
#200598 = CARTESIAN_POINT ( 'NONE',  ( 2.400782916097830455, 0.4286735998642232648, 1.922169311629307931 ) ) ;
#200599 = CARTESIAN_POINT ( 'NONE',  ( 3.509261751715045730, -1.912814363422868480, 0.3349611914155846693 ) ) ;
#200600 = ORIENTED_EDGE ( 'NONE', *, *, #132358, .F. ) ;
#200601 = CARTESIAN_POINT ( 'NONE',  ( -6.749980374757255319, 8.968339418673846097, 1.599625672291269396 ) ) ;
#200603 = CARTESIAN_POINT ( 'NONE',  ( 4.377262645480927361, -1.895543854172193399, -0.9507902649282941043 ) ) ;
#200602 = CARTESIAN_POINT ( 'NONE',  ( 8.005163354226054295, 8.304055099544019214, 0.000000000000000000 ) ) ;
#200604 = CARTESIAN_POINT ( 'NONE',  ( 5.736508392357904107, 5.865217010605237924, 0.000000000000000000 ) ) ;
#200605 = CARTESIAN_POINT ( 'NONE',  ( 9.368847842243145152, 10.88907622316056312, 1.199719254218453823 ) ) ;
#200606 = CARTESIAN_POINT ( 'NONE',  ( 5.946581215072361815, 6.122072269273588496, 0.7275674859277461159 ) ) ;
#200607 = CARTESIAN_POINT ( 'NONE',  ( -1.177073619093324419, 3.074321498342245995, -0.7749999999999918066 ) ) ;
#200608 = EDGE_LOOP ( 'NONE', ( #102382, #185901, #134456, #48539, #189672 ) ) ;
#200609 = CARTESIAN_POINT ( 'NONE',  ( 5.345992642490140057, 5.131412925860272090, 1.040834085586084257E-14 ) ) ;
#200610 = AXIS2_PLACEMENT_3D ( 'NONE', #193613, #32184, #164317 ) ;
#200611 = CARTESIAN_POINT ( 'NONE',  ( 5.091969210384201361, 8.098325291160362482, 1.199719254218452047 ) ) ;
#200612 = CARTESIAN_POINT ( 'NONE',  ( -9.604686356149274573, 3.481540744127369802, 7.193747284969079558 ) ) ;
#200613 = CARTESIAN_POINT ( 'NONE',  ( 4.125493313500066428, -1.746467973620144942, 0.5319596651164605339 ) ) ;
#200614 = CARTESIAN_POINT ( 'NONE',  ( -6.518203450479854943, 5.167241622962448488, 2.437504649502892473 ) ) ;
#200615 = CARTESIAN_POINT ( 'NONE',  ( -8.188761592974040937, 11.53701037756964887, -1.082531754730543971 ) ) ;
#200616 = CARTESIAN_POINT ( 'NONE',  ( -4.622835856459495574, 8.451390222604121760, 0.3997878540293615113 ) ) ;
#200617 = DIRECTION ( 'NONE',  ( -5.828670879282089587E-16, 0.8656921114426507913, -0.5005768354468322912 ) ) ;
#200618 = CARTESIAN_POINT ( 'NONE',  ( 4.979306205331720747, 1.745251617482036943, -0.6738592683939447214 ) ) ;
#200619 = CARTESIAN_POINT ( 'NONE',  ( 6.414979237560321401, 10.63589287712906462, 1.040834085586084257E-14 ) ) ;
#200620 = CARTESIAN_POINT ( 'NONE',  ( 3.492722931844041145, -0.3765888977748827471, -1.889173544197232824 ) ) ;
#200621 = CARTESIAN_POINT ( 'NONE',  ( -4.303823697334223652, 7.108545849276850959, -1.199719254218452047 ) ) ;
#200622 = CARTESIAN_POINT ( 'NONE',  ( 3.032219910950674890, 6.689340329417765574, 0.7998128361456321445 ) ) ;
#200623 = CARTESIAN_POINT ( 'NONE',  ( 1.364683531249997417, 9.046875000341403350, 2.602085213965210642E-15 ) ) ;
#200624 = CARTESIAN_POINT ( 'NONE',  ( -7.223796917982883592, 7.322184580601816428, -0.7998128361456291469 ) ) ;
#200625 = CARTESIAN_POINT ( 'NONE',  ( 3.846762897975340767, 5.510976019103107859, -1.599625672291256295 ) ) ;
#200627 = EDGE_CURVE ( 'NONE', #163746, #23490, #89166, .T. ) ;
#200626 = AXIS2_PLACEMENT_3D ( 'NONE', #78183, #194061, #44643 ) ;
#200628 = CARTESIAN_POINT ( 'NONE',  ( -7.445362632559989535, 8.715286488521982733, 1.199719254218452047 ) ) ;
#200629 = CARTESIAN_POINT ( 'NONE',  ( 0.9314518356654817310, -1.671823418590481447, -1.299033474062233351 ) ) ;
#200630 = CARTESIAN_POINT ( 'NONE',  ( 9.053093885623066939, 11.58502883802551153, -1.599625672291262513 ) ) ;
#200631 = CARTESIAN_POINT ( 'NONE',  ( -11.97929049433705373, 11.37999999999999901, -0.7046979865771834106 ) ) ;
#200632 = CARTESIAN_POINT ( 'NONE',  ( 6.789897376884641567, -1.347643488625469121, -1.571692526165118009 ) ) ;
#200634 = CARTESIAN_POINT ( 'NONE',  ( 4.159596813995052322, 7.384974941181836172, -0.7733407813514819873 ) ) ;
#200633 = CARTESIAN_POINT ( 'NONE',  ( 1.505144418776669601, -1.827259764946763454, 0.2261131901925839127 ) ) ;
#200635 = CARTESIAN_POINT ( 'NONE',  ( 6.371969008742804697, 7.496680600697164465, -1.082531754730543083 ) ) ;
#200637 = CARTESIAN_POINT ( 'NONE',  ( 0.4841293774267214634, 6.672680601848989035, 3.378195143392549671 ) ) ;
#200636 = CARTESIAN_POINT ( 'NONE',  ( 4.584065335196271462, 5.481069324884694005, 1.082531754730549078 ) ) ;
#200638 = CARTESIAN_POINT ( 'NONE',  ( 1.113678556162515543, -2.235424308229993162, 0.5066684154252357741 ) ) ;
#200639 = CARTESIAN_POINT ( 'NONE',  ( -4.496171506534410334, 8.048216686630670580, 2.444650791391992151 ) ) ;
#200640 = CARTESIAN_POINT ( 'NONE',  ( 5.507742394360604088, -0.8750994344452074358, -1.733673826448577593 ) ) ;
#200641 = ORIENTED_EDGE ( 'NONE', *, *, #113228, .T. ) ;
#200642 = CARTESIAN_POINT ( 'NONE',  ( 7.402388682937041331, 11.57994453016116587, 1.040834085586084257E-14 ) ) ;
#200643 = CARTESIAN_POINT ( 'NONE',  ( 0.4221356392010866543, -2.003110517487953324, 0.2016333174496009462 ) ) ;
#200644 = CARTESIAN_POINT ( 'NONE',  ( -9.622536337397040285, 12.24937836509514710, 1.599625672291281386 ) ) ;
#200646 = CARTESIAN_POINT ( 'NONE',  ( -1.292128843000392768, 8.373613470998940045, -10.90074592850029767 ) ) ;
#200645 = CARTESIAN_POINT ( 'NONE',  ( -8.015895134177625891, 10.37496362800581018, 1.599625672291295375 ) ) ;
#200647 = CARTESIAN_POINT ( 'NONE',  ( -6.642568916052639771, 6.714361588341672515, 0.000000000000000000 ) ) ;
#200649 = CARTESIAN_POINT ( 'NONE',  ( 2.606023559441010828, -0.6750964425338638053, -1.636234759011189421 ) ) ;
#200648 = CARTESIAN_POINT ( 'NONE',  ( 3.837900784552390476, 2.080585211200749018, 0.2046572434392830431 ) ) ;
#200650 = CARTESIAN_POINT ( 'NONE',  ( 8.014278199453780616, 8.522615118883788199, 0.000000000000000000 ) ) ;
#200651 = CARTESIAN_POINT ( 'NONE',  ( 5.314510991623739855, 2.116275055252315074, 0.8812819573641057502 ) ) ;
#200652 = CARTESIAN_POINT ( 'NONE',  ( 3.749730547248275148, 0.6284987560769598192, 1.623061768561576468 ) ) ;
#200653 = EDGE_CURVE ( 'NONE', #11477, #138322, #66889, .T. ) ;
#200654 = CARTESIAN_POINT ( 'NONE',  ( 9.297140650669039275, 11.86975006391249643, 1.599625672291281386 ) ) ;
#200655 = CARTESIAN_POINT ( 'NONE',  ( 5.574337433874081427, 6.532423756721743580, -1.199719254218452047 ) ) ;
#200656 = CARTESIAN_POINT ( 'NONE',  ( 3.321388563693925544, -1.314311947043474538, 1.130952296748084951 ) ) ;
#200657 = CARTESIAN_POINT ( 'NONE',  ( 4.018178019744323315, 2.155211776303669335, -0.2622048733134130782 ) ) ;
#200658 = CARTESIAN_POINT ( 'NONE',  ( 4.172158584703322681, 5.890604320285754980, -1.599625672291256295 ) ) ;
#200659 = CARTESIAN_POINT ( 'NONE',  ( 4.645720405014278853, 1.993893748393640086, -0.3006458143828410479 ) ) ;
#200660 = CARTESIAN_POINT ( 'NONE',  ( 1.281250000000000444, 0.7852924748300526003, 1.895863743164061255 ) ) ;
#200661 = CARTESIAN_POINT ( 'NONE',  ( 1.499999999999987121, 3.827083334016153415, -0.8660254037844323793 ) ) ;
#200662 = CARTESIAN_POINT ( 'NONE',  ( 2.239170187357332420, -1.721643101494104044, 0.8643732543716446948 ) ) ;
#200663 = CARTESIAN_POINT ( 'NONE',  ( 0.7500000000000006661, 8.697916667349467446, -1.299038105676657340 ) ) ;
#200664 = CARTESIAN_POINT ( 'NONE',  ( 6.047183177241617358, 0.2169752325061699572, 2.210822359046988428 ) ) ;
#200665 = ORIENTED_EDGE ( 'NONE', *, *, #114498, .F. ) ;
#200666 = CARTESIAN_POINT ( 'NONE',  ( -0.2108831679771203116, 0.7314853703891763814, -1.979988191570913880 ) ) ;
#200667 = CARTESIAN_POINT ( 'NONE',  ( -1.499999999999997780, 2.150000000000019895, 1.214306433183764966E-14 ) ) ;
#200668 = CARTESIAN_POINT ( 'NONE',  ( 7.447506452608354088, 7.583179037664891098, 0.7998128361456341429 ) ) ;
#200669 = CARTESIAN_POINT ( 'NONE',  ( 3.185802909086937973, 6.660594460669327255, 0.7216878364870317197 ) ) ;
#200670 = CARTESIAN_POINT ( 'NONE',  ( 3.285556943750000070, -1.334374999522040861, 0.000000000000000000 ) ) ;
#200671 = CARTESIAN_POINT ( 'NONE',  ( 0.9794852244889130644, -2.010350447809361896, -0.9450808295136583492 ) ) ;
#200673 = CARTESIAN_POINT ( 'NONE',  ( 5.828557447170540584, -1.245780601409246957, 1.515539014345569147 ) ) ;
#200672 = AXIS2_PLACEMENT_3D ( 'NONE', #18924, #118644, #67657 ) ;
#200674 = CARTESIAN_POINT ( 'NONE',  ( 8.595506201384013778, 10.09080732544527592, 1.082531754730558626 ) ) ;
#200675 = CARTESIAN_POINT ( 'NONE',  ( -0.1115135314127749661, 3.398037119535586292, 2.078540374709471283 ) ) ;
#200676 = CARTESIAN_POINT ( 'NONE',  ( 0.1929406647830470833, -0.4748886411078504510, -2.116594070111991410 ) ) ;
#200677 = CARTESIAN_POINT ( 'NONE',  ( 5.174371902270911150, 6.065797303184739420, 1.199719254218452047 ) ) ;
#200678 = CARTESIAN_POINT ( 'NONE',  ( -4.001064729808656573, 7.682009594836471500, 1.214306433183764966E-14 ) ) ;
#200679 = CARTESIAN_POINT ( 'NONE',  ( 3.859879052112312969, -0.6014189565349871147, 1.973034901002912678 ) ) ;
#200680 = CARTESIAN_POINT ( 'NONE',  ( -5.525111292768871252, 6.404716915440499037, -1.199719254218446718 ) ) ;
#200681 = CARTESIAN_POINT ( 'NONE',  ( 0.7499999999999902300, 3.597916667349487785, -1.299038105676658228 ) ) ;
#200682 = CARTESIAN_POINT ( 'NONE',  ( 1.364683531249988757, -0.3656249996585800299, 0.000000000000000000 ) ) ;
#200683 = CARTESIAN_POINT ( 'NONE',  ( 5.870339087135666212, -1.187030499695044039, 1.445606174157453738 ) ) ;
#200684 = CARTESIAN_POINT ( 'NONE',  ( 4.289544331642456854, 1.336530783054422189, -1.104934575851760137 ) ) ;
#200685 = CARTESIAN_POINT ( 'NONE',  ( 3.790341827058436142, 1.467891733132551613, -0.9347920342070329403 ) ) ;
#200686 = CARTESIAN_POINT ( 'NONE',  ( 8.392133896734652154, 12.73464727959172293, 0.7216878364870438212 ) ) ;
#200687 = CARTESIAN_POINT ( 'NONE',  ( 1.839794590071419211, 0.8728355696882350578, -2.119893007042342958 ) ) ;
#200688 = CARTESIAN_POINT ( 'NONE',  ( -0.6823417656249969321, 3.530208333674754506, -1.181850606188749264 ) ) ;
#200689 = CARTESIAN_POINT ( 'NONE',  ( 5.460518745505165583, -1.890641411385725501, -0.8928391682238371319 ) ) ;
#200690 = CARTESIAN_POINT ( 'NONE',  ( 6.544875487120448199, -1.561333999131156780, -1.154546517916557269 ) ) ;
#200691 = EDGE_CURVE ( 'NONE', #53448, #194558, #120291, .T. ) ;
#200692 = DIRECTION ( 'NONE',  ( 0.000000000000000000, 0.000000000000000000, -1.000000000000000000 ) ) ;
#200693 = CARTESIAN_POINT ( 'NONE',  ( 1.617814789376757156, 0.2004366740697149929, 2.006445999502483257 ) ) ;
#200694 = CARTESIAN_POINT ( 'NONE',  ( 0.4631483011842302822, 0.2107759881739782182, -2.181290363801504650 ) ) ;
#200695 = CARTESIAN_POINT ( 'NONE',  ( 7.459175572040564361, 13.90551515481552691, -8.979190973933295794 ) ) ;
#200696 = CARTESIAN_POINT ( 'NONE',  ( -7.690499447449645309, 9.995335326823163058, 1.599625672291295375 ) ) ;
#200697 = CARTESIAN_POINT ( 'NONE',  ( 5.469824908109481854, 8.468880595181346393, -1.199719254218446718 ) ) ;
#200698 = CARTESIAN_POINT ( 'NONE',  ( 2.157031413788193852, 0.4673396547767159070, 2.068183735011968505 ) ) ;
#200699 = CARTESIAN_POINT ( 'NONE',  ( -0.6823417656250246877, -1.198958332991911790, 1.181850606188755259 ) ) ;
#200700 = CARTESIAN_POINT ( 'NONE',  ( 5.092344371507952161, -1.812320225013038133, -0.2200062734805732223 ) ) ;
#200701 = B_SPLINE_CURVE_WITH_KNOTS ( 'NONE', 3,
 ( #19103, #68906, #119889, #88397, #69970, #202098 ),
 .UNSPECIFIED., .F., .F.,
 ( 4, 2, 4 ),
 ( 0.000000000000000000, 0.0005322801792318878960, 0.001064560358463775792 ),
 .UNSPECIFIED. ) ;
#200702 = ORIENTED_EDGE ( 'NONE', *, *, #117977, .F. ) ;
#200703 = CARTESIAN_POINT ( 'NONE',  ( -4.945692173934974178, 8.992000979557944973, 0.000000000000000000 ) ) ;
#200704 = CARTESIAN_POINT ( 'NONE',  ( -4.903732577545095062, 4.837283930932079201, 0.1501914610188368193 ) ) ;
#200705 = CARTESIAN_POINT ( 'NONE',  ( 3.285556943750000070, -0.3718749995220427262, 0.000000000000000000 ) ) ;
#200706 = CARTESIAN_POINT ( 'NONE',  ( -6.124532705071231931, 8.168374127381657246, -1.599625672291263179 ) ) ;
#200707 = CARTESIAN_POINT ( 'NONE',  ( 2.760026041568770072, 0.7230886973167930387, -1.886116010022680589 ) ) ;
#200708 = CARTESIAN_POINT ( 'NONE',  ( 6.282275147445602670, -1.185768659569720329, 1.860957768143455038 ) ) ;
#200709 = CARTESIAN_POINT ( 'NONE',  ( 8.594979316059474073, 12.11489407112305372, 1.199719254218450271 ) ) ;
#200710 = CARTESIAN_POINT ( 'NONE',  ( 4.170637490619288457, 1.318561355513592215, -1.313476238859044409 ) ) ;
#200711 = CARTESIAN_POINT ( 'NONE',  ( 9.348510611822643313, 10.86534945433664134, 1.199719254218453823 ) ) ;
#200712 = EDGE_CURVE ( 'NONE', #85779, #80427, #121105, .T. ) ;
#200713 = ORIENTED_EDGE ( 'NONE', *, *, #103222, .F. ) ;
#200714 = CARTESIAN_POINT ( 'NONE',  ( -4.464712657601869417, 4.103252943490596216, 0.7998128361456341429 ) ) ;
#200715 = COLOUR_RGB ( '', 0.08235294, 0.09019608, 0.10196078) ;
#200716 = CARTESIAN_POINT ( 'NONE',  ( -8.843996274815957293, 9.212417163573759282, 1.040834085586084257E-14 ) ) ;
#200718 = CARTESIAN_POINT ( 'NONE',  ( -4.153558989372251986, 7.618438364782146976, 0.8772435784342603737 ) ) ;
#200717 = CARTESIAN_POINT ( 'NONE',  ( -5.749539660647037032, 8.865490816466966351, 1.199719254218454489 ) ) ;
#200719 = CARTESIAN_POINT ( 'NONE',  ( 1.364683531249986537, -0.5947916663252456049, -0.7879004041258309554 ) ) ;
#200720 = CARTESIAN_POINT ( 'NONE',  ( 1.457864220016273693, 1.308402020977760261, 1.137755859488085886 ) ) ;
#200721 = CARTESIAN_POINT ( 'NONE',  ( 1.376469814831126071, 1.609123190100629985, -0.6634216792447115152 ) ) ;
#200723 = CARTESIAN_POINT ( 'NONE',  ( 6.805829924380097040, 10.88395931184472154, 0.7216878364870438212 ) ) ;
#200722 = CARTESIAN_POINT ( 'NONE',  ( 5.233197408665407835, 0.1653354203888204033, 2.301840570688079790 ) ) ;
#200724 = CARTESIAN_POINT ( 'NONE',  ( 4.146814880933355596, 5.931313009212638931, 1.599625672291261402 ) ) ;
#200725 = CARTESIAN_POINT ( 'NONE',  ( 1.159529407832321501, 0.4047576141815812378, -2.020457351226915055 ) ) ;
#200726 = CARTESIAN_POINT ( 'NONE',  ( 4.333802657862601215, 8.207853534148366492, 0.7998128361456462443 ) ) ;
#200727 = CARTESIAN_POINT ( 'NONE',  ( 6.591202130252849400, 1.331619970128885777, -1.873199602832905430 ) ) ;
#200728 = DIRECTION ( 'NONE',  ( 0.000000000000000000, 0.000000000000000000, -1.000000000000000000 ) ) ;
#200729 = CARTESIAN_POINT ( 'NONE',  ( -6.798487682609798632, 6.896266815991691779, 0.7998128361456341429 ) ) ;
#200730 = CARTESIAN_POINT ( 'NONE',  ( 0.1628737759792201201, -1.759808232078699630, -0.8888803535714930870 ) ) ;
#200733 = EDGE_CURVE ( 'NONE', #136449, #65494, #1851, .T. ) ;
#200732 = CARTESIAN_POINT ( 'NONE',  ( -6.129694847154211423, 9.205042184104968328, -1.082531754730549967 ) ) ;
#200731 = CARTESIAN_POINT ( 'NONE',  ( 4.306835718904429733, -0.4242474483713705169, -1.864571660543254961 ) ) ;
#200734 = CARTESIAN_POINT ( 'NONE',  ( 6.217417563691929772, -0.2743312036321900460, 2.189694890431858276 ) ) ;
#200735 = CARTESIAN_POINT ( 'NONE',  ( -0.6125000000000383471, 1.854166667349464781, 1.060881119635894487 ) ) ;
#200736 = CARTESIAN_POINT ( 'NONE',  ( 1.499999999999996891, 10.64583333333333037, -0.8660254037844378194 ) ) ;
#200737 = CARTESIAN_POINT ( 'NONE',  ( 5.682275777458854371, 5.801945626556378244, 0.7216878364870328300 ) ) ;
#200738 = CARTESIAN_POINT ( 'NONE',  ( -5.438229012412911345, 5.517224400669388018, -0.7216878364870338292 ) ) ;
#200739 = CARTESIAN_POINT ( 'NONE',  ( 6.375647721065083928, 0.3630326626483972308, -2.089014862189771726 ) ) ;
#200740 = VERTEX_POINT ( 'NONE', #33307 ) ;
#200741 = EDGE_CURVE ( 'NONE', #160913, #202042, #13058, .T. ) ;
#200742 = CARTESIAN_POINT ( 'NONE',  ( 3.716130297413534844, -2.273962828982917017, 0.3916390033968617512 ) ) ;
#200743 = CARTESIAN_POINT ( 'NONE',  ( 4.809014631063706524, -1.576880339463518022, 1.167019128429528374 ) ) ;
#200744 = CARTESIAN_POINT ( 'NONE',  ( 0.6198768371072012062, 1.941228818809427104, -0.2821078022595123747 ) ) ;
#200745 = DIRECTION ( 'NONE',  ( 0.000000000000000000, 1.000000000000000000, -8.546850786086437571E-32 ) ) ;
#200746 = DIRECTION ( 'NONE',  ( -1.276756478318932585E-15, 1.000000000000000000, -1.665334536937738262E-16 ) ) ;
#200747 = ORIENTED_EDGE ( 'NONE', *, *, #90049, .F. ) ;
#200748 = CARTESIAN_POINT ( 'NONE',  ( 0.4623062725150044461, -1.170719190667910414, 1.764065175548671593 ) ) ;
#200750 = CARTESIAN_POINT ( 'NONE',  ( -8.993135964566285168, 9.386413468282476913, -0.7998128361456291469 ) ) ;
#200749 = CARTESIAN_POINT ( 'NONE',  ( -5.762378981008047241, 6.681529218386182301, 1.199719254218450271 ) ) ;
#200751 = CARTESIAN_POINT ( 'NONE',  ( 0.2691533882960769897, 1.057504993221158873, 1.506941669042777265 ) ) ;
#200752 = CARTESIAN_POINT ( 'NONE',  ( 3.204148022151423802, 0.7856563700287253482, -2.024084340642897661 ) ) ;
#200753 = CARTESIAN_POINT ( 'NONE',  ( 0.3596124336656087994, 2.795337124577100152, 2.035015742620380319 ) ) ;
#200754 = CARTESIAN_POINT ( 'NONE',  ( 1.195735321641926197, 1.957225868588155837, -0.8166992996602240318 ) ) ;
#200755 = CARTESIAN_POINT ( 'NONE',  ( -1.500000000000013101, 1.910416667349488451, -0.8660254037844313801 ) ) ;
#200756 = CARTESIAN_POINT ( 'NONE',  ( 8.028399517586572998, 12.51821653715971472, -0.7998128361456352531 ) ) ;
#200757 = CARTESIAN_POINT ( 'NONE',  ( 11.96212011828583677, 13.82812445049936834, -0.9569185076418588176 ) ) ;
#200758 = CARTESIAN_POINT ( 'NONE',  ( 6.536750166778501736, 6.811520125210166476, 0.4662371894542677864 ) ) ;
#200759 = CARTESIAN_POINT ( 'NONE',  ( 2.231779466116891708, -1.343800923419868010, -1.562491722542774797 ) ) ;
#200761 = DIRECTION ( 'NONE',  ( -0.000000000000000000, 1.000000000000000000, -0.000000000000000000 ) ) ;
#200760 = CARTESIAN_POINT ( 'NONE',  ( -9.642873567817536795, 12.27310513391906532, 1.599625672291281386 ) ) ;
#200762 = CARTESIAN_POINT ( 'NONE',  ( -1.201851678989727383E-14, 1.821875000341421691, 1.575800808251672791 ) ) ;
#200763 = PLANE ( 'NONE',  #94689 ) ;
#200764 = CARTESIAN_POINT ( 'NONE',  ( -3.733524485140432336, 7.410126666105575133, 2.499999999999998668 ) ) ;
#200765 = ORIENTED_EDGE ( 'NONE', *, *, #111897, .F. ) ;
#200766 = CARTESIAN_POINT ( 'NONE',  ( 4.688094572372190960, 1.103980140559155831, 1.561224650464939190 ) ) ;
#200767 = CARTESIAN_POINT ( 'NONE',  ( 11.92050416151432835, 12.44794624720375786, -1.381922468431410866 ) ) ;
#200768 = CARTESIAN_POINT ( 'NONE',  ( 1.036823874139713997, 2.229064601995099260, 0.3862009557947677640 ) ) ;
#200769 = CARTESIAN_POINT ( 'NONE',  ( -9.002250809793991948, 12.48608113052627289, -1.082531754730543971 ) ) ;
#200770 = CARTESIAN_POINT ( 'NONE',  ( 1.335881098409009704, -1.007921504507871102, -1.505067075931452392 ) ) ;
#200771 = CARTESIAN_POINT ( 'NONE',  ( 0.5498253489954890716, 0.9468162992772524156, 1.665335589065963129 ) ) ;
#200772 = CARTESIAN_POINT ( 'NONE',  ( 1.609917502266303480, 0.6029389078928657497, -1.980602105166151095 ) ) ;
#200773 = CARTESIAN_POINT ( 'NONE',  ( -1.402160292154681736E-14, 0.6343750003414162508, 1.575800808251672791 ) ) ;
#200774 = CARTESIAN_POINT ( 'NONE',  ( 6.789956943122251509, -0.7972922127613899512, 1.690610701080223821 ) ) ;
#200775 = CARTESIAN_POINT ( 'NONE',  ( 5.690048631714204497, -0.8642791622572744137, 1.721823430457876780 ) ) ;
#200777 = CARTESIAN_POINT ( 'NONE',  ( 5.559975706299111309, 7.414571502401146930, -1.245397951563255834 ) ) ;
#200776 = CARTESIAN_POINT ( 'NONE',  ( 0.2414294658986924358, 0.4011018576653562207, 2.272434410966933438 ) ) ;
#200778 = CARTESIAN_POINT ( 'NONE',  ( 0.6823417656249899377, 1.092708333674752286, 1.181850606188755259 ) ) ;
#200779 = CARTESIAN_POINT ( 'NONE',  ( 3.877431937021211361, -0.1548021625025173265, 2.056941320008953245 ) ) ;
#200780 = CARTESIAN_POINT ( 'NONE',  ( -7.223796917982883592, 7.322184580601816428, -0.7998128361456291469 ) ) ;
#200781 = CARTESIAN_POINT ( 'NONE',  ( 9.237182729612253951, 9.671134694169463586, 0.7998128361456462443 ) ) ;
#200782 = CARTESIAN_POINT ( 'NONE',  ( 5.190073875932979419, 4.949507698210251938, 0.7998128361456341429 ) ) ;
#200783 = CARTESIAN_POINT ( 'NONE',  ( 5.626797444871351139, 6.523350759560078593, 1.199719254218462483 ) ) ;
#200785 = CARTESIAN_POINT ( 'NONE',  ( -1.201851678989727383E-14, 3.712500000000020339, 1.732050807568877637 ) ) ;
#200784 = CARTESIAN_POINT ( 'NONE',  ( 4.876057405804426814, 1.210321851207227795, 1.723226277364843462 ) ) ;
#200786 = B_SPLINE_CURVE_WITH_KNOTS ( 'NONE', 3,
 ( #17904, #83990, #99199, #49379, #65587, #28060 ),
 .UNSPECIFIED., .F., .F.,
 ( 4, 2, 4 ),
 ( 0.000000000000000000, 0.0002955107118803974257, 0.0005910214237607931166 ),
 .UNSPECIFIED. ) ;
#200787 = CARTESIAN_POINT ( 'NONE',  ( 6.602015318333181781, 0.7961593463888805289, -1.911361562896146671 ) ) ;
#200788 = CARTESIAN_POINT ( 'NONE',  ( -0.6823417656250003738, 0.7802083336747520637, -1.181850606188749264 ) ) ;
#200789 = CARTESIAN_POINT ( 'NONE',  ( 4.552137767457805850, 2.161219302129935738, -0.04802546048104232301 ) ) ;
#200790 = CARTESIAN_POINT ( 'NONE',  ( 5.127605754342813960, -0.2940821729933600914, 1.998008755081616572 ) ) ;
#200791 = CARTESIAN_POINT ( 'NONE',  ( -0.1399997263889663501, 0.2375346743129815030, -2.034463206964792548 ) ) ;
#200794 = CARTESIAN_POINT ( 'NONE',  ( 5.829642864196162400, 7.824335979694092558, 1.443375672974062551 ) ) ;
#200793 = CARTESIAN_POINT ( 'NONE',  ( -3.285556943750000514, -1.888541666188711110, -1.896917185911906500 ) ) ;
#200792 = CARTESIAN_POINT ( 'NONE',  ( 7.309781096423290769, 8.557108029695882578, 1.199719254218452935 ) ) ;
#200795 = CARTESIAN_POINT ( 'NONE',  ( -6.631873415740034083, 7.766215735565355160, 1.199719254218452047 ) ) ;
#200796 = CARTESIAN_POINT ( 'NONE',  ( 3.995327539805045181, -0.3399590882401174463, 1.987497567597557468 ) ) ;
#200797 = CARTESIAN_POINT ( 'NONE',  ( -7.557780564614042795, 10.90482886110335414, -1.199719254218446718 ) ) ;
#200799 = CARTESIAN_POINT ( 'NONE',  ( -6.685579144870156476, 9.853573864773576219, 1.082531754730549967 ) ) ;
#200798 = CARTESIAN_POINT ( 'NONE',  ( -3.307299406729781399, 5.945934176904983381, -1.199719254218452935 ) ) ;
#200800 = CARTESIAN_POINT ( 'NONE',  ( -11.97929049433705551, 12.22000000000000064, -0.7046979865771821894 ) ) ;
#200801 = CARTESIAN_POINT ( 'NONE',  ( -2.449742653233059286, 3.300000000000011369, 0.3999999999999750422 ) ) ;
#200803 = CARTESIAN_POINT ( 'NONE',  ( 4.288685525864014636, 1.556897452430844320, -1.281376678550147474 ) ) ;
#200802 = CARTESIAN_POINT ( 'NONE',  ( -6.493992390821436977, 10.52014885602626393, 0.7216878364870458196 ) ) ;
#200804 = CARTESIAN_POINT ( 'NONE',  ( 1.499999999999989120, 5.504166666666685970, 0.8660254037844524744 ) ) ;
#200805 = CARTESIAN_POINT ( 'NONE',  ( 0.2754634098539961440, 0.9884889332615778290, 1.413329177942000303 ) ) ;
#200806 = CARTESIAN_POINT ( 'NONE',  ( 6.900173834712277632, 7.014900660111269559, -0.7998128361456341429 ) ) ;
#200808 = CARTESIAN_POINT ( 'NONE',  ( 1.980939963429169115, 3.482546949474367715, 0.4617747962883785862 ) ) ;
#200807 = CARTESIAN_POINT ( 'NONE',  ( 6.453317930424781856, 10.47269531889685545, -0.7216878364870267237 ) ) ;
#200809 = CIRCLE ( 'NONE', #194361, 0.04999999999999969746 ) ;
#200810 = CARTESIAN_POINT ( 'NONE',  ( -10.49167311136684866, 5.343773310534622567, 5.730690286876301442 ) ) ;
#200811 = CARTESIAN_POINT ( 'NONE',  ( 5.448468942325162878, 0.5420331153751513087, 1.790312535500695024 ) ) ;
#200812 = CARTESIAN_POINT ( 'NONE',  ( 5.976820168803962829, -1.420628428873932814, 1.426715538211227763 ) ) ;
#200813 = CARTESIAN_POINT ( 'NONE',  ( -4.230676207738683026, 3.979449701155983288, 0.5095693755076350362 ) ) ;
#200814 = CARTESIAN_POINT ( 'NONE',  ( -7.566859129758459979, 8.000626204239226880, 0.000000000000000000 ) ) ;
#200815 = ORIENTED_EDGE ( 'NONE', *, *, #186726, .T. ) ;
#200816 = CARTESIAN_POINT ( 'NONE',  ( 1.071888921174158016, -0.9040910708146729924, 1.802427947461216373 ) ) ;
#200817 = CARTESIAN_POINT ( 'NONE',  ( 1.072181177352715453, 0.7354878280073854357, 1.655762779942154372 ) ) ;
#200818 = CARTESIAN_POINT ( 'NONE',  ( 7.876360894896227371, 8.153785563659219804, -0.7998128361456341429 ) ) ;
#200819 = CARTESIAN_POINT ( 'NONE',  ( 6.561405286136596793, 0.3748316153167964848, -2.128808860954830795 ) ) ;
#200820 =( GEOMETRIC_REPRESENTATION_CONTEXT ( 3 ) GLOBAL_UNCERTAINTY_ASSIGNED_CONTEXT ( ( #161340 ) ) GLOBAL_UNIT_ASSIGNED_CONTEXT ( ( #71720, #56574, #122733 ) ) REPRESENTATION_CONTEXT ( 'NONE', 'WORKASPACE' ) );
#200821 = CARTESIAN_POINT ( 'NONE',  ( 5.601490020740366838, 9.686822124172440596, 1.040834085586084257E-14 ) ) ;
#200823 = CARTESIAN_POINT ( 'NONE',  ( -0.1181432109131977104, -1.915350881444439102, -0.04437447078771068754 ) ) ;
#200822 = CARTESIAN_POINT ( 'NONE',  ( -4.394814349124112951, 8.279033840620114049, -0.7998128361456281477 ) ) ;
#200824 = CARTESIAN_POINT ( 'NONE',  ( 11.55950211276791251, 11.37999999999999901, -3.221476510067114329 ) ) ;
#200825 = FILL_AREA_STYLE_COLOUR ( '', #142278 ) ;
#200826 = CARTESIAN_POINT ( 'NONE',  ( 1.364683531249986537, -0.7822916663252464931, -0.7879004041258309554 ) ) ;
#200827 = CARTESIAN_POINT ( 'NONE',  ( 4.541618270897912701, 4.400902192243413502, 1.214306433183764966E-14 ) ) ;
#200828 = CARTESIAN_POINT ( 'NONE',  ( -9.110189153378817295, 12.71597221466224603, 1.199719254218462483 ) ) ;
#200829 = CARTESIAN_POINT ( 'NONE',  ( 3.784175263432405956, -1.067420458145739826, 1.879713924940962677 ) ) ;
#200830 = CARTESIAN_POINT ( 'NONE',  ( -6.617788377246196951, 7.853746207276256719, -1.082531754730549967 ) ) ;
#200831 = CARTESIAN_POINT ( 'NONE',  ( 5.207740401424913124, 9.089797878388800711, -0.7216878364870458196 ) ) ;
#200832 = CARTESIAN_POINT ( 'NONE',  ( 0.5980879788009090259, 1.428637019467562830, 1.567290143595565066 ) ) ;
#200833 = CARTESIAN_POINT ( 'NONE',  ( 4.177028312937637544, 3.976447072691611684, -0.04407265314626420544 ) ) ;
#200834 = CARTESIAN_POINT ( 'NONE',  ( 2.530492563074437928, 1.911271491015430035, 0.4824842627236708426 ) ) ;
#200835 = CARTESIAN_POINT ( 'NONE',  ( 4.394721148579957770, -1.856311205515799312, -0.4593126252911489127 ) ) ;
#200836 = ORIENTED_EDGE ( 'NONE', *, *, #211067, .F. ) ;
#200837 = FACE_OUTER_BOUND ( 'NONE', #26092, .T. ) ;
#200838 = CARTESIAN_POINT ( 'NONE',  ( 6.584429662329396749, 1.135205087083859476, -1.609268749140836618 ) ) ;
#200839 = CARTESIAN_POINT ( 'NONE',  ( 1.165847801482827517, -1.232189268765693235, 1.500965459471349961 ) ) ;
#200840 = ORIENTED_EDGE ( 'NONE', *, *, #108295, .F. ) ;
#200841 = CARTESIAN_POINT ( 'NONE',  ( -5.822300622425855110, 5.757381912443740646, 0.7998128361456281477 ) ) ;
#200843 = FACE_OUTER_BOUND ( 'NONE', #163884, .T. ) ;
#200842 = CARTESIAN_POINT ( 'NONE',  ( -7.024532985656169792, 9.288650798055913427, 1.443375672974064550 ) ) ;
#200845 = CARTESIAN_POINT ( 'NONE',  ( 5.465345319640213972, 8.429967735338637524, -1.082531754730548412 ) ) ;
#200844 = CARTESIAN_POINT ( 'NONE',  ( 8.118635056484817980, 8.366162408854107113, 0.7998128361456481317 ) ) ;
#200847 = ORIENTED_EDGE ( 'NONE', *, *, #119697, .T. ) ;
#200846 = CARTESIAN_POINT ( 'NONE',  ( 4.723256143441832755, 1.665581346147155806, 0.9393396248940300008 ) ) ;
#200848 = CARTESIAN_POINT ( 'NONE',  ( 3.563272299071856164, -1.946135509614330239, -1.040604674307284316 ) ) ;
#200849 = EDGE_CURVE ( 'NONE', #182678, #106531, #19862, .T. ) ;
#200850 = CARTESIAN_POINT ( 'NONE',  ( 1.677102584378454608, -2.095606157416990190, -0.6917391671936305997 ) ) ;
#200851 = DIRECTION ( 'NONE',  ( 0.000000000000000000, -1.000000000000000000, 0.000000000000000000 ) ) ;
#200852 = CARTESIAN_POINT ( 'NONE',  ( 1.137202173061176547, -0.04613941135153502154, 1.911881008470908139 ) ) ;
#200853 = B_SPLINE_CURVE_WITH_KNOTS ( 'NONE', 3,
 ( #2847, #184808, #185875, #37511, #152333, #150212, #153400 ),
 .UNSPECIFIED., .F., .F.,
 ( 4, 3, 4 ),
 ( 0.000000000000000000, 2.778074687866575757E-05, 5.739355541035052121E-05 ),
 .UNSPECIFIED. ) ;
#200854 = CARTESIAN_POINT ( 'NONE',  ( -0.4019237886466933696, 8.801335450315374231, 1.500000000000005995 ) ) ;
#200856 = CARTESIAN_POINT ( 'NONE',  ( -2.335117776279159951, 5.399932185023237352, 0.6440902300205594289 ) ) ;
#200855 = PRESENTATION_LAYER_ASSIGNMENT (  '', '', ( #86633 ) ) ;
#200857 = CARTESIAN_POINT ( 'NONE',  ( 7.785697387528199762E-15, 0.4375000000000076605, -1.225000000000032951 ) ) ;
#200858 = CARTESIAN_POINT ( 'NONE',  ( 3.490741092712910998, 2.019281663078629219, 0.4563312328872349277 ) ) ;
#200859 = CARTESIAN_POINT ( 'NONE',  ( -6.196239896645333367, 7.187700286629718605, -1.199719254218446718 ) ) ;
#200860 = CARTESIAN_POINT ( 'NONE',  ( -4.864640111294652236, 8.076240785039992431, 0.9165970657895030627 ) ) ;
#200862 = CARTESIAN_POINT ( 'NONE',  ( 0.5323697292517782786, 1.110078392871534314, -1.854780036684190669 ) ) ;
#200861 = CARTESIAN_POINT ( 'NONE',  ( -3.741160322367112379, 6.452105245148518797, 1.199719254218464037 ) ) ;
#200863 = CARTESIAN_POINT ( 'NONE',  ( 3.228257827484398490, 2.138632370135685523, 0.4780590757816546854 ) ) ;
#200864 = CIRCLE ( 'NONE', #152509, 2.250000000000006661 ) ;
#200865 = DIRECTION ( 'NONE',  ( 5.578564026256490882E-16, 1.000000000000000000, 9.066213480720158442E-32 ) ) ;
#200866 = ADVANCED_FACE ( 'NONE', ( #118898 ), #116873, .T. ) ;
#200867 = CARTESIAN_POINT ( 'NONE',  ( 4.773879485787624333, 4.742149952939897162, -0.7216878364870357165 ) ) ;
#200868 = CARTESIAN_POINT ( 'NONE',  ( 0.3912817730720326015, -6.709848117146032465, 9.483257663143165317 ) ) ;
#200869 = CARTESIAN_POINT ( 'NONE',  ( 1.364683531249997417, 13.54687500034139980, 2.602085213965210642E-15 ) ) ;
#200870 = CARTESIAN_POINT ( 'NONE',  ( -6.168033539574333979, 6.160736982450306876, 0.7998128361456281477 ) ) ;
#200871 = EDGE_CURVE ( 'NONE', #192999, #107993, #23407, .T. ) ;
#200872 = CARTESIAN_POINT ( 'NONE',  ( 5.713412806352172524, 1.673543110082301721, 0.4542079487798825199 ) ) ;
#200873 = CARTESIAN_POINT ( 'NONE',  ( -8.337901282724359930, 12.67137589657970409, 1.040834085586084257E-14 ) ) ;
#200874 = CARTESIAN_POINT ( 'NONE',  ( 3.379797469122407083, -1.996479967689598789, 0.5476083754193948883 ) ) ;
#200875 = CARTESIAN_POINT ( 'NONE',  ( 4.341493734318905950, 0.4621530863439751724, -2.066033417628045932 ) ) ;
#200876 = CARTESIAN_POINT ( 'NONE',  ( 5.113396490648394632, 9.117379672398465473, 1.040834085586084257E-14 ) ) ;
#200877 = CARTESIAN_POINT ( 'NONE',  ( -1.364683531250010740, 5.238541667008085767, -0.7879004041258300672 ) ) ;
#200878 = CARTESIAN_POINT ( 'NONE',  ( 3.309381622104785148, -1.607321225346239668, -1.137771303188861660 ) ) ;
#200879 = CARTESIAN_POINT ( 'NONE',  ( 0.4219365929402639215, -1.902980170924161385, 0.1897552588234762416 ) ) ;
#200880 = CARTESIAN_POINT ( 'NONE',  ( 4.998102599042142380, -0.7687487195138610341, -2.159632177038037337 ) ) ;
#200881 = CARTESIAN_POINT ( 'NONE',  ( 2.859763506297557711, 1.816872213737670938, -0.1792109616642542924 ) ) ;
#200882 = CARTESIAN_POINT ( 'NONE',  ( 3.040771591214902259, 6.769593633051179005, -0.7998128361456362523 ) ) ;
#200883 = CARTESIAN_POINT ( 'NONE',  ( 4.487385655998867406, 8.179107665399927285, 0.7216878364870438212 ) ) ;
#200884 = CARTESIAN_POINT ( 'NONE',  ( -6.880926654135487652, 7.986501503701545879, 1.199719254218450271 ) ) ;
#200885 = CARTESIAN_POINT ( 'NONE',  ( 4.236591777569945982, 1.235091891264840314, -1.589779643154372701 ) ) ;
#200886 = CARTESIAN_POINT ( 'NONE',  ( 4.030091663008243508, 1.086175826233202857, 1.633415718976807041 ) ) ;
#200887 = CARTESIAN_POINT ( 'NONE',  ( -6.398558430645608475, 9.552403038140164782, -1.199719254218440723 ) ) ;
#200888 = CARTESIAN_POINT ( 'NONE',  ( -4.076197739202962467, 7.907314462378773001, 1.040834085586084257E-14 ) ) ;
#200889 = CARTESIAN_POINT ( 'NONE',  ( 0.1755611466353447780, 1.308645672766622914, -2.493865953706751792 ) ) ;
#200891 = CARTESIAN_POINT ( 'NONE',  ( 5.981276632755388789, 1.633781900041403334, -0.6810181619275444964 ) ) ;
#200890 = CARTESIAN_POINT ( 'NONE',  ( 0.08173368997131927327, -0.9817114319007680390, 1.845913477919949086 ) ) ;
#200892 = CARTESIAN_POINT ( 'NONE',  ( 10.96785329849812918, -5.223431457505069098, -0.4373225248172805113 ) ) ;
#200893 = CARTESIAN_POINT ( 'NONE',  ( 1.517799938645987057, -1.219565478727736574, -1.820545776841306029 ) ) ;
#200894 = CARTESIAN_POINT ( 'NONE',  ( 6.246048974015395494, 0.5531718476652900396, 1.650163303580793217 ) ) ;
#200895 = CARTESIAN_POINT ( 'NONE',  ( 7.396136491454752715, 8.587579647240744407, 1.199719254218462483 ) ) ;
#200896 = CARTESIAN_POINT ( 'NONE',  ( 0.2335667940002632559, 2.006215057630795773, -2.568298294197084886 ) ) ;
#200897 = CARTESIAN_POINT ( 'NONE',  ( 0.6973489402126078485, -0.6253137818992074992, 1.607738891190332753 ) ) ;
#200898 = CARTESIAN_POINT ( 'NONE',  ( 0.4921457485732755321, 2.200376924867069484, 0.6639341530902067579 ) ) ;
#200899 = CARTESIAN_POINT ( 'NONE',  ( 0.6268464039562298140, 0.1668571106153530770, 2.185281662807083691 ) ) ;
#200900 = CARTESIAN_POINT ( 'NONE',  ( 2.702037527177497012, -0.6914408288211832954, 2.095836555436859872 ) ) ;
#200901 = CARTESIAN_POINT ( 'NONE',  ( 6.672352044927558623, -1.017530931492259816, -1.917974758356699505 ) ) ;
#200902 = CARTESIAN_POINT ( 'NONE',  ( 1.499999999999989120, 4.004166666666685970, 0.8660254037844522523 ) ) ;
#200903 = CARTESIAN_POINT ( 'NONE',  ( 0.8841682305550628840, -2.117513412274423690, 0.006320426156874307463 ) ) ;
#200904 = CARTESIAN_POINT ( 'NONE',  ( 6.727182134110237577, 2.938513203633616566, 2.740843696613648017 ) ) ;
#200905 = CARTESIAN_POINT ( 'NONE',  ( 5.262690832784179484, -1.395389315813623909, 1.328347855495640273 ) ) ;
#200906 = ORIENTED_EDGE ( 'NONE', *, *, #186853, .F. ) ;
#200908 = CARTESIAN_POINT ( 'NONE',  ( 0.6823417656249864960, -1.011458332991911568, -1.181850606188749264 ) ) ;
#200907 = CARTESIAN_POINT ( 'NONE',  ( 1.171857018789014271, 1.370485515009724820, 1.837452469633732210 ) ) ;
#200909 = CARTESIAN_POINT ( 'NONE',  ( 3.979481780810941949, 4.601482484822914998, 1.199719254218464037 ) ) ;
#200910 = B_SPLINE_CURVE_WITH_KNOTS ( 'NONE', 3,
 ( #178308, #127503, #76514, #60267, #143708, #142625 ),
 .UNSPECIFIED., .F., .F.,
 ( 4, 2, 4 ),
 ( 0.000000000000000000, 0.001225895755212361464, 0.002451791510424722927 ),
 .UNSPECIFIED. ) ;
#200911 = CARTESIAN_POINT ( 'NONE',  ( 4.821896187954575197, 8.777295985922343391, 0.7998128361456462443 ) ) ;
#200912 = CARTESIAN_POINT ( 'NONE',  ( 3.844553043330910747, 1.187701353711614338, -1.876932147738763268 ) ) ;
#200913 = CARTESIAN_POINT ( 'NONE',  ( -6.371969008742801144, 10.37778824360119145, 0.7216878364870458196 ) ) ;
#200914 =( NAMED_UNIT ( * ) SI_UNIT ( $, .STERADIAN. ) SOLID_ANGLE_UNIT ( ) );
#200915 = CARTESIAN_POINT ( 'NONE',  ( 4.677199807034550183, 8.400557508274889784, 1.040834085586084257E-14 ) ) ;
#200916 = CARTESIAN_POINT ( 'NONE',  ( -8.148087131688692253, 10.52918762510205042, -1.443375672974058777 ) ) ;
#200917 =( GEOMETRIC_REPRESENTATION_CONTEXT ( 3 ) GLOBAL_UNCERTAINTY_ASSIGNED_CONTEXT ( ( #160207 ) ) GLOBAL_UNIT_ASSIGNED_CONTEXT ( ( #179115, #181227, #198527 ) ) REPRESENTATION_CONTEXT ( 'NONE', 'WORKASPACE' ) );
#200918 = CARTESIAN_POINT ( 'NONE',  ( 5.343321937561575474, 8.287607122913563273, -1.082531754730548412 ) ) ;
#200919 = CARTESIAN_POINT ( 'NONE',  ( 1.916638904718031000, -1.319229391439219246, -1.525043083973671498 ) ) ;
#200921 = CARTESIAN_POINT ( 'NONE',  ( 0.6552251538811122433, 1.716912266053271408, -1.142698840430116602 ) ) ;
#200920 = CARTESIAN_POINT ( 'NONE',  ( 7.076466111328892694, 10.34329533227067799, -1.199719254218441611 ) ) ;
#200922 = FILL_AREA_STYLE_COLOUR ( '', #61226 ) ;
#200923 = CARTESIAN_POINT ( 'NONE',  ( 5.899206235277530297, 7.015400374979486209, -1.082531754730548412 ) ) ;
#200924 = DIRECTION ( 'NONE',  ( 0.000000000000000000, -0.000000000000000000, 1.000000000000000000 ) ) ;
#200925 = CARTESIAN_POINT ( 'NONE',  ( -0.6823417656250212460, 3.801041667008085767, 1.181850606188767472 ) ) ;
#200926 = CARTESIAN_POINT ( 'NONE',  ( 4.242245924764226572, 0.5834501570099770440, 2.112278566661344392 ) ) ;
#200927 = CARTESIAN_POINT ( 'NONE',  ( 0.9850002542920628379, -2.016597020373378513, 0.002813405579435435122 ) ) ;
#200928 = CARTESIAN_POINT ( 'NONE',  ( 0.7668492355173107677, 1.774547462407764842, -0.4907661837717376407 ) ) ;
#200929 = CARTESIAN_POINT ( 'NONE',  ( 5.161814014510654580, 1.128026202373041853, 1.995582457067740068 ) ) ;
#200930 = CARTESIAN_POINT ( 'NONE',  ( 3.011469152984513009, -0.9080073089506625061, -1.601583425259824001 ) ) ;
#200931 = ADVANCED_FACE ( 'NONE', ( #207547 ), #6127, .F. ) ;
#200932 = CARTESIAN_POINT ( 'NONE',  ( 7.476431642932036326, 10.80992178580769014, 1.199719254218460707 ) ) ;
#200933 = CARTESIAN_POINT ( 'NONE',  ( 4.190329584092522097, -1.805708503706305423, -0.2678305112727846771 ) ) ;
#200934 = CARTESIAN_POINT ( 'NONE',  ( 4.623672751230786027, 0.3474658942751900903, 1.986100912583692812 ) ) ;
#200935 = CARTESIAN_POINT ( 'NONE',  ( -9.176171038350775078, 9.599954387697719582, -0.7998128361456291469 ) ) ;
#200937 = CARTESIAN_POINT ( 'NONE',  ( -6.444921918449773024, 8.612437886315108315, 1.599625672291269396 ) ) ;
#200936 = CARTESIAN_POINT ( 'NONE',  ( 4.241306175801488720, -1.970289653591940970, 1.112044505652502346 ) ) ;
#200938 = CARTESIAN_POINT ( 'NONE',  ( 6.651405291617982662, -1.688965747674558759, -1.257743519153362355 ) ) ;
#200939 = CARTESIAN_POINT ( 'NONE',  ( 4.255647627037042355E-16, -6.776263578034402713E-18, 3.474999999999992095 ) ) ;
#200940 = CARTESIAN_POINT ( 'NONE',  ( 3.719242722441223226, -1.824546119899137731, -0.9785211796824041519 ) ) ;
#200941 = CARTESIAN_POINT ( 'NONE',  ( 2.367870383881045981, 5.914265881169853856, 0.000000000000000000 ) ) ;
#200942 = CARTESIAN_POINT ( 'NONE',  ( -1.360316468750002672, 1.921875000341424666, -3.642919299551294898E-14 ) ) ;
#200943 = SHAPE_DEFINITION_REPRESENTATION ( #142260, #137092 ) ;
#200945 = CARTESIAN_POINT ( 'NONE',  ( 1.594233254470639238, -1.917152233794093164, -0.1895178900164773139 ) ) ;
#200944 = CARTESIAN_POINT ( 'NONE',  ( -9.667127221743832877, 11.23706883257798772, 1.199719254218462483 ) ) ;
#200946 = CARTESIAN_POINT ( 'NONE',  ( -9.748756651491515157, 4.000000000000000888, 7.301653494243616649 ) ) ;
#200947 = CARTESIAN_POINT ( 'NONE',  ( 6.543809977506837683, 1.355650292293397507, 1.428865145875155340 ) ) ;
#200948 = CARTESIAN_POINT ( 'NONE',  ( 5.194182247366878613, 6.192872389083746043, 1.082531754730549078 ) ) ;
#200949 = CARTESIAN_POINT ( 'NONE',  ( 5.891837173953166307, 5.977390820968681240, -0.04595957878574669087 ) ) ;
#200950 = CARTESIAN_POINT ( 'NONE',  ( 1.230761180058546289, 3.271116465842660581, -0.7749999999999874767 ) ) ;
#200951 = CARTESIAN_POINT ( 'NONE',  ( -4.613852347352193739, 4.277249248199312071, 1.214306433183764966E-14 ) ) ;
#200952 = CARTESIAN_POINT ( 'NONE',  ( 2.092296997076743548, 1.370790743785160970, 1.747926019109148799 ) ) ;
#200953 = CARTESIAN_POINT ( 'NONE',  ( 3.452270085047473458, 2.106147100029008179, 0.001788861226008006461 ) ) ;
#200955 = CARTESIAN_POINT ( 'NONE',  ( -6.936931872047518155, 8.122117267924091166, 1.199719254218452047 ) ) ;
#200954 = STYLED_ITEM ( 'NONE', ( #53801 ), #170192 ) ;
#200956 = CARTESIAN_POINT ( 'NONE',  ( 7.949158136313996259, 8.168439335321471262, 1.040834085586084257E-14 ) ) ;
#200957 = CARTESIAN_POINT ( 'NONE',  ( 1.011883965753940018, 1.859189825682316277, -0.08597224477241424689 ) ) ;
#200958 = CARTESIAN_POINT ( 'NONE',  ( 7.447506452608354088, 7.583179037664891098, 0.7998128361456341429 ) ) ;
#200959 = EDGE_CURVE ( 'NONE', #26788, #95577, #26665, .T. ) ;
#200960 = CARTESIAN_POINT ( 'NONE',  ( 3.988069740714122791, 7.804498464141805592, 0.7998128361456321445 ) ) ;
#200961 = CARTESIAN_POINT ( 'NONE',  ( -6.780486220610195680, 7.083191143566240910, -0.7216878364870338292 ) ) ;
#200962 = CARTESIAN_POINT ( 'NONE',  ( -7.863365906246068349, 9.236643647784308797, -1.082531754730543971 ) ) ;
#200963 = CARTESIAN_POINT ( 'NONE',  ( 0.8793290508635929204, -1.919567575575848339, -0.9014759086384205311 ) ) ;
#200964 = CARTESIAN_POINT ( 'NONE',  ( -6.343235766347277149, 8.493804042195527870, -1.599625672291271394 ) ) ;
#200966 = CARTESIAN_POINT ( 'NONE',  ( 4.914483161888778540, 0.7490505147796695518, 1.813437088826752142 ) ) ;
#200965 = CARTESIAN_POINT ( 'NONE',  ( -1.225000000000016076, 0.2708333333333532988, 0.7072540797572717253 ) ) ;
#200967 = CARTESIAN_POINT ( 'NONE',  ( 3.766626874709140704, -1.453462046928340579, 1.600284095077113333 ) ) ;
#200968 = CARTESIAN_POINT ( 'NONE',  ( 1.505144418776669601, -1.827259764946763454, 0.2261131901925839127 ) ) ;
#200969 = CARTESIAN_POINT ( 'NONE',  ( -4.026828402897194792, 7.608452879803509816, -0.2354461595876176927 ) ) ;
#200970 = CARTESIAN_POINT ( 'NONE',  ( 4.806723615010448736E-13, -7.868798029037617603, -9.500000000000001776 ) ) ;
#200971 = CARTESIAN_POINT ( 'NONE',  ( 5.068161541800582093, -1.640353732806285825, -0.5817517365288951137 ) ) ;
#200972 = CARTESIAN_POINT ( 'NONE',  ( -6.671583288098925202, 14.00000000000492939, -9.747470831327131435 ) ) ;
#200973 = CARTESIAN_POINT ( 'NONE',  ( 4.202664430556241726, 7.846932902383524144, 0.7216878364870298324 ) ) ;
#200974 = CARTESIAN_POINT ( 'NONE',  ( -10.37109829931902816, 6.927524423111719898, -5.134218648570218591 ) ) ;
#200975 = CIRCLE ( 'NONE', #21154, 2.000000000000000000 ) ;
#200976 = CARTESIAN_POINT ( 'NONE',  ( 1.534274790466340299, 1.065227450066742687, -1.880959520452238465 ) ) ;
#200977 = CARTESIAN_POINT ( 'NONE',  ( 2.987657498945671897, 1.897406709466815444, 0.6818930838706839248 ) ) ;
#200978 = CARTESIAN_POINT ( 'NONE',  ( -8.907343734053998929, 12.37535620882957588, 1.082531754730558626 ) ) ;
#200979 = CARTESIAN_POINT ( 'NONE',  ( 1.569428280142046717, 0.1587979871724466974, -2.155937297210829495 ) ) ;
#200980 = CARTESIAN_POINT ( 'NONE',  ( 3.028153684870387607, 1.096474020163393792, -1.638230769948149534 ) ) ;
#200981 = CARTESIAN_POINT ( 'NONE',  ( 6.509000000000047415, 2.458121647476101401, 2.283885694139938138 ) ) ;
#200982 = CARTESIAN_POINT ( 'NONE',  ( 3.509261751715045730, -1.912814363422868480, 0.3349611914155846693 ) ) ;
#200986 = ORIENTED_EDGE ( 'NONE', *, *, #4745, .F. ) ;
#200985 = EDGE_CURVE ( 'NONE', #122127, #126275, #84957, .T. ) ;
#200984 = CARTESIAN_POINT ( 'NONE',  ( -5.153507786970285665, 5.185049637652990207, -0.7216878364870338292 ) ) ;
#200983 = CARTESIAN_POINT ( 'NONE',  ( -9.449669878600616357, 12.04770082983265844, -1.443375672974058777 ) ) ;
#200987 = CARTESIAN_POINT ( 'NONE',  ( -4.123088111887291518, 7.824370207261548416, 0.000000000000000000 ) ) ;
#200988 = CARTESIAN_POINT ( 'NONE',  ( -0.1108833634137010582, 5.723767666350643601, -2.491012016648496363 ) ) ;
#200989 = CARTESIAN_POINT ( 'NONE',  ( 4.766573523656222555, 7.718696989977711809, 1.199719254218452047 ) ) ;
#200990 = CARTESIAN_POINT ( 'NONE',  ( -3.969505113751027547, 7.853116076009993840, 1.214306433183764966E-14 ) ) ;
#200991 = CARTESIAN_POINT ( 'NONE',  ( -5.661411662158206681, 8.762674818229999829, -1.199719254218452047 ) ) ;
#200992 = CARTESIAN_POINT ( 'NONE',  ( -8.636180661780658241, 12.05899929117736846, -1.082531754730543083 ) ) ;
#200993 = ADVANCED_FACE ( 'NONE', ( #155612 ), #81432, .T. ) ;
#200994 = CARTESIAN_POINT ( 'NONE',  ( 6.721674876502457430, -2.240710703332372766, 0.5512419492274822641 ) ) ;
#200995 = CARTESIAN_POINT ( 'NONE',  ( 3.285556943750000070, -3.084374999522042415, 0.000000000000000000 ) ) ;
#200996 = CARTESIAN_POINT ( 'NONE',  ( 4.065250617491710905, 1.680331827152386159, 1.012218702928203706 ) ) ;
#200997 = CARTESIAN_POINT ( 'NONE',  ( 7.904567251967224095, 9.180748867838630645, 1.199719254218462483 ) ) ;
#200998 = CARTESIAN_POINT ( 'NONE',  ( 2.092422861153935276, -0.4390285686692517175, 1.967888031366466395 ) ) ;
#200999 = ORIENTED_EDGE ( 'NONE', *, *, #34638, .F. ) ;
#201000 = CARTESIAN_POINT ( 'NONE',  ( 3.186815374238487930, 1.666415522689016049, -1.306070977860743110 ) ) ;
#201001 = CARTESIAN_POINT ( 'NONE',  ( -1.499999999999997780, 1.681250000682817047, 0.000000000000000000 ) ) ;
#201003 = CARTESIAN_POINT ( 'NONE',  ( -6.389970470742427189, 6.349387058821269747, -0.7998128361456291469 ) ) ;
#201002 = CARTESIAN_POINT ( 'NONE',  ( 0.07459516483346650961, 6.948550711820903558, -2.350542341214032493 ) ) ;
#201004 = CARTESIAN_POINT ( 'NONE',  ( 2.958754162918545205, 0.2696264243384552950, -1.821159755858774654 ) ) ;
#201005 = ORIENTED_EDGE ( 'NONE', *, *, #153308, .T. ) ;
#201006 = CARTESIAN_POINT ( 'NONE',  ( -9.820183334999905256, 10.35130206712171130, 1.040834085586084257E-14 ) ) ;
#201007 = CARTESIAN_POINT ( 'NONE',  ( 0.000000000000000000, 3.956598013261175772, 0.000000000000000000 ) ) ;
#201008 = CARTESIAN_POINT ( 'NONE',  ( 3.937823072884456099, -2.028283017459261650, 0.6187693826033290323 ) ) ;
#201009 = CARTESIAN_POINT ( 'NONE',  ( 0.4999999999999674705, 3.999999999999989786, 0.4499999999999625966 ) ) ;
#201010 = CARTESIAN_POINT ( 'NONE',  ( 6.745345117998789775, 7.828323044875442172, 1.199719254218462483 ) ) ;
#201011 = CARTESIAN_POINT ( 'NONE',  ( 5.202442474109128412, -0.6904536177961515531, -1.941828258638809368 ) ) ;
#201013 = CARTESIAN_POINT ( 'NONE',  ( 2.542321706073047416, -1.529623444112483632, 1.024600984555257277 ) ) ;
#201012 = CARTESIAN_POINT ( 'NONE',  ( 1.205250485101029723, -1.463924481597483007, -1.148973905474151014 ) ) ;
#201014 = CARTESIAN_POINT ( 'NONE',  ( 8.666686507633574621, 11.13422023037111330, 1.599625672291281386 ) ) ;
#201015 = CARTESIAN_POINT ( 'NONE',  ( 4.469950146539259705, 7.269956441268025316, -1.287814263469128750 ) ) ;
#201016 =( BOUNDED_CURVE ( )  B_SPLINE_CURVE ( 3, ( #53987, #136317, #172010, #23602 ),
 .UNSPECIFIED., .F., .T. ) 
 B_SPLINE_CURVE_WITH_KNOTS ( ( 4, 4 ),
 ( 1.420228054018210617, 1.445468495626831329 ),
 .UNSPECIFIED. ) 
 CURVE ( )  GEOMETRIC_REPRESENTATION_ITEM ( )  RATIONAL_B_SPLINE_CURVE ( ( 1.000000000000000000, 0.9999469107135832147, 0.9999469107135832147, 1.000000000000000000 ) ) 
 REPRESENTATION_ITEM ( '' )  );
#201017 = CARTESIAN_POINT ( 'NONE',  ( -8.120407659942227241, 8.438506789546210030, 0.7998128361456341429 ) ) ;
#201018 = CARTESIAN_POINT ( 'NONE',  ( 10.98194350564910593, -7.666862915010147717, -0.6300133639306331190 ) ) ;
#201019 = AXIS2_PLACEMENT_3D ( 'NONE', #93166, #45475, #128919 ) ;
#201020 = CARTESIAN_POINT ( 'NONE',  ( 1.963769682107346037, 0.3752889857368995608, -2.174583152744386627 ) ) ;
#201021 = CARTESIAN_POINT ( 'NONE',  ( 4.991644252507740021, 1.671830779756987573, 1.524457814443666903 ) ) ;
#201022 = AXIS2_PLACEMENT_3D ( 'NONE', #62336, #212831, #48242 ) ;
#201023 = CARTESIAN_POINT ( 'NONE',  ( -7.375272376154096143, 8.667201196010339004, -1.082531754730544860 ) ) ;
#201024 = CARTESIAN_POINT ( 'NONE',  ( 4.552869461240817373, 0.3164949366275445208, 1.783561479213832346 ) ) ;
#201025 = CARTESIAN_POINT ( 'NONE',  ( 4.294081978838642399, -0.8244651323695743050, -1.729401801750865442 ) ) ;
#201026 = EDGE_CURVE ( 'NONE', #71404, #38200, #201170, .T. ) ;
#201027 = CARTESIAN_POINT ( 'NONE',  ( -1.201851678989727383E-14, 4.259375000341417028, -1.575800808251660134 ) ) ;
#201028 = CARTESIAN_POINT ( 'NONE',  ( 4.030118584743531684, 1.055711351780568741, -1.664808796107832389 ) ) ;
#201029 = CARTESIAN_POINT ( 'NONE',  ( 5.155093292349416600, -1.580716073637401076, -1.000049079914612449 ) ) ;
#201030 = CARTESIAN_POINT ( 'NONE',  ( 5.072628826387419743, 1.283713728693743894, -1.347665127999774448 ) ) ;
#201031 = CARTESIAN_POINT ( 'NONE',  ( 0.6823417656249899377, 5.426041667008087543, -1.181850606188754593 ) ) ;
#201032 = CARTESIAN_POINT ( 'NONE',  ( 0.02267320670834571672, 0.3494893071277604402, 1.985867805234131644 ) ) ;
#201034 = CARTESIAN_POINT ( 'NONE',  ( 1.594499780405156830, -2.096077427685174577, -0.2048490792218547185 ) ) ;
#201033 = CARTESIAN_POINT ( 'NONE',  ( -4.256897044566581911, 4.068727428190179296, 1.214306433183764966E-14 ) ) ;
#201035 = CARTESIAN_POINT ( 'NONE',  ( 9.317477881089539338, 11.89347683273640932, 1.599625672291279388 ) ) ;
#201037 = CARTESIAN_POINT ( 'NONE',  ( -9.022061154889962964, 12.61315621642528129, -1.199719254218446718 ) ) ;
#201036 = CARTESIAN_POINT ( 'NONE',  ( 1.364683531249988535, 4.967708333674756283, -0.7879004041258300672 ) ) ;
#201038 = CARTESIAN_POINT ( 'NONE',  ( 3.375340920106313813, -1.871962376360849056, -0.9962781187466958066 ) ) ;
#201039 = CARTESIAN_POINT ( 'NONE',  ( 0.000000000000000000, 0.5000000000000004441, -3.475000000000000089 ) ) ;
#201040 = CARTESIAN_POINT ( 'NONE',  ( 1.582292005822239167, 1.041880795974026608, 1.730197787189115433 ) ) ;
#201041 = CARTESIAN_POINT ( 'NONE',  ( -0.6823417656250212460, 1.551041667008083769, 1.181850606188755259 ) ) ;
#201042 = CARTESIAN_POINT ( 'NONE',  ( -4.012850279964973232, 4.744375417122949301, 1.082531754730560403 ) ) ;
#201043 = CARTESIAN_POINT ( 'NONE',  ( 5.522248639467795428, 5.337044922334209573, -0.7998128361456231517 ) ) ;
#201044 = ORIENTED_EDGE ( 'NONE', *, *, #175741, .T. ) ;
#201045 = CARTESIAN_POINT ( 'NONE',  ( 2.636181727411972098, 1.021492356387411427, -1.905029093917938399 ) ) ;
#201046 = CARTESIAN_POINT ( 'NONE',  ( 6.890000000000005898, 2.048573291599069091, 2.305811639209849773 ) ) ;
#201049 = CARTESIAN_POINT ( 'NONE',  ( 2.236732156574683827, 5.553345249405011508, 1.040834085586084257E-14 ) ) ;
#201048 = CARTESIAN_POINT ( 'NONE',  ( -5.905025204060999400, 4.805319369736078094, -2.499999999999995115 ) ) ;
#201047 = CARTESIAN_POINT ( 'NONE',  ( 5.032011289327418702, 5.899709921417326974, 1.199719254218452935 ) ) ;
#201050 = CARTESIAN_POINT ( 'NONE',  ( 1.249000902703301108E-16, 4.500000000000003553, -2.250000000000006661 ) ) ;
#201051 = CARTESIAN_POINT ( 'NONE',  ( -7.720982910012857303, -6.306565840633416187, 7.834948813061215489 ) ) ;
#201052 = CARTESIAN_POINT ( 'NONE',  ( -7.537970219518089543, 8.857015346601659900, -1.082531754730543971 ) ) ;
#201053 = ADVANCED_FACE ( 'NONE', ( #104738 ), #22376, .T. ) ;
#201054 = CARTESIAN_POINT ( 'NONE',  ( 0.5038066827526345159, -2.180447833630628107, 0.2205874978757973448 ) ) ;
#201055 = CARTESIAN_POINT ( 'NONE',  ( 3.946537740505224878, 2.817530495244566335, 0.7750000000000135669 ) ) ;
#201057 = CARTESIAN_POINT ( 'NONE',  ( -1.364683531250000748, 12.60937500034139980, 0.000000000000000000 ) ) ;
#201056 = CARTESIAN_POINT ( 'NONE',  ( 1.393865445735403830, 1.714438158727617179, 1.476448846179352348 ) ) ;
#201058 = CARTESIAN_POINT ( 'NONE',  ( -8.565000355531095622, 11.01558638625153286, -1.599625672291263179 ) ) ;
#201059 = CARTESIAN_POINT ( 'NONE',  ( -3.240035523541616502, 6.723865844199768738, 0.7216878364870317197 ) ) ;
#201060 = CARTESIAN_POINT ( 'NONE',  ( 1.364683531249988757, 1.946875000341415030, 0.000000000000000000 ) ) ;
#201061 = CARTESIAN_POINT ( 'NONE',  ( 4.596835240751270035, 8.371391889155539445, -0.09823007671119071693 ) ) ;
#201062 = CARTESIAN_POINT ( 'NONE',  ( 1.500000000000001332, 9.125000000000001776, 0.000000000000000000 ) ) ;
#201063 = CARTESIAN_POINT ( 'NONE',  ( 3.668305164303451882, -1.157086425697685828, 1.279375231203205621 ) ) ;
#201064 = CARTESIAN_POINT ( 'NONE',  ( 6.319508997745523438, 9.426492026461511742, -1.082531754730548412 ) ) ;
#201065 = CARTESIAN_POINT ( 'NONE',  ( 2.371989033382770895, -1.092842237840240482, 1.391882982410238556 ) ) ;
#201066 = CARTESIAN_POINT ( 'NONE',  ( 2.912746486309669258, -0.5863433081114779455, -1.925794048158388394 ) ) ;
#201067 = EDGE_CURVE ( 'NONE', #139878, #213712, #113340, .T. ) ;
#201068 = CARTESIAN_POINT ( 'NONE',  ( 4.876106637443972325, 1.267215935518750669, 1.806476597341267087 ) ) ;
#201069 = ORIENTED_EDGE ( 'NONE', *, *, #185077, .F. ) ;
#201070 = CARTESIAN_POINT ( 'NONE',  ( 4.148698013468838930, 1.981613772426650266, 0.3898967627796907642 ) ) ;
#201071 = CARTESIAN_POINT ( 'NONE',  ( -5.773793314573309132, 7.829454515125894964, 1.599625672291263179 ) ) ;
#201072 = CARTESIAN_POINT ( 'NONE',  ( 4.183220377109976518, 1.621195451842275315, 1.198844725951081047 ) ) ;
#201074 = ORIENTED_EDGE ( 'NONE', *, *, #213533, .T. ) ;
#201073 = CARTESIAN_POINT ( 'NONE',  ( 4.412255891540381114, -1.811360455869342578, -0.03765339742955660374 ) ) ;
#201075 = CARTESIAN_POINT ( 'NONE',  ( 2.975316878787794828, 1.776827963633962559, -0.5852370025475408521 ) ) ;
#201076 = AXIS2_PLACEMENT_3D ( 'NONE', #130787, #179481, #180530 ) ;
#201077 = CARTESIAN_POINT ( 'NONE',  ( -1.284279953904132077, 2.909610286488902187, -0.7749999999999935829 ) ) ;
#201078 = CARTESIAN_POINT ( 'NONE',  ( 1.511816067030671729, -0.6413169068853613597, 1.801808535584384252 ) ) ;
#201079 = CARTESIAN_POINT ( 'NONE',  ( 0.000000000000000000, 0.08000000000000020983, 0.000000000000000000 ) ) ;
#201080 = CARTESIAN_POINT ( 'NONE',  ( -10.90756946389101323, 4.636105284860334130, -4.485523696119589232 ) ) ;
#201081 = CARTESIAN_POINT ( 'NONE',  ( 1.734723475976807094E-15, -7.105553651663779391, 3.150000000000000799 ) ) ;
#201082 = CARTESIAN_POINT ( 'NONE',  ( 1.364683531249988535, 2.676041667008082214, 0.7879004041258500513 ) ) ;
#201083 = CARTESIAN_POINT ( 'NONE',  ( -0.2049973002360427898, -0.1418364932926942379, -1.881151990943498387 ) ) ;
#201084 = CARTESIAN_POINT ( 'NONE',  ( 7.038091139269835317, 7.383730215335837954, 0.000000000000000000 ) ) ;
#201085 = CARTESIAN_POINT ( 'NONE',  ( 1.223018651738450480, -1.772137153356953432, -0.8420139538000551704 ) ) ;
#201086 = CARTESIAN_POINT ( 'NONE',  ( 0.1458495181914116201, -0.1430550213798176262, -1.983920851313693223 ) ) ;
#201087 = CARTESIAN_POINT ( 'NONE',  ( -6.611536185319534908, 7.742488966741438716, 1.199719254218452047 ) ) ;
#201088 = CARTESIAN_POINT ( 'NONE',  ( 5.203433420164765622, 1.869144303625443371, -1.001675624404389620 ) ) ;
#201090 = CARTESIAN_POINT ( 'NONE',  ( -10.57232049882948388, 5.599334429189661400, -4.968988939937085014 ) ) ;
#201089 = CARTESIAN_POINT ( 'NONE',  ( 8.211434591371064684, 12.73175745657494851, -0.7998128361456352531 ) ) ;
#201091 = CARTESIAN_POINT ( 'NONE',  ( 6.063742386902314152, 1.942598920255795392, -0.3345802184639041776 ) ) ;
#201092 = CARTESIAN_POINT ( 'NONE',  ( -1.364683531250014514, 1.738541667008085545, -0.7879004041258289570 ) ) ;
#201093 = CARTESIAN_POINT ( 'NONE',  ( 0.2990880961862537601, -0.2507095357664780866, -1.997497332983847906 ) ) ;
#201094 = VERTEX_POINT ( 'NONE', #175079 ) ;
#201095 = CARTESIAN_POINT ( 'NONE',  ( 1.652128961607162827, 1.091750937195800519, 1.813926670343589898 ) ) ;
#201096 = CARTESIAN_POINT ( 'NONE',  ( 11.96883372729383055, 6.669921767506581389, -0.9937123909951041112 ) ) ;
#201097 = CARTESIAN_POINT ( 'NONE',  ( 2.787621587699981696, -1.932700977737045633, 0.7428295258242522126 ) ) ;
#201098 = B_SPLINE_CURVE_WITH_KNOTS ( 'NONE', 3,
 ( #176722, #145334, #191883, #211335 ),
 .UNSPECIFIED., .F., .F.,
 ( 4, 4 ),
 ( 0.000000000000000000, 0.0003384805362160000402 ),
 .UNSPECIFIED. ) ;
#201099 = CARTESIAN_POINT ( 'NONE',  ( 5.551137550152489553, 5.441024994791534120, 0.7998128361456352531 ) ) ;
#201100 = CARTESIAN_POINT ( 'NONE',  ( 5.091969210384201361, 8.098325291160362482, 1.199719254218452047 ) ) ;
#201101 = ORIENTED_EDGE ( 'NONE', *, *, #110409, .F. ) ;
#201103 = CARTESIAN_POINT ( 'NONE',  ( 4.517891501851804215, 6.293959390292322986, -1.599625672291255185 ) ) ;
#201102 = CARTESIAN_POINT ( 'NONE',  ( 4.910148475136437263, 1.442109633637311372, -1.513870239069979196 ) ) ;
#201106 = ORIENTED_EDGE ( 'NONE', *, *, #75988, .T. ) ;
#201105 = CARTESIAN_POINT ( 'NONE',  ( 1.857782056280156580, 0.6927856907082428073, -1.673962145341382435 ) ) ;
#201104 = CARTESIAN_POINT ( 'NONE',  ( 3.469579810302122702, 1.781292651720441711, -0.3989491859636914994 ) ) ;
#201107 = CARTESIAN_POINT ( 'NONE',  ( 6.147136880733683917, -1.866598994669690148, 1.177069016086537356 ) ) ;
#201108 = CARTESIAN_POINT ( 'NONE',  ( 8.806171940766569506, 13.38206018750110360, -7.684638306840279043 ) ) ;
#201109 = MECHANICAL_DESIGN_GEOMETRIC_PRESENTATION_REPRESENTATION (  '', ( #48859 ), #159560 ) ;
#201110 = CARTESIAN_POINT ( 'NONE',  ( 5.491335294905154818, 1.948586811899848614, -1.035780281143129811 ) ) ;
#201111 = CARTESIAN_POINT ( 'NONE',  ( 1.364683531249997417, 9.546875000341396245, 2.602085213965210642E-15 ) ) ;
#201112 = ORIENTED_EDGE ( 'NONE', *, *, #30212, .F. ) ;
#201113 = CARTESIAN_POINT ( 'NONE',  ( 3.932203299393256302, -0.9856607118853939475, -1.638553295466014248 ) ) ;
#201114 = CARTESIAN_POINT ( 'NONE',  ( -4.029797971759847997, 5.724516938518342535, -1.599625672291256295 ) ) ;
#201115 = CARTESIAN_POINT ( 'NONE',  ( 8.067265095331215718, 9.370563018429956870, 1.199719254218462483 ) ) ;
#201116 = CARTESIAN_POINT ( 'NONE',  ( 6.848098043024292814, -0.8888149443028300345, 1.868052569137634400 ) ) ;
#201117 = CARTESIAN_POINT ( 'NONE',  ( -1.360316468749996899, 0.4010416670080598767, -0.7853790794158941324 ) ) ;
#201118 = CARTESIAN_POINT ( 'NONE',  ( 3.334942598837264960, 6.834590765378040444, 1.214306433183764966E-14 ) ) ;
#201119 = DIRECTION ( 'NONE',  ( 0.000000000000000000, 1.000000000000000000, 0.000000000000000000 ) ) ;
#201120 = CARTESIAN_POINT ( 'NONE',  ( -1.387358672534977355, 7.315968950353621381, -4.254625267138091971 ) ) ;
#201121 = CARTESIAN_POINT ( 'NONE',  ( -4.933501174700577302E-10, 15.51845925587262975, -12.00000000000000355 ) ) ;
#201122 = EDGE_LOOP ( 'NONE', ( #119301, #19705, #46167, #25319 ) ) ;
#201124 = EDGE_CURVE ( 'NONE', #94484, #89267, #102997, .T. ) ;
#201123 = AXIS2_PLACEMENT_3D ( 'NONE', #141752, #26878, #159026 ) ;
#201125 = CARTESIAN_POINT ( 'NONE',  ( -3.475000000000000533, -2.129166666666665542, -2.006292185433948827 ) ) ;
#201126 = CARTESIAN_POINT ( 'NONE',  ( 4.165207536865437099, 0.2314014899743311315, -1.856129391651973215 ) ) ;
#201127 = CARTESIAN_POINT ( 'NONE',  ( 6.318982112420993502, 9.529840343536603697, -1.199719254218452047 ) ) ;
#201128 = CARTESIAN_POINT ( 'NONE',  ( -0.7500000000000179856, 12.57291666734946389, 1.299038105676658228 ) ) ;
#201129 = CARTESIAN_POINT ( 'NONE',  ( -7.388830529767770550, 7.722649827591604677, 1.040834085586084257E-14 ) ) ;
#201130 = CARTESIAN_POINT ( 'NONE',  ( 4.329849954717849947, 6.144853928627882489, 1.599625672291262513 ) ) ;
#201131 = CARTESIAN_POINT ( 'NONE',  ( 5.473741331615251227, 7.409117525016355010, -1.599625672291262513 ) ) ;
#201132 = CARTESIAN_POINT ( 'NONE',  ( 6.702015291077846548, 0.7979701500827086624, -1.910492173269620508 ) ) ;
#201133 = CARTESIAN_POINT ( 'NONE',  ( 1.071888921174158016, -0.9040910708146729924, 1.802427947461216373 ) ) ;
#201134 = CARTESIAN_POINT ( 'NONE',  ( -9.158696461231359720, 10.64389961198009615, 1.199719254218462483 ) ) ;
#201135 = CARTESIAN_POINT ( 'NONE',  ( 7.340813827156391191, 7.528980651296110160, 0.7998128361456281477 ) ) ;
#201136 = DIRECTION ( 'NONE',  ( 2.949029909160572061E-17, 1.000000000000000000, -8.673600428462616880E-15 ) ) ;
#201137 = CARTESIAN_POINT ( 'NONE',  ( 1.429895766826321690, 1.077743243251317429, -1.908043295719801025 ) ) ;
#201138 = CARTESIAN_POINT ( 'NONE',  ( 6.463509179248936753, 0.3066564278407272193, -1.799597105106438777 ) ) ;
#201139 = CARTESIAN_POINT ( 'NONE',  ( -2.948008335967658322, 5.526761261015804116, 1.199719254218462483 ) ) ;
#201140 = CARTESIAN_POINT ( 'NONE',  ( 5.397554552016228691, 5.469770863539975991, 0.7216878364870328300 ) ) ;
#201141 = CARTESIAN_POINT ( 'NONE',  ( 10.24726517383036928, 10.84956421242393887, 0.000000000000000000 ) ) ;
#201142 = EDGE_CURVE ( 'NONE', #206605, #180652, #22778, .T. ) ;
#201143 = CARTESIAN_POINT ( 'NONE',  ( 3.999819011231439347, 4.625209253646830554, 1.199719254218464037 ) ) ;
#201144 = CARTESIAN_POINT ( 'NONE',  ( 7.702440666339465558, 8.158804663583751449, -0.7216878364870317197 ) ) ;
#201145 = VERTEX_POINT ( 'NONE', #123209 ) ;
#201147 = CARTESIAN_POINT ( 'NONE',  ( 0.8385398129025347647, 1.197303422201956957, -1.618206657969661011 ) ) ;
#201146 = CARTESIAN_POINT ( 'NONE',  ( 3.948646536499214932, -1.533023199436277961, -1.019512891124202403 ) ) ;
#201148 = CARTESIAN_POINT ( 'NONE',  ( 2.548584303619909175, 2.101849941811538169, -0.9302779420137051725 ) ) ;
#201150 = CARTESIAN_POINT ( 'NONE',  ( 1.287708147089029032, -1.175244795098003614, -1.442924398407473108 ) ) ;
#201149 = CARTESIAN_POINT ( 'NONE',  ( 3.931501358282940117, 4.649468341827285300, -1.082531754730543083 ) ) ;
#201151 = CARTESIAN_POINT ( 'NONE',  ( 1.001543065824772753E-15, -3.171874999522042327, 3.793834371823811669 ) ) ;
#201152 = CARTESIAN_POINT ( 'NONE',  ( -3.903858165731105778, 6.641919395739846799, 1.199719254218464037 ) ) ;
#201153 = CARTESIAN_POINT ( 'NONE',  ( 4.271672842113056312, 0.4137096367802223784, -1.866957553337177611 ) ) ;
#201154 = CARTESIAN_POINT ( 'NONE',  ( -9.541187415715041809, 12.15447128979948310, -1.599625672291263179 ) ) ;
#201155 = CARTESIAN_POINT ( 'NONE',  ( 6.491225937077876651, 6.748298437306541331, 0.07656069123261090292 ) ) ;
#201156 = CARTESIAN_POINT ( 'NONE',  ( -6.129694847154211423, 9.205042184104968328, -1.082531754730549967 ) ) ;
#201158 = CARTESIAN_POINT ( 'NONE',  ( 1.762360912074714125, -1.325010844092512796, 1.320751239342173200 ) ) ;
#201157 = CARTESIAN_POINT ( 'NONE',  ( 3.298458272841266137, 1.646618950329106434, -1.288217307904614639 ) ) ;
#201159 = CARTESIAN_POINT ( 'NONE',  ( 8.785320351975350661, 9.351887953500479966, -0.7216878364870197293 ) ) ;
#201160 = CARTESIAN_POINT ( 'NONE',  ( 1.364683531249988535, 5.217708333674750065, -0.7879004041258300672 ) ) ;
#201161 = CARTESIAN_POINT ( 'NONE',  ( 3.720004753662985664, 1.653986544816415494, 0.5419736716202552262 ) ) ;
#201162 = CARTESIAN_POINT ( 'NONE',  ( 3.649115900372475796, 7.409052317076538330, 1.040834085586084257E-14 ) ) ;
#201164 = CARTESIAN_POINT ( 'NONE',  ( 5.029711800545521250, 5.930713857800314237, -1.082531754730549078 ) ) ;
#201163 = CARTESIAN_POINT ( 'NONE',  ( 1.500000000000053291, 7.750000000000000000, 15.74999999999999289 ) ) ;
#201165 = CARTESIAN_POINT ( 'NONE',  ( 4.301177763854931335, 1.387281528384849860, 1.024788870506128990 ) ) ;
#201166 = CARTESIAN_POINT ( 'NONE',  ( -6.256197817702116026, 9.386315656372753224, -1.199719254218440723 ) ) ;
#201167 = CARTESIAN_POINT ( 'NONE',  ( 3.913774547416096095, -1.127657808996849198, -1.879056921112078893 ) ) ;
#201168 = CARTESIAN_POINT ( 'NONE',  ( 6.358075476802443227, 2.201304964888863402, -0.1578768562689457922 ) ) ;
#201169 = AXIS2_PLACEMENT_3D ( 'NONE', #43328, #9729, #111572 ) ;
#201171 = CARTESIAN_POINT ( 'NONE',  ( 3.555704413576792788, 1.708454066091537493, 1.339533783212579099 ) ) ;
#201170 = B_SPLINE_CURVE_WITH_KNOTS ( 'NONE', 3,
 ( #42953, #73269, #109062, #122129, #39724, #141539 ),
 .UNSPECIFIED., .F., .F.,
 ( 4, 2, 4 ),
 ( 0.000000000000000000, 0.002403937268455931617, 0.004807874536911863235 ),
 .UNSPECIFIED. ) ;
#201172 = CARTESIAN_POINT ( 'NONE',  ( 2.560947663861262491, -1.588335953301520220, -0.9000364273514869229 ) ) ;
#201173 = CARTESIAN_POINT ( 'NONE',  ( -1.500000000000001110, 9.302083334016128191, 0.8660254037844418162 ) ) ;
#201174 = CARTESIAN_POINT ( 'NONE',  ( 4.399685268140280492, -2.075804279169701339, 0.4165508703993703876 ) ) ;
#201175 = CIRCLE ( 'NONE', #107893, 0.08000000000000014044 ) ;
#201176 = VERTEX_POINT ( 'NONE', #74364 ) ;
#201178 = CARTESIAN_POINT ( 'NONE',  ( -1.402160292154681736E-14, 2.509375000341417028, -1.575800808251660134 ) ) ;
#201177 = CARTESIAN_POINT ( 'NONE',  ( 4.370831947049586219, 0.0005328150827835219676, -2.292545470631628390 ) ) ;
#201179 = CARTESIAN_POINT ( 'NONE',  ( 6.720655732516679137, 4.703287744343486843, 2.289001594030832365 ) ) ;
#201180 = CARTESIAN_POINT ( 'NONE',  ( 10.70146331988817323, 11.37946204949139251, 0.7998128361456341429 ) ) ;
#201181 = CARTESIAN_POINT ( 'NONE',  ( 0.9793288802587530872, -1.918618388578940737, -0.9032494106611321794 ) ) ;
#201182 = CARTESIAN_POINT ( 'NONE',  ( -4.609409038966245653, 6.400729850259146758, -1.443375672974053447 ) ) ;
#201183 = CARTESIAN_POINT ( 'NONE',  ( 2.846849069189655967, 5.304779099821139710, -1.082531754730543083 ) ) ;
#201184 = CARTESIAN_POINT ( 'NONE',  ( -6.358410854684796831, 6.520493539994793863, -0.7216878364870267237 ) ) ;
#201186 = CARTESIAN_POINT ( 'NONE',  ( -1.500000000000008216, 12.78125000068279427, 3.469446951953614189E-15 ) ) ;
#201185 = CARTESIAN_POINT ( 'NONE',  ( -10.99861993420630135, -9.955063214563455887, 0.1919715503786826039 ) ) ;
#201187 = ORIENTED_EDGE ( 'NONE', *, *, #76187, .F. ) ;
#201188 = CARTESIAN_POINT ( 'NONE',  ( 5.871720251644387822, -0.2986239867289949834, -1.994071864161291119 ) ) ;
#201190 = CARTESIAN_POINT ( 'NONE',  ( 4.627816428071820809, 2.001945081875619259, -0.4960309448565465851 ) ) ;
#201189 = CARTESIAN_POINT ( 'NONE',  ( 2.998324526916512411, 6.649795714711241423, 0.000000000000000000 ) ) ;
#201192 = CARTESIAN_POINT ( 'NONE',  ( 9.578206935422253210, -9.900000000000005684, -0.1671882239536598425 ) ) ;
#201191 = CARTESIAN_POINT ( 'NONE',  ( 6.424584688029230328, 8.588711117491191871, 1.599625672291268286 ) ) ;
#201193 = CARTESIAN_POINT ( 'NONE',  ( 5.501576472095266901, 9.640532660744973725, -0.7998128361456481317 ) ) ;
#201194 = CARTESIAN_POINT ( 'NONE',  ( 3.285556943750000070, -0.6343749995220415716, 0.000000000000000000 ) ) ;
#201195 = CARTESIAN_POINT ( 'NONE',  ( 0.1331565106231571705, 6.948071080078889850, -2.540993614958915181 ) ) ;
#201196 = CARTESIAN_POINT ( 'NONE',  ( 0.3223637989299525941, 2.001183132641819906, 0.6049928108779398794 ) ) ;
#201197 = CARTESIAN_POINT ( 'NONE',  ( 4.904922738988922504, -1.081064280317966420, -1.701948707654332704 ) ) ;
#201198 = CARTESIAN_POINT ( 'NONE',  ( 4.229911503591711863, 1.806553461410321582, 0.3548724298726435022 ) ) ;
#201199 = EDGE_CURVE ( 'NONE', #183422, #192481, #190826, .T. ) ;
#201200 = CARTESIAN_POINT ( 'NONE',  ( 6.505214776458575265, 6.483838748823460563, 1.040834085586084257E-14 ) ) ;
#201201 = CARTESIAN_POINT ( 'NONE',  ( 1.271983708484729636, -1.098657341177114999, 1.329575768613028286 ) ) ;
#201202 = CARTESIAN_POINT ( 'NONE',  ( 0.3215004009857677092, -1.429452135790244549, -1.422604240635255479 ) ) ;
#201203 =( BOUNDED_CURVE ( )  B_SPLINE_CURVE ( 2, ( #65320, #184416, #199593, #67444, #197470, #163933, #3513, #198523, #1383 ),
 .UNSPECIFIED., .F., .T. ) 
 B_SPLINE_CURVE_WITH_KNOTS ( ( 3, 2, 2, 2, 3 ),
 ( 0.2343749999999997780, 0.2395833333333333426, 0.2500000000000000000, 0.2604166666666666852, 0.2656250000000002220 ),
 .UNSPECIFIED. ) 
 CURVE ( )  GEOMETRIC_REPRESENTATION_ITEM ( )  RATIONAL_B_SPLINE_CURVE ( ( 0.9330127018922194093, 0.9330127018922165227, 1.000000000000000000, 0.8660254037844387076, 1.000000000000000000, 0.8660254037844387076, 1.000000000000000000, 0.9330127018922165227, 0.9330127018922194093 ) ) 
 REPRESENTATION_ITEM ( '' )  );
#201204 = CARTESIAN_POINT ( 'NONE',  ( 1.337049673779285852, 0.6609975811289883207, -2.201632501652720286 ) ) ;
#201205 = CARTESIAN_POINT ( 'NONE',  ( -4.889686956022917919, 8.856385215335397021, 1.214306433183764966E-14 ) ) ;
#201206 = CARTESIAN_POINT ( 'NONE',  ( 1.564152511173346749, 2.229009205740081434, -0.3863987453041685116 ) ) ;
#201207 = CARTESIAN_POINT ( 'NONE',  ( 3.106188079018203041, -2.103647721026543405, 0.1036251941764678303 ) ) ;
#201208 = CARTESIAN_POINT ( 'NONE',  ( -6.283277845290492714, 6.295188672452495915, -0.7998128361456362523 ) ) ;
#201209 = APPLICATION_CONTEXT ( 'automotive_design' ) ;
#201210 = CARTESIAN_POINT ( 'NONE',  ( 6.238723240582662477, 10.43026088065513513, -0.7998128361456291469 ) ) ;
#201211 = CARTESIAN_POINT ( 'NONE',  ( 7.322812364712459221, 7.715904978352238430, 0.000000000000000000 ) ) ;
#201212 = SURFACE_SIDE_STYLE ('',( #153563 ) ) ;
#201213 = CARTESIAN_POINT ( 'NONE',  ( -4.737684612971557740, 7.614716917520386374, 1.199719254218464037 ) ) ;
#201214 = CARTESIAN_POINT ( 'NONE',  ( 7.104109303436412226, 7.390475063538369582, 1.040834085586084257E-14 ) ) ;
#201215 = CARTESIAN_POINT ( 'NONE',  ( 5.396677706949416731, 6.496517479030419651, 1.312881173378084521 ) ) ;
#201216 = CARTESIAN_POINT ( 'NONE',  ( -2.611917148927046295, 6.198987107056845858, 1.040834085586084257E-14 ) ) ;
#201217 = CARTESIAN_POINT ( 'NONE',  ( 4.922253396635227318, -2.210645704158546554, 0.2187456033138199529 ) ) ;
#201218 = CARTESIAN_POINT ( 'NONE',  ( 2.203317661949526052, -0.4785072280911427667, 2.138412878249687399 ) ) ;
#201219 = CARTESIAN_POINT ( 'NONE',  ( -6.247609857798938293, 6.183299677053865295, -0.7998128361456291469 ) ) ;
#201220 = CARTESIAN_POINT ( 'NONE',  ( -4.146814880933400005, 5.931313009212638931, 1.599625672291270506 ) ) ;
#201221 = CARTESIAN_POINT ( 'NONE',  ( 5.494571831323358246, 1.932540981948445147, 0.3370517209014682325 ) ) ;
#201222 = CARTESIAN_POINT ( 'NONE',  ( -0.6823417656250212460, 1.551041667008083769, 1.181850606188755259 ) ) ;
#201223 = DIRECTION ( 'NONE',  ( -1.000000000000000000, 0.000000000000000000, 0.000000000000000000 ) ) ;
#201224 = CARTESIAN_POINT ( 'NONE',  ( -4.690757960648240577, 6.495636925554817864, 1.443375672974064550 ) ) ;
#201225 = CARTESIAN_POINT ( 'NONE',  ( 4.271814301144261528, 0.4616217191124799002, -2.069597271375968273 ) ) ;
#201226 = CARTESIAN_POINT ( 'NONE',  ( -7.105881907338178038, 7.462819444748888920, -0.7216878364870338292 ) ) ;
#201227 = ORIENTED_EDGE ( 'NONE', *, *, #191412, .F. ) ;
#201229 = CARTESIAN_POINT ( 'NONE',  ( 6.491117449447131982, 1.883434485765375310, -1.060826435891427666 ) ) ;
#201228 = CARTESIAN_POINT ( 'NONE',  ( -6.807602527837528505, 7.114826835331461652, 0.7216878364870317197 ) ) ;
#201230 = CARTESIAN_POINT ( 'NONE',  ( 6.979750152936881058, 7.037463354714830643, 0.7998128361456341429 ) ) ;
#201231 = CARTESIAN_POINT ( 'NONE',  ( 5.442854017605395889, -1.455216020186438364, -1.127989967910733693 ) ) ;
#201232 = CARTESIAN_POINT ( 'NONE',  ( 1.364683531249986537, 2.467708333674753174, -0.7879004041258239610 ) ) ;
#201233 = CARTESIAN_POINT ( 'NONE',  ( 1.557743604271996762, -1.230989698698783608, 1.230628217043183925 ) ) ;
#201234 = CARTESIAN_POINT ( 'NONE',  ( -0.4019237886466802689, 11.22991455036742714, -1.500000000000002887 ) ) ;
#201235 = CARTESIAN_POINT ( 'NONE',  ( -1.364683531250014514, -0.9072916663252470482, 0.7879004041258379498 ) ) ;
#201236 = CARTESIAN_POINT ( 'NONE',  ( 9.998716872439858960, 9.834509080145350524, -6.644787476054019315 ) ) ;
#201237 = CARTESIAN_POINT ( 'NONE',  ( 5.295850518597075229, -0.7817450549502875656, 2.015575934489414411 ) ) ;
#201238 = CARTESIAN_POINT ( 'NONE',  ( -4.308793891044708779, 3.921347715840572956, 1.214306433183764966E-14 ) ) ;
#201239 = AXIS2_PLACEMENT_3D ( 'NONE', #25464, #204183, #21171 ) ;
#201240 = CARTESIAN_POINT ( 'NONE',  ( -8.148087131688699358, 8.608449196499371681, -0.7216878364870267237 ) ) ;
#201241 = CARTESIAN_POINT ( 'NONE',  ( 4.909125497034264818, 1.879091090907711425, 1.068517025386829467 ) ) ;
#201242 = CARTESIAN_POINT ( 'NONE',  ( 0.6823417656249899377, 3.176041667008085323, -1.181850606188754593 ) ) ;
#201243 = CARTESIAN_POINT ( 'NONE',  ( 5.219980872528355853, -1.052265754357907701, -1.666845346888909729 ) ) ;
#201244 = CARTESIAN_POINT ( 'NONE',  ( 3.549848462767680068, 1.568450346167485243, -0.7392937452721718428 ) ) ;
#201245 = CARTESIAN_POINT ( 'NONE',  ( 1.031118135130421498, -1.979082047791239418, 0.9416876394413642437 ) ) ;
#201246 = CARTESIAN_POINT ( 'NONE',  ( 2.626355190031507192, -1.328241637659173247, -1.886819894403545028 ) ) ;
#201247 = CARTESIAN_POINT ( 'NONE',  ( 4.393860645892766037, -0.7923225987812362314, 1.902584447174461291 ) ) ;
#201248 = CARTESIAN_POINT ( 'NONE',  ( 6.304245038521663957, 1.436082020041820506, -1.307557180447990186 ) ) ;
#201250 = EDGE_CURVE ( 'NONE', #30537, #172216, #100299, .T. ) ;
#201249 = CARTESIAN_POINT ( 'NONE',  ( -5.531363484251157203, 9.397081798360927607, 0.000000000000000000 ) ) ;
#201251 = CARTESIAN_POINT ( 'NONE',  ( -4.956387674247580755, 7.940146832334256111, 1.199719254218452935 ) ) ;
#201252 = FACE_OUTER_BOUND ( 'NONE', #105828, .T. ) ;
#201253 = CARTESIAN_POINT ( 'NONE',  ( 0.9498425221252141393, -1.824119990893595888, -0.8596288560165299408 ) ) ;
#201254 = CARTESIAN_POINT ( 'NONE',  ( -5.531363484251157203, 9.397081798360927607, 0.000000000000000000 ) ) ;
#201255 = CARTESIAN_POINT ( 'NONE',  ( 3.223846859376262142, -2.127229092858519799, 0.5869343725257711863 ) ) ;
#201256 = CARTESIAN_POINT ( 'NONE',  ( 1.001543065824772753E-15, -1.859374999522040550, 3.793834371823811669 ) ) ;
#201257 = CARTESIAN_POINT ( 'NONE',  ( 6.948121807170864805, -0.8414398651286276731, 1.770450887113049099 ) ) ;
#201258 = CARTESIAN_POINT ( 'NONE',  ( 1.500085555261172932, 3.249813679204478056, -0.08157497973214339337 ) ) ;
#201259 = CARTESIAN_POINT ( 'NONE',  ( -0.7499999999999972244, 4.889583334016150751, -1.299038105676652899 ) ) ;
#201260 = DIRECTION ( 'NONE',  ( 0.000000000000000000, -1.000000000000000000, 0.000000000000000000 ) ) ;
#201262 = CARTESIAN_POINT ( 'NONE',  ( 6.825078400183551608, 1.261667030487168439, 2.159888225955305163 ) ) ;
#201261 = CARTESIAN_POINT ( 'NONE',  ( -4.882431421883429046, 8.154724402237897962, -1.012048471081774093 ) ) ;
#201263 = CARTESIAN_POINT ( 'NONE',  ( 6.052668933152094866, -1.581501214056714177, -0.9424504099920794076 ) ) ;
#201264 = EDGE_LOOP ( 'NONE', ( #189807, #143100, #46936, #164780 ) ) ;
#201265 = CARTESIAN_POINT ( 'NONE',  ( 3.151298293300933029, -1.683901109147158737, -1.187873040408020886 ) ) ;
#201266 = CARTESIAN_POINT ( 'NONE',  ( -0.6801582343750368631, 1.682291667008048552, 1.178068619123803451 ) ) ;
#201267 = ADVANCED_FACE ( 'NONE', ( #194502 ), #183886, .T. ) ;
#201268 = CARTESIAN_POINT ( 'NONE',  ( -7.217017841176048165, 7.314275657660511243, 1.040834085586084257E-14 ) ) ;
#201269 = CARTESIAN_POINT ( 'NONE',  ( 1.787766293494430725, 1.931992495155916867, -0.5885693585916639270 ) ) ;
#201270 = CARTESIAN_POINT ( 'NONE',  ( 1.499999999999987566, 0.02500000000001806333, 0.000000000000000000 ) ) ;
#201271 = CARTESIAN_POINT ( 'NONE',  ( 2.659370686574860976, 6.254349567645977714, -0.7998128361456291469 ) ) ;
#201272 = CARTESIAN_POINT ( 'NONE',  ( 2.096624111547572777, -0.5486670241920866831, -1.986447216630163659 ) ) ;
#201274 = CARTESIAN_POINT ( 'NONE',  ( -1.402160292154681736E-14, 13.17187500034139980, 1.575800808251682339 ) ) ;
#201273 = CARTESIAN_POINT ( 'NONE',  ( 3.147653791585713901, 8.920000000000001705, -2.500000000000002220 ) ) ;
#201275 = CARTESIAN_POINT ( 'NONE',  ( 5.309989718046547402, 9.346738437696316737, 0.7998128361456462443 ) ) ;
#201276 = B_SPLINE_CURVE_WITH_KNOTS ( 'NONE', 3,
 ( #190925, #137939, #157393, #23081, #39358, #206113, #154183, #153110 ),
 .UNSPECIFIED., .F., .F.,
 ( 4, 2, 2, 4 ),
 ( 0.000000000000000000, 0.002997375907120270865, 0.004496063860680406081, 0.005994751814240539996 ),
 .UNSPECIFIED. ) ;
#201277 =( LENGTH_UNIT ( ) NAMED_UNIT ( * ) SI_UNIT ( .MILLI., .METRE. ) );
#201278 = CARTESIAN_POINT ( 'NONE',  ( 5.197975494389605267, -0.7968864405506062010, 2.058166701804148957 ) ) ;
#201279 = CARTESIAN_POINT ( 'NONE',  ( 1.247603677004164746, -1.703183937513498281, -1.330886036463780009 ) ) ;
#201280 = CARTESIAN_POINT ( 'NONE',  ( -4.609409038966245653, 6.400729850259146758, -1.443375672974053447 ) ) ;
#201281 = CARTESIAN_POINT ( 'NONE',  ( 0.4621254960020632074, -1.116205757145168231, 1.679226196708947239 ) ) ;
#201282 = PLANE ( 'NONE',  #204948 ) ;
#201283 = FACE_OUTER_BOUND ( 'NONE', #111020, .T. ) ;
#201284 = CARTESIAN_POINT ( 'NONE',  ( 1.849150832860071647, 8.949220158640459388, -0.7749999999999996891 ) ) ;
#201285 = EDGE_CURVE ( 'NONE', #39789, #60352, #147863, .T. ) ;
#201286 = CARTESIAN_POINT ( 'NONE',  ( 1.656895194024514906, -1.602792776363659133, -0.9643473572949823325 ) ) ;
#201287 = CARTESIAN_POINT ( 'NONE',  ( 4.048064755690682581, 0.9548552675892291175, 1.776167154503265566 ) ) ;
#201289 = CARTESIAN_POINT ( 'NONE',  ( 11.45846087878786790, 13.59311600781417972, 3.566076377698205846 ) ) ;
#201288 = CARTESIAN_POINT ( 'NONE',  ( 1.364683531249988535, 2.613541667008089764, 0.7879004041258500513 ) ) ;
#201291 = CARTESIAN_POINT ( 'NONE',  ( 5.004563900840214963, -0.7087877200973876635, -1.983347251131000855 ) ) ;
#201290 = CARTESIAN_POINT ( 'NONE',  ( -8.552495972122143186, 8.872333477097637200, 0.7998128361456462443 ) ) ;
#201292 = CARTESIAN_POINT ( 'NONE',  ( 7.579171565239241737, 8.801120566655981747, 1.199719254218462483 ) ) ;
#201293 = CARTESIAN_POINT ( 'NONE',  ( -7.365103760721662951, 9.615707025640515937, 1.599625672291295375 ) ) ;
#201294 = CARTESIAN_POINT ( 'NONE',  ( 1.432836755002401904E-15, 0.9999999999999978906, -11.69999999999999041 ) ) ;
#201295 = CARTESIAN_POINT ( 'NONE',  ( 5.291273337336410698, -0.05367003302336400411, -2.019259759236047280 ) ) ;
#201296 = CARTESIAN_POINT ( 'NONE',  ( 1.499999999999987121, -0.9645833326505173222, 0.8660254037844524744 ) ) ;
#201297 = CARTESIAN_POINT ( 'NONE',  ( 1.200133799977639137, 0.8395725688425963451, -1.884152621438263342 ) ) ;
#201298 = CARTESIAN_POINT ( 'NONE',  ( 9.273413882067330860, 9.921330405274451536, -0.7216878364870257245 ) ) ;
#201299 = CARTESIAN_POINT ( 'NONE',  ( 5.342795052237045539, 8.390955439988655229, -1.199719254218450271 ) ) ;
#201300 = CARTESIAN_POINT ( 'NONE',  ( 5.224688093219824303, 7.188831756880171397, -1.599625672291283607 ) ) ;
#201301 = CARTESIAN_POINT ( 'NONE',  ( -1.364683531250012516, 1.092708333674754506, 0.7879004041258379498 ) ) ;
#201303 = CARTESIAN_POINT ( 'NONE',  ( 8.794101853178714734, 3.696394713403113652, 7.873312689837477230 ) ) ;
#201302 = CARTESIAN_POINT ( 'NONE',  ( 4.529305835417093640, 7.441884687032027657, -1.199719254218450271 ) ) ;
#201304 = CARTESIAN_POINT ( 'NONE',  ( 7.795575137733369075, 9.157554417852841411, -1.082531754730537976 ) ) ;
#201306 = CARTESIAN_POINT ( 'NONE',  ( 11.44789321844504215, 12.29999999999998295, 3.303298730975393838 ) ) ;
#201305 = CARTESIAN_POINT ( 'NONE',  ( 3.297511149327167601, -1.916070068265750992, 1.021083071776592410 ) ) ;
#201308 = CARTESIAN_POINT ( 'NONE',  ( 1.768857366986800184, 1.761637791510446860, -0.5354853023365884201 ) ) ;
#201307 = CARTESIAN_POINT ( 'NONE',  ( -3.470524135418294520, 6.992769224722559684, -0.7216878364870267237 ) ) ;
#201309 = CARTESIAN_POINT ( 'NONE',  ( 1.364683531249988535, 3.363541667008084879, 0.7879004041258500513 ) ) ;
#201310 = CARTESIAN_POINT ( 'NONE',  ( 4.810206850810132551, 1.511280187219691928, -1.587364365194674498 ) ) ;
#201311 = CARTESIAN_POINT ( 'NONE',  ( -15.75000000000000000, 13.79999999999999893, -1.800000000000001155 ) ) ;
#201312 = CARTESIAN_POINT ( 'NONE',  ( 4.592800228568824750, -0.4914316458759260264, -2.208360408168393629 ) ) ;
#201313 = CARTESIAN_POINT ( 'NONE',  ( -5.717788096661253761, 7.693838750903348789, 1.599625672291269396 ) ) ;
#201314 = CARTESIAN_POINT ( 'NONE',  ( -1.448815997565459757, 7.903552007303734861, -10.65195286442483358 ) ) ;
#201315 = CARTESIAN_POINT ( 'NONE',  ( 5.528015674651411970, 7.440572265265038787, -1.248273786418591103 ) ) ;
#201316 = CARTESIAN_POINT ( 'NONE',  ( -1.500000000000001110, 14.02083333333333037, 0.8660254037844419273 ) ) ;
#201317 = CARTESIAN_POINT ( 'NONE',  ( -5.438229012412899799, 7.437962829272074750, -1.443375672974066548 ) ) ;
#201318 = CARTESIAN_POINT ( 'NONE',  ( 3.933273961740286317, 7.602920365423422311, 0.7216878364870257245 ) ) ;
#201319 = CARTESIAN_POINT ( 'NONE',  ( 5.553870903591159092, 1.767663364219349553, -0.08767779694792036949 ) ) ;
#201320 = AXIS2_PLACEMENT_3D ( 'NONE', #107275, #90981, #121411 ) ;
#201321 = CARTESIAN_POINT ( 'NONE',  ( 7.741869408603235136, 8.990934717247309749, 1.199719254218462483 ) ) ;
#201322 = CARTESIAN_POINT ( 'NONE',  ( 2.204260208318520764, -2.105514897310766020, 0.05069945311739902649 ) ) ;
#201323 = CIRCLE ( 'NONE', #52616, 1.000000000000000000 ) ;
#201325 = CARTESIAN_POINT ( 'NONE',  ( -0.7500000000000215383, 1.941666666666688634, 1.299038105676659116 ) ) ;
#201324 = CARTESIAN_POINT ( 'NONE',  ( -0.6823417656250039265, 11.81770833367473017, -1.181850606188755259 ) ) ;
#201326 = CARTESIAN_POINT ( 'NONE',  ( 1.644903635585378554, -0.2856866470503526823, -1.948579891484893079 ) ) ;
#201327 = CARTESIAN_POINT ( 'NONE',  ( 0.4439547499465161251, 1.865322535695708606, 0.1421067652795371117 ) ) ;
#201328 = CARTESIAN_POINT ( 'NONE',  ( 1.170277241841523264, -0.8789641444944886750, -1.754005360843587047 ) ) ;
#201330 = VERTEX_POINT ( 'NONE', #183574 ) ;
#201329 = CARTESIAN_POINT ( 'NONE',  ( 6.187769672300552415, 1.730736780639136496, -0.5351268960485565662 ) ) ;
#201331 = CARTESIAN_POINT ( 'NONE',  ( 6.155038550924144758, 8.203964280876741455, 1.443375672974076540 ) ) ;
#201332 = CARTESIAN_POINT ( 'NONE',  ( 1.364683531249986981, -1.053124999658580752, 0.000000000000000000 ) ) ;
#201333 = CARTESIAN_POINT ( 'NONE',  ( 5.858239598252557023, 0.7595784280203802252, 1.709674162104061423 ) ) ;
#201334 = FACE_OUTER_BOUND ( 'NONE', #111242, .T. ) ;
#201335 = ORIENTED_EDGE ( 'NONE', *, *, #167354, .F. ) ;
#201336 = CARTESIAN_POINT ( 'NONE',  ( 5.524307029080701703, 1.015476208609331188, 1.803995072556117352 ) ) ;
#201337 = CARTESIAN_POINT ( 'NONE',  ( -1.225000000000018074, 2.979166666666678065, -0.7072540797572998139 ) ) ;
#201338 = CARTESIAN_POINT ( 'NONE',  ( -5.519577934094894722, 7.532869904567736974, 1.443375672974058777 ) ) ;
#201339 = CARTESIAN_POINT ( 'NONE',  ( 0.2915762745691782287, -1.893489616766583339, 0.8377075429084477332 ) ) ;
#201340 = CARTESIAN_POINT ( 'NONE',  ( -1.402160292154681736E-14, -0.03749999999998095135, 1.732050807568877637 ) ) ;
#201341 = CARTESIAN_POINT ( 'NONE',  ( 8.426556166093362776, 9.789735934319136135, -1.199719254218446718 ) ) ;
#201342 = CARTESIAN_POINT ( 'NONE',  ( -8.962103233833181193, 10.41454084668224489, -1.199719254218446718 ) ) ;
#201343 = CARTESIAN_POINT ( 'NONE',  ( 5.234329823327693809, 8.264412672927770487, 1.199719254218451159 ) ) ;
#201344 = CARTESIAN_POINT ( 'NONE',  ( 1.364683531249986537, -0.09479166632524321789, -0.7879004041258309554 ) ) ;
#201345 = CARTESIAN_POINT ( 'NONE',  ( 1.499999999999989120, 0.7750000000000187850, 0.000000000000000000 ) ) ;
#201347 = CARTESIAN_POINT ( 'NONE',  ( 4.334856428067313416, 6.080418470877079429, -1.599625672291256295 ) ) ;
#201346 = CARTESIAN_POINT ( 'NONE',  ( 5.283633159863808437, -1.863482887291990409, 0.6137318589548645953 ) ) ;
#201348 = CARTESIAN_POINT ( 'NONE',  ( 3.040388574052850235, 1.915307028720541371, -0.6297779509270851062 ) ) ;
#201349 = CARTESIAN_POINT ( 'NONE',  ( 2.501083532561697798, -0.1830384092258540707, 1.906917772027187929 ) ) ;
#201350 = CARTESIAN_POINT ( 'NONE',  ( 11.86239285000045918, 9.719999999999998863, -1.812080536912753059 ) ) ;
#201351 = CARTESIAN_POINT ( 'NONE',  ( 0.3104468679729632807, 1.506874830639578056, -1.591553791636945991 ) ) ;
#201352 = CARTESIAN_POINT ( 'NONE',  ( 0.2333690889706820926, 2.873202992247088083, -2.541887414127189881 ) ) ;
#201353 = CARTESIAN_POINT ( 'NONE',  ( 2.706148147531197701, -0.7121320899835179574, -1.729884524348634933 ) ) ;
#201354 = CARTESIAN_POINT ( 'NONE',  ( -0.7500000000000249800, -0.2770833326505156569, 1.299038105676659116 ) ) ;
#201355 = CARTESIAN_POINT ( 'NONE',  ( 4.535406599088565471, -0.09463749723611977749, 2.011077795214308406 ) ) ;
#201356 = CARTESIAN_POINT ( 'NONE',  ( -6.672584156219988571, 10.93643194889866521, -0.7998128361456291469 ) ) ;
#201358 = CARTESIAN_POINT ( 'NONE',  ( 4.903976463145187203, -1.133744943205544642, -1.787932202283550875 ) ) ;
#201357 = CARTESIAN_POINT ( 'NONE',  ( -4.094199201646926412, 7.720390135322642067, 0.7216878364870317197 ) ) ;
#201359 = CARTESIAN_POINT ( 'NONE',  ( -0.07933194154488883154, -9.900000000000005684, -9.499668754385620417 ) ) ;
#201360 = CARTESIAN_POINT ( 'NONE',  ( 6.232888004217203459, -1.964670499678453197, -0.6532144590316590893 ) ) ;
#201362 = CARTESIAN_POINT ( 'NONE',  ( 6.720655732516655156, 7.629137130509086262, 2.873739711112702544 ) ) ;
#201361 = CARTESIAN_POINT ( 'NONE',  ( 1.610996488345920907, -0.2524672473064055733, 2.075362222853482930 ) ) ;
#201364 = ORIENTED_EDGE ( 'NONE', *, *, #19121, .T. ) ;
#201363 = CARTESIAN_POINT ( 'NONE',  ( 6.563509198815889789, 0.3086105522638156184, -1.799150958419073909 ) ) ;
#201365 = CARTESIAN_POINT ( 'NONE',  ( 8.599949509769960088, 8.927695937686774386, 1.040834085586084257E-14 ) ) ;
#201366 = CARTESIAN_POINT ( 'NONE',  ( 7.074468237148123784, 15.51887838114830309, 9.694533992922792720 ) ) ;
#201368 = PRESENTATION_LAYER_ASSIGNMENT (  '', '', ( #94122 ) ) ;
#201367 = CARTESIAN_POINT ( 'NONE',  ( -3.074561225638268725E-14, 3.499999999999960920, -1.052419468952713544 ) ) ;
#201369 = FACE_OUTER_BOUND ( 'NONE', #132276, .T. ) ;
#201370 = CARTESIAN_POINT ( 'NONE',  ( 6.765155463094759014, 7.955398130774449683, 1.082531754730558626 ) ) ;
#201371 = CARTESIAN_POINT ( 'NONE',  ( 1.364683531249997417, 13.29687500034139980, 2.602085213965210642E-15 ) ) ;
#201373 = CARTESIAN_POINT ( 'NONE',  ( 0.6624192275643402406, 0.5246805835648783445, 1.733790746550630146 ) ) ;
#201372 = CARTESIAN_POINT ( 'NONE',  ( 7.991605200612358573, 8.288237253661408843, 0.7998128361456281477 ) ) ;
#201374 = CARTESIAN_POINT ( 'NONE',  ( -6.347188469492005325, 10.55680364771601809, -0.7998128361456291469 ) ) ;
#201375 = CARTESIAN_POINT ( 'NONE',  ( 4.306686350635271054, 8.176217842383143974, -0.7998128361456221525 ) ) ;
#201376 = CARTESIAN_POINT ( 'NONE',  ( 0.3793797362571560972, -6.699757570937929785, 10.99387514841215285 ) ) ;
#201377 = CARTESIAN_POINT ( 'NONE',  ( -11.52901446936773944, 11.29425527467597412, 3.330874149801173356 ) ) ;
#201378 = CARTESIAN_POINT ( 'NONE',  ( 3.388648328411762556, 6.040841252200647382, 1.199719254218462483 ) ) ;
#201379 = EDGE_LOOP ( 'NONE', ( #151633, #102588, #159750, #81956, #49032, #135061 ) ) ;
#201380 = EDGE_CURVE ( 'NONE', #88429, #71979, #132736, .T. ) ;
#201381 = CARTESIAN_POINT ( 'NONE',  ( 5.659779856126235131, 1.203369751103126717, 1.617807692209995984 ) ) ;
#201382 = CARTESIAN_POINT ( 'NONE',  ( -0.07530339154229391541, -0.9103892951793614019, -1.913193754492636067 ) ) ;
#201383 = DIRECTION ( 'NONE',  ( 0.000000000000000000, 0.000000000000000000, 1.000000000000000000 ) ) ;
#201384 = CIRCLE ( 'NONE', #170184, 0.07999999999999946043 ) ;
#201385 = AXIS2_PLACEMENT_3D ( 'NONE', #59713, #141015, #125873 ) ;
#201386 = CARTESIAN_POINT ( 'NONE',  ( -0.1399997263889819765, 0.7174702203470960660, -2.082715917450683740 ) ) ;
#201387 = CARTESIAN_POINT ( 'NONE',  ( -1.360316468750033980, 2.906250000341399797, -3.469446951953614189E-14 ) ) ;
#201388 = CARTESIAN_POINT ( 'NONE',  ( -4.528060117284246289, 6.305822774963486310, 1.443375672974064550 ) ) ;
#201389 = CARTESIAN_POINT ( 'NONE',  ( 8.920901888111989919, 11.43080484092926241, 1.443375672974076540 ) ) ;
#201390 = CARTESIAN_POINT ( 'NONE',  ( 3.133609412646401360, 1.871568317120005265, -0.6134489921753321084 ) ) ;
#201391 = CARTESIAN_POINT ( 'NONE',  ( 4.429314653828757109, -1.560513098751922900, -1.277029310785951388 ) ) ;
#201392 = CARTESIAN_POINT ( 'NONE',  ( -5.343885102080728977, 9.386283052402845328, 0.7998128361456481317 ) ) ;
#201393 = CARTESIAN_POINT ( 'NONE',  ( 0.4288785890452437299, 3.049942316455264812, -0.4196807566835009662 ) ) ;
#201394 = CARTESIAN_POINT ( 'NONE',  ( 0.000000000000000000, 0.9999999999999978906, 11.69999999999999041 ) ) ;
#201395 = CARTESIAN_POINT ( 'NONE',  ( 4.576244502665470115, -2.125281509430646754, -0.5339713055512520512 ) ) ;
#201396 = CARTESIAN_POINT ( 'NONE',  ( -1.123270288250315163, 3.047697346350006331, -0.7749999999993613109 ) ) ;
#201397 = CARTESIAN_POINT ( 'NONE',  ( 2.643477790179576292, -1.426271481392614948, -1.295054687222449541 ) ) ;
#201398 = CARTESIAN_POINT ( 'NONE',  ( -8.206763054973658100, 8.468978407091068306, 0.7998128361456602331 ) ) ;
#201399 = CARTESIAN_POINT ( 'NONE',  ( -0.1296875068447882473, 5.724785194352729256, -2.420566058096422779 ) ) ;
#201400 = DIRECTION ( 'NONE',  ( 1.000000000000000000, -7.771561172376097755E-16, -4.440892098500627148E-16 ) ) ;
#201401 = CARTESIAN_POINT ( 'NONE',  ( 5.578458550106256020, 6.334871154397518467, -1.146459521134872483 ) ) ;
#201402 = EDGE_LOOP ( 'NONE', ( #13074, #134532, #85239, #209235, #101234, #89437 ) ) ;
#201403 = CARTESIAN_POINT ( 'NONE',  ( 4.095971805104285934, 6.832365301713403838, 1.082531754730549078 ) ) ;
#201404 = CARTESIAN_POINT ( 'NONE',  ( 5.471530992243406999, -0.2926990004611991214, 1.947462276923512370 ) ) ;
#201406 = CARTESIAN_POINT ( 'NONE',  ( 3.932292794061467589, -1.036904606752734326, -1.725386108540658103 ) ) ;
#201405 = CARTESIAN_POINT ( 'NONE',  ( 0.2748124788713289246, 1.811699325429259488, -0.6999492020843509632 ) ) ;
#201407 = CARTESIAN_POINT ( 'NONE',  ( 5.958471553546731414, 1.734833135700924345, 1.507719323494296937 ) ) ;
#201409 = CARTESIAN_POINT ( 'NONE',  ( 4.047575586610673071, 1.345269348194571668, 1.286062638920927537 ) ) ;
#201408 = CARTESIAN_POINT ( 'NONE',  ( -7.469616286486262524, 7.679250187180907794, 0.7998128361456341429 ) ) ;
#201410 = CARTESIAN_POINT ( 'NONE',  ( 5.528692779322568640, 9.672168352510192690, 0.7998128361456341429 ) ) ;
#201411 = CARTESIAN_POINT ( 'NONE',  ( -1.500000000000015099, 11.47916666666666252, -0.8660254037844309360 ) ) ;
#201412 = DIRECTION ( 'NONE',  ( 0.000000000000000000, 0.000000000000000000, 1.000000000000000000 ) ) ;
#201413 = CARTESIAN_POINT ( 'NONE',  ( -5.343885102080728977, 9.386283052402845328, 0.7998128361456481317 ) ) ;
#201414 = CARTESIAN_POINT ( 'NONE',  ( -3.338938632592583833, -0.9270362344595499682, 0.07568478739854733739 ) ) ;
#201415 = CARTESIAN_POINT ( 'NONE',  ( 0.5740950506661415265, -1.212703583203307511, 1.825263377225619266 ) ) ;
#201416 = CARTESIAN_POINT ( 'NONE',  ( 3.823036129373602154, 6.443664003369091731, -1.082531754730548412 ) ) ;
#201417 = ORIENTED_EDGE ( 'NONE', *, *, #87595, .F. ) ;
#201418 = AXIS2_PLACEMENT_3D ( 'NONE', #121410, #3277, #87757 ) ;
#201419 = FACE_OUTER_BOUND ( 'NONE', #186359, .T. ) ;
#201420 = CARTESIAN_POINT ( 'NONE',  ( 0.5217476098421744979, -0.9739702522407606144, -1.544006022310390192 ) ) ;
#201421 = CARTESIAN_POINT ( 'NONE',  ( -4.973143418114339021, 4.696422164088486895, 0.7998128361456341429 ) ) ;
#201422 = CARTESIAN_POINT ( 'NONE',  ( 3.076526641549358398, -0.6997103666757237272, 1.586905598789583482 ) ) ;
#201423 = DIRECTION ( 'NONE',  ( -1.000000000000000000, 0.000000000000000000, 3.491481338843133355E-15 ) ) ;
#201424 = CARTESIAN_POINT ( 'NONE',  ( 6.509000000000011887, 3.696273625755361447, 2.514342382328867753 ) ) ;
#201425 = DIRECTION ( 'NONE',  ( 1.000000000000000000, 0.000000000000000000, 0.000000000000000000 ) ) ;
#201426 = CARTESIAN_POINT ( 'NONE',  ( 5.145057536039753465, -1.563975785779356587, 0.9416349707431559413 ) ) ;
#201427 = CARTESIAN_POINT ( 'NONE',  ( 3.221486639279776298, 0.2924833653642990861, -1.939731193138781951 ) ) ;
#201428 = CARTESIAN_POINT ( 'NONE',  ( 1.224999999999989875, -1.062499999317199961, -3.469446951953614189E-15 ) ) ;
#201429 = CARTESIAN_POINT ( 'NONE',  ( -9.691380875670077444, 10.20103253123691189, 0.7998128361456462443 ) ) ;
#201430 = CARTESIAN_POINT ( 'NONE',  ( 6.856673000209174695, 9.022537805042615489, 1.599625672291281386 ) ) ;
#201431 = CARTESIAN_POINT ( 'NONE',  ( 5.320985837513584116, 1.605487267134264595, -1.385306402853322405 ) ) ;
#201432 = CARTESIAN_POINT ( 'NONE',  ( 6.535912570239620578, 9.782925877658371405, 1.199719254218452047 ) ) ;
#201433 = CARTESIAN_POINT ( 'NONE',  ( -10.30827686509187835, 10.92074451889568643, 1.040834085586084257E-14 ) ) ;
#201434 = CARTESIAN_POINT ( 'NONE',  ( 2.729418486472269922, 0.1060373921930452268, -2.067687848736274869 ) ) ;
#201436 = CARTESIAN_POINT ( 'NONE',  ( -1.402160292154681736E-14, -0.4906249996585810846, -1.575800808251665908 ) ) ;
#201435 = CARTESIAN_POINT ( 'NONE',  ( -11.86145017031048177, 11.00581953513854394, 1.099999999999996980 ) ) ;
#201438 = ORIENTED_EDGE ( 'NONE', *, *, #150221, .F. ) ;
#201437 = CARTESIAN_POINT ( 'NONE',  ( 4.776165916792348476, 2.197254790419100434, -0.3252806346676767046 ) ) ;
#201439 = CARTESIAN_POINT ( 'NONE',  ( 3.340769233699531604, 0.5564940052410914939, -2.230230389815818892 ) ) ;
#201440 = CARTESIAN_POINT ( 'NONE',  ( 7.890482213473377193, 11.18901776815221716, -1.082531754730543083 ) ) ;
#201442 = CARTESIAN_POINT ( 'NONE',  ( 3.285556943749998737, -2.705208332855374209, -1.896917185911906500 ) ) ;
#201441 = CARTESIAN_POINT ( 'NONE',  ( 7.187230829020129441, 8.518095734345896730, 1.082531754730549967 ) ) ;
#201443 = PLANE ( 'NONE',  #26736 ) ;
#201444 = ORIENTED_EDGE ( 'NONE', *, *, #35195, .F. ) ;
#201445 = CARTESIAN_POINT ( 'NONE',  ( -5.503043298372868541, 6.255613091374303991, -0.9824725695728808716 ) ) ;
#201446 = CARTESIAN_POINT ( 'NONE',  ( 3.199369407753744454, 1.726971514772487559, -0.8218122705464236954 ) ) ;
#201447 = CARTESIAN_POINT ( 'NONE',  ( -9.367496997601300279, 15.00000000000599343, -7.499999999995378808 ) ) ;
#201448 = CARTESIAN_POINT ( 'NONE',  ( 4.612129873793564094, -0.7390372460917455921, -1.558541145072767975 ) ) ;
#201449 = CARTESIAN_POINT ( 'NONE',  ( 2.905482715143858030, -1.942096844255640109, 0.5424705965835219246 ) ) ;
#201450 = CARTESIAN_POINT ( 'NONE',  ( 3.955939753277417648, -2.145046849925678956, -0.8267234532119535073 ) ) ;
#201451 = CYLINDRICAL_SURFACE ( 'NONE', #125595, 1.250000000000000000 ) ;
#201452 = CARTESIAN_POINT ( 'NONE',  ( 6.041652760897754604, -1.524265013729691143, -1.453574456173498231 ) ) ;
#201453 = CARTESIAN_POINT ( 'NONE',  ( -4.340018570150306232, 8.077455741901736985, -0.7216878364870338292 ) ) ;
#201454 = ORIENTED_EDGE ( 'NONE', *, *, #126765, .F. ) ;
#201455 = CARTESIAN_POINT ( 'NONE',  ( 4.551851636600127371, 1.769384361346277856, -0.04241240985469392488 ) ) ;
#201457 = CARTESIAN_POINT ( 'NONE',  ( 0.5336625369133874974, -1.625122730996070297, -1.616870241932764074 ) ) ;
#201456 = CARTESIAN_POINT ( 'NONE',  ( 7.523848900940885542, 7.742521570711348389, 0.7998128361456291469 ) ) ;
#201458 = CARTESIAN_POINT ( 'NONE',  ( 0.1810874682179625661, -0.8250252819957092365, 1.532327275369157915 ) ) ;
#201459 = CARTESIAN_POINT ( 'NONE',  ( -7.608060475923978494, 8.905100639113307182, 1.199719254218452047 ) ) ;
#201460 = CARTESIAN_POINT ( 'NONE',  ( 6.439412520197737244, 0.8424478218750917069, -2.023249321508275855 ) ) ;
#201461 = CARTESIAN_POINT ( 'NONE',  ( -4.085803189671902480, 5.860132702740892263, -1.599625672291271394 ) ) ;
#201462 = CARTESIAN_POINT ( 'NONE',  ( 1.360316468749969809, -0.6822916663252893699, -0.7853790794159082322 ) ) ;
#201463 = CARTESIAN_POINT ( 'NONE',  ( 9.499065438569621378, -8.103879979615417284, -0.1510907968719069627 ) ) ;
#201464 = CARTESIAN_POINT ( 'NONE',  ( 0.7312207505087648940, -2.044463659613379392, -0.7311735514200778940 ) ) ;
#201465 = CARTESIAN_POINT ( 'NONE',  ( 0.9543149826918421175, -1.275552737861269437, 1.561884623745241951 ) ) ;
#201466 = AXIS2_PLACEMENT_3D ( 'NONE', #88311, #121954, #5952 ) ;
#201467 = CARTESIAN_POINT ( 'NONE',  ( -1.201851678989727383E-14, 5.696875000341416140, -1.575800808251660134 ) ) ;
#201468 = CARTESIAN_POINT ( 'NONE',  ( 4.899011302651929078, 1.600714092801895472, -1.071686876026227475 ) ) ;
#201469 = CARTESIAN_POINT ( 'NONE',  ( -8.012344526598182026E-15, 11.54687500034139980, -1.575800808251669460 ) ) ;
#201470 = CARTESIAN_POINT ( 'NONE',  ( 0.8268048150999330881, -1.005496690709275720, -1.980927387359689318 ) ) ;
#201472 = ORIENTED_EDGE ( 'NONE', *, *, #11734, .F. ) ;
#201471 = CARTESIAN_POINT ( 'NONE',  ( 8.594979316059474073, 12.11489407112305372, 1.199719254218450271 ) ) ;
#201475 = TOROIDAL_SURFACE ( 'NONE', #201636, 11.92000000000000171, 0.08000000000000000167 ) ;
#201474 = DIRECTION ( 'NONE',  ( 0.000000000000000000, 0.000000000000000000, -1.000000000000000000 ) ) ;
#201473 = DIRECTION ( 'NONE',  ( -0.1510067114093955887, 0.000000000000000000, -0.9885327375000383388 ) ) ;
#201476 = CARTESIAN_POINT ( 'NONE',  ( -0.4716924744713574813, 3.050499071788768113, -1.943633845707283703 ) ) ;
#201477 = CARTESIAN_POINT ( 'NONE',  ( 10.40318394038753702, 11.03146944007395724, -0.7998128361456281477 ) ) ;
#201478 = DIRECTION ( 'NONE',  ( 0.000000000000000000, -1.000000000000000000, 0.000000000000000000 ) ) ;
#201479 = CARTESIAN_POINT ( 'NONE',  ( 1.772826578343081660, 3.950000000000036593, -0.4000000000000478728 ) ) ;
#201480 = CARTESIAN_POINT ( 'NONE',  ( 4.651753270297207976, 0.6719488171132372845, 1.605710474869048499 ) ) ;
#201481 = CARTESIAN_POINT ( 'NONE',  ( 1.908577322519442454, 0.6123880975643314351, 1.863924812142327747 ) ) ;
#201483 = CARTESIAN_POINT ( 'NONE',  ( 0.6823417656249882723, 2.238541667008084435, -1.181850606188749264 ) ) ;
#201482 = CARTESIAN_POINT ( 'NONE',  ( 5.522248639467795428, 5.337044922334209573, -0.7998128361456231517 ) ) ;
#201484 = CARTESIAN_POINT ( 'NONE',  ( 10.98765602437503830, -5.221050908132835566, 8.077306185017006456E-15 ) ) ;
#201485 = CARTESIAN_POINT ( 'NONE',  ( 6.531700620877029628, 1.877769495358465157, -0.5682946464737671510 ) ) ;
#201486 = CARTESIAN_POINT ( 'NONE',  ( -7.263417608619167076, 9.497073181520933716, -1.599625672291263179 ) ) ;
#201487 = CARTESIAN_POINT ( 'NONE',  ( -5.083944415000202888, 5.033616027029415463, 0.7216878364870317197 ) ) ;
#201488 = CARTESIAN_POINT ( 'NONE',  ( 1.288340396327339432, -1.015645312862264227, 2.021827887327799722 ) ) ;
#201490 = VERTEX_POINT ( 'NONE', #86081 ) ;
#201489 = CARTESIAN_POINT ( 'NONE',  ( -6.338600509588822263, 7.353787668397130162, -1.199719254218446718 ) ) ;
#201491 = CARTESIAN_POINT ( 'NONE',  ( 0.7499999999999885647, 0.5979166673494851203, -1.299038105676652899 ) ) ;
#201492 = CARTESIAN_POINT ( 'NONE',  ( 1.387741975113141235, -0.8460221195879283895, 1.668388151239764028 ) ) ;
#201493 = CARTESIAN_POINT ( 'NONE',  ( 0.3165338080420940781, 0.8936020571472038654, -1.485981903106075031 ) ) ;
#201494 = CARTESIAN_POINT ( 'NONE',  ( 3.931328349035985603, -1.512150646884598215, -1.586510368271301541 ) ) ;
#201495 = CARTESIAN_POINT ( 'NONE',  ( 5.051972272063284031, 0.7293918257267332228, -2.189345848185173082 ) ) ;
#201496 = B_SPLINE_CURVE_WITH_KNOTS ( 'NONE', 3,
 ( #119844, #185822, #103532, #169591, #21173, #54777, #90494, #187962 ),
 .UNSPECIFIED., .F., .F.,
 ( 4, 2, 2, 4 ),
 ( -5.999999999245582952E-08, 0.001012685428351500902, 0.001519058142527249765, 0.002025430856702998845 ),
 .UNSPECIFIED. ) ;
#201497 = CARTESIAN_POINT ( 'NONE',  ( 1.077108160694364214, -0.04970969036830223675, -2.060456431261459276 ) ) ;
#201498 = CARTESIAN_POINT ( 'NONE',  ( 3.468632250064273670, 0.04687378517908299957, -1.941542025766171298 ) ) ;
#201499 = CARTESIAN_POINT ( 'NONE',  ( -2.928197990427299668, 6.360055388899728435, 1.040834085586084257E-14 ) ) ;
#201500 = CARTESIAN_POINT ( 'NONE',  ( 5.413307058180727438, -0.2754873708227522644, 1.850039175317084617 ) ) ;
#201501 = CARTESIAN_POINT ( 'NONE',  ( 0.4546835345321549871, 13.29443243002577191, 1.375797179799232106 ) ) ;
#201502 = CARTESIAN_POINT ( 'NONE',  ( 0.1745346383498986020, -0.7352478164647980874, -1.569626033853884106 ) ) ;
#201503 = CARTESIAN_POINT ( 'NONE',  ( 3.743459811148990291, 7.381470523066878009, -0.7216878364870338292 ) ) ;
#201504 = CARTESIAN_POINT ( 'NONE',  ( -0.6801582343750299797, 1.182291667008061875, 1.178068619123820771 ) ) ;
#201505 = CARTESIAN_POINT ( 'NONE',  ( 5.080704010962952211, -0.7231418808758652839, 1.882473355234378865 ) ) ;
#201506 = CARTESIAN_POINT ( 'NONE',  ( -5.083944415000202888, 5.033616027029415463, 0.7216878364870317197 ) ) ;
#201507 = CARTESIAN_POINT ( 'NONE',  ( 7.072549687823125097, 11.40305840243567381, -0.7998128361456291469 ) ) ;
#201509 = CARTESIAN_POINT ( 'NONE',  ( -6.701130152864324785, -6.864242550357222861, 6.729185449012851983 ) ) ;
#201508 = CARTESIAN_POINT ( 'NONE',  ( 1.664397423953474009, -1.292156093668932693, 1.290017532847971271 ) ) ;
#201510 = CARTESIAN_POINT ( 'NONE',  ( -4.502189528189771472, 7.410248995266807803, -1.199719254218453823 ) ) ;
#201511 = CARTESIAN_POINT ( 'NONE',  ( -5.330290668828105538, 6.247702530834755130, 1.199719254218452935 ) ) ;
#201512 = CARTESIAN_POINT ( 'NONE',  ( -9.970593900173907898, 5.552053933461305490, 5.997145116287158295 ) ) ;
#201513 = ORIENTED_EDGE ( 'NONE', *, *, #161432, .F. ) ;
#201514 = CARTESIAN_POINT ( 'NONE',  ( -6.468648687051513413, 7.679749902049126220, 1.082531754730549078 ) ) ;
#201515 = EDGE_CURVE ( 'NONE', #93276, #189704, #71799, .T. ) ;
#201516 = CARTESIAN_POINT ( 'NONE',  ( -1.284279953904156280, 3.202889714876734573, 0.7750000000000117906 ) ) ;
#201517 = CARTESIAN_POINT ( 'NONE',  ( -4.827553558169476844, 4.879519697517697985, -0.5995761563960356755 ) ) ;
#201518 = CARTESIAN_POINT ( 'NONE',  ( 5.742833863956755103, 1.946992082993486584, 0.5367204025522700483 ) ) ;
#201520 = VERTEX_POINT ( 'NONE', #201926 ) ;
#201519 = CARTESIAN_POINT ( 'NONE',  ( 0.1531979293848736434, 0.3668625560977051281, 2.088361607889513305 ) ) ;
#201521 = CARTESIAN_POINT ( 'NONE',  ( -5.424143973919053785, 8.485862515284315677, 1.199719254218454489 ) ) ;
#201522 = CARTESIAN_POINT ( 'NONE',  ( 4.008406971134620633, 7.828225232965717595, 0.7998128361456321445 ) ) ;
#201523 = CARTESIAN_POINT ( 'NONE',  ( 5.172756020173422620, -1.939746602593624081, -0.6965250322775017322 ) ) ;
#201524 = CARTESIAN_POINT ( 'NONE',  ( 4.641250102003462885, 0.7743139518727222281, 1.862017545363145343 ) ) ;
#201525 = VERTEX_POINT ( 'NONE', #68739 ) ;
#201526 = EDGE_LOOP ( 'NONE', ( #193839, #19063 ) ) ;
#201527 = DIRECTION ( 'NONE',  ( 0.000000000000000000, 0.000000000000000000, -1.000000000000000000 ) ) ;
#201528 = CARTESIAN_POINT ( 'NONE',  ( 4.216749469050096621, 4.878294787768598262, -1.199719254218452047 ) ) ;
#201530 = VERTEX_POINT ( 'NONE', #213919 ) ;
#201529 = CARTESIAN_POINT ( 'NONE',  ( -6.818824913030298696, 6.919993584815607335, 0.7998128361456341429 ) ) ;
#201531 = CARTESIAN_POINT ( 'NONE',  ( 4.632842592818133376, 8.443130954262043630, -0.3954830847591808696 ) ) ;
#201532 = CARTESIAN_POINT ( 'NONE',  ( 5.044295983762377311, 1.882185518538554314, -0.7230303062365079914 ) ) ;
#201533 = CARTESIAN_POINT ( 'NONE',  ( 3.767381502543519112, 1.024135474229198151, 1.529801857347697025 ) ) ;
#201534 = CARTESIAN_POINT ( 'NONE',  ( 0.000000000000000000, 6.999999999999999112, 0.000000000000000000 ) ) ;
#201535 = CARTESIAN_POINT ( 'NONE',  ( 2.719673384174253972, -0.2251885735481904405, 2.296679687964820360 ) ) ;
#201536 = CARTESIAN_POINT ( 'NONE',  ( 7.205232291019763480, 7.370802192470005565, -0.7998128361456341429 ) ) ;
#201537 = CARTESIAN_POINT ( 'NONE',  ( 4.411504763889100289, -0.3743020017868466387, 2.128795073437335095 ) ) ;
#201538 = CARTESIAN_POINT ( 'NONE',  ( 8.796542737168120851, 9.157054702984622097, -0.7998128361456211532 ) ) ;
#201539 = CARTESIAN_POINT ( 'NONE',  ( -0.04160512940111232155, -1.735061556407999417, -0.8725848562033207134 ) ) ;
#201540 = CARTESIAN_POINT ( 'NONE',  ( -5.220052836461385404, 6.048815383081766583, -1.199719254218446718 ) ) ;
#201541 = CARTESIAN_POINT ( 'NONE',  ( 3.972236164830291738, 1.968842830503451991, 1.185689330230592642 ) ) ;
#201542 = CARTESIAN_POINT ( 'NONE',  ( -9.372067988322836385, 15.41907390678799494, -7.405912380499037440 ) ) ;
#201543 =( GEOMETRIC_REPRESENTATION_CONTEXT ( 3 ) GLOBAL_UNCERTAINTY_ASSIGNED_CONTEXT ( ( #32340 ) ) GLOBAL_UNIT_ASSIGNED_CONTEXT ( ( #87568, #55069, #153635 ) ) REPRESENTATION_CONTEXT ( 'NONE', 'WORKASPACE' ) );
#201544 = CARTESIAN_POINT ( 'NONE',  ( 3.924554409752772699, 1.776107677202539925, 0.5873546117282567591 ) ) ;
#201545 = COLOUR_RGB ( '', 0.31764706, 0.68627451, 0.89019608) ;
#201546 = ADVANCED_FACE ( 'NONE', ( #166264 ), #110598, .T. ) ;
#201547 = CARTESIAN_POINT ( 'NONE',  ( 0.2804619692761011751, -1.911105013696552168, -0.4832259537779006742 ) ) ;
#201549 = CARTESIAN_POINT ( 'NONE',  ( -7.923814432544069142, 8.209148024248356990, 0.000000000000000000 ) ) ;
#201548 = CARTESIAN_POINT ( 'NONE',  ( 1.499999999999987566, -1.193749999317185395, 0.000000000000000000 ) ) ;
#201550 = CARTESIAN_POINT ( 'NONE',  ( 1.436444770134176485, 1.085300811998829662, -1.921501399296850821 ) ) ;
#201551 = VERTEX_POINT ( 'NONE', #148954 ) ;
#201552 = CARTESIAN_POINT ( 'NONE',  ( -3.253593677155282471, 6.739683690082376444, 1.040834085586084257E-14 ) ) ;
#201553 = CARTESIAN_POINT ( 'NONE',  ( 4.192495815123822744, 5.914331089109666983, -1.599625672291255185 ) ) ;
#201554 = CARTESIAN_POINT ( 'NONE',  ( -5.461236948206312114, 5.265864615862458464, 0.7998128361456341429 ) ) ;
#201555 = CARTESIAN_POINT ( 'NONE',  ( -0.1963700886235999477, -6.681311647492901962, -9.612263720970510406 ) ) ;
#201556 = CARTESIAN_POINT ( 'NONE',  ( 6.702032618711820433, -1.971027473680329045, 0.04818573739380492549 ) ) ;
#201557 = CARTESIAN_POINT ( 'NONE',  ( 0.5523711044835468709, 0.7197940642212009577, -2.192503933474987843 ) ) ;
#201558 = CARTESIAN_POINT ( 'NONE',  ( 0.3792546940144908563, -0.1001052471676349837, 1.959448305358338693 ) ) ;
#201559 = CARTESIAN_POINT ( 'NONE',  ( 4.557522945366278222, 1.653560713460072051, 1.232637662666216549 ) ) ;
#201560 = CARTESIAN_POINT ( 'NONE',  ( 6.155038550924155416, 6.283225852274053835, 0.7216878364870317197 ) ) ;
#201561 = AXIS2_PLACEMENT_3D ( 'NONE', #199326, #2180, #20579 ) ;
#201562 = CARTESIAN_POINT ( 'NONE',  ( 7.530627977747744062, 7.750430493652658015, -0.7998128361456341429 ) ) ;
#201563 = ORIENTED_EDGE ( 'NONE', *, *, #80091, .T. ) ;
#201564 = CARTESIAN_POINT ( 'NONE',  ( 8.554831740098663317, 9.082984572977682802, 0.7216878364870458196 ) ) ;
#201565 = CARTESIAN_POINT ( 'NONE',  ( -1.364683531250012516, 5.051041667008085767, -0.7879004041258300672 ) ) ;
#201566 = DIRECTION ( 'NONE',  ( -1.000000000000000000, 0.000000000000000000, 0.000000000000000000 ) ) ;
#201567 = CARTESIAN_POINT ( 'NONE',  ( 3.999292125906899198, 6.649295999324608353, 1.082531754730558626 ) ) ;
#201568 = CARTESIAN_POINT ( 'NONE',  ( 6.443812750726708671, 1.492410320797844747, 1.577172898185905670 ) ) ;
#201570 = CARTESIAN_POINT ( 'NONE',  ( 5.126429434416579056, 0.1410513515392505246, 1.835921608166577013 ) ) ;
#201569 = CARTESIAN_POINT ( 'NONE',  ( 9.499562137383495752, -9.414773216041249171, -0.1228851354130882229 ) ) ;
#201571 = CARTESIAN_POINT ( 'NONE',  ( 11.91826849282518275, 12.69999999999997975, 1.399999999999998579 ) ) ;
#201572 = DIRECTION ( 'NONE',  ( -0.6507913734559596097, 0.7592566023653043450, 0.000000000000000000 ) ) ;
#201573 = DIRECTION ( 'NONE',  ( 0.000000000000000000, 1.000000000000000000, 0.000000000000000000 ) ) ;
#201575 = CARTESIAN_POINT ( 'NONE',  ( -4.377387467589398007, 7.366231944554199274, 1.201952607213795821 ) ) ;
#201574 = AXIS2_PLACEMENT_3D ( 'NONE', #174586, #190789, #210236 ) ;
#201576 = CARTESIAN_POINT ( 'NONE',  ( 5.092389439195339484, 7.944299729584391123, -1.199137415704543130 ) ) ;
#201577 = CARTESIAN_POINT ( 'NONE',  ( 1.364683531249990311, 4.696875000341417916, 1.214306433183764966E-14 ) ) ;
#201578 = CARTESIAN_POINT ( 'NONE',  ( 0.9438406676962156627, -1.213610516764839664, -1.477797202995428938 ) ) ;
#201579 = CARTESIAN_POINT ( 'NONE',  ( 1.814973546968738027, -0.2204486908502552300, 1.755991699180702748 ) ) ;
#201580 = CARTESIAN_POINT ( 'NONE',  ( 0.1352199593073095951, -0.09384731153385186819, 1.910084486482076294 ) ) ;
#201582 = CARTESIAN_POINT ( 'NONE',  ( 4.886306726311728355, -0.6496138446146214607, -1.802220356481977204 ) ) ;
#201581 = CARTESIAN_POINT ( 'NONE',  ( -10.31505594189871111, 10.92865344183699428, -0.7998128361456291469 ) ) ;
#201583 = DIRECTION ( 'NONE',  ( -0.000000000000000000, -0.000000000000000000, 1.000000000000000000 ) ) ;
#201584 = CARTESIAN_POINT ( 'NONE',  ( 5.775830853014204180, -1.921903692836058886, 0.4298591908668251138 ) ) ;
#201585 = CARTESIAN_POINT ( 'NONE',  ( 0.2289750728588327566, 1.457791096766167360, -1.540313549178488284 ) ) ;
#201586 = CARTESIAN_POINT ( 'NONE',  ( -0.3866901564497978727, 3.102326550341739875, 2.027579305719746205 ) ) ;
#201587 = CARTESIAN_POINT ( 'NONE',  ( 4.399188623838041323, 1.502396186649012311, 1.114296746780506497 ) ) ;
#201589 = VERTEX_POINT ( 'NONE', #150029 ) ;
#201588 = CARTESIAN_POINT ( 'NONE',  ( 6.727182134110236689, 0.008744176509112643741, 1.710970312420513562 ) ) ;
#201591 = CARTESIAN_POINT ( 'NONE',  ( 4.555176424511575561, 4.416720038126027426, -0.7216878364870188411 ) ) ;
#201590 = CARTESIAN_POINT ( 'NONE',  ( 3.334799921508072806, 2.153101868192684343, 0.4835390122766567433 ) ) ;
#201592 = CARTESIAN_POINT ( 'NONE',  ( -0.6823417656249969321, 4.780208333674755394, -1.181850606188749264 ) ) ;
#201593 = CARTESIAN_POINT ( 'NONE',  ( 0.8716181059342765769, -0.3045769538833371648, 2.039966307373513033 ) ) ;
#201594 = CARTESIAN_POINT ( 'NONE',  ( 6.089583550832340819, 10.25626457594641749, 1.040834085586084257E-14 ) ) ;
#201595 = CARTESIAN_POINT ( 'NONE',  ( -9.504429378379839477, 11.04725468198666150, 1.199719254218462483 ) ) ;
#201596 = CYLINDRICAL_SURFACE ( 'NONE', #133717, 0.05000000000000002359 ) ;
#201597 = CARTESIAN_POINT ( 'NONE',  ( -3.581325132304157943, 7.329963087663487364, -0.7998128361456282587 ) ) ;
#201598 = CARTESIAN_POINT ( 'NONE',  ( -1.499999999999960476, 6.999999999999999112, 10.89724735885168982 ) ) ;
#201599 = EDGE_LOOP ( 'NONE', ( #168172, #131134, #155611, #176765 ) ) ;
#201600 = CARTESIAN_POINT ( 'NONE',  ( 3.104029480343179603, 0.7476448069429382226, -1.930825944200013966 ) ) ;
#201601 = CARTESIAN_POINT ( 'NONE',  ( -1.499999999999997780, 4.400000000000021672, 1.214306433183764966E-14 ) ) ;
#201602 = CARTESIAN_POINT ( 'NONE',  ( 5.847644326195776010, 5.716673223516856694, -0.7998128361456281477 ) ) ;
#201603 = CARTESIAN_POINT ( 'NONE',  ( -6.606716786301501720, 6.763562328987043237, 0.1806677948501221598 ) ) ;
#201604 = CARTESIAN_POINT ( 'NONE',  ( 0.7330764811492549438, 1.866981473359119237, 0.7708630573498123084 ) ) ;
#201605 = DIRECTION ( 'NONE',  ( -7.387867266669436732E-31, 1.000000000000000000, -8.546850786086437571E-32 ) ) ;
#201607 = CARTESIAN_POINT ( 'NONE',  ( 7.619319141200057821, 10.87266085050000974, 1.082531754730557072 ) ) ;
#201606 = CARTESIAN_POINT ( 'NONE',  ( 0.07479286986305369589, 4.095183424177953668, -2.410510762676120411 ) ) ;
#201608 = CARTESIAN_POINT ( 'NONE',  ( 6.890000000000050306, -0.002781820520068867264, 1.999840353888074240 ) ) ;
#201609 = CARTESIAN_POINT ( 'NONE',  ( 5.893738820153655134, -1.900388249151972353, 0.2415585323580979049 ) ) ;
#201610 = CARTESIAN_POINT ( 'NONE',  ( 4.353197867323560288, 0.4795420089713005041, -2.138300074133951068 ) ) ;
#201611 =( BOUNDED_CURVE ( )  B_SPLINE_CURVE ( 2, ( #202771, #133571, #68505, #69568, #38169, #117345, #292, #54421, #118414 ),
 .UNSPECIFIED., .F., .T. ) 
 B_SPLINE_CURVE_WITH_KNOTS ( ( 3, 2, 2, 2, 3 ),
 ( 0.7946428571428572063, 0.7976190476190476719, 0.8035714285714286031, 0.8095238095238095344, 0.8125000000000000000 ),
 .UNSPECIFIED. ) 
 CURVE ( )  GEOMETRIC_REPRESENTATION_ITEM ( )  RATIONAL_B_SPLINE_CURVE ( ( 0.9330127018922194093, 0.9330127018922206306, 1.000000000000000000, 0.8660254037844387076, 1.000000000000000000, 0.8660254037844387076, 1.000000000000000000, 0.9330127018922194093, 0.9330127018922194093 ) ) 
 REPRESENTATION_ITEM ( '' )  );
#201612 = CARTESIAN_POINT ( 'NONE',  ( 1.499999999999989120, 4.035416667349482012, 0.8660254037844524744 ) ) ;
#201613 = CARTESIAN_POINT ( 'NONE',  ( 3.955252344019274169, -1.661368509396843995, 0.9470704235666274062 ) ) ;
#201614 = CARTESIAN_POINT ( 'NONE',  ( -4.042302355168801320, 7.867769847672247074, 0.7998128361456341429 ) ) ;
#201615 = CARTESIAN_POINT ( 'NONE',  ( 4.677199806590210507, 4.559080650551097236, -0.7216878364870197293 ) ) ;
#201617 = CARTESIAN_POINT ( 'NONE',  ( 0.7203276360899166786, 1.987051886588153682, 0.3419113104980234241 ) ) ;
#201616 = CARTESIAN_POINT ( 'NONE',  ( 3.469446951953614189E-15, 6.180000000000019256, 1.214306433183764966E-14 ) ) ;
#201618 = CARTESIAN_POINT ( 'NONE',  ( -1.402160292154681736E-14, 11.48437500034139980, 1.575800808251682339 ) ) ;
#201620 = CARTESIAN_POINT ( 'NONE',  ( -5.842637852846353397, 5.781108681267656202, 0.7998128361456281477 ) ) ;
#201619 = CARTESIAN_POINT ( 'NONE',  ( 6.216381822182693639, 2.044192415450503120, 0.7905562269360306704 ) ) ;
#201622 = ORIENTED_EDGE ( 'NONE', *, *, #25508, .T. ) ;
#201621 = CARTESIAN_POINT ( 'NONE',  ( 3.504663807952506538, 1.359994529648723249, -1.060664293495124477 ) ) ;
#201623 = CARTESIAN_POINT ( 'NONE',  ( -0.1399997263889611598, 2.874570648431204578, -2.488748559936367233 ) ) ;
#201624 = CARTESIAN_POINT ( 'NONE',  ( 7.579171565239241737, 8.801120566655981747, 1.199719254218462483 ) ) ;
#201625 = CARTESIAN_POINT ( 'NONE',  ( 3.323720213644492993, 7.029424015893889433, 1.040834085586084257E-14 ) ) ;
#201626 = CARTESIAN_POINT ( 'NONE',  ( 11.89942855770814312, 11.29999999999999893, 0.6999999999999992895 ) ) ;
#201627 = CARTESIAN_POINT ( 'NONE',  ( 1.346068015636435522, -0.8851805579040676886, 1.750911360861057142 ) ) ;
#201628 =( BOUNDED_SURFACE ( )  B_SPLINE_SURFACE ( 3, 2, ( 
 ( #9040, #107681, #190972 ),
 ( #108747, #75114, #25285 ),
 ( #126077, #154231, #40492 ),
 ( #188856, #206165, #141226 ) ),
 .UNSPECIFIED., .F., .F., .F. ) 
 B_SPLINE_SURFACE_WITH_KNOTS ( ( 4, 4 ),
 ( 3, 3 ),
 ( 0.5050616349177513564, 1.570796326794896558 ),
 ( 0.000000000000000000, 1.000000000000000000 ),
 .UNSPECIFIED. ) 
 GEOMETRIC_REPRESENTATION_ITEM ( )  RATIONAL_B_SPLINE_SURFACE ( (
 ( 1.000000000000000000, 0.9374448844494494004, 1.000000000000000000),
 ( 1.000000000000000000, 0.8980788380694090245, 1.000000000000000000),
 ( 1.000000000000000000, 0.8161930835858599576, 1.000000000000000000),
 ( 1.000000000000000000, 0.7071067811865933139, 1.000000000000000000) ) ) 
 REPRESENTATION_ITEM ( '' )  SURFACE ( )  );
#201629 = CARTESIAN_POINT ( 'NONE',  ( 5.192936529234042808, 6.017179691316550283, -1.199719254218452047 ) ) ;
#201630 = CARTESIAN_POINT ( 'NONE',  ( 0.1755611466353446948, 4.081716065625639267, -2.798746370182193743 ) ) ;
#201631 = EDGE_LOOP ( 'NONE', ( #111854, #32551, #186346, #76430 ) ) ;
#201632 = FACE_OUTER_BOUND ( 'NONE', #13492, .T. ) ;
#201633 = ORIENTED_EDGE ( 'NONE', *, *, #190367, .T. ) ;
#201634 = CARTESIAN_POINT ( 'NONE',  ( 4.195841788199461853, 1.186545534222239962, 1.368844175430401933 ) ) ;
#201635 = ORIENTED_EDGE ( 'NONE', *, *, #154010, .F. ) ;
#201636 = AXIS2_PLACEMENT_3D ( 'NONE', #84686, #150773, #149693 ) ;
#201637 = CARTESIAN_POINT ( 'NONE',  ( 0.000000000000000000, -1.399999999999998579, 0.000000000000000000 ) ) ;
#201638 = CARTESIAN_POINT ( 'NONE',  ( 5.232992382607310589, 1.676000702356477134, 0.6878641890804160219 ) ) ;
#201639 = CARTESIAN_POINT ( 'NONE',  ( 5.668717623845194176, 9.627604637879139560, 0.000000000000000000 ) ) ;
#201640 = CARTESIAN_POINT ( 'NONE',  ( -6.634380643896215624, -6.684699857435322023, -6.783773228136961819 ) ) ;
#201641 = CARTESIAN_POINT ( 'NONE',  ( 4.825424889954152086, 6.722588627200480893, -1.249340337910074705 ) ) ;
#201642 = EDGE_CURVE ( 'NONE', #124142, #22696, #64954, .T. ) ;
#201644 = CARTESIAN_POINT ( 'NONE',  ( 10.38962578677386084, 11.01565159419135043, 0.000000000000000000 ) ) ;
#201643 = CARTESIAN_POINT ( 'NONE',  ( 4.703460533163725366, -1.437978410778781857, -1.181371033526560144 ) ) ;
#201645 = CARTESIAN_POINT ( 'NONE',  ( 2.776846452629442297, 1.641606522343663555, -0.9870246354491112317 ) ) ;
#201646 = CARTESIAN_POINT ( 'NONE',  ( -6.396834479292728304, -8.176568542494925040, -7.055228938193916832 ) ) ;
#201647 = CARTESIAN_POINT ( 'NONE',  ( -10.90756946389101323, 4.636105284860338571, -4.485523696119586567 ) ) ;
#201648 = CARTESIAN_POINT ( 'NONE',  ( 1.364683531249986981, -1.115624999658580752, 0.000000000000000000 ) ) ;
#201649 = CARTESIAN_POINT ( 'NONE',  ( 6.819388077993785657, 7.058300300521964665, 1.040834085586084257E-14 ) ) ;
#201650 = CARTESIAN_POINT ( 'NONE',  ( -8.487040972474682476, 12.84537220128841817, 0.7216878364870338292 ) ) ;
#201651 = CARTESIAN_POINT ( 'NONE',  ( 0.4093245661422850179, 1.881582470445356314, 1.064130679222355491 ) ) ;
#201652 = CARTESIAN_POINT ( 'NONE',  ( -5.576146316970437944, 9.727530813099326323, 0.000000000000000000 ) ) ;
#201653 = EDGE_CURVE ( 'NONE', #110797, #93128, #132697, .T. ) ;
#201654 = CARTESIAN_POINT ( 'NONE',  ( 1.939510448661335484, 0.7990184383764920018, -1.932127011870365951 ) ) ;
#201655 = CARTESIAN_POINT ( 'NONE',  ( 5.987861119090863049, 7.014868056141362551, 1.199719254218452047 ) ) ;
#201656 = CARTESIAN_POINT ( 'NONE',  ( 0.5162701059127188241, 1.262803565755654001, -1.318596375272471199 ) ) ;
#201657 = CARTESIAN_POINT ( 'NONE',  ( -4.771579997005698459, 7.654261532226910525, -1.199719254218452047 ) ) ;
#201658 = CARTESIAN_POINT ( 'NONE',  ( 2.924607851032960504, 1.718362407962298111, 0.6167639819729957562 ) ) ;
#201659 = CYLINDRICAL_SURFACE ( 'NONE', #48138, 10.24999999999998934 ) ;
#201660 = CARTESIAN_POINT ( 'NONE',  ( 2.127084423382288314, 1.709874882824816478, 0.8565708355050825062 ) ) ;
#201661 = CARTESIAN_POINT ( 'NONE',  ( 2.576555279139204568, 1.288776560207754551, -1.489423508990360023 ) ) ;
#201662 = EDGE_LOOP ( 'NONE', ( #210164, #58091, #28605, #63282 ) ) ;
#201663 = CARTESIAN_POINT ( 'NONE',  ( 3.649888709942475273, 0.7017510601828327310, 1.811005675494174350 ) ) ;
#201664 = ORIENTED_EDGE ( 'NONE', *, *, #137524, .F. ) ;
#201665 = CARTESIAN_POINT ( 'NONE',  ( -7.747558435566414659, 8.003516027774422170, -0.7998128361456362523 ) ) ;
#201667 = CARTESIAN_POINT ( 'NONE',  ( 4.711248855110969913, 1.761570823303935551, -1.180294879073326308 ) ) ;
#201666 = CARTESIAN_POINT ( 'NONE',  ( 6.831329296439236032, 9.063246493969506545, -1.599625672291267398 ) ) ;
#201668 = LINE ( 'NONE', #71671, #180686 ) ;
#201669 = CARTESIAN_POINT ( 'NONE',  ( 8.398386088661320414, 11.88553530582519357, -1.199719254218446718 ) ) ;
#201670 = CARTESIAN_POINT ( 'NONE',  ( 5.975483201341563522, 6.103571115010600678, 0.6665044388154163224 ) ) ;
#201671 = CARTESIAN_POINT ( 'NONE',  ( 0.2331563151865486683, 2.034376611827843906, -2.362208330281903024 ) ) ;
#201672 = AXIS2_PLACEMENT_3D ( 'NONE', #23462, #9367, #26678 ) ;
#201673 = CARTESIAN_POINT ( 'NONE',  ( 7.147083253059300922, 8.367293879104554577, 1.199719254218452935 ) ) ;
#201674 = DIRECTION ( 'NONE',  ( 0.000000000000000000, 1.000000000000000000, 0.000000000000000000 ) ) ;
#201675 = CARTESIAN_POINT ( 'NONE',  ( 4.019992336727182369, -0.9402185374879183932, -1.564826772493657536 ) ) ;
#201676 = CARTESIAN_POINT ( 'NONE',  ( -2.428612866367529932E-14, 2.999999999999999112, 2.420000000000000373 ) ) ;
#201677 = CARTESIAN_POINT ( 'NONE',  ( -9.178506806771670412, 9.810605484096178941, 1.040834085586084257E-14 ) ) ;
#201678 =( BOUNDED_SURFACE ( )  B_SPLINE_SURFACE ( 3, 2, ( 
 ( #187975, #191168, #141423 ),
 ( #105705, #140341, #174962 ),
 ( #139252, #42835, #40689 ),
 ( #106792, #24392, #206359 ),
 ( #57986, #26544, #124149 ),
 ( #41764, #173903, #25478 ),
 ( #137118, #91585, #157637 ),
 ( #9235, #207429, #71005 ),
 ( #59048, #108941, #180278 ),
 ( #210631, #192233, #128418 ),
 ( #112149, #62257, #60117 ),
 ( #64391, #160827, #95851 ),
 ( #63322, #126276, #13494 ),
 ( #145688, #129483, #92652 ),
 ( #28693, #142473, #46028 ),
 ( #194385, #127348, #162970 ),
 ( #158694, #178151, #193317 ),
 ( #27615, #161907, #61188 ),
 ( #79569, #29766, #48169 ),
 ( #111071, #93715, #211686 ),
 ( #177077, #159756, #195465 ),
 ( #179217, #12419, #11353 ),
 ( #113212, #94779, #77434 ),
 ( #78499, #144616, #47096 ),
 ( #43896, #30842, #96919 ),
 ( #110010, #176023, #14550 ),
 ( #80646, #146738, #212756 ),
 ( #130535, #143551, #196526 ),
 ( #114282, #10292, #76366 ),
 ( #209545, #44963, #208481 ),
 ( #149913, #69689, #16677 ),
 ( #201817, #118529, #197573 ),
 ( #15613, #100084, #135793 ),
 ( #148835, #119599, #116391 ),
 ( #51339, #32956, #99031 ),
 ( #97979, #18808, #2546 ),
 ( #213800, #83820, #407 ),
 ( #134744, #165086, #49217 ) ),
 .UNSPECIFIED., .F., .F., .T. ) 
 B_SPLINE_SURFACE_WITH_KNOTS ( ( 4, 2, 2, 2, 2, 2, 2, 2, 2, 2, 2, 2, 2, 2, 2, 2, 2, 2, 4 ),
 ( 3, 3 ),
 ( -6.071532165918824830E-18, 0.001328702784605519409, 0.002657405569211044889, 0.003986108353816570152, 0.005314811138422095849, 0.005979162530724858697, 0.006643513923027621546, 0.007972216707633147242, 0.009300919492238671205, 0.01062962227684419690, 0.01129397366914695888, 0.01195832506144972260, 0.01328702784605524656, 0.01461573063066077226, 0.01594443341526629795, 0.01727313619987182192, 0.01860183898447734935, 0.01993054176908287678, 0.02125924455368840074 ),
 ( 0.000000000000000000, 1.000000000000000000 ),
 .UNSPECIFIED. ) 
 GEOMETRIC_REPRESENTATION_ITEM ( )  RATIONAL_B_SPLINE_SURFACE ( (
 ( 1.000000000000000000, 0.8435444081808770589, 1.000000000000000000),
 ( 1.000000000000000000, 0.8432483325082756886, 1.000000000000000000),
 ( 1.000000000000000000, 0.8427406575464768679, 1.000000000000000000),
 ( 1.000000000000000000, 0.8410405345067828442, 1.000000000000000000),
 ( 1.000000000000000000, 0.8398681797021982920, 1.000000000000000000),
 ( 1.000000000000000000, 0.8370024961260722485, 1.000000000000000000),
 ( 1.000000000000000000, 0.8353284867502276390, 1.000000000000000000),
 ( 1.000000000000000000, 0.8314541250028352204, 1.000000000000000000),
 ( 1.000000000000000000, 0.8292703529264303652, 1.000000000000000000),
 ( 1.000000000000000000, 0.8250608724160720664, 1.000000000000000000),
 ( 1.000000000000000000, 0.8247076902036051260, 1.000000000000000000),
 ( 1.000000000000000000, 0.8254996870500060924, 1.000000000000000000),
 ( 1.000000000000000000, 0.8265215800901872800, 1.000000000000000000),
 ( 1.000000000000000000, 0.8285699112141275968, 1.000000000000000000),
 ( 1.000000000000000000, 0.8294744577800686747, 1.000000000000000000),
 ( 1.000000000000000000, 0.8313365137719098685, 1.000000000000000000),
 ( 1.000000000000000000, 0.8318058077052401522, 1.000000000000000000),
 ( 1.000000000000000000, 0.8328176945125120856, 1.000000000000000000),
 ( 1.000000000000000000, 0.8334056329371573035, 1.000000000000000000),
 ( 1.000000000000000000, 0.8334130558649108789, 1.000000000000000000),
 ( 1.000000000000000000, 0.8331786830936150912, 1.000000000000000000),
 ( 1.000000000000000000, 0.8326565767077455105, 1.000000000000000000),
 ( 1.000000000000000000, 0.8323703136855602480, 1.000000000000000000),
 ( 1.000000000000000000, 0.8316300192767074329, 1.000000000000000000),
 ( 1.000000000000000000, 0.8314051384442139314, 1.000000000000000000),
 ( 1.000000000000000000, 0.8294588192946742433, 1.000000000000000000),
 ( 1.000000000000000000, 0.8281603792329889080, 1.000000000000000000),
 ( 1.000000000000000000, 0.8254551073024104513, 1.000000000000000000),
 ( 1.000000000000000000, 0.8237213491650171582, 1.000000000000000000),
 ( 1.000000000000000000, 0.8292902593114940268, 1.000000000000000000),
 ( 1.000000000000000000, 0.8313446087002768214, 1.000000000000000000),
 ( 1.000000000000000000, 0.8350647946855377368, 1.000000000000000000),
 ( 1.000000000000000000, 0.8366996347242240395, 1.000000000000000000),
 ( 1.000000000000000000, 0.8395672446973311276, 1.000000000000000000),
 ( 1.000000000000000000, 0.8407915391627092117, 1.000000000000000000),
 ( 1.000000000000000000, 0.8426130235641089428, 1.000000000000000000),
 ( 1.000000000000000000, 0.8431855836768197276, 1.000000000000000000),
 ( 1.000000000000000000, 0.8434758251109458760, 1.000000000000000000) ) ) 
 REPRESENTATION_ITEM ( '' )  SURFACE ( )  );
#201679 = CARTESIAN_POINT ( 'NONE',  ( -4.749858536263919184, 8.300932276130108534, 0.7929127856809523589 ) ) ;
#201680 = DIRECTION ( 'NONE',  ( -0.000000000000000000, 1.000000000000000000, -0.000000000000000000 ) ) ;
#201681 = CARTESIAN_POINT ( 'NONE',  ( 5.067206508511894469, 0.1826785619755930679, -1.861722072867748823 ) ) ;
#201682 = CARTESIAN_POINT ( 'NONE',  ( 7.076466111328892694, 10.34329533227067799, -1.199719254218441611 ) ) ;
#201684 = EDGE_CURVE ( 'NONE', #178508, #94234, #50387, .T. ) ;
#201683 = CARTESIAN_POINT ( 'NONE',  ( 2.631371740967450634, -1.797512724518410598, 0.6935160474876176373 ) ) ;
#201685 = CARTESIAN_POINT ( 'NONE',  ( 6.262552437187629550, -0.7028992384056665932, -1.831702256219314151 ) ) ;
#201686 = CARTESIAN_POINT ( 'NONE',  ( 4.729096653068339151, 4.411700938201493116, -0.7998128361456211532 ) ) ;
#201687 = CARTESIAN_POINT ( 'NONE',  ( -8.012344526598182026E-15, 9.359375000341399797, -1.575800808251669460 ) ) ;
#201688 = CARTESIAN_POINT ( 'NONE',  ( -7.061099074618889304, 7.132370430010492868, -0.7998128361456291469 ) ) ;
#201689 = CARTESIAN_POINT ( 'NONE',  ( 3.684065054611349144, 5.321161868511784299, -1.599625672291262513 ) ) ;
#201690 = CARTESIAN_POINT ( 'NONE',  ( -3.323157048681004699, 6.891117300187535655, -0.7216878364870458196 ) ) ;
#201691 = AXIS2_PLACEMENT_3D ( 'NONE', #32367, #63790, #46491 ) ;
#201692 = AXIS2_PLACEMENT_3D ( 'NONE', #102650, #71182, #37643 ) ;
#201693 = CARTESIAN_POINT ( 'NONE',  ( 1.740021635027885649, 2.111287947816307575, -0.1595968877764943616 ) ) ;
#201694 = DIRECTION ( 'NONE',  ( 4.440892098500630106E-16, 3.330669073875473073E-16, 1.000000000000000000 ) ) ;
#201696 = ADVANCED_FACE ( 'NONE', ( #151102 ), #157972, .T. ) ;
#201695 = CARTESIAN_POINT ( 'NONE',  ( 0.2517284219400194867, 6.998906413027644824, 3.965208550724196090 ) ) ;
#201697 = CARTESIAN_POINT ( 'NONE',  ( 6.086797785588474063, 1.993605056338519699, 0.5577928598018768724 ) ) ;
#201699 = CARTESIAN_POINT ( 'NONE',  ( 4.184706906298553797, 7.590773377710720915, -0.8858016571234141878 ) ) ;
#201698 = CARTESIAN_POINT ( 'NONE',  ( -0.02423404108400224743, -1.785672699080865788, -0.4486397487279417118 ) ) ;
#201700 = CARTESIAN_POINT ( 'NONE',  ( 6.381448165025822128, -0.6081200552338487109, -2.216719476268604438 ) ) ;
#201701 = CARTESIAN_POINT ( 'NONE',  ( 5.016153647376196290, 8.796003655340152605, 0.7216878364870438212 ) ) ;
#201702 = CARTESIAN_POINT ( 'NONE',  ( 4.909461021924254709, 5.860697626067345567, 1.082531754730549078 ) ) ;
#201703 = CARTESIAN_POINT ( 'NONE',  ( 1.394904949290655116, 1.871713452925367616, -1.323071089866036276 ) ) ;
#201704 = CARTESIAN_POINT ( 'NONE',  ( 7.785697387528199762E-15, 0.4375000000000076605, -1.225000000000032951 ) ) ;
#201705 = CARTESIAN_POINT ( 'NONE',  ( -7.096767062110449942, 7.244259425409119046, -0.7998128361456362523 ) ) ;
#201706 = ADVANCED_FACE ( 'NONE', ( #187836 ), #139112, .F. ) ;
#201707 = CARTESIAN_POINT ( 'NONE',  ( 6.122988667457554435, -1.827782563270570648, 0.6563872640158885385 ) ) ;
#201708 = ORIENTED_EDGE ( 'NONE', *, *, #115282, .T. ) ;
#201709 = CARTESIAN_POINT ( 'NONE',  ( 6.927853306458731986, 11.02631992426980112, 0.7216878364870438212 ) ) ;
#201710 = AXIS2_PLACEMENT_3D ( 'NONE', #105085, #159142, #10744 ) ;
#201711 = CARTESIAN_POINT ( 'NONE',  ( 0.3869771421881840201, -1.897093440144840937, -0.6742409396158774992 ) ) ;
#201712 = LINE ( 'NONE', #17627, #154959 ) ;
#201714 = CARTESIAN_POINT ( 'NONE',  ( -15.75000000000000000, 10.89999999999998259, 3.199999999999997957 ) ) ;
#201713 = CARTESIAN_POINT ( 'NONE',  ( -8.178592977541617515, 10.56477777859713463, 1.599625672291295375 ) ) ;
#201715 = CARTESIAN_POINT ( 'NONE',  ( 3.285556943750000070, -0.3718749995220427262, 0.000000000000000000 ) ) ;
#201717 = CARTESIAN_POINT ( 'NONE',  ( 0.9359865740741512008, 1.742660192269055663, 0.3080425777817352162 ) ) ;
#201716 = CARTESIAN_POINT ( 'NONE',  ( 2.871125768194443761, 1.984923283205226818, -0.6565763796619171755 ) ) ;
#201718 = LINE ( 'NONE', #24045, #181961 ) ;
#201720 = CARTESIAN_POINT ( 'NONE',  ( 4.136908408643169111, -1.995281682711878668, 1.128303315244700178 ) ) ;
#201719 = CARTESIAN_POINT ( 'NONE',  ( 4.248501033035879004, 6.049946853332221153, -1.599625672291273171 ) ) ;
#201721 = CARTESIAN_POINT ( 'NONE',  ( 3.081702191724482454, -1.714667182045168214, -0.2967042344550906985 ) ) ;
#201722 = VECTOR ( 'NONE', #104789, 1000.000000000000000 ) ;
#201723 = CARTESIAN_POINT ( 'NONE',  ( 3.297657676621871925, 4.870353260857385180, 1.599625672291267398 ) ) ;
#201724 = CARTESIAN_POINT ( 'NONE',  ( -10.95308175811721085, 11.29999999999999893, -1.800000000000001155 ) ) ;
#201725 = CARTESIAN_POINT ( 'NONE',  ( 3.461945267817592597, 1.365228559796902719, 1.068630620724864588 ) ) ;
#201726 = CARTESIAN_POINT ( 'NONE',  ( 4.123599099448671090, 0.2696675481538573504, -2.154320840723603414 ) ) ;
#201727 = CARTESIAN_POINT ( 'NONE',  ( 4.147904930777053245, 6.926640621626830807, -1.199719254218452047 ) ) ;
#201728 = CARTESIAN_POINT ( 'NONE',  ( 4.944546133779973651, -1.457238331152037825, 1.394083050251286870 ) ) ;
#201729 = CARTESIAN_POINT ( 'NONE',  ( 3.156250000000002665, -1.895863743164019288, 0.7852924748301466362 ) ) ;
#201730 = CARTESIAN_POINT ( 'NONE',  ( -0.7500000000000215383, 4.722916667349482012, 1.299038105676671107 ) ) ;
#201731 = CARTESIAN_POINT ( 'NONE',  ( 1.588762598846172436, -0.2802010128373257913, -1.905785462699102206 ) ) ;
#201732 = CARTESIAN_POINT ( 'NONE',  ( 1.499999999999997113, 8.427083334016133520, -0.8660254037844378194 ) ) ;
#201733 = CARTESIAN_POINT ( 'NONE',  ( 4.588250468535750137, 1.280153277506433707, 1.815263839992816042 ) ) ;
#201734 = ORIENTED_EDGE ( 'NONE', *, *, #7576, .T. ) ;
#201735 = CARTESIAN_POINT ( 'NONE',  ( -0.1110810684432777806, 1.403644835841436400, -2.056232460864733103 ) ) ;
#201736 = CARTESIAN_POINT ( 'NONE',  ( 1.499999999999987121, 1.754166666666691521, 0.8660254037844524744 ) ) ;
#201737 = CARTESIAN_POINT ( 'NONE',  ( 6.908042961362778733, 8.018137195466769285, 1.199719254218462483 ) ) ;
#201738 = CARTESIAN_POINT ( 'NONE',  ( 3.660338285565247762, 7.214219066560688454, 1.040834085586084257E-14 ) ) ;
#201739 = CARTESIAN_POINT ( 'NONE',  ( -1.642778471874998480, -2.501041666188707158, 2.845375778867863303 ) ) ;
#201740 = CARTESIAN_POINT ( 'NONE',  ( 1.120143885658178906, -0.5347273011463581360, 2.155877112962206965 ) ) ;
#201741 = CARTESIAN_POINT ( 'NONE',  ( 5.775826483351648832, -1.914393393812302113, 0.4282712878391075062 ) ) ;
#201742 = CARTESIAN_POINT ( 'NONE',  ( 8.975134502566660899, 10.53370701015836275, -1.082531754730543083 ) ) ;
#201743 = CARTESIAN_POINT ( 'NONE',  ( 6.819576192995205233, -2.197070018990463502, 0.5395731105267542738 ) ) ;
#201744 = CARTESIAN_POINT ( 'NONE',  ( 3.867818961648523235, 7.734482231890414283, 1.040834085586084257E-14 ) ) ;
#201745 = CARTESIAN_POINT ( 'NONE',  ( -4.746763178560296836, 6.631252689777363152, 1.443375672974058777 ) ) ;
#201746 = CARTESIAN_POINT ( 'NONE',  ( 3.437984354829794142, 1.306305779046763149, 1.596332929251530253 ) ) ;
#201747 = CARTESIAN_POINT ( 'NONE',  ( -5.229694566569281555, 7.124396299129368337, 1.599625672291267398 ) ) ;
#201748 = CARTESIAN_POINT ( 'NONE',  ( -1.201851678989727383E-14, 3.493750000682815493, 1.732050807568877637 ) ) ;
#201749 = CARTESIAN_POINT ( 'NONE',  ( -1.364683531250010295, 5.342708333674750953, 0.7879004041258379498 ) ) ;
#201750 = CARTESIAN_POINT ( 'NONE',  ( 5.923093557443566581, -0.04637014295935313474, 1.870147476527424635 ) ) ;
#201751 = CARTESIAN_POINT ( 'NONE',  ( 4.430095426116970714, -1.344173880920132458, -1.095666204706043700 ) ) ;
#201752 = CARTESIAN_POINT ( 'NONE',  ( 3.509068237933731016, -1.713987098263862086, 0.3013083454645076875 ) ) ;
#201753 = CARTESIAN_POINT ( 'NONE',  ( 1.365189820700737577, 0.1628935585381158235, -2.286633867385555519 ) ) ;
#201754 = CARTESIAN_POINT ( 'NONE',  ( 1.364683531249988535, 3.426041667008085323, 0.7879004041258500513 ) ) ;
#201755 = CARTESIAN_POINT ( 'NONE',  ( 6.233939691744167177, 2.068093053085200417, 0.3059697267470474769 ) ) ;
#201756 = CARTESIAN_POINT ( 'NONE',  ( 6.632770897174698810, -1.733374817101345000, 0.8757406700844807546 ) ) ;
#201757 = FACE_OUTER_BOUND ( 'NONE', #130769, .T. ) ;
#201758 =( LENGTH_UNIT ( ) NAMED_UNIT ( * ) SI_UNIT ( .MILLI., .METRE. ) );
#201759 = CARTESIAN_POINT ( 'NONE',  ( 1.442029965644067158, -1.730867108953790590, -1.034163949609874233 ) ) ;
#201760 = CARTESIAN_POINT ( 'NONE',  ( 0.2346725361867564585, 0.3788711812165134196, 2.158297013397599162 ) ) ;
#201761 = CARTESIAN_POINT ( 'NONE',  ( 9.573135803333604699, 13.80976963840737248, -8.295511852730781399 ) ) ;
#201762 = CARTESIAN_POINT ( 'NONE',  ( -9.040589502214116280, 9.441775928871617651, 0.7998128361456462443 ) ) ;
#201763 = CARTESIAN_POINT ( 'NONE',  ( 6.440286661691305703, 7.472421512516709718, 1.199719254218462483 ) ) ;
#201765 = B_SPLINE_CURVE_WITH_KNOTS ( 'NONE', 3,
 ( #119396, #170207, #4475, #202690, #21791, #54340, #103086, #87900 ),
 .UNSPECIFIED., .F., .F.,
 ( 4, 2, 2, 4 ),
 ( 0.000000000000000000, 0.0002034531274099171216, 0.0004069062548198347853, 0.0008138125096396682696 ),
 .UNSPECIFIED. ) ;
#201764 = CARTESIAN_POINT ( 'NONE',  ( 2.877707679121459527, 0.3088738507561124003, -2.097740099398600400 ) ) ;
#201766 = CARTESIAN_POINT ( 'NONE',  ( 4.787437623848783907, 6.678706240755900581, -1.249999999999999334 ) ) ;
#201767 = CARTESIAN_POINT ( 'NONE',  ( 5.602125774977974260, -1.825872481414937853, 0.004271240736861136277 ) ) ;
#201768 = ORIENTED_EDGE ( 'NONE', *, *, #177985, .F. ) ;
#201769 = CARTESIAN_POINT ( 'NONE',  ( -7.065734331377342414, 8.272386803808890576, -1.199719254218452047 ) ) ;
#201770 = EDGE_CURVE ( 'NONE', #28948, #60914, #12430, .T. ) ;
#201771 = CYLINDRICAL_SURFACE ( 'NONE', #143924, 0.09999999999999982514 ) ;
#201772 = CARTESIAN_POINT ( 'NONE',  ( -3.475000000000000533, -4.185416665710754103, -2.006292185433948827 ) ) ;
#201773 = CARTESIAN_POINT ( 'NONE',  ( -6.157374318900681764, 10.33535380535947290, 0.7998128361456481317 ) ) ;
#201774 = CARTESIAN_POINT ( 'NONE',  ( 1.652609354460622626, 1.998416004623180697, 0.2920258124684270706 ) ) ;
#201775 = CARTESIAN_POINT ( 'NONE',  ( 0.5168062790325059774, 1.452128344422070283, -1.525477944039640432 ) ) ;
#201776 = CARTESIAN_POINT ( 'NONE',  ( 10.56588178375152864, 11.22128359066528169, -0.7998128361456281477 ) ) ;
#201777 = CARTESIAN_POINT ( 'NONE',  ( 4.100341000477321529, 1.851659804611929472, 0.1859286059659806256 ) ) ;
#201778 = CARTESIAN_POINT ( 'NONE',  ( 9.185812768458653466, 10.67553530374532045, 1.199719254218453823 ) ) ;
#201779 = CARTESIAN_POINT ( 'NONE',  ( 11.94655611907589865, 13.65200944546904083, -1.134828163062138628 ) ) ;
#201780 = CARTESIAN_POINT ( 'NONE',  ( -4.939248034080176097, 4.656877549381960080, 1.214306433183764966E-14 ) ) ;
#201781 = CARTESIAN_POINT ( 'NONE',  ( -8.830438121202295321, 9.196599317691152464, -0.7998128361456291469 ) ) ;
#201782 = CARTESIAN_POINT ( 'NONE',  ( 5.022008369909983116, -0.9795521577263366364, -1.540466923627185292 ) ) ;
#201783 = CIRCLE ( 'NONE', #115300, 10.99999999999738698 ) ;
#201785 = CARTESIAN_POINT ( 'NONE',  ( -3.975603406396657213, 7.849426279905078019, -0.02588959144292704573 ) ) ;
#201784 = CARTESIAN_POINT ( 'NONE',  ( -7.611976899429754084, 7.845337568948314022, 0.7998128361456341429 ) ) ;
#201786 = CARTESIAN_POINT ( 'NONE',  ( 1.364683531249986537, -0.8447916663252468261, -0.7879004041258309554 ) ) ;
#201787 = CARTESIAN_POINT ( 'NONE',  ( 2.002904151241869712, 1.714182390810105927, 0.2594085799107764823 ) ) ;
#201788 = CARTESIAN_POINT ( 'NONE',  ( 6.456982894382444549, 0.3095715517048603371, -1.814770079682447967 ) ) ;
#201790 = CARTESIAN_POINT ( 'NONE',  ( 8.595506201384013778, 10.09080732544527592, 1.082531754730558626 ) ) ;
#201789 = CARTESIAN_POINT ( 'NONE',  ( 5.110162711920646750, -2.297000869944005430, 0.2220405423442091408 ) ) ;
#201791 = CARTESIAN_POINT ( 'NONE',  ( -10.60630082101195804, 5.715768461961713953, -4.896526734066639186 ) ) ;
#201792 = CARTESIAN_POINT ( 'NONE',  ( 1.141951006405941715, 0.8376953415718463303, -1.883039458060199900 ) ) ;
#201793 = EDGE_CURVE ( 'NONE', #45587, #322, #35849, .T. ) ;
#201794 = CARTESIAN_POINT ( 'NONE',  ( 6.450549897212096262, 1.577601184540510681, 1.671684124095852653 ) ) ;
#201795 = CARTESIAN_POINT ( 'NONE',  ( 1.278248824818062671E-15, 1.062499999999996003, 1.224999999999968781 ) ) ;
#201796 = CARTESIAN_POINT ( 'NONE',  ( -5.855142236255304944, 7.924361590421551860, -1.599625672291271394 ) ) ;
#201797 = CARTESIAN_POINT ( 'NONE',  ( 6.596569749568344854, -0.5012203084251048990, -1.802199723311518786 ) ) ;
#201799 = CARTESIAN_POINT ( 'NONE',  ( -3.447516199624892419, 7.244129009529488350, 0.7998128361456352531 ) ) ;
#201798 = CARTESIAN_POINT ( 'NONE',  ( 3.550944491985886575, 0.2853618425060593378, 1.890879049853078087 ) ) ;
#201800 = CARTESIAN_POINT ( 'NONE',  ( 4.653060005753134831, -1.773635849817876586, 1.313014255023836618 ) ) ;
#201801 = CARTESIAN_POINT ( 'NONE',  ( -0.6124999999999984901, 2.354166667349471886, 1.060881119635896264 ) ) ;
#201802 = CARTESIAN_POINT ( 'NONE',  ( -6.061904078641520144, 10.08632216847484031, 0.7216878364870267237 ) ) ;
#201803 = CARTESIAN_POINT ( 'NONE',  ( 4.001064729364292916, 6.721640380016713934, -1.082531754730548412 ) ) ;
#201804 = CARTESIAN_POINT ( 'NONE',  ( -8.106849506328558164, 8.422688943663599659, 0.000000000000000000 ) ) ;
#201805 = CARTESIAN_POINT ( 'NONE',  ( 6.059260758684835046, -1.791542317298041365, 1.134111293253435182 ) ) ;
#201806 = VERTEX_POINT ( 'NONE', #56783 ) ;
#201807 = CARTESIAN_POINT ( 'NONE',  ( 3.434905211628926480, 2.250879548190734436, 0.5077644651142860788 ) ) ;
#201808 = CARTESIAN_POINT ( 'NONE',  ( 4.246505328441081417, -1.940195102956907336, -0.2900488188990399396 ) ) ;
#201809 = CARTESIAN_POINT ( 'NONE',  ( 0.6726124357511429341, 1.356994209013298036, -1.416925378234991095 ) ) ;
#201810 = CARTESIAN_POINT ( 'NONE',  ( 7.185352960343817763, 15.44063983605676604, 9.557346848789475047 ) ) ;
#201811 = CARTESIAN_POINT ( 'NONE',  ( 6.770610912236886492, -7.154544010627095219, 6.663994888585879295 ) ) ;
#201812 = ORIENTED_EDGE ( 'NONE', *, *, #9881, .T. ) ;
#201813 = CARTESIAN_POINT ( 'NONE',  ( 6.210172754313918908, 1.157103754073171675, -1.651340222398114843 ) ) ;
#201814 = CARTESIAN_POINT ( 'NONE',  ( -9.481229494658258261, 9.955855920056455588, -0.7998128361456291469 ) ) ;
#201815 = DIRECTION ( 'NONE',  ( 0.000000000000000000, 0.1994302930878473212, -0.9799120155396071619 ) ) ;
#201816 = CARTESIAN_POINT ( 'NONE',  ( 2.764704757504053756, -0.8271204958998740198, -2.007528505447711886 ) ) ;
#201817 = CARTESIAN_POINT ( 'NONE',  ( 10.35141017034361788, 10.47591664987898241, -5.982769973146199405 ) ) ;
#201818 = CARTESIAN_POINT ( 'NONE',  ( 0.6508261300204335464, 2.090236094481153550, 0.3566229023672163878 ) ) ;
#201819 = CARTESIAN_POINT ( 'NONE',  ( -1.500000000000013101, 1.410416667349486008, -0.8660254037844313801 ) ) ;
#201820 = CARTESIAN_POINT ( 'NONE',  ( 8.353795204314554468, 12.89784483834236184, -0.7998128361456352531 ) ) ;
#201821 = CARTESIAN_POINT ( 'NONE',  ( 0.2653090297881668391, 2.688473650299893158, -2.056485102041657242 ) ) ;
#201822 = CARTESIAN_POINT ( 'NONE',  ( 6.344829475870412239, 6.940264737885684987, 0.8615092103797560297 ) ) ;
#201823 = CARTESIAN_POINT ( 'NONE',  ( 1.651711298185059684, 0.6011997390959940013, -1.971106496394055885 ) ) ;
#201825 = CARTESIAN_POINT ( 'NONE',  ( -7.034482758620708154, 5.227586206896615018, 1.300454001123785972E-14 ) ) ;
#201824 = CARTESIAN_POINT ( 'NONE',  ( -8.642432853707342488, 12.17025653171218558, 1.199719254218462483 ) ) ;
#201826 = CARTESIAN_POINT ( 'NONE',  ( 1.364683531249988535, 2.363541667008088432, 0.7879004041258500513 ) ) ;
#201827 = CARTESIAN_POINT ( 'NONE',  ( -2.788906526875773208E-15, 9.187500000000001776, -1.499999999999998446 ) ) ;
#201828 = ORIENTED_EDGE ( 'NONE', *, *, #87019, .F. ) ;
#201829 = CARTESIAN_POINT ( 'NONE',  ( 4.811142580195256535, 1.587781804131962682, -1.065416552848017062 ) ) ;
#201830 = CARTESIAN_POINT ( 'NONE',  ( 2.958220528980558761, -1.197304571117228100, 1.622486353517027968 ) ) ;
#201831 = CARTESIAN_POINT ( 'NONE',  ( 11.80247861663003484, 9.799999999999984723, 1.695431928471866190 ) ) ;
#201832 = CARTESIAN_POINT ( 'NONE',  ( -2.605138072120212200, 6.191078184115536232, -0.7998128361456281477 ) ) ;
#201833 = CARTESIAN_POINT ( 'NONE',  ( -0.1231740688493014324, -1.618022042794277748, -0.8147913963296258277 ) ) ;
#201835 = CARTESIAN_POINT ( 'NONE',  ( 0.3213152726999657927, -1.356817153130492004, -1.352679412961822925 ) ) ;
#201834 = CARTESIAN_POINT ( 'NONE',  ( 7.346809171966453889, -6.836568542494980250, 8.002408263930263388 ) ) ;
#201836 = CARTESIAN_POINT ( 'NONE',  ( 1.961466609329724164, 1.720096886549182136, 1.151944459977225055 ) ) ;
#201837 = CARTESIAN_POINT ( 'NONE',  ( 1.364683531249986537, 0.4260416670080872659, 0.7879004041258500513 ) ) ;
#201838 = CARTESIAN_POINT ( 'NONE',  ( 0.4968692282744023303, 1.640418903650592508, -1.093199247851096789 ) ) ;
#201839 = CARTESIAN_POINT ( 'NONE',  ( 3.141029808440584326, -1.609794727316344209, 0.8612202190056221784 ) ) ;
#201840 = EDGE_CURVE ( 'NONE', #103541, #95942, #87144, .T. ) ;
#201842 = CARTESIAN_POINT ( 'NONE',  ( 5.825676364550436581, 7.207913871576331566, 1.168708750232345883 ) ) ;
#201841 = CARTESIAN_POINT ( 'NONE',  ( 0.04808971849027363077, -1.788275647358487985, -1.458162290246179715 ) ) ;
#201843 = CARTESIAN_POINT ( 'NONE',  ( 0.6823417656249899377, 1.342708333674752508, 1.181850606188755259 ) ) ;
#201844 = CARTESIAN_POINT ( 'NONE',  ( 3.789554774376595159, -1.906935327315992579, 0.7867413014382127479 ) ) ;
#201846 = CARTESIAN_POINT ( 'NONE',  ( -6.632963465583701534, 8.761543347979550589, -1.599625672291263179 ) ) ;
#201845 = PRESENTATION_LAYER_ASSIGNMENT (  '', '', ( #80818 ) ) ;
#201847 = CARTESIAN_POINT ( 'NONE',  ( 8.437251666405968464, 8.737881787095446384, 1.040834085586084257E-14 ) ) ;
#201848 = CARTESIAN_POINT ( 'NONE',  ( 5.379888026524302980, 5.170957540566795352, -0.7998128361456211532 ) ) ;
#201849 = CARTESIAN_POINT ( 'NONE',  ( 5.681030059326015014, 6.586622143090519188, -1.199719254218445830 ) ) ;
#201851 = CARTESIAN_POINT ( 'NONE',  ( 1.499999999999989120, 3.754166666666685082, 0.8660254037844524744 ) ) ;
#201850 = CARTESIAN_POINT ( 'NONE',  ( 5.807678370005410429, -0.5150985282868367765, 2.041858835689168927 ) ) ;
#201852 = CARTESIAN_POINT ( 'NONE',  ( 6.654741963219192868, -0.5482099483974657295, -1.996413779700876301 ) ) ;
#201854 = CARTESIAN_POINT ( 'NONE',  ( -1.364683531250012516, 1.842708333674749843, 0.7879004041258379498 ) ) ;
#201853 = VECTOR ( 'NONE', #196023, 1000.000000000000000 ) ;
#201855 = CARTESIAN_POINT ( 'NONE',  ( 3.725982817344280829, -1.284327275973631277, -1.738548686538298416 ) ) ;
#201856 = CARTESIAN_POINT ( 'NONE',  ( 4.565106334443884251, -1.620744288901782904, 1.204869856736161537 ) ) ;
#201857 = CIRCLE ( 'NONE', #38915, 0.1000000000000000472 ) ;
#201860 = CARTESIAN_POINT ( 'NONE',  ( 5.341549334104184865, 8.215262742221458581, 1.082531754730558626 ) ) ;
#201859 = CARTESIAN_POINT ( 'NONE',  ( -1.642778471875000035, -4.017708332855376874, -2.845375778867859751 ) ) ;
#201858 = CARTESIAN_POINT ( 'NONE',  ( 0.3000000000000016542, 4.000000000000003553, -1.007084189318387502 ) ) ;
#201861 = CARTESIAN_POINT ( 'NONE',  ( -7.117104292530948229, 7.267986194233038155, -0.7998128361456362523 ) ) ;
#201862 = CARTESIAN_POINT ( 'NONE',  ( 2.659388954101277847, 1.913261587491304150, -0.6371546050257800298 ) ) ;
#201863 = CARTESIAN_POINT ( 'NONE',  ( -9.365985188942097750, 9.821404230054264772, 0.7998128361456462443 ) ) ;
#201865 = CARTESIAN_POINT ( 'NONE',  ( -4.271669656942582272, 7.425251299075903866, -1.032879151585558875 ) ) ;
#201864 = CARTESIAN_POINT ( 'NONE',  ( -3.554208825076827782, 7.298327395898266623, 0.7998128361456341429 ) ) ;
#201866 = CARTESIAN_POINT ( 'NONE',  ( 0.000000000000000000, 2.000000000000001776, 0.000000000000000000 ) ) ;
#201868 = CARTESIAN_POINT ( 'NONE',  ( 4.446888776373093322, -1.802426293348384334, -0.9040943451460029534 ) ) ;
#201867 = CARTESIAN_POINT ( 'NONE',  ( -6.033015167956794933, 9.982342096017511324, -0.7216878364870267237 ) ) ;
#201869 = CARTESIAN_POINT ( 'NONE',  ( 1.499999999999989120, 5.545833333333350268, -0.8660254037844323793 ) ) ;
#201870 = CARTESIAN_POINT ( 'NONE',  ( 0.5040132504689893711, -0.5763820916803040761, -1.625860608634047244 ) ) ;
#201871 = CARTESIAN_POINT ( 'NONE',  ( 4.538947565524982686, 8.517465603079630299, 0.000000000000000000 ) ) ;
#201873 = DIRECTION ( 'NONE',  ( 0.000000000000000000, 1.000000000000000000, 0.000000000000000000 ) ) ;
#201872 = CARTESIAN_POINT ( 'NONE',  ( 7.537970219518073556, 9.817384560903001045, -1.443375672974057666 ) ) ;
#201874 = CARTESIAN_POINT ( 'NONE',  ( -10.79501016327925633, 6.383858692899066156, 5.153711710998491569 ) ) ;
#201875 = CARTESIAN_POINT ( 'NONE',  ( 5.413307058180727438, -0.2754873708227522644, 1.850039175317084617 ) ) ;
#201876 = CARTESIAN_POINT ( 'NONE',  ( 6.205343618373656334, 1.749435416034326618, -0.9961562333783975376 ) ) ;
#201877 = CARTESIAN_POINT ( 'NONE',  ( -5.750066545527201534, 9.722511713174800008, 0.000000000000000000 ) ) ;
#201878 = VERTEX_POINT ( 'NONE', #89301 ) ;
#201879 = CARTESIAN_POINT ( 'NONE',  ( 9.531018800282598846, 12.14260790512831889, 1.443375672974076540 ) ) ;
#201880 = CARTESIAN_POINT ( 'NONE',  ( 0.4742327405582689170, -2.001515332587662233, -0.2440062454662216829 ) ) ;
#201881 = CARTESIAN_POINT ( 'NONE',  ( 1.546807606353679754, 0.1796435140209233228, 1.802673299184972322 ) ) ;
#201882 = EDGE_CURVE ( 'NONE', #17720, #77260, #28191, .T. ) ;
#201883 = CARTESIAN_POINT ( 'NONE',  ( 4.706088717274906408, 5.623429937309770921, 1.082531754730549078 ) ) ;
#201884 = CARTESIAN_POINT ( 'NONE',  ( 0.000000000000000000, 8.999999999999998224, 0.000000000000000000 ) ) ;
#201885 = CARTESIAN_POINT ( 'NONE',  ( 6.262976894508937242, 9.394224579314053969, -1.199719254218440723 ) ) ;
#201887 = CARTESIAN_POINT ( 'NONE',  ( 5.993738795899758998, -1.900512161056673088, 0.2395553810000446704 ) ) ;
#201886 = CARTESIAN_POINT ( 'NONE',  ( -4.608882153641705059, 7.464447381635583412, -1.199719254218452047 ) ) ;
#201888 = CARTESIAN_POINT ( 'NONE',  ( -7.334597915313094241, 9.580116872663850813, 1.040834085586084257E-14 ) ) ;
#201889 = CARTESIAN_POINT ( 'NONE',  ( 0.3423093779009768189, 2.999999999999988898, -0.4000000000000409339 ) ) ;
#201890 = CARTESIAN_POINT ( 'NONE',  ( -1.364683531250014514, -1.157291666325248158, 0.7879004041258379498 ) ) ;
#201892 = ORIENTED_EDGE ( 'NONE', *, *, #126245, .T. ) ;
#201891 = CARTESIAN_POINT ( 'NONE',  ( 4.053524740805938720, 3.831459740469437936, 1.214306433183764966E-14 ) ) ;
#201893 = CARTESIAN_POINT ( 'NONE',  ( -4.634189577772691138, 4.300976017023221409, 1.214306433183764966E-14 ) ) ;
#201894 = CARTESIAN_POINT ( 'NONE',  ( 4.188458007013862172, -2.137797052781073237, -0.3198388112101158143 ) ) ;
#201895 = CARTESIAN_POINT ( 'NONE',  ( -6.617788377246193399, 8.814115421577600529, -1.443375672974066548 ) ) ;
#201896 = EDGE_CURVE ( 'NONE', #15498, #106354, #196308, .T. ) ;
#201897 = CARTESIAN_POINT ( 'NONE',  ( 6.699137298928158124, 6.988284068270579574, 0.7216878364870328300 ) ) ;
#201898 = CARTESIAN_POINT ( 'NONE',  ( 0.2992908618118708675, -0.2657624787030036240, -2.103842954668332599 ) ) ;
#201899 = CARTESIAN_POINT ( 'NONE',  ( 5.543921259432438298, 0.7380120197021734496, -1.669944898041133774 ) ) ;
#201900 = CARTESIAN_POINT ( 'NONE',  ( 2.653541938639871756, 0.5291849669812850321, -1.898919477364902741 ) ) ;
#201901 = CARTESIAN_POINT ( 'NONE',  ( 4.201352949932454450, 1.705870964349815333, -0.8646410313453978258 ) ) ;
#201902 = VERTEX_POINT ( 'NONE', #121865 ) ;
#201903 = CARTESIAN_POINT ( 'NONE',  ( 4.367134876933267407, 8.109091433148536865, 0.000000000000000000 ) ) ;
#201904 = CARTESIAN_POINT ( 'NONE',  ( 6.057084849134293236, 1.611049215779712940, -1.132701646639628246 ) ) ;
#201905 = CARTESIAN_POINT ( 'NONE',  ( 0.4802856102240244951, -0.2370191179813440352, -1.927374317010506877 ) ) ;
#201906 = ORIENTED_EDGE ( 'NONE', *, *, #176811, .T. ) ;
#201907 = CARTESIAN_POINT ( 'NONE',  ( -3.800028193580205382, 7.655393002477360653, -0.7998128361456481317 ) ) ;
#201908 = CARTESIAN_POINT ( 'NONE',  ( -3.902768115887413014, 5.646591783325653147, -1.599625672291283607 ) ) ;
#201910 = CARTESIAN_POINT ( 'NONE',  ( 7.146556367734776316, 7.510272981878305387, 0.7216878364870267237 ) ) ;
#201909 = CARTESIAN_POINT ( 'NONE',  ( 6.936968151686458306, 11.24487994360957188, 0.7998128361456462443 ) ) ;
#201912 = VERTEX_POINT ( 'NONE', #136979 ) ;
#201911 = CARTESIAN_POINT ( 'NONE',  ( 4.846305138012901637, 0.9798207982155520135, -1.642033262021398654 ) ) ;
#201913 = CARTESIAN_POINT ( 'NONE',  ( 0.3939699847536023980, 1.636818068892214262, 1.480257586202008646 ) ) ;
#201914 = CARTESIAN_POINT ( 'NONE',  ( 1.499999999999990452, 8.654128368560188633, 2.562285273914694184 ) ) ;
#201915 = CARTESIAN_POINT ( 'NONE',  ( 0.1176276963383571517, -0.5100272734060510293, 1.842954807014775653 ) ) ;
#201917 = AXIS2_PLACEMENT_3D ( 'NONE', #12000, #61832, #78075 ) ;
#201916 = CARTESIAN_POINT ( 'NONE',  ( -0.02319159430947368913, 6.948789054712430691, -2.406029888528108618 ) ) ;
#201918 = CARTESIAN_POINT ( 'NONE',  ( -0.02978472384952053284, 15.46795719462065577, 11.98291739243534160 ) ) ;
#201919 = CARTESIAN_POINT ( 'NONE',  ( -6.392587740394331419, -6.532648833121162291, -6.999862025036984292 ) ) ;
#201920 = CARTESIAN_POINT ( 'NONE',  ( 2.770052221688572125, -2.048192801557855436, 0.3012726569043902569 ) ) ;
#201921 = CARTESIAN_POINT ( 'NONE',  ( -6.410307701162927252, 6.373113827645189744, -0.7998128361456291469 ) ) ;
#201922 = CARTESIAN_POINT ( 'NONE',  ( -4.603364586660168456, 8.384938909114524108, 0.004600842637982396899 ) ) ;
#201924 = CARTESIAN_POINT ( 'NONE',  ( 0.07536363704235826688, -0.001874865094115066300, -2.144269471569634877 ) ) ;
#201923 = CARTESIAN_POINT ( 'NONE',  ( -2.916975605234527702, 6.554888639415577423, 1.040834085586084257E-14 ) ) ;
#201925 = PLANE ( 'NONE',  #17305 ) ;
#201926 = CARTESIAN_POINT ( 'NONE',  ( -5.514013019825418915, 5.994650414344389056, -0.9619886414689113874 ) ) ;
#201927 = CARTESIAN_POINT ( 'NONE',  ( 0.6823417656249969321, 13.58854166700806942, -1.181850606188757036 ) ) ;
#201928 = CARTESIAN_POINT ( 'NONE',  ( -6.805266759416629618, 6.904175738932996964, 0.000000000000000000 ) ) ;
#201929 = CARTESIAN_POINT ( 'NONE',  ( 5.695915039874445362, 1.533740007788013449, 0.8092579662780824412 ) ) ;
#201930 = CARTESIAN_POINT ( 'NONE',  ( -2.903417451620861289, 6.539070793532962611, 0.7998128361456341429 ) ) ;
#201931 = CARTESIAN_POINT ( 'NONE',  ( 3.555589372526322123, 1.629040189086952362, 1.277421477176057474 ) ) ;
#201932 = CARTESIAN_POINT ( 'NONE',  ( 4.271193901148872207, 1.890388351848461657, -0.9536453560208182356 ) ) ;
#201933 = CARTESIAN_POINT ( 'NONE',  ( 5.126954644262057492, 9.133197518281081173, 0.7998128361456462443 ) ) ;
#201935 = EDGE_CURVE ( 'NONE', #193490, #17518, #154794, .T. ) ;
#201934 = CARTESIAN_POINT ( 'NONE',  ( -0.6823417656250212460, 4.801041667008086655, 1.181850606188767472 ) ) ;
#201936 = CARTESIAN_POINT ( 'NONE',  ( 2.764455286864405004, -0.7492524419267130309, -1.821560881719074709 ) ) ;
#201937 = CARTESIAN_POINT ( 'NONE',  ( 1.072351618572921605, 0.7776387867773439933, 1.747342548420704800 ) ) ;
#201938 = CARTESIAN_POINT ( 'NONE',  ( 4.681715291062889861, -1.083280430520225046, 2.020132927424389102 ) ) ;
#201939 = CARTESIAN_POINT ( 'NONE',  ( 3.228933428962964758, 0.04559371896543929631, 1.825288036790246204 ) ) ;
#201940 = EDGE_CURVE ( 'NONE', #209056, #198860, #180491, .T. ) ;
#201941 = CARTESIAN_POINT ( 'NONE',  ( 4.960304097753311936, 6.880383762169266504, 1.599625672291268286 ) ) ;
#201942 = CARTESIAN_POINT ( 'NONE',  ( 6.778713616708431644, 7.010846762355714468, 1.040834085586084257E-14 ) ) ;
#201943 = CARTESIAN_POINT ( 'NONE',  ( -7.393273838153706201, 7.519907654134449615, 0.7998128361456341429 ) ) ;
#201944 = CARTESIAN_POINT ( 'NONE',  ( 3.937747632521654495, -1.925297015496162611, 0.5883167919090799280 ) ) ;
#201945 = CARTESIAN_POINT ( 'NONE',  ( 3.239059677355364375, -0.1396402669299641186, -1.956817938210092089 ) ) ;
#201946 = CARTESIAN_POINT ( 'NONE',  ( -8.206763054973658100, 8.468978407091068306, 0.7998128361456602331 ) ) ;
#201947 = CARTESIAN_POINT ( 'NONE',  ( -5.087333953625788219, 6.958308917361963886, 1.599625672291267398 ) ) ;
#201948 = CYLINDRICAL_SURFACE ( 'NONE', #78324, 1.250000000000000000 ) ;
#201950 = CARTESIAN_POINT ( 'NONE',  ( 5.155052684544634722, -1.496415494590461748, -0.9447146595812674352 ) ) ;
#201949 = CARTESIAN_POINT ( 'NONE',  ( 6.263634082940216175, 1.073540726731788908, 1.793809194602818735 ) ) ;
#201951 = DIRECTION ( 'NONE',  ( 1.014813233446432150E-15, 1.000000000000000000, -4.583713267641621330E-32 ) ) ;
#201952 = CARTESIAN_POINT ( 'NONE',  ( 2.168174125648382411, -1.346884454587377711, 1.728604079486287137 ) ) ;
#201953 = CARTESIAN_POINT ( 'NONE',  ( 6.720655732516681802, 0.008434553976941013345, 1.726293928996263549 ) ) ;
#201954 = CARTESIAN_POINT ( 'NONE',  ( 5.764187864104357573, 9.876636274763768597, 1.040834085586084257E-14 ) ) ;
#201955 = CARTESIAN_POINT ( 'NONE',  ( -11.84668730067608600, 10.19999999999998153, 1.319999999999998286 ) ) ;
#201956 = CARTESIAN_POINT ( 'NONE',  ( 0.02935885042023527250, -1.056071399167260783, -1.364091372971764748 ) ) ;
#201957 = CARTESIAN_POINT ( 'NONE',  ( 0.7205771127097709838, -1.942975266472912299, -1.227557580038857399 ) ) ;
#201958 = CARTESIAN_POINT ( 'NONE',  ( 0.3807642395799659130, -0.2741851280289032688, -2.174293136291181483 ) ) ;
#201959 = CARTESIAN_POINT ( 'NONE',  ( 6.784571902810725419, -1.680486618648807218, 0.4264331113166124343 ) ) ;
#201960 = CARTESIAN_POINT ( 'NONE',  ( 3.194164748978207680, -0.8942147705085048415, 2.017778291555922809 ) ) ;
#201961 = CARTESIAN_POINT ( 'NONE',  ( 0.7784788067067629491, -1.160020112895485456, -1.834993543685500939 ) ) ;
#201962 = CARTESIAN_POINT ( 'NONE',  ( -5.000000000000009770, 3.850000000000006306, 6.071532165918824830E-15 ) ) ;
#201963 = CARTESIAN_POINT ( 'NONE',  ( 0.6029268795967283046, 1.958829854606686904, 0.8042956034161384826 ) ) ;
#201964 = CARTESIAN_POINT ( 'NONE',  ( 6.620655732516649294, 0.5674144795907026806, 2.226195167976598110 ) ) ;
#201965 = CARTESIAN_POINT ( 'NONE',  ( 5.227533229383872104, -1.829308364520453978, 0.6040709075912870096 ) ) ;
#201966 = VERTEX_POINT ( 'NONE', #164711 ) ;
#201968 = CARTESIAN_POINT ( 'NONE',  ( 0.7499999999999902300, 5.316666666666685082, -1.299038105676658228 ) ) ;
#201967 = CARTESIAN_POINT ( 'NONE',  ( 1.083963445724302588, -1.025016635393001252, 2.050507297876194901 ) ) ;
#201969 = CARTESIAN_POINT ( 'NONE',  ( 4.304877467538922531, 4.981110786005563007, 1.199719254218464037 ) ) ;
#201970 = CARTESIAN_POINT ( 'NONE',  ( 4.632082037363250748, 8.555846143565791095, -0.7998128361456231517 ) ) ;
#201971 = CARTESIAN_POINT ( 'NONE',  ( 3.282088111431053612, 2.166828800601192206, -0.4882270792503102808 ) ) ;
#201972 = CARTESIAN_POINT ( 'NONE',  ( -7.537970219518089543, 8.857015346601659900, -1.082531754730543971 ) ) ;
#201973 = FACE_OUTER_BOUND ( 'NONE', #21010, .T. ) ;
#201974 = CARTESIAN_POINT ( 'NONE',  ( 6.670248388243460447, 6.884303995813253252, -0.7216878364870257245 ) ) ;
#201975 = CARTESIAN_POINT ( 'NONE',  ( -8.988692655735990300, 9.589155641221221771, 0.7216878364870438212 ) ) ;
#201976 = VECTOR ( 'NONE', #50994, 1000.000000000000000 ) ;
#201977 = CARTESIAN_POINT ( 'NONE',  ( 5.885648082108199119, 6.999582529615296700, 1.082531754730549967 ) ) ;
#201978 = CARTESIAN_POINT ( 'NONE',  ( 2.250625165576759290, 1.976955744075848065, -0.3961026872240576702 ) ) ;
#201980 = CARTESIAN_POINT ( 'NONE',  ( 1.112259789790952746, 2.060362754584772471, -0.09740899567091049205 ) ) ;
#201979 = CARTESIAN_POINT ( 'NONE',  ( 7.065770611016287006, 11.39514947949436774, 1.040834085586084257E-14 ) ) ;
#201981 = CARTESIAN_POINT ( 'NONE',  ( 4.882939164911702434, 4.877617891921787852, 0.1515561221680329362 ) ) ;
#201982 = CARTESIAN_POINT ( 'NONE',  ( 6.549997608733495902, 7.774656977344789333, -1.082531754730548412 ) ) ;
#201983 = CARTESIAN_POINT ( 'NONE',  ( 6.550362485727940332, -1.338708790221679656, 1.112040286498132025 ) ) ;
#201984 = CARTESIAN_POINT ( 'NONE',  ( -0.6823417656250212460, 2.801041667008084879, 1.181850606188767472 ) ) ;
#201985 = CARTESIAN_POINT ( 'NONE',  ( 2.829092851278795617, -1.652813950429321999, 0.6331040572071617856 ) ) ;
#201986 = CARTESIAN_POINT ( 'NONE',  ( 1.442029965644067158, -1.730867108953790590, -1.034163949609874233 ) ) ;
#201987 = CARTESIAN_POINT ( 'NONE',  ( 0.4152503475762688856, -0.9843521281015167324, -1.555853522519357934 ) ) ;
#201988 = CARTESIAN_POINT ( 'NONE',  ( 5.601222333718593127, -0.5599829797399961118, 2.222829207915150374 ) ) ;
#201989 = CARTESIAN_POINT ( 'NONE',  ( 3.925598083870453614, 0.9833751987384667936, -1.556331266066004027 ) ) ;
#201990 = CARTESIAN_POINT ( 'NONE',  ( 7.584896871841365851, 10.93646455286856956, -1.199719254218446718 ) ) ;
#201991 = CARTESIAN_POINT ( 'NONE',  ( 3.662960631648714216, -1.609669772967847079, -0.8612380056681954166 ) ) ;
#201992 = CARTESIAN_POINT ( 'NONE',  ( 5.291638762709002464, 1.525045427759319727, -1.319226660814104335 ) ) ;
#201993 = CARTESIAN_POINT ( 'NONE',  ( -8.154339323615371171, 11.60081407993821045, 1.199719254218453823 ) ) ;
#201995 = CARTESIAN_POINT ( 'NONE',  ( -6.957269102468015554, 8.145844036748005834, 1.199719254218452047 ) ) ;
#201994 = CARTESIAN_POINT ( 'NONE',  ( 3.450319916561462197, 2.262689076145682598, 0.002162386163321801912 ) ) ;
#201996 = CARTESIAN_POINT ( 'NONE',  ( 6.018611168240656006, 1.417078199399327332, -1.558035186251781612 ) ) ;
#201997 = CARTESIAN_POINT ( 'NONE',  ( 3.613788337741298040, 0.5058112091442801272, -2.007490274132675445 ) ) ;
#201998 = CARTESIAN_POINT ( 'NONE',  ( 2.381428537494710618, 5.930083727052461562, 0.7998128361456462443 ) ) ;
#201999 = CARTESIAN_POINT ( 'NONE',  ( 0.6801582343749952297, 2.088541667008066316, -1.178068619123855409 ) ) ;
#202000 = CARTESIAN_POINT ( 'NONE',  ( 5.426475896148662770, -0.9536019125786737716, -1.894055658958586852 ) ) ;
#202001 = PRODUCT_CONTEXT ( 'NONE', #11751, 'mechanical' ) ;
#202002 = B_SPLINE_CURVE_WITH_KNOTS ( 'NONE', 3,
 ( #193440, #45084, #93835, #29884, #177197, #210747 ),
 .UNSPECIFIED., .F., .F.,
 ( 4, 2, 4 ),
 ( 3.785604876262024909E-17, 0.0006272018345858698966, 0.001254403669171702063 ),
 .UNSPECIFIED. ) ;
#202004 = CARTESIAN_POINT ( 'NONE',  ( 2.508321089405711746, -0.7374124507862482858, -1.779973396525496909 ) ) ;
#202003 = CARTESIAN_POINT ( 'NONE',  ( -8.130085669689073313, 12.63685038127928806, 0.7998128361456481317 ) ) ;
#202005 = CARTESIAN_POINT ( 'NONE',  ( -3.383641855062333281, 6.105276709951447778, -1.199719254218452047 ) ) ;
#202006 = CARTESIAN_POINT ( 'NONE',  ( 6.614111185624225620, 1.964402775464332507, -0.1412838390872969141 ) ) ;
#202007 = CARTESIAN_POINT ( 'NONE',  ( 4.543390873910906791, 6.393985001019784953, 1.443375672974065660 ) ) ;
#202008 = CARTESIAN_POINT ( 'NONE',  ( 5.671489233189207724, 6.113434141373025099, 0.7590443732325997672 ) ) ;
#202009 = CARTESIAN_POINT ( 'NONE',  ( -11.92619526913699879, 10.89999999999998259, 1.328859060402684644 ) ) ;
#202010 = CARTESIAN_POINT ( 'NONE',  ( -2.415323921528888196, 5.969628341758991930, 0.7998128361456341429 ) ) ;
#202011 = CARTESIAN_POINT ( 'NONE',  ( 0.4928134435002875513, -1.227493105415909946, 1.851297100075269153 ) ) ;
#202012 = CARTESIAN_POINT ( 'NONE',  ( 2.924945619078959336, 1.982447918529605557, 0.7109604360746536456 ) ) ;
#202013 = CARTESIAN_POINT ( 'NONE',  ( -4.004454267989906668, 5.765225627445230927, 1.599625672291270506 ) ) ;
#202014 = CARTESIAN_POINT ( 'NONE',  ( 6.805303039055573322, 10.02693841461847057, 1.199719254218460707 ) ) ;
#202015 = CARTESIAN_POINT ( 'NONE',  ( 0.9064450206472760563, 0.5352286137044174330, 1.782442419352270102 ) ) ;
#202016 = CARTESIAN_POINT ( 'NONE',  ( 5.438792177376376991, 9.497007973581119700, 1.040834085586084257E-14 ) ) ;
#202017 = CARTESIAN_POINT ( 'NONE',  ( 5.345992642490140057, 5.131412925860272090, 1.040834085586084257E-14 ) ) ;
#202018 = CARTESIAN_POINT ( 'NONE',  ( -6.536439455564198475, 8.719208346281938304, 1.443375672974064550 ) ) ;
#202019 = CARTESIAN_POINT ( 'NONE',  ( -8.202319746587722449, 8.671720580548228696, 1.040834085586084257E-14 ) ) ;
#202020 = CARTESIAN_POINT ( 'NONE',  ( 1.705496241919310707, 1.842552997918958768, -1.049655202612943095 ) ) ;
#202021 = CARTESIAN_POINT ( 'NONE',  ( -5.966470118465691641, 9.118576350588734059, -1.199719254218452047 ) ) ;
#202023 = CARTESIAN_POINT ( 'NONE',  ( 4.141029529442549872, -0.1900441490861082827, -1.952618137025011746 ) ) ;
#202022 = CARTESIAN_POINT ( 'NONE',  ( -0.6125000000000279110, 1.291666666666656305, 1.060881119635892933 ) ) ;
#202024 = CARTESIAN_POINT ( 'NONE',  ( 2.149508875876861236, -1.735919364271593768, -1.288018159417112729 ) ) ;
#202025 = CARTESIAN_POINT ( 'NONE',  ( 1.575478407343299692, -0.9843019613302635973, 1.555867251595323353 ) ) ;
#202027 = CARTESIAN_POINT ( 'NONE',  ( -4.043761313400059620, 7.584134902449670257, 0.3518898875958225703 ) ) ;
#202026 = DIRECTION ( 'NONE',  ( 0.000000000000000000, -1.000000000000000000, 0.000000000000000000 ) ) ;
#202028 = CARTESIAN_POINT ( 'NONE',  ( 2.958654558096874609, 0.2547609298257165200, -1.721438497358678932 ) ) ;
#202029 = CARTESIAN_POINT ( 'NONE',  ( 0.6674790882332001241, 14.00000000000001066, -11.66566053519550650 ) ) ;
#202030 = CARTESIAN_POINT ( 'NONE',  ( 6.182154858151487353, 6.314861544039274577, -0.7216878364870257245 ) ) ;
#202031 = CARTESIAN_POINT ( 'NONE',  ( -10.50660484223216606, 5.359830900411396648, 5.105327592218940502 ) ) ;
#202032 = CARTESIAN_POINT ( 'NONE',  ( 1.358524781292804517, 0.8764843271744371389, 1.976213614152767750 ) ) ;
#202033 = CARTESIAN_POINT ( 'NONE',  ( 3.409529676982744562, 0.4871283372531940992, 1.956261718130556382 ) ) ;
#202034 = CARTESIAN_POINT ( 'NONE',  ( 0.7500000000000006661, 12.86458333401613352, 1.299038105676657340 ) ) ;
#202035 = CARTESIAN_POINT ( 'NONE',  ( 0.8839147992780393981, 1.452536163361785260, 1.601146772000871188 ) ) ;
#202036 = CARTESIAN_POINT ( 'NONE',  ( 3.819176294577591779, -0.1464417209034867828, 1.966092509880690065 ) ) ;
#202037 = AXIS2_PLACEMENT_3D ( 'NONE', #142748, #126545, #44158 ) ;
#202038 = CARTESIAN_POINT ( 'NONE',  ( 6.509000000000039421, 4.695815278351551214, 2.562658139094181386 ) ) ;
#202039 = CARTESIAN_POINT ( 'NONE',  ( 2.630336588288070043, 0.2403035443280654992, 1.927090367541855365 ) ) ;
#202042 = VERTEX_POINT ( 'NONE', #49898 ) ;
#202041 = CARTESIAN_POINT ( 'NONE',  ( -3.336715202739028552, 6.906935146588564223, 0.7216878364870338292 ) ) ;
#202040 = CYLINDRICAL_SURFACE ( 'NONE', #87619, 1.500000000000000222 ) ;
#202043 = CARTESIAN_POINT ( 'NONE',  ( -5.492461626867567226, 6.540864998501174199, 1.082531754730549078 ) ) ;
#202044 = CARTESIAN_POINT ( 'NONE',  ( -0.1110810684433142237, 6.948330828014858795, -2.391984312838004278 ) ) ;
#202045 = CARTESIAN_POINT ( 'NONE',  ( 4.050854035433010480, 7.948023151305657841, 0.000000000000000000 ) ) ;
#202046 = CARTESIAN_POINT ( 'NONE',  ( -4.736594563127865420, 6.619389305106191834, -1.599625672291271394 ) ) ;
#202048 = EDGE_LOOP ( 'NONE', ( #202396, #89104, #178730, #174378 ) ) ;
#202047 = CARTESIAN_POINT ( 'NONE',  ( -7.767895665986912057, 8.027242796598338614, -0.7998128361456362523 ) ) ;
#202049 = CARTESIAN_POINT ( 'NONE',  ( -8.961576348508637935, 12.43862759236002269, -1.082531754730543083 ) ) ;
#202050 = CARTESIAN_POINT ( 'NONE',  ( 6.581126798121099242, -0.1039769691308822797, -2.305377512668804751 ) ) ;
#202051 = CARTESIAN_POINT ( 'NONE',  ( 3.285556943749998737, -3.055208332855376518, -1.896917185911906500 ) ) ;
#202052 = CARTESIAN_POINT ( 'NONE',  ( 4.117980938109369937, 1.947433809354440326, -0.2358448244534834815 ) ) ;
#202053 = CARTESIAN_POINT ( 'NONE',  ( 8.609591239877852686, 10.00327685373437347, -1.199719254218445830 ) ) ;
#202054 = CARTESIAN_POINT ( 'NONE',  ( 2.110000207431836472, 0.002812218110825881467, 2.016597019944998959 ) ) ;
#202055 = ORIENTED_EDGE ( 'NONE', *, *, #207484, .T. ) ;
#202056 = CARTESIAN_POINT ( 'NONE',  ( 3.925106927653505995, -1.840236814299311741, 1.047156446301507948 ) ) ;
#202057 = CARTESIAN_POINT ( 'NONE',  ( 1.499999999999987121, 2.077083334016153415, -0.8660254037844262731 ) ) ;
#202059 = CARTESIAN_POINT ( 'NONE',  ( -7.040761844198392794, 7.108643661186573759, -0.7998128361456291469 ) ) ;
#202058 = CARTESIAN_POINT ( 'NONE',  ( -10.20634067979409565, 1.972237431424338716, 5.892633538919476166 ) ) ;
#202060 = CARTESIAN_POINT ( 'NONE',  ( 3.538839456958355889, -1.395042877683351890, -1.201619466480362108 ) ) ;
#202061 = ORIENTED_EDGE ( 'NONE', *, *, #170654, .F. ) ;
#202062 = CARTESIAN_POINT ( 'NONE',  ( -7.862839020921525091, 11.26073039346208660, -1.199719254218446718 ) ) ;
#202063 = CARTESIAN_POINT ( 'NONE',  ( -15.75000000000000000, 13.40000000000000036, -3.600000000000002309 ) ) ;
#202064 = CARTESIAN_POINT ( 'NONE',  ( 3.551138032611600437, 0.3147205237276836653, 2.097014573754731881 ) ) ;
#202065 = CARTESIAN_POINT ( 'NONE',  ( -10.04957930738605931, 3.829867255648770730, -5.932860765075387732 ) ) ;
#202066 = CARTESIAN_POINT ( 'NONE',  ( 6.962275575817444384, 8.081408578997208991, -1.199719254218446718 ) ) ;
#202067 = EDGE_LOOP ( 'NONE', ( #98312, #72295, #116526, #29045 ) ) ;
#202068 = CARTESIAN_POINT ( 'NONE',  ( 4.991509756128800213, 1.524171611017493655, 1.387147876433484806 ) ) ;
#202070 = CARTESIAN_POINT ( 'NONE',  ( 2.067674361007607597, -1.131582805410412673, 1.452419944642673100 ) ) ;
#202069 = CARTESIAN_POINT ( 'NONE',  ( -7.335124800193271177, 8.516399340768996851, -1.199719254218452935 ) ) ;
#202071 = CARTESIAN_POINT ( 'NONE',  ( 7.723341061279088038, 12.16231500480096983, -0.7998128361456291469 ) ) ;
#202072 = CARTESIAN_POINT ( 'NONE',  ( 0.6823417656249917140, 5.592708333674749177, 1.181850606188765695 ) ) ;
#202073 = PLANE ( 'NONE',  #136111 ) ;
#202074 = CARTESIAN_POINT ( 'NONE',  ( -4.840079859301741116, 5.046757083302627400, -0.8962971793361621531 ) ) ;
#202075 = CARTESIAN_POINT ( 'NONE',  ( 3.475000000000000533, -1.531249999044085541, 0.000000000000000000 ) ) ;
#202076 = CARTESIAN_POINT ( 'NONE',  ( 2.315298440750997777, 1.971968782506158924, 0.9909306302095726160 ) ) ;
#202077 = CARTESIAN_POINT ( 'NONE',  ( 3.479979345725477291, 1.432071248269211505, 1.751504329374527158 ) ) ;
#202078 = CARTESIAN_POINT ( 'NONE',  ( -6.561783159334121152, 10.59923808595773664, -0.7216878364870278340 ) ) ;
#202079 = CARTESIAN_POINT ( 'NONE',  ( 4.254050669898622239, 0.7686244906546428890, -1.640568623306848606 ) ) ;
#202080 = CARTESIAN_POINT ( 'NONE',  ( 4.364398177449787752, -1.859642558872817375, -0.4596742015197906595 ) ) ;
#202081 = EDGE_CURVE ( 'NONE', #116082, #174777, #167910, .T. ) ;
#202082 = CARTESIAN_POINT ( 'NONE',  ( -1.364683531250010295, 4.592708333674755394, 0.7879004041258379498 ) ) ;
#202083 = CARTESIAN_POINT ( 'NONE',  ( 3.801606108737245471, -0.5733388152893458267, 1.886244881718708521 ) ) ;
#202084 = CARTESIAN_POINT ( 'NONE',  ( 4.627732503263369601, -1.150995203733524930, -1.474563928533303869 ) ) ;
#202085 = EDGE_CURVE ( 'NONE', #105749, #47983, #30407, .T. ) ;
#202086 = CARTESIAN_POINT ( 'NONE',  ( 3.299772510450727836, 1.819142665603549425, 1.419829399881943566 ) ) ;
#202087 = CARTESIAN_POINT ( 'NONE',  ( 4.492532346964829060, 1.824898331334467549, 0.3640980636450250052 ) ) ;
#202088 = CARTESIAN_POINT ( 'NONE',  ( 0.04536344973641179279, -10.00000000000001954, 9.579592128872851831 ) ) ;
#202089 = CLOSED_SHELL ( 'NONE', ( #188055, #35218, #193152, #114894, #105435, #132377, #24000, #145997 ) ) ;
#202090 = CARTESIAN_POINT ( 'NONE',  ( -0.1355283706049141557, -1.957205112593700003, -0.4852584411360050254 ) ) ;
#202092 = CARTESIAN_POINT ( 'NONE',  ( 1.735132801782751200, 0.2076089413485527335, 2.095809512812545350 ) ) ;
#202091 = CARTESIAN_POINT ( 'NONE',  ( -4.595850884908229794, 4.464173575255435011, 0.7216878364870317197 ) ) ;
#202093 = B_SPLINE_CURVE_WITH_KNOTS ( 'NONE', 3,
 ( #53640, #119773, #102388, #169523, #134917, #168456, #152214 ),
 .UNSPECIFIED., .F., .F.,
 ( 4, 3, 4 ),
 ( 0.0001126021369352508755, 0.001495765174703660855, 0.002006790696433096138 ),
 .UNSPECIFIED. ) ;
#202094 = CARTESIAN_POINT ( 'NONE',  ( 3.267151830768944443, 4.834763107362302748, -1.443375672974058777 ) ) ;
#202096 = DIRECTION ( 'NONE',  ( 0.000000000000000000, 1.000000000000000000, 0.000000000000000000 ) ) ;
#202095 = CARTESIAN_POINT ( 'NONE',  ( -1.201851678989727383E-14, 5.259375000341421469, -1.575800808251660134 ) ) ;
#202097 = CARTESIAN_POINT ( 'NONE',  ( 3.006218798242997980, -0.8556837461295877523, 1.940463308995137526 ) ) ;
#202098 = CARTESIAN_POINT ( 'NONE',  ( -4.913752204202785023, 4.881785571126718182, -0.5639616748225815268 ) ) ;
#202099 = CARTESIAN_POINT ( 'NONE',  ( 1.301042304527067817, -0.3004618026806615272, -1.997203725593140078 ) ) ;
#202100 = CARTESIAN_POINT ( 'NONE',  ( -1.364683531250000748, 0.2593750003414205252, 0.000000000000000000 ) ) ;
#202101 = CARTESIAN_POINT ( 'NONE',  ( -3.714570900464290393, 5.356752022006865843, 1.443375672974064550 ) ) ;
#202102 = CARTESIAN_POINT ( 'NONE',  ( 5.172599298813543633, 5.993452922492633839, -1.199719254218452047 ) ) ;
#202103 = EDGE_LOOP ( 'NONE', ( #68478, #200906, #22667, #163663 ) ) ;
#202104 = CARTESIAN_POINT ( 'NONE',  ( 1.880366631079612549, -1.158069840294423392, 1.825029014904603342 ) ) ;
#202105 = DIRECTION ( 'NONE',  ( -0.6483454320283800199, 0.000000000000000000, 0.7613463080411787542 ) ) ;
#202108 = CARTESIAN_POINT ( 'NONE',  ( 6.639320575229294974, 0.002105643433562139673, 2.003388605011639179 ) ) ;
#202107 = CARTESIAN_POINT ( 'NONE',  ( 6.925078400183550364, 4.698656493127392864, 2.418320467900983761 ) ) ;
#202106 = CARTESIAN_POINT ( 'NONE',  ( 5.411639590510088027, 6.342609606130419131, -1.199719254218452047 ) ) ;
#202109 = CARTESIAN_POINT ( 'NONE',  ( -11.04536101718726293, 12.69999999999999929, 1.099999999999996758 ) ) ;
#202110 = CARTESIAN_POINT ( 'NONE',  ( 5.964077395145578109, -1.074666730956087335, 1.706109649615504154 ) ) ;
#202111 = CARTESIAN_POINT ( 'NONE',  ( -6.860062538834774237, 10.94723069537516302, 0.7216878364870458196 ) ) ;
#202112 = CARTESIAN_POINT ( 'NONE',  ( 6.480031082513550089, -2.050496881725831777, -0.4073240614407472315 ) ) ;
#202113 = CARTESIAN_POINT ( 'NONE',  ( -10.10286202908859465, -8.578580700073972665, 0.6127037010540659079 ) ) ;
#202115 = CARTESIAN_POINT ( 'NONE',  ( -0.6823417656250003738, 11.40104166700806765, 1.181850606188754593 ) ) ;
#202114 = CARTESIAN_POINT ( 'NONE',  ( 1.358695222972395422, 0.9186288065576648787, 2.067797507578944760 ) ) ;
#202116 = CARTESIAN_POINT ( 'NONE',  ( -8.239604668803112375, 10.63595808506888396, -1.599625672291263179 ) ) ;
#202117 = CARTESIAN_POINT ( 'NONE',  ( -4.785665035499573783, 5.645992631913323123, 1.082531754730558626 ) ) ;
#202118 = CARTESIAN_POINT ( 'NONE',  ( 1.364683531249986537, 1.717708333674749399, -0.7879004041258239610 ) ) ;
#202119 = CARTESIAN_POINT ( 'NONE',  ( 0.4019237886466778820, 9.323664549684631098, 1.500000000000001554 ) ) ;
#202120 = CARTESIAN_POINT ( 'NONE',  ( -0.7500000000000179856, 9.041666666666669627, 1.299038105676658228 ) ) ;
#202121 = CARTESIAN_POINT ( 'NONE',  ( 3.844159338287247429, 1.716807015663003311, 0.1666082703000223986 ) ) ;
#202122 = ADVANCED_FACE ( 'NONE', ( #149530 ), #33637, .T. ) ;
#202123 = CARTESIAN_POINT ( 'NONE',  ( 6.066347387471824781, 6.042103138330730872, -0.7998128361456481317 ) ) ;
#202124 = CARTESIAN_POINT ( 'NONE',  ( 2.178617772012156006, -0.08127397458944020381, -1.767985329221566815 ) ) ;
#202125 = CARTESIAN_POINT ( 'NONE',  ( 3.070950286465543577, -1.523008450377001832, 1.316504112208529920 ) ) ;
#202126 = CARTESIAN_POINT ( 'NONE',  ( 5.667066814448853407, -1.992748536412903615, -0.9483587796220711574 ) ) ;
#202127 = VERTEX_POINT ( 'NONE', #36828 ) ;
#202128 = CARTESIAN_POINT ( 'NONE',  ( 3.902606965841335818, -1.998407076283228223, -0.2920856897847978195 ) ) ;
#202129 = CARTESIAN_POINT ( 'NONE',  ( -7.422162748838431412, 7.623887726591770608, -0.7998128361456362523 ) ) ;
#202131 = CARTESIAN_POINT ( 'NONE',  ( 4.130482583401101415, 0.5405105419177670401, 1.942537254285629178 ) ) ;
#202130 = CARTESIAN_POINT ( 'NONE',  ( 5.444028431581452665, -1.345373016635186714, -1.639009079359869725 ) ) ;
#202133 = ORIENTED_EDGE ( 'NONE', *, *, #14440, .F. ) ;
#202132 = CARTESIAN_POINT ( 'NONE',  ( 4.271601952734533469, 0.3905692737867596520, -1.768816315278500584 ) ) ;
#202134 = ORIENTED_EDGE ( 'NONE', *, *, #33948, .T. ) ;
#202135 = CARTESIAN_POINT ( 'NONE',  ( 1.990876257202532695, 1.628914321797021669, -0.9196232060951770038 ) ) ;
#202136 = AXIS2_PLACEMENT_3D ( 'NONE', #172423, #210228, #175633 ) ;
#202137 = CARTESIAN_POINT ( 'NONE',  ( 4.907894938888475167, 6.474487383728034118, -2.499999999999995115 ) ) ;
#202138 = CARTESIAN_POINT ( 'NONE',  ( 6.129554203544218538, -0.2143803907406968412, 1.798669436738309368 ) ) ;
#202139 = DIRECTION ( 'NONE',  ( -0.6507913734559640506, -0.7592566023653004592, 0.000000000000000000 ) ) ;
#202140 = CARTESIAN_POINT ( 'NONE',  ( -10.74038358936941506, 4.109630040845076770, -4.806702709432750353 ) ) ;
#202141 = SURFACE_SIDE_STYLE ('',( #203223 ) ) ;
#202142 = VECTOR ( 'NONE', #7729, 1000.000000000000000 ) ;
#202143 = CARTESIAN_POINT ( 'NONE',  ( 1.364683531249988535, 3.217708333674748289, -0.7879004041258239610 ) ) ;
#202144 = CARTESIAN_POINT ( 'NONE',  ( 0.6504702201592416078, 1.884490048413577368, 0.3244712162126031085 ) ) ;
#202145 = CARTESIAN_POINT ( 'NONE',  ( 5.885648082108190238, 7.959951743916638733, 1.443375672974065660 ) ) ;
#202146 = CARTESIAN_POINT ( 'NONE',  ( 1.961309178647975715, 1.629323162926434199, 1.092499269706406428 ) ) ;
#202147 = FACE_OUTER_BOUND ( 'NONE', #204823, .T. ) ;
#202148 = EDGE_CURVE ( 'NONE', #190431, #90194, #151013, .T. ) ;
#202149 = CARTESIAN_POINT ( 'NONE',  ( -6.784929528996132220, 6.880448970109080520, 0.000000000000000000 ) ) ;
#202150 = CARTESIAN_POINT ( 'NONE',  ( 3.779626292077962191, 0.2561244552635975058, -2.104982076983111572 ) ) ;
#202152 = CARTESIAN_POINT ( 'NONE',  ( 10.94445979172680694, -5.609732095436334554, -0.02903434592765111177 ) ) ;
#202151 = CARTESIAN_POINT ( 'NONE',  ( 8.723781775389312543, 12.26516360700784958, -1.199719254218446718 ) ) ;
#202153 = CARTESIAN_POINT ( 'NONE',  ( 5.290288327143207958, -1.956129722686357431, -0.2442305991610035365 ) ) ;
#202154 = CARTESIAN_POINT ( 'NONE',  ( -0.6823417656250212460, 1.301041667008083547, 1.181850606188755259 ) ) ;
#202156 = CARTESIAN_POINT ( 'NONE',  ( 0.8967405870976161708, -1.965081358092489516, -0.4369277762777488139 ) ) ;
#202155 = VECTOR ( 'NONE', #29097, 1000.000000000000000 ) ;
#202157 = B_SPLINE_CURVE_WITH_KNOTS ( 'NONE', 3,
 ( #163602, #28260, #94353, #11996 ),
 .UNSPECIFIED., .F., .F.,
 ( 4, 4 ),
 ( 0.000000000000000000, 6.033646489357627837E-05 ),
 .UNSPECIFIED. ) ;
#202158 = EDGE_LOOP ( 'NONE', ( #162558, #35057, #119691, #182515 ) ) ;
#202159 = CARTESIAN_POINT ( 'NONE',  ( 1.036884384669316539, -1.666496236897334615, 1.305811245984341173 ) ) ;
#202160 = CARTESIAN_POINT ( 'NONE',  ( 12.00010711203362312, 6.624312021734491296, -0.4953576099243469089 ) ) ;
#202161 = CARTESIAN_POINT ( 'NONE',  ( 2.330607996690749140, -1.275545549462468120, 1.630658604070814199 ) ) ;
#202162 = CARTESIAN_POINT ( 'NONE',  ( 4.903208829997618423, 5.749440385532527564, -1.199719254218450271 ) ) ;
#202163 = CARTESIAN_POINT ( 'NONE',  ( 6.723917837734620484, 6.809268663637336516, 0.000000000000000000 ) ) ;
#202164 = ORIENTED_EDGE ( 'NONE', *, *, #91398, .T. ) ;
#202166 = CARTESIAN_POINT ( 'NONE',  ( 3.655894977179307226, 7.416961240017848844, -0.7998128361456291469 ) ) ;
#202165 = CARTESIAN_POINT ( 'NONE',  ( 4.945306066807232170, 0.6564501001628511023, -1.984974157428524899 ) ) ;
#202169 = ORIENTED_EDGE ( 'NONE', *, *, #129583, .T. ) ;
#202168 = CARTESIAN_POINT ( 'NONE',  ( 2.139049582973771457, 0.0009909630806471080022, 1.811656970554485602 ) ) ;
#202167 = CARTESIAN_POINT ( 'NONE',  ( 3.047666980291532823, 0.6586017179070653427, -1.702814618940437619 ) ) ;
#202170 = CARTESIAN_POINT ( 'NONE',  ( 6.586557750117827403, -2.163372447211810989, -0.4352210726449382006 ) ) ;
#202171 = CARTESIAN_POINT ( 'NONE',  ( 3.766852362949911992, 6.052795590908778500, 1.321332388365988875 ) ) ;
#202172 = CARTESIAN_POINT ( 'NONE',  ( 12.19178133996304148, 6.204039751267350411, 2.192769013902648112 ) ) ;
#202173 = CARTESIAN_POINT ( 'NONE',  ( 5.772568991252683190, -1.404203161598962968, 1.702366421003978392 ) ) ;
#202174 = CARTESIAN_POINT ( 'NONE',  ( 1.364683531250000748, 9.317708333674731946, -0.7879004041258355073 ) ) ;
#202175 = EDGE_CURVE ( 'NONE', #177247, #153954, #186275, .T. ) ;
#202176 = VERTEX_POINT ( 'NONE', #85585 ) ;
#202177 = CARTESIAN_POINT ( 'NONE',  ( 3.650944405621194377, 0.2833616294029631111, 1.891055170903446658 ) ) ;
#202178 = CARTESIAN_POINT ( 'NONE',  ( -3.002240950422295995, 5.590032644546251817, -1.199719254218452935 ) ) ;
#202179 = CARTESIAN_POINT ( 'NONE',  ( 6.760712154708803823, 11.03924794713562818, 1.040834085586084257E-14 ) ) ;
#202180 = CARTESIAN_POINT ( 'NONE',  ( 6.373496627357888578, -0.2573980274669443458, 2.054251119134167691 ) ) ;
#202181 = CARTESIAN_POINT ( 'NONE',  ( 0.000000000000000000, 4.000000000000003553, 12.00000000000000178 ) ) ;
#202182 = CARTESIAN_POINT ( 'NONE',  ( 5.495707582769355781, -2.191739722525353429, -0.0009102486706394352645 ) ) ;
#202183 = CARTESIAN_POINT ( 'NONE',  ( 5.413027408713817046, 7.651055653456078076, -1.328921179265474262 ) ) ;
#202184 = CARTESIAN_POINT ( 'NONE',  ( -4.363504500571202982, 15.44735459669111854, -11.13999821485972674 ) ) ;
#202185 = CARTESIAN_POINT ( 'NONE',  ( 1.451998047843343409, 7.315968950353815892, -4.301760722578415574 ) ) ;
#202186 = CARTESIAN_POINT ( 'NONE',  ( 3.585083614955932863, 1.692364770286663322, -0.7970176776704934740 ) ) ;
#202187 = CARTESIAN_POINT ( 'NONE',  ( -0.02319159430947542039, 1.394398620246390275, -2.068318759734718792 ) ) ;
#202188 = DIRECTION ( 'NONE',  ( 6.938893903907222067E-15, 1.000000000000000000, 0.000000000000000000 ) ) ;
#202189 =( BOUNDED_SURFACE ( )  B_SPLINE_SURFACE ( 1, 2, ( 
 ( #193222, #61092, #73051, #140238, #141322, #91480, #42736, #26448, #139150, #92557, #62166, #112052, #181230, #176980, #161806, #97881, #66385, #115240, #132533, #29670, #28598, #13397, #45933, #180182, #32858, #46996, #211587, #113113, #96822, #94686, #160728, #128325, #194288, #178052, #212654, #129386, #78402, #49122, #65328, #95754, #12321, #210532, #79473, #179118, #130441, #195365, #197478, #163942, #15517, #30741, #114184, #98933, #131475, #162871, #147687, #145591, #164988, #213704, #16578, #63223, #144522, #314, #14451, #80542, #82661, #146639, #64295, #148745, #48073, #81602, #196428, #31805, #44868, #110974, #4583, #200658, #149818, #102121, #21899, #153006, #53368, #70657, #104265, #17642, #166056, #38193, #183366, #68526, #99990, #71728, #169255, #116297, #198530, #83727, #3519, #50177, #33914, #1389, #88009, #5647, #182288, #67450, #133595, #170311, #85871, #134655, #69591, #135701, #199600, #120587, #154080, #51243, #201727, #202795, #54445, #168190, #117369, #186565, #19789, #136767, #34970, #101042, #167132, #18717, #119503, #84801, #52307, #150889, #2451, #185488, #118437, #184424, #36041, #151948, #37114, #103192, #20841, #86940, #188705, #155150, #204932, #62686, #55507, #40341, #193756, #162345, #211061, #13928, #122742, #121661, #106447, #138912, #61635, #128845, #139990, #90161, #206011, #189766, #187629, #39256, #6732, #72811, #56583, #94162, #7804, #171387, #145058, #161275, #172470, #105350, #89097, #24058, #57646, #11804, #73897, #78936, #45403, #111519, #123806, #209993, #194827, #12862, #41418, #29137, #156227, #46462, #95225, #112584, #107525, #22978, #96293, #173556, #25129, #178596, #160201, #77879, #30206, #144001, #177525, #127802, #137840, #203862, #34460, #100531, #82139, #31281, #198021, #117918, #166606, #149282, #18195, #200146, #113657, #47545, #134139, #64825, #164469, #195908, #167667, #50715, #212124, #80008, #179661, #99473, #146113, #129922, #97356, #183911, #101599, #63762, #163413, #14989, #51800, #181762, #16055, #165532, #17124, #81083, #1937, #35522, #147170, #83200, #84280, #150367, #49649, #213197, #67997, #115772, #130970, #196962, #48600, #114718, #180713, #863, #32336, #148231, #98404, #214233, #66929, #65861, #132011, #133071, #33395, #199069, #116841, #182842, #38741, #120060, #168734, #71207, #86422, #5132, #4070, #23533, #70140, #36588, #152488, #155694, #151431, #136252, #72278, #40892, #89641, #106996, #202272, #3004, #53923, #20335, #154629, #7276, #21387, #186035, #87496, #137323, #69073, #135193, #102675, #37671, #103747, #187107, #169798, #52848, #73353, #39811, #153561, #201210, #184962, #203339, #54992, #104823, #121144, #171942, #138387, #204405, #170869, #88571, #139456, #105917, #22459, #122215, #6209, #205488, #188177, #57122, #56058, #118983, #189252, #123289, #19268, #85350, #109145, #58187, #28894, #176217, #77631, #142671, #110208, #75504, #127549, #193520, #175158, #124345, #76561, #210824, #45161, #27819, #111275, #78692, #206559, #140546, #12619, #157837, #43033, #74443, #46225, #143753, #90711, #173021, #190303, #192433, #24602, #8359, #41960, #62449, #194579, #156773, #108072, #174100, #144817, #60311, #26744, #44088, #93916, #25673, #94978, #128612, #91780, #159957, #177278, #161024, #208682, #9434, #141615, #126470, #207625, #59243, #125401, #191366, #92847, #158891, #10488, #209748, #61390, #11561, #48359, #47296, #198818, #601, #199890, #31039, #116583, #132814, #114470, #164222, #14750, #180471, #15809, #211884, #49404, #80842, #67733, #100274, #63525, #13690, #197766, #50464, #32086, #166340, #149026, #98174, #130727, #29962, #212949, #178354, #115523, #64586, #181518, #129677, #66667, #196718, #81895, #182578, #17931, #34200, #82952, #84016, #147981, #146932, #113411, #179417, #150107, #97113, #213991, #165277, #65611, #131761, #1679, #133883, #33147, #112342, #163165, #99227, #96048, #16871, #162101, #79760, #145876, #195662, #120873, #54724, #37403, #53657, #69875, #89378, #183653, #21119, #2743, #187911, #151172, #117661, #19007, #4865, #5942, #3801, #184704, #35258, #22187, #186847, #155427, #39541, #55788 ),
 ( #52590, #138126, #88302, #87225, #105642, #154363, #153289, #118717, #204135, #135984, #171669, #68813, #121945, #7013, #23266, #134935, #101334, #170600, #200941, #201998, #72013, #73088, #139189, #103477, #86159, #36326, #102404, #51536, #168472, #119789, #104556, #20070, #70943, #167416, #85088, #137054, #152230, #185770, #169539, #203079, #38479, #142418, #56861, #193261, #57926, #60061, #208427, #191111, #207376, #9175, #28638, #123035, #174909, #156511, #127290, #90443, #188986, #172760, #158639, #159699, #157582, #124091, #40630, #175966, #126217, #94725, #44908, #209489, #8100, #10236, #43839, #106733, #26487, #107816, #192178, #24335, #75250, #27560, #109955, #190054, #111016, #140282, #206302, #77377, #93656, #92597, #177021, #11298, #76311, #41706, #143493, #141363, #160770, #74190, #61130, #12363, #78442, #173841, #25418, #205219, #91524, #58996, #125152, #42778, #108886, #194330, #115277, #49160, #162911, #80583, #79515, #16619, #32895, #17680, #63264, #148780, #165025, #146681, #196470, #47039, #212697, #48112, #29712, #81641, #113155, #100030, #132566, #95793, #45972, #15554, #82701, #64338, #198567, #181269, #130480, #14493, #62206, #30784, #210572, #147726, #96863, #213743, #161850, #98973, #114224, #180222, #350, #50216, #166092, #211629, #13438, #66423, #31844, #145633, #116335, #65366, #182325, #97921, #131513, #179160, #33954, #144562, #163979, #129426, #197516, #128363, #112093, #178095, #195410, #203901, #117409, #51284, #137881, #68566, #168230, #199638, #171428, #54481, #1427, #83766, #183405, #103232, #149859, #133636, #101080, #121701, #105389, #67491, #35009, #167169, #55547, #185527, #19827, #169292, #20877, #18756, #5688, #187665, #84841, #86976, #88047, #154118, #201763, #150930, #71765, #119542, #104303, #2491, #200697, #134693, #52349, #153046, #118476, #85912, #184461, #36079, #4621, #102162, #151986, #135741, #3560, #69633, #53404, #39295, #37153, #70693, #136806, #202832, #120626, #186602, #38229, #170352, #21937, #44648, #7844, #6769, #140025, #24095, #158388, #11040, #25170, #189804, #91271, #75001, #155187, #72845, #40380, #106483, #172510, #190862, #107563, #56617, #27298, #43586, #90199, #138950, #188741, #156263, #157328, #108630, #173598, #175708, #142161, #76062, #8920, #92349, #159442, #109703, #141110, #125965, #57686, #93405, #191921, #77119, #73932, #204971, #123842, #174657, #89133, #143242, #206051, #9984, #26232, #207121, #58746, #41455, #60876, #122781, #124899, #42525, #209231, #208178, #59810, #127035, #192995, #110762, #23016, #95545, #160512, #147476, #31590, #100, #98716, #181019, #194066, #130224, #15303, #12115, #146425, #79263, #97665, #28377, #195152, #213496, #81391, #161596, #82443, #111838, #177842, #48902, #65118, #212439, #16365, #131274, #64081, #29455, #115022, #129175, #148533, #45719, #32639, #132312, #66166, #13185, #78189, #197262, #61949, #46786, #164775, #198318, #96606, #144315, #49958, #176761, #112900, #178911, #145380, #94471, #210313, #128108, #211378, #63004, #30526, #162659, #14229, #80324, #196218, #47859, #113971, #179968, #163723, #71512, #104048, #67241, #17427, #201507, #136554, #35828, #170094, #152788, #118219, #134443, #33699, #2235, #182067, #53155, #68312, #185270, #133375, #4368, #200446, #19577, #202575, #21680, #54227, #86719, #120365, #101906, #150674, #117149, #183152, #186340, #34755, #52092, #169033, #84587, #69377, #70438, #87790, #151737, #153864, #51027, #184205, #99776, #1177, #167971, #37975, #5433, #85650, #165841, #137624, #20630, #3307, #135485, #100829, #203641, #116077, #83510, #166914, #149593, #199380, #119284, #36893, #18508, #102975, #173326, #154928, #206857, #172250, #10783, #43327, #6513, #171167, #140845, #75803, #189547, #109445, #92080, #57422, #73667, #187411, #155995, #121442, #58489, #7582, #124645, #72589, #158137, #139766, #24904, #141911, #175452, #207923, #25974, #59544, #41195, #89944, #56357, #122520, #125704, #188483, #205792, #108373, #23837, #8661, #9728, #27036, #91010, #93145, #204707, #123584, #39042, #107302, #190602, #105127, #159182, #40113, #42260, #174396, #157072, #74740 ) ),
 .UNSPECIFIED., .F., .F., .T. ) 
 B_SPLINE_SURFACE_WITH_KNOTS ( ( 2, 2 ),
 ( 3, 2, 2, 2, 2, 2, 2, 2, 2, 2, 2, 2, 2, 2, 2, 2, 2, 2, 2, 2, 2, 2, 2, 2, 2, 2, 2, 2, 2, 2, 2, 2, 2, 2, 2, 2, 2, 2, 2, 2, 2, 2, 2, 2, 2, 2, 2, 2, 2, 2, 2, 2, 2, 2, 2, 2, 2, 2, 2, 2, 2, 2, 2, 2, 2, 2, 2, 2, 2, 2, 2, 2, 2, 2, 2, 2, 2, 2, 2, 2, 2, 2, 2, 2, 2, 2, 2, 2, 2, 2, 2, 2, 2, 2, 2, 2, 2, 2, 2, 2, 2, 2, 2, 2, 2, 2, 2, 2, 2, 2, 2, 2, 2, 2, 2, 2, 2, 2, 2, 2, 2, 2, 2, 2, 2, 2, 2, 2, 2, 2, 2, 2, 2, 2, 2, 2, 2, 2, 2, 2, 2, 2, 2, 2, 2, 2, 2, 2, 2, 2, 2, 2, 2, 2, 2, 2, 2, 2, 2, 2, 2, 2, 2, 2, 2, 2, 2, 2, 2, 2, 2, 2, 2, 2, 2, 2, 2, 2, 2, 2, 2, 2, 2, 2, 2, 2, 2, 2, 2, 2, 2, 2, 2, 2, 2, 2, 2, 2, 2, 2, 2, 2, 2, 2, 2, 2, 2, 2, 2, 2, 2, 2, 2, 2, 2, 2, 2, 2, 2, 2, 2, 2, 2, 2, 2, 2, 2, 2, 2, 2, 2, 2, 2, 2, 2, 2, 2, 2, 2, 2, 3 ),
 ( 0.000000000000000000, 1.000000000000000000 ),
 ( 0.000000000000000000, 0.004166666666666666609, 0.008333333333333333218, 0.01250000000000000069, 0.01666666666666666644, 0.02083333333333333218, 0.02500000000000000139, 0.02916666666666666713, 0.03333333333333333287, 0.03749999999999999861, 0.04166666666666666435, 0.04583333333333333010, 0.05000000000000000278, 0.05416666666666666852, 0.05833333333333333426, 0.06250000000000000000, 0.06666666666666666574, 0.07083333333333333148, 0.07499999999999999722, 0.07916666666666666297, 0.08333333333333332871, 0.08749999999999999445, 0.09166666666666666019, 0.09583333333333333981, 0.1000000000000000056, 0.1041666666666666713, 0.1083333333333333370, 0.1125000000000000028, 0.1166666666666666685, 0.1208333333333333343, 0.1250000000000000000, 0.1291666666666666796, 0.1333333333333333315, 0.1375000000000000111, 0.1416666666666666630, 0.1458333333333333426, 0.1499999999999999944, 0.1541666666666666741, 0.1583333333333333259, 0.1625000000000000056, 0.1666666666666666574, 0.1708333333333333370, 0.1749999999999999889, 0.1791666666666666685, 0.1833333333333333204, 0.1875000000000000000, 0.1916666666666666796, 0.1958333333333333315, 0.2000000000000000111, 0.2041666666666666630, 0.2083333333333333426, 0.2124999999999999944, 0.2166666666666666741, 0.2208333333333333259, 0.2250000000000000056, 0.2291666666666666574, 0.2333333333333333370, 0.2374999999999999889, 0.2416666666666666685, 0.2458333333333333204, 0.2500000000000000000, 0.2541666666666666519, 0.2583333333333333592, 0.2625000000000000111, 0.2666666666666666630, 0.2708333333333333148, 0.2750000000000000222, 0.2791666666666666741, 0.2833333333333333259, 0.2874999999999999778, 0.2916666666666666852, 0.2958333333333333370, 0.2999999999999999889, 0.3041666666666666408, 0.3083333333333333481, 0.3125000000000000000, 0.3166666666666666519, 0.3208333333333333592, 0.3250000000000000111, 0.3291666666666666630, 0.3333333333333333148, 0.3375000000000000222, 0.3416666666666666741, 0.3458333333333333259, 0.3499999999999999778, 0.3541666666666666852, 0.3583333333333333370, 0.3624999999999999889, 0.3666666666666666408, 0.3708333333333333481, 0.3750000000000000000, 0.3791666666666666519, 0.3833333333333333592, 0.3875000000000000111, 0.3916666666666666630, 0.3958333333333333148, 0.4000000000000000222, 0.4041666666666666741, 0.4083333333333333259, 0.4124999999999999778, 0.4166666666666666852, 0.4208333333333333370, 0.4249999999999999889, 0.4291666666666666408, 0.4333333333333333481, 0.4375000000000000000, 0.4416666666666666519, 0.4458333333333333592, 0.4500000000000000111, 0.4541666666666666630, 0.4583333333333333148, 0.4625000000000000222, 0.4666666666666666741, 0.4708333333333333259, 0.4749999999999999778, 0.4791666666666666852, 0.4833333333333333370, 0.4874999999999999889, 0.4916666666666666408, 0.4958333333333333481, 0.5000000000000000000, 0.5041666666666666519, 0.5083333333333333037, 0.5124999999999999556, 0.5166666666666667185, 0.5208333333333333703, 0.5250000000000000222, 0.5291666666666666741, 0.5333333333333333259, 0.5374999999999999778, 0.5416666666666666297, 0.5458333333333332815, 0.5500000000000000444, 0.5541666666666666963, 0.5583333333333333481, 0.5625000000000000000, 0.5666666666666666519, 0.5708333333333333037, 0.5749999999999999556, 0.5791666666666667185, 0.5833333333333333703, 0.5875000000000000222, 0.5916666666666666741, 0.5958333333333333259, 0.5999999999999999778, 0.6041666666666666297, 0.6083333333333332815, 0.6125000000000000444, 0.6166666666666666963, 0.6208333333333333481, 0.6250000000000000000, 0.6291666666666666519, 0.6333333333333333037, 0.6374999999999999556, 0.6416666666666667185, 0.6458333333333333703, 0.6500000000000000222, 0.6541666666666666741, 0.6583333333333333259, 0.6624999999999999778, 0.6666666666666666297, 0.6708333333333332815, 0.6750000000000000444, 0.6791666666666666963, 0.6833333333333333481, 0.6875000000000000000, 0.6916666666666666519, 0.6958333333333333037, 0.6999999999999999556, 0.7041666666666667185, 0.7083333333333333703, 0.7125000000000000222, 0.7166666666666666741, 0.7208333333333333259, 0.7249999999999999778, 0.7291666666666666297, 0.7333333333333332815, 0.7375000000000000444, 0.7416666666666666963, 0.7458333333333333481, 0.7500000000000000000, 0.7541666666666666519, 0.7583333333333333037, 0.7624999999999999556, 0.7666666666666667185, 0.7708333333333333703, 0.7750000000000000222, 0.7791666666666666741, 0.7833333333333333259, 0.7874999999999999778, 0.7916666666666666297, 0.7958333333333332815, 0.8000000000000000444, 0.8041666666666666963, 0.8083333333333333481, 0.8125000000000000000, 0.8166666666666666519, 0.8208333333333333037, 0.8249999999999999556, 0.8291666666666667185, 0.8333333333333333703, 0.8375000000000000222, 0.8416666666666666741, 0.8458333333333333259, 0.8499999999999999778, 0.8541666666666666297, 0.8583333333333332815, 0.8625000000000000444, 0.8666666666666666963, 0.8708333333333333481, 0.8750000000000000000, 0.8791666666666666519, 0.8833333333333333037, 0.8874999999999999556, 0.8916666666666667185, 0.8958333333333333703, 0.9000000000000000222, 0.9041666666666666741, 0.9083333333333333259, 0.9124999999999999778, 0.9166666666666666297, 0.9208333333333332815, 0.9250000000000000444, 0.9291666666666666963, 0.9333333333333333481, 0.9375000000000000000, 0.9416666666666666519, 0.9458333333333333037, 0.9499999999999999556, 0.9541666666666667185, 0.9583333333333333703, 0.9625000000000000222, 0.9666666666666666741, 0.9708333333333333259, 0.9749999999999999778, 0.9791666666666666297, 0.9833333333333332815, 0.9875000000000000444, 0.9916666666666666963, 0.9958333333333333481, 1.000000000000000000 ),
 .UNSPECIFIED. ) 
 GEOMETRIC_REPRESENTATION_ITEM ( )  RATIONAL_B_SPLINE_SURFACE ( (
 ( 1.000000000000000000, 0.8660254037844387076, 1.000000000000000000, 0.8660254037844387076, 1.000000000000000000, 0.8660254037844387076, 1.000000000000000000, 0.8660254037844387076, 1.000000000000000000, 0.8660254037844387076, 1.000000000000000000, 0.8660254037844387076, 1.000000000000000000, 0.8660254037844387076, 1.000000000000000000, 0.8660254037844387076, 1.000000000000000000, 0.8660254037844387076, 1.000000000000000000, 0.8660254037844387076, 1.000000000000000000, 0.8660254037844387076, 1.000000000000000000, 0.8660254037844387076, 1.000000000000000000, 0.8660254037844387076, 1.000000000000000000, 0.8660254037844387076, 1.000000000000000000, 0.8660254037844387076, 1.000000000000000000, 0.8660254037844387076, 1.000000000000000000, 0.8660254037844387076, 1.000000000000000000, 0.8660254037844387076, 1.000000000000000000, 0.8660254037844387076, 1.000000000000000000, 0.8660254037844387076, 1.000000000000000000, 0.8660254037844387076, 1.000000000000000000, 0.8660254037844387076, 1.000000000000000000, 0.8660254037844387076, 1.000000000000000000, 0.8660254037844387076, 1.000000000000000000, 0.8660254037844387076, 1.000000000000000000, 0.8660254037844387076, 1.000000000000000000, 0.8660254037844387076, 1.000000000000000000, 0.8660254037844387076, 1.000000000000000000, 0.8660254037844387076, 1.000000000000000000, 0.8660254037844387076, 1.000000000000000000, 0.8660254037844387076, 1.000000000000000000, 0.8660254037844387076, 1.000000000000000000, 0.8660254037844387076, 1.000000000000000000, 0.8660254037844387076, 1.000000000000000000, 0.8660254037844387076, 1.000000000000000000, 0.8660254037844387076, 1.000000000000000000, 0.8660254037844387076, 1.000000000000000000, 0.8660254037844387076, 1.000000000000000000, 0.8660254037844387076, 1.000000000000000000, 0.8660254037844387076, 1.000000000000000000, 0.8660254037844387076, 1.000000000000000000, 0.8660254037844387076, 1.000000000000000000, 0.8660254037844387076, 1.000000000000000000, 0.8660254037844387076, 1.000000000000000000, 0.8660254037844387076, 1.000000000000000000, 0.8660254037844387076, 1.000000000000000000, 0.8660254037844387076, 1.000000000000000000, 0.8660254037844387076, 1.000000000000000000, 0.8660254037844387076, 1.000000000000000000, 0.8660254037844387076, 1.000000000000000000, 0.8660254037844387076, 1.000000000000000000, 0.8660254037844387076, 1.000000000000000000, 0.8660254037844387076, 1.000000000000000000, 0.8660254037844387076, 1.000000000000000000, 0.8660254037844387076, 1.000000000000000000, 0.8660254037844387076, 1.000000000000000000, 0.8660254037844387076, 1.000000000000000000, 0.8660254037844387076, 1.000000000000000000, 0.8660254037844387076, 1.000000000000000000, 0.8660254037844387076, 1.000000000000000000, 0.8660254037844387076, 1.000000000000000000, 0.8660254037844387076, 1.000000000000000000, 0.8660254037844387076, 1.000000000000000000, 0.8660254037844387076, 1.000000000000000000, 0.8660254037844387076, 1.000000000000000000, 0.8660254037844387076, 1.000000000000000000, 0.8660254037844387076, 1.000000000000000000, 0.8660254037844387076, 1.000000000000000000, 0.8660254037844387076, 1.000000000000000000, 0.8660254037844387076, 1.000000000000000000, 0.8660254037844387076, 1.000000000000000000, 0.8660254037844387076, 1.000000000000000000, 0.8660254037844387076, 1.000000000000000000, 0.8660254037844387076, 1.000000000000000000, 0.8660254037844387076, 1.000000000000000000, 0.8660254037844387076, 1.000000000000000000, 0.8660254037844387076, 1.000000000000000000, 0.8660254037844387076, 1.000000000000000000, 0.8660254037844387076, 1.000000000000000000, 0.8660254037844387076, 1.000000000000000000, 0.8660254037844387076, 1.000000000000000000, 0.8660254037844387076, 1.000000000000000000, 0.8660254037844387076, 1.000000000000000000, 0.8660254037844387076, 1.000000000000000000, 0.8660254037844387076, 1.000000000000000000, 0.8660254037844387076, 1.000000000000000000, 0.8660254037844387076, 1.000000000000000000, 0.8660254037844387076, 1.000000000000000000, 0.8660254037844387076, 1.000000000000000000, 0.8660254037844387076, 1.000000000000000000, 0.8660254037844387076, 1.000000000000000000, 0.8660254037844387076, 1.000000000000000000, 0.8660254037844387076, 1.000000000000000000, 0.8660254037844387076, 1.000000000000000000, 0.8660254037844387076, 1.000000000000000000, 0.8660254037844387076, 1.000000000000000000, 0.8660254037844387076, 1.000000000000000000, 0.8660254037844387076, 1.000000000000000000, 0.8660254037844387076, 1.000000000000000000, 0.8660254037844387076, 1.000000000000000000, 0.8660254037844387076, 1.000000000000000000, 0.8660254037844387076, 1.000000000000000000, 0.8660254037844387076, 1.000000000000000000, 0.8660254037844387076, 1.000000000000000000, 0.8660254037844387076, 1.000000000000000000, 0.8660254037844387076, 1.000000000000000000, 0.8660254037844387076, 1.000000000000000000, 0.8660254037844387076, 1.000000000000000000, 0.8660254037844387076, 1.000000000000000000, 0.8660254037844387076, 1.000000000000000000, 0.8660254037844387076, 1.000000000000000000, 0.8660254037844387076, 1.000000000000000000, 0.8660254037844387076, 1.000000000000000000, 0.8660254037844387076, 1.000000000000000000, 0.8660254037844387076, 1.000000000000000000, 0.8660254037844387076, 1.000000000000000000, 0.8660254037844387076, 1.000000000000000000, 0.8660254037844387076, 1.000000000000000000, 0.8660254037844387076, 1.000000000000000000, 0.8660254037844387076, 1.000000000000000000, 0.8660254037844387076, 1.000000000000000000, 0.8660254037844387076, 1.000000000000000000, 0.8660254037844387076, 1.000000000000000000, 0.8660254037844387076, 1.000000000000000000, 0.8660254037844387076, 1.000000000000000000, 0.8660254037844387076, 1.000000000000000000, 0.8660254037844387076, 1.000000000000000000, 0.8660254037844387076, 1.000000000000000000, 0.8660254037844387076, 1.000000000000000000, 0.8660254037844387076, 1.000000000000000000, 0.8660254037844387076, 1.000000000000000000, 0.8660254037844387076, 1.000000000000000000, 0.8660254037844387076, 1.000000000000000000, 0.8660254037844387076, 1.000000000000000000, 0.8660254037844387076, 1.000000000000000000, 0.8660254037844387076, 1.000000000000000000, 0.8660254037844387076, 1.000000000000000000, 0.8660254037844387076, 1.000000000000000000, 0.8660254037844387076, 1.000000000000000000, 0.8660254037844387076, 1.000000000000000000, 0.8660254037844387076, 1.000000000000000000, 0.8660254037844387076, 1.000000000000000000, 0.8660254037844387076, 1.000000000000000000, 0.8660254037844387076, 1.000000000000000000, 0.8660254037844387076, 1.000000000000000000, 0.8660254037844387076, 1.000000000000000000, 0.8660254037844387076, 1.000000000000000000, 0.8660254037844387076, 1.000000000000000000, 0.8660254037844387076, 1.000000000000000000, 0.8660254037844387076, 1.000000000000000000, 0.8660254037844387076, 1.000000000000000000, 0.8660254037844387076, 1.000000000000000000, 0.8660254037844387076, 1.000000000000000000, 0.8660254037844387076, 1.000000000000000000, 0.8660254037844387076, 1.000000000000000000, 0.8660254037844387076, 1.000000000000000000, 0.8660254037844387076, 1.000000000000000000, 0.8660254037844387076, 1.000000000000000000, 0.8660254037844387076, 1.000000000000000000, 0.8660254037844387076, 1.000000000000000000, 0.8660254037844387076, 1.000000000000000000, 0.8660254037844387076, 1.000000000000000000, 0.8660254037844387076, 1.000000000000000000, 0.8660254037844387076, 1.000000000000000000, 0.8660254037844387076, 1.000000000000000000, 0.8660254037844387076, 1.000000000000000000, 0.8660254037844387076, 1.000000000000000000, 0.8660254037844387076, 1.000000000000000000, 0.8660254037844387076, 1.000000000000000000, 0.8660254037844387076, 1.000000000000000000, 0.8660254037844387076, 1.000000000000000000, 0.8660254037844387076, 1.000000000000000000, 0.8660254037844387076, 1.000000000000000000, 0.8660254037844387076, 1.000000000000000000, 0.8660254037844387076, 1.000000000000000000, 0.8660254037844387076, 1.000000000000000000, 0.8660254037844387076, 1.000000000000000000, 0.8660254037844387076, 1.000000000000000000, 0.8660254037844387076, 1.000000000000000000, 0.8660254037844387076, 1.000000000000000000, 0.8660254037844387076, 1.000000000000000000, 0.8660254037844387076, 1.000000000000000000, 0.8660254037844387076, 1.000000000000000000, 0.8660254037844387076, 1.000000000000000000, 0.8660254037844387076, 1.000000000000000000, 0.8660254037844387076, 1.000000000000000000, 0.8660254037844387076, 1.000000000000000000, 0.8660254037844387076, 1.000000000000000000, 0.8660254037844387076, 1.000000000000000000, 0.8660254037844387076, 1.000000000000000000, 0.8660254037844387076, 1.000000000000000000, 0.8660254037844387076, 1.000000000000000000, 0.8660254037844387076, 1.000000000000000000, 0.8660254037844387076, 1.000000000000000000, 0.8660254037844387076, 1.000000000000000000, 0.8660254037844387076, 1.000000000000000000, 0.8660254037844387076, 1.000000000000000000, 0.8660254037844387076, 1.000000000000000000, 0.8660254037844387076, 1.000000000000000000, 0.8660254037844387076, 1.000000000000000000, 0.8660254037844387076, 1.000000000000000000, 0.8660254037844387076, 1.000000000000000000, 0.8660254037844387076, 1.000000000000000000, 0.8660254037844387076, 1.000000000000000000, 0.8660254037844387076, 1.000000000000000000, 0.8660254037844387076, 1.000000000000000000, 0.8660254037844387076, 1.000000000000000000, 0.8660254037844387076, 1.000000000000000000, 0.8660254037844387076, 1.000000000000000000, 0.8660254037844387076, 1.000000000000000000, 0.8660254037844387076, 1.000000000000000000, 0.8660254037844387076, 1.000000000000000000, 0.8660254037844387076, 1.000000000000000000, 0.8660254037844387076, 1.000000000000000000, 0.8660254037844387076, 1.000000000000000000, 0.8660254037844387076, 1.000000000000000000, 0.8660254037844387076, 1.000000000000000000, 0.8660254037844387076, 1.000000000000000000, 0.8660254037844387076, 1.000000000000000000, 0.8660254037844387076, 1.000000000000000000, 0.8660254037844387076, 1.000000000000000000, 0.8660254037844387076, 1.000000000000000000, 0.8660254037844387076, 1.000000000000000000, 0.8660254037844387076, 1.000000000000000000, 0.8660254037844387076, 1.000000000000000000, 0.8660254037844387076, 1.000000000000000000, 0.8660254037844387076, 1.000000000000000000, 0.8660254037844387076, 1.000000000000000000, 0.8660254037844387076, 1.000000000000000000, 0.8660254037844387076, 1.000000000000000000, 0.8660254037844387076, 1.000000000000000000, 0.8660254037844387076, 1.000000000000000000, 0.8660254037844387076, 1.000000000000000000, 0.8660254037844387076, 1.000000000000000000, 0.8660254037844387076, 1.000000000000000000, 0.8660254037844387076, 1.000000000000000000, 0.8660254037844387076, 1.000000000000000000, 0.8660254037844387076, 1.000000000000000000, 0.8660254037844387076, 1.000000000000000000, 0.8660254037844387076, 1.000000000000000000),
 ( 1.000000000000000000, 0.8660254037844387076, 1.000000000000000000, 0.8660254037844387076, 1.000000000000000000, 0.8660254037844387076, 1.000000000000000000, 0.8660254037844387076, 1.000000000000000000, 0.8660254037844387076, 1.000000000000000000, 0.8660254037844387076, 1.000000000000000000, 0.8660254037844387076, 1.000000000000000000, 0.8660254037844387076, 1.000000000000000000, 0.8660254037844387076, 1.000000000000000000, 0.8660254037844387076, 1.000000000000000000, 0.8660254037844387076, 1.000000000000000000, 0.8660254037844387076, 1.000000000000000000, 0.8660254037844387076, 1.000000000000000000, 0.8660254037844387076, 1.000000000000000000, 0.8660254037844387076, 1.000000000000000000, 0.8660254037844387076, 1.000000000000000000, 0.8660254037844387076, 1.000000000000000000, 0.8660254037844387076, 1.000000000000000000, 0.8660254037844387076, 1.000000000000000000, 0.8660254037844387076, 1.000000000000000000, 0.8660254037844387076, 1.000000000000000000, 0.8660254037844387076, 1.000000000000000000, 0.8660254037844387076, 1.000000000000000000, 0.8660254037844387076, 1.000000000000000000, 0.8660254037844387076, 1.000000000000000000, 0.8660254037844387076, 1.000000000000000000, 0.8660254037844387076, 1.000000000000000000, 0.8660254037844387076, 1.000000000000000000, 0.8660254037844387076, 1.000000000000000000, 0.8660254037844387076, 1.000000000000000000, 0.8660254037844387076, 1.000000000000000000, 0.8660254037844387076, 1.000000000000000000, 0.8660254037844387076, 1.000000000000000000, 0.8660254037844387076, 1.000000000000000000, 0.8660254037844387076, 1.000000000000000000, 0.8660254037844387076, 1.000000000000000000, 0.8660254037844387076, 1.000000000000000000, 0.8660254037844387076, 1.000000000000000000, 0.8660254037844387076, 1.000000000000000000, 0.8660254037844387076, 1.000000000000000000, 0.8660254037844387076, 1.000000000000000000, 0.8660254037844387076, 1.000000000000000000, 0.8660254037844387076, 1.000000000000000000, 0.8660254037844387076, 1.000000000000000000, 0.8660254037844387076, 1.000000000000000000, 0.8660254037844387076, 1.000000000000000000, 0.8660254037844387076, 1.000000000000000000, 0.8660254037844387076, 1.000000000000000000, 0.8660254037844387076, 1.000000000000000000, 0.8660254037844387076, 1.000000000000000000, 0.8660254037844387076, 1.000000000000000000, 0.8660254037844387076, 1.000000000000000000, 0.8660254037844387076, 1.000000000000000000, 0.8660254037844387076, 1.000000000000000000, 0.8660254037844387076, 1.000000000000000000, 0.8660254037844387076, 1.000000000000000000, 0.8660254037844387076, 1.000000000000000000, 0.8660254037844387076, 1.000000000000000000, 0.8660254037844387076, 1.000000000000000000, 0.8660254037844387076, 1.000000000000000000, 0.8660254037844387076, 1.000000000000000000, 0.8660254037844387076, 1.000000000000000000, 0.8660254037844387076, 1.000000000000000000, 0.8660254037844387076, 1.000000000000000000, 0.8660254037844387076, 1.000000000000000000, 0.8660254037844387076, 1.000000000000000000, 0.8660254037844387076, 1.000000000000000000, 0.8660254037844387076, 1.000000000000000000, 0.8660254037844387076, 1.000000000000000000, 0.8660254037844387076, 1.000000000000000000, 0.8660254037844387076, 1.000000000000000000, 0.8660254037844387076, 1.000000000000000000, 0.8660254037844387076, 1.000000000000000000, 0.8660254037844387076, 1.000000000000000000, 0.8660254037844387076, 1.000000000000000000, 0.8660254037844387076, 1.000000000000000000, 0.8660254037844387076, 1.000000000000000000, 0.8660254037844387076, 1.000000000000000000, 0.8660254037844387076, 1.000000000000000000, 0.8660254037844387076, 1.000000000000000000, 0.8660254037844387076, 1.000000000000000000, 0.8660254037844387076, 1.000000000000000000, 0.8660254037844387076, 1.000000000000000000, 0.8660254037844387076, 1.000000000000000000, 0.8660254037844387076, 1.000000000000000000, 0.8660254037844387076, 1.000000000000000000, 0.8660254037844387076, 1.000000000000000000, 0.8660254037844387076, 1.000000000000000000, 0.8660254037844387076, 1.000000000000000000, 0.8660254037844387076, 1.000000000000000000, 0.8660254037844387076, 1.000000000000000000, 0.8660254037844387076, 1.000000000000000000, 0.8660254037844387076, 1.000000000000000000, 0.8660254037844387076, 1.000000000000000000, 0.8660254037844387076, 1.000000000000000000, 0.8660254037844387076, 1.000000000000000000, 0.8660254037844387076, 1.000000000000000000, 0.8660254037844387076, 1.000000000000000000, 0.8660254037844387076, 1.000000000000000000, 0.8660254037844387076, 1.000000000000000000, 0.8660254037844387076, 1.000000000000000000, 0.8660254037844387076, 1.000000000000000000, 0.8660254037844387076, 1.000000000000000000, 0.8660254037844387076, 1.000000000000000000, 0.8660254037844387076, 1.000000000000000000, 0.8660254037844387076, 1.000000000000000000, 0.8660254037844387076, 1.000000000000000000, 0.8660254037844387076, 1.000000000000000000, 0.8660254037844387076, 1.000000000000000000, 0.8660254037844387076, 1.000000000000000000, 0.8660254037844387076, 1.000000000000000000, 0.8660254037844387076, 1.000000000000000000, 0.8660254037844387076, 1.000000000000000000, 0.8660254037844387076, 1.000000000000000000, 0.8660254037844387076, 1.000000000000000000, 0.8660254037844387076, 1.000000000000000000, 0.8660254037844387076, 1.000000000000000000, 0.8660254037844387076, 1.000000000000000000, 0.8660254037844387076, 1.000000000000000000, 0.8660254037844387076, 1.000000000000000000, 0.8660254037844387076, 1.000000000000000000, 0.8660254037844387076, 1.000000000000000000, 0.8660254037844387076, 1.000000000000000000, 0.8660254037844387076, 1.000000000000000000, 0.8660254037844387076, 1.000000000000000000, 0.8660254037844387076, 1.000000000000000000, 0.8660254037844387076, 1.000000000000000000, 0.8660254037844387076, 1.000000000000000000, 0.8660254037844387076, 1.000000000000000000, 0.8660254037844387076, 1.000000000000000000, 0.8660254037844387076, 1.000000000000000000, 0.8660254037844387076, 1.000000000000000000, 0.8660254037844387076, 1.000000000000000000, 0.8660254037844387076, 1.000000000000000000, 0.8660254037844387076, 1.000000000000000000, 0.8660254037844387076, 1.000000000000000000, 0.8660254037844387076, 1.000000000000000000, 0.8660254037844387076, 1.000000000000000000, 0.8660254037844387076, 1.000000000000000000, 0.8660254037844387076, 1.000000000000000000, 0.8660254037844387076, 1.000000000000000000, 0.8660254037844387076, 1.000000000000000000, 0.8660254037844387076, 1.000000000000000000, 0.8660254037844387076, 1.000000000000000000, 0.8660254037844387076, 1.000000000000000000, 0.8660254037844387076, 1.000000000000000000, 0.8660254037844387076, 1.000000000000000000, 0.8660254037844387076, 1.000000000000000000, 0.8660254037844387076, 1.000000000000000000, 0.8660254037844387076, 1.000000000000000000, 0.8660254037844387076, 1.000000000000000000, 0.8660254037844387076, 1.000000000000000000, 0.8660254037844387076, 1.000000000000000000, 0.8660254037844387076, 1.000000000000000000, 0.8660254037844387076, 1.000000000000000000, 0.8660254037844387076, 1.000000000000000000, 0.8660254037844387076, 1.000000000000000000, 0.8660254037844387076, 1.000000000000000000, 0.8660254037844387076, 1.000000000000000000, 0.8660254037844387076, 1.000000000000000000, 0.8660254037844387076, 1.000000000000000000, 0.8660254037844387076, 1.000000000000000000, 0.8660254037844387076, 1.000000000000000000, 0.8660254037844387076, 1.000000000000000000, 0.8660254037844387076, 1.000000000000000000, 0.8660254037844387076, 1.000000000000000000, 0.8660254037844387076, 1.000000000000000000, 0.8660254037844387076, 1.000000000000000000, 0.8660254037844387076, 1.000000000000000000, 0.8660254037844387076, 1.000000000000000000, 0.8660254037844387076, 1.000000000000000000, 0.8660254037844387076, 1.000000000000000000, 0.8660254037844387076, 1.000000000000000000, 0.8660254037844387076, 1.000000000000000000, 0.8660254037844387076, 1.000000000000000000, 0.8660254037844387076, 1.000000000000000000, 0.8660254037844387076, 1.000000000000000000, 0.8660254037844387076, 1.000000000000000000, 0.8660254037844387076, 1.000000000000000000, 0.8660254037844387076, 1.000000000000000000, 0.8660254037844387076, 1.000000000000000000, 0.8660254037844387076, 1.000000000000000000, 0.8660254037844387076, 1.000000000000000000, 0.8660254037844387076, 1.000000000000000000, 0.8660254037844387076, 1.000000000000000000, 0.8660254037844387076, 1.000000000000000000, 0.8660254037844387076, 1.000000000000000000, 0.8660254037844387076, 1.000000000000000000, 0.8660254037844387076, 1.000000000000000000, 0.8660254037844387076, 1.000000000000000000, 0.8660254037844387076, 1.000000000000000000, 0.8660254037844387076, 1.000000000000000000, 0.8660254037844387076, 1.000000000000000000, 0.8660254037844387076, 1.000000000000000000, 0.8660254037844387076, 1.000000000000000000, 0.8660254037844387076, 1.000000000000000000, 0.8660254037844387076, 1.000000000000000000, 0.8660254037844387076, 1.000000000000000000, 0.8660254037844387076, 1.000000000000000000, 0.8660254037844387076, 1.000000000000000000, 0.8660254037844387076, 1.000000000000000000, 0.8660254037844387076, 1.000000000000000000, 0.8660254037844387076, 1.000000000000000000, 0.8660254037844387076, 1.000000000000000000, 0.8660254037844387076, 1.000000000000000000, 0.8660254037844387076, 1.000000000000000000, 0.8660254037844387076, 1.000000000000000000, 0.8660254037844387076, 1.000000000000000000, 0.8660254037844387076, 1.000000000000000000, 0.8660254037844387076, 1.000000000000000000, 0.8660254037844387076, 1.000000000000000000, 0.8660254037844387076, 1.000000000000000000, 0.8660254037844387076, 1.000000000000000000, 0.8660254037844387076, 1.000000000000000000, 0.8660254037844387076, 1.000000000000000000, 0.8660254037844387076, 1.000000000000000000, 0.8660254037844387076, 1.000000000000000000, 0.8660254037844387076, 1.000000000000000000, 0.8660254037844387076, 1.000000000000000000, 0.8660254037844387076, 1.000000000000000000, 0.8660254037844387076, 1.000000000000000000, 0.8660254037844387076, 1.000000000000000000, 0.8660254037844387076, 1.000000000000000000, 0.8660254037844387076, 1.000000000000000000, 0.8660254037844387076, 1.000000000000000000, 0.8660254037844387076, 1.000000000000000000, 0.8660254037844387076, 1.000000000000000000, 0.8660254037844387076, 1.000000000000000000, 0.8660254037844387076, 1.000000000000000000, 0.8660254037844387076, 1.000000000000000000, 0.8660254037844387076, 1.000000000000000000, 0.8660254037844387076, 1.000000000000000000, 0.8660254037844387076, 1.000000000000000000, 0.8660254037844387076, 1.000000000000000000, 0.8660254037844387076, 1.000000000000000000, 0.8660254037844387076, 1.000000000000000000, 0.8660254037844387076, 1.000000000000000000, 0.8660254037844387076, 1.000000000000000000, 0.8660254037844387076, 1.000000000000000000, 0.8660254037844387076, 1.000000000000000000) ) ) 
 REPRESENTATION_ITEM ( '' )  SURFACE ( )  );
#202191 = CARTESIAN_POINT ( 'NONE',  ( -6.724481002698115439, 10.78905223654906109, -0.7216878364870267237 ) ) ;
#202190 = AXIS2_PLACEMENT_3D ( 'NONE', #34505, #165579, #17173 ) ;
#202192 = CARTESIAN_POINT ( 'NONE',  ( 5.096939404094710468, 4.911127157724081371, 0.000000000000000000 ) ) ;
#202193 = CARTESIAN_POINT ( 'NONE',  ( 4.774442650306744085, 8.721933525333202653, -0.7998128361456281477 ) ) ;
#202194 = CARTESIAN_POINT ( 'NONE',  ( 6.596543124887806364, 2.046857425119428697, 0.3097440254393943881 ) ) ;
#202195 = CARTESIAN_POINT ( 'NONE',  ( 0.8433753223025289847, 0.3905737783656983431, -1.978056610397058712 ) ) ;
#202196 = CARTESIAN_POINT ( 'NONE',  ( -8.286004436246233951, 12.81875560892930466, 1.040834085586084257E-14 ) ) ;
#202197 = CARTESIAN_POINT ( 'NONE',  ( 5.692444392891300886, 7.734547439830227411, -1.599625672291281386 ) ) ;
#202198 = EDGE_CURVE ( 'NONE', #161718, #59844, #78910, .T. ) ;
#202199 = CARTESIAN_POINT ( 'NONE',  ( 0.8674257402763450031, 2.111068143204323455, -0.5878430487569612506 ) ) ;
#202200 = CARTESIAN_POINT ( 'NONE',  ( 5.813091150998386247, 1.612263477354998864, 0.8566026058636074803 ) ) ;
#202201 = CARTESIAN_POINT ( 'NONE',  ( -3.810004860640155311, 4.403759411290286252, 1.199719254218462483 ) ) ;
#202202 = AXIS2_PLACEMENT_3D ( 'NONE', #73230, #74327, #159838 ) ;
#202203 = EDGE_CURVE ( 'NONE', #135251, #18531, #127426, .T. ) ;
#202204 = CARTESIAN_POINT ( 'NONE',  ( 5.234856708652233515, 6.240325927249993576, 1.082531754730549078 ) ) ;
#202205 = CARTESIAN_POINT ( 'NONE',  ( 8.910733272679570049, 11.41894145625809820, -1.599625672291255185 ) ) ;
#202206 = CARTESIAN_POINT ( 'NONE',  ( 2.855963913973019963, 6.483708332943829866, 0.000000000000000000 ) ) ;
#202207 = CARTESIAN_POINT ( 'NONE',  ( 4.913904330310220558, 4.697586238308844919, 0.000000000000000000 ) ) ;
#202208 = ORIENTED_EDGE ( 'NONE', *, *, #170740, .T. ) ;
#202210 = CARTESIAN_POINT ( 'NONE',  ( 1.031890287230966985, -1.963566467742537069, 0.4430998199175004704 ) ) ;
#202209 = CARTESIAN_POINT ( 'NONE',  ( 3.280630368989821743, 1.663260157205956880, -0.7901080472864712156 ) ) ;
#202211 = CARTESIAN_POINT ( 'NONE',  ( 2.530986164375541581, 2.254368048762548593, -0.4469772407268405301 ) ) ;
#202213 = CARTESIAN_POINT ( 'NONE',  ( 0.9888277058803507380, 0.1293858107240040412, 1.856492687334237335 ) ) ;
#202212 = CARTESIAN_POINT ( 'NONE',  ( 4.690757960648234359, 4.574898496952131133, 0.7216878364870317197 ) ) ;
#202214 = CARTESIAN_POINT ( 'NONE',  ( -3.285556943750000070, -3.259374999522044014, 0.000000000000000000 ) ) ;
#202215 = CARTESIAN_POINT ( 'NONE',  ( -3.744022975668147790, 7.519777238254810925, -0.7998128361456281477 ) ) ;
#202216 = CARTESIAN_POINT ( 'NONE',  ( -9.523271317088290999, 14.62225410442589002, -7.301265812034692715 ) ) ;
#202217 = CARTESIAN_POINT ( 'NONE',  ( 4.412309042748480792, -1.912102599942141268, -0.04143165621695726192 ) ) ;
#202218 = CARTESIAN_POINT ( 'NONE',  ( -7.960608749518247151, 12.43912730774665576, 0.000000000000000000 ) ) ;
#202219 = CARTESIAN_POINT ( 'NONE',  ( 6.492506472431533560, 6.747478052702773788, -0.04572756507489894595 ) ) ;
#202220 = CARTESIAN_POINT ( 'NONE',  ( -3.471769853551161411, 6.208092708188416076, 1.199719254218452935 ) ) ;
#202222 = CARTESIAN_POINT ( 'NONE',  ( 2.500682550815761740, 1.503739811390795378, -1.112508705057350999 ) ) ;
#202221 = CARTESIAN_POINT ( 'NONE',  ( 3.263305109790759939, 2.039240668410980284, -0.4604351538632973639 ) ) ;
#202223 = CARTESIAN_POINT ( 'NONE',  ( 8.758204044748005401, 10.28062147603659504, 1.082531754730549967 ) ) ;
#202224 = CARTESIAN_POINT ( 'NONE',  ( 1.364683531249990311, 4.946875000341417916, 1.214306433183764966E-14 ) ) ;
#202225 = B_SPLINE_CURVE_WITH_KNOTS ( 'NONE', 3,
 ( #35949, #85774, #182191, #149715, #151855, #67353 ),
 .UNSPECIFIED., .F., .F.,
 ( 4, 2, 4 ),
 ( 0.000000000000000000, 0.0003258677429877276867, 0.0006517354859754553734 ),
 .UNSPECIFIED. ) ;
#202226 = CARTESIAN_POINT ( 'NONE',  ( 2.893823712666950598, -0.5078125688623453815, -1.664683006417116751 ) ) ;
#202227 = CARTESIAN_POINT ( 'NONE',  ( 4.660252114795294887, 6.460046772059735432, -1.599625672291256295 ) ) ;
#202229 = CARTESIAN_POINT ( 'NONE',  ( -0.004145910806160996512, 3.413539372451380949, -2.083557531367431270 ) ) ;
#202228 = CARTESIAN_POINT ( 'NONE',  ( -0.07538891330675576152, -7.154544010627095219, 9.499700864329900796 ) ) ;
#202230 = CARTESIAN_POINT ( 'NONE',  ( 3.474969472568560480, 0.04075424684168299505, -1.724569731432665121 ) ) ;
#202231 = CARTESIAN_POINT ( 'NONE',  ( 4.318054327947466575, 1.347776305887092185, -1.728067674571641898 ) ) ;
#202232 = CARTESIAN_POINT ( 'NONE',  ( 6.621690180768193379, -2.141820631849135292, 0.5315211216728524812 ) ) ;
#202233 = DIRECTION ( 'NONE',  ( 0.9782075119096779181, 0.1245777785628398998, -0.1661037047504532738 ) ) ;
#202234 = CARTESIAN_POINT ( 'NONE',  ( 3.221698175004498399, 0.3232067185854271552, -2.146787281877101439 ) ) ;
#202235 = CARTESIAN_POINT ( 'NONE',  ( 2.279681363911123970, 1.122676072794186908, 1.439608767588994365 ) ) ;
#202236 = CARTESIAN_POINT ( 'NONE',  ( 0.2390249890181182224, -0.1369461163322066299, -1.930431041017650395 ) ) ;
#202237 = CARTESIAN_POINT ( 'NONE',  ( 4.557876730116875663, 1.221875164117897539, 1.729014733294547801 ) ) ;
#202238 = ORIENTED_EDGE ( 'NONE', *, *, #59260, .T. ) ;
#202240 = CARTESIAN_POINT ( 'NONE',  ( 1.364683531249990311, 3.196875000341416140, 1.214306433183764966E-14 ) ) ;
#202239 = CARTESIAN_POINT ( 'NONE',  ( 5.161814014510654580, 1.128026202373041853, 1.995582457067740068 ) ) ;
#202241 = CARTESIAN_POINT ( 'NONE',  ( 6.620655732516647518, 0.01042156863438310939, 1.726407961933309920 ) ) ;
#202242 = EDGE_CURVE ( 'NONE', #121570, #45318, #40924, .T. ) ;
#202243 = CARTESIAN_POINT ( 'NONE',  ( 8.920375002787457319, 12.49452237230570084, 1.199719254218450271 ) ) ;
#202244 = CARTESIAN_POINT ( 'NONE',  ( -0.1046615654881309365, -0.1561857951268459388, -2.086345279447648249 ) ) ;
#202245 = CARTESIAN_POINT ( 'NONE',  ( -5.775410249741523394, 5.840326167560965231, 0.7216878364870317197 ) ) ;
#202246 = DIRECTION ( 'NONE',  ( 0.000000000000000000, -1.000000000000000000, 0.000000000000000000 ) ) ;
#202247 = B_SPLINE_CURVE_WITH_KNOTS ( 'NONE', 3,
 ( #27293, #146075, #98365, #149243, #131969, #84242 ),
 .UNSPECIFIED., .F., .F.,
 ( 4, 2, 4 ),
 ( 0.000000000000000000, 0.0003132070624402877746, 0.0006264141248805755492 ),
 .UNSPECIFIED. ) ;
#202248 = CARTESIAN_POINT ( 'NONE',  ( -6.521108698048791119, 6.710307690586118312, -0.7216878364870267237 ) ) ;
#202251 = B_SPLINE_CURVE_WITH_KNOTS ( 'NONE', 3,
 ( #158192, #42315, #9783, #154983 ),
 .UNSPECIFIED., .F., .F.,
 ( 4, 4 ),
 ( 0.0006294919072214896988, 0.001039439579420691623 ),
 .UNSPECIFIED. ) ;
#202250 = CARTESIAN_POINT ( 'NONE',  ( 1.499999999999993117, 10.88541666734946389, 0.8660254037844409281 ) ) ;
#202249 = CARTESIAN_POINT ( 'NONE',  ( 3.469446951953614189E-15, 5.900000000000023448, 1.214306433183764966E-14 ) ) ;
#202252 = ORIENTED_EDGE ( 'NONE', *, *, #196460, .T. ) ;
#202253 = CARTESIAN_POINT ( 'NONE',  ( 5.256482491209823138, 1.942542154241846397, -0.5404887192124520068 ) ) ;
#202255 = CARTESIAN_POINT ( 'NONE',  ( 4.223522562419862680, 0.2575905095270197287, -2.046390306194557418 ) ) ;
#202254 = CARTESIAN_POINT ( 'NONE',  ( 4.299907273828439180, 8.168308919441841454, 1.040834085586084257E-14 ) ) ;
#202257 = CARTESIAN_POINT ( 'NONE',  ( -0.2408018239684408812, 2.868499929943384874, -2.588695376639174484 ) ) ;
#202256 = CARTESIAN_POINT ( 'NONE',  ( 5.169401708560450004, 9.252995436621013425, 0.000000000000000000 ) ) ;
#202258 = CARTESIAN_POINT ( 'NONE',  ( 7.201315867513990554, 8.430565262634994284, -1.199719254218452047 ) ) ;
#202259 = CARTESIAN_POINT ( 'NONE',  ( 3.285556943749998737, -0.6052083328553753416, -1.896917185911906500 ) ) ;
#202260 = CARTESIAN_POINT ( 'NONE',  ( -0.1265553566730630297, 3.463015919485879834, -2.076146368081344118 ) ) ;
#202261 = CARTESIAN_POINT ( 'NONE',  ( 0.7266515212380560973, 0.1555473773823950467, 2.084908828405390491 ) ) ;
#202262 = CARTESIAN_POINT ( 'NONE',  ( 4.447888798048591497, -1.802416534049579910, -0.9041112711936499791 ) ) ;
#202263 = CARTESIAN_POINT ( 'NONE',  ( 3.720104550828434942, 1.749555917645674530, 0.5740644926693627692 ) ) ;
#202264 = CARTESIAN_POINT ( 'NONE',  ( 5.632522751473472589, 8.658694745772667289, -1.199719254218440723 ) ) ;
#202265 = CARTESIAN_POINT ( 'NONE',  ( 0.9731894095723004900, 1.663878915475509812, -0.4539961392346722469 ) ) ;
#202266 = CARTESIAN_POINT ( 'NONE',  ( -3.789667630219657912, 4.380032642466370696, 1.199719254218462483 ) ) ;
#202267 = CARTESIAN_POINT ( 'NONE',  ( 1.354533853113936814, 0.1633331948888619711, -2.292934881128176450 ) ) ;
#202268 = CARTESIAN_POINT ( 'NONE',  ( -6.911959384868566758, 6.958374125301778790, 1.040834085586084257E-14 ) ) ;
#202269 = CARTESIAN_POINT ( 'NONE',  ( 0.2107632190684857465, -0.9678151086435597961, -2.042474306115627414 ) ) ;
#202270 = CARTESIAN_POINT ( 'NONE',  ( 2.983145545965359080, -0.1552688264333592638, -2.100405815202969873 ) ) ;
#202271 = CARTESIAN_POINT ( 'NONE',  ( -3.623772196602547346, 7.449761006003425834, 0.000000000000000000 ) ) ;
#202272 = CARTESIAN_POINT ( 'NONE',  ( 6.479907352327590964, 9.647310113435821677, 1.199719254218462483 ) ) ;
#202273 = CARTESIAN_POINT ( 'NONE',  ( 4.841670253411575864, 8.662716039039905169, -0.7216878364870458196 ) ) ;
#202274 = CARTESIAN_POINT ( 'NONE',  ( 5.500000000000004441, -3.262149103155007084E-13, -2.052068128417942283 ) ) ;
#202275 = CARTESIAN_POINT ( 'NONE',  ( -6.093499974338126179, 9.196501505781426999, -1.199719254218440723 ) ) ;
#202276 = CARTESIAN_POINT ( 'NONE',  ( 7.592202833528386208, 7.959917515312338487, 1.040834085586084257E-14 ) ) ;
#202277 = CARTESIAN_POINT ( 'NONE',  ( 4.188544580023894071, 7.586160867502751870, 0.8937768461303140510 ) ) ;
#202278 = CARTESIAN_POINT ( 'NONE',  ( -2.950870989268691957, 6.594433254122103349, -0.7998128361456281477 ) ) ;
#202279 = CARTESIAN_POINT ( 'NONE',  ( 5.502238596801645620, -0.9988962762179309784, 1.984187878789472892 ) ) ;
#202280 = CARTESIAN_POINT ( 'NONE',  ( 2.484552680892829546, -0.3758780662847274190, -2.158817762932266682 ) ) ;
#202281 = CARTESIAN_POINT ( 'NONE',  ( -4.737684612971557740, 7.614716917520386374, 1.199719254218464037 ) ) ;
#202282 = CARTESIAN_POINT ( 'NONE',  ( -4.821859908315634158, 5.654533310236863564, 1.199719254218452935 ) ) ;
#202283 = CARTESIAN_POINT ( 'NONE',  ( 5.459412808053472510, 1.602871733476991079, 1.130958114227413436 ) ) ;
#202284 =( BOUNDED_SURFACE ( )  B_SPLINE_SURFACE ( 3, 2, ( 
 ( #64677, #92949, #193616 ),
 ( #158995, #76665, #97211 ),
 ( #78790, #142779, #208785 ),
 ( #96149, #60415, #79861 ),
 ( #95080, #31136, #27923 ),
 ( #179517, #210920, #147026 ),
 ( #61487, #45257, #163263 ),
 ( #192536, #94018, #175260 ),
 ( #110310, #211982, #191471 ),
 ( #111376, #11661, #213049 ),
 ( #14845, #176318, #43138 ),
 ( #77734, #143856, #26845 ),
 ( #44190, #145970, #209848 ),
 ( #127652, #63622, #80935 ),
 ( #177380, #161129, #144913 ),
 ( #62546, #128709, #194678 ) ),
 .UNSPECIFIED., .F., .F., .T. ) 
 B_SPLINE_SURFACE_WITH_KNOTS ( ( 4, 2, 2, 2, 2, 2, 2, 4 ),
 ( 3, 3 ),
 ( -3.469446951953614189E-18, 0.0005295610108084591698, 0.001059122021616921809, 0.001588683032425384448, 0.002118244043233847088, 0.002647805054042309727, 0.003177366064850772366, 0.004236488086467697645 ),
 ( 0.000000000000000000, 1.000000000000000000 ),
 .UNSPECIFIED. ) 
 GEOMETRIC_REPRESENTATION_ITEM ( )  RATIONAL_B_SPLINE_SURFACE ( (
 ( 1.000000000000000000, 0.8434758251109465421, 1.000000000000000000),
 ( 1.000000000000000000, 0.8438484666245520405, 1.000000000000000000),
 ( 1.000000000000000000, 0.8442947513603508147, 1.000000000000000000),
 ( 1.000000000000000000, 0.8452199691704415097, 1.000000000000000000),
 ( 1.000000000000000000, 0.8457194463841322118, 1.000000000000000000),
 ( 1.000000000000000000, 0.8468087058708519965, 1.000000000000000000),
 ( 1.000000000000000000, 0.8474271749261985676, 1.000000000000000000),
 ( 1.000000000000000000, 0.8486845056840492951, 1.000000000000000000),
 ( 1.000000000000000000, 0.8493328185060563529, 1.000000000000000000),
 ( 1.000000000000000000, 0.8502002772864952762, 1.000000000000000000),
 ( 1.000000000000000000, 0.8502729042284375982, 1.000000000000000000),
 ( 1.000000000000000000, 0.8504148911931121990, 1.000000000000000000),
 ( 1.000000000000000000, 0.8504126782990119038, 1.000000000000000000),
 ( 1.000000000000000000, 0.8505517453013814455, 1.000000000000000000),
 ( 1.000000000000000000, 0.8508995438024010705, 1.000000000000000000),
 ( 1.000000000000000000, 0.8509629433967770273, 1.000000000000000000) ) ) 
 REPRESENTATION_ITEM ( '' )  SURFACE ( )  );
#202285 = CARTESIAN_POINT ( 'NONE',  ( 1.364683531249988757, 2.384375000341422357, 1.214306433183764966E-14 ) ) ;
#202286 = CARTESIAN_POINT ( 'NONE',  ( 6.610000000000028741, 1.211438232176115237, 2.390254139237833808 ) ) ;
#202287 = CARTESIAN_POINT ( 'NONE',  ( -4.446711195602239819, 8.131654128270509929, -0.7216878364870267237 ) ) ;
#202288 = CARTESIAN_POINT ( 'NONE',  ( 4.060867369437678676, 0.5686956411946364476, 2.042824496258560441 ) ) ;
#202289 = CARTESIAN_POINT ( 'NONE',  ( -2.986538976760251263, 6.706322249520737522, -0.7998128361456481317 ) ) ;
#202290 = ORIENTED_EDGE ( 'NONE', *, *, #206026, .F. ) ;
#202292 = CARTESIAN_POINT ( 'NONE',  ( -1.436838838544729491, 7.449283400311743186, -4.203727439823575551 ) ) ;
#202291 = CARTESIAN_POINT ( 'NONE',  ( -6.305950844131887223, 6.529566537674873494, 0.000000000000000000 ) ) ;
#202293 = CARTESIAN_POINT ( 'NONE',  ( 7.305145839664861640, 7.417091655897478653, 0.7998128361456341429 ) ) ;
#202294 = CARTESIAN_POINT ( 'NONE',  ( 5.214338956685346638, 1.703448749313410282, 0.6994016148276982481 ) ) ;
#202295 = CARTESIAN_POINT ( 'NONE',  ( 0.000000000000000000, 0.08000000000000020983, 0.000000000000000000 ) ) ;
#202296 = CARTESIAN_POINT ( 'NONE',  ( -1.364683531250012516, 2.551041667008089320, -0.7879004041258289570 ) ) ;
#202297 = CARTESIAN_POINT ( 'NONE',  ( 0.6611568445531558202, 0.8558493542428649015, 1.515405575314775044 ) ) ;
#202298 = CARTESIAN_POINT ( 'NONE',  ( -1.500000000000015099, 11.26041666734946567, -0.8660254037844309360 ) ) ;
#202299 = CARTESIAN_POINT ( 'NONE',  ( 0.6823417656249882723, -0.8447916663252494907, 1.181850606188755259 ) ) ;
#202300 = CARTESIAN_POINT ( 'NONE',  ( 3.092648394857516525, 6.449253795920727228, -0.4031905389056261724 ) ) ;
#202301 = CARTESIAN_POINT ( 'NONE',  ( 5.418883921851007202, 1.995750516393671514, 0.8311057252617033431 ) ) ;
#202302 = VECTOR ( 'NONE', #72797, 1000.000000000000000 ) ;
#202303 = CARTESIAN_POINT ( 'NONE',  ( -4.948889764188092677, 5.732458465429559169, 1.199719254218462483 ) ) ;
#202304 = CARTESIAN_POINT ( 'NONE',  ( -7.876924059415400414, 9.252461493148505411, 1.082531754730558626 ) ) ;
#202305 = CARTESIAN_POINT ( 'NONE',  ( 4.399409362686744096, 1.734418756986338295, 1.290045131933370781 ) ) ;
#202306 = CARTESIAN_POINT ( 'NONE',  ( -0.6823417656250212460, 2.301041667008084435, 1.181850606188767472 ) ) ;
#202307 = CARTESIAN_POINT ( 'NONE',  ( 4.903572647403447782, -0.5284346980384787562, 1.899126047080600621 ) ) ;
#202308 = CARTESIAN_POINT ( 'NONE',  ( 4.499182623014930549, 1.700326773844270667, 0.3381245445180857123 ) ) ;
#202309 = VECTOR ( 'NONE', #199002, 1000.000000000000000 ) ;
#202310 = CARTESIAN_POINT ( 'NONE',  ( 0.4861908890553789941, -2.175720422541329580, -0.2624175912114696252 ) ) ;
#202311 = CARTESIAN_POINT ( 'NONE',  ( 2.766999470516241288, -1.591810197153446182, 1.670866638877396060 ) ) ;
#202312 = CARTESIAN_POINT ( 'NONE',  ( 4.218082229858637788, -1.055972844705153291, -1.769506188133779467 ) ) ;
#202313 = CARTESIAN_POINT ( 'NONE',  ( 6.321825213571911739, 1.114395046473240392, -1.590342819258899532 ) ) ;
#202315 = EDGE_LOOP ( 'NONE', ( #159080, #122083, #106602, #48801 ) ) ;
#202314 = CARTESIAN_POINT ( 'NONE',  ( -8.175203438916030407, 8.640084888264587093, 0.7216878364870578100 ) ) ;
#202316 = B_SPLINE_CURVE_WITH_KNOTS ( 'NONE', 3,
 ( #85928, #135756, #116351, #201779, #119556, #16636 ),
 .UNSPECIFIED., .F., .F.,
 ( 4, 2, 4 ),
 ( 0.000000000000000000, 0.0003767643964918269734, 0.0007535287929836536214 ),
 .UNSPECIFIED. ) ;
#202317 = CARTESIAN_POINT ( 'NONE',  ( -6.005335696210345020, 5.970922831858983315, 0.7998128361456281477 ) ) ;
#202318 = CARTESIAN_POINT ( 'NONE',  ( 0.000000000000000000, 4.400000000000001243, 0.000000000000000000 ) ) ;
#202319 = CARTESIAN_POINT ( 'NONE',  ( -7.659993601596726265, 8.039006744725394782, -0.7216878364870267237 ) ) ;
#202320 = EDGE_CURVE ( 'NONE', #758, #28052, #47736, .T. ) ;
#202321 = CARTESIAN_POINT ( 'NONE',  ( 3.821466819111440927, -0.1649144712266135959, 2.200675313789305143 ) ) ;
#202322 = CARTESIAN_POINT ( 'NONE',  ( 3.285556943750000514, -2.501041666188708046, 1.896917185911906500 ) ) ;
#202323 = CARTESIAN_POINT ( 'NONE',  ( 0.8306204695724854759, -1.749664030167530138, -0.6342216345150762935 ) ) ;
#202324 = CARTESIAN_POINT ( 'NONE',  ( 1.493132593725484458, 3.264523918964489457, -0.1629718138060145538 ) ) ;
#202325 = CARTESIAN_POINT ( 'NONE',  ( -1.201851678989727383E-14, 5.368750000682816825, -1.732050807568863648 ) ) ;
#202326 = CARTESIAN_POINT ( 'NONE',  ( 6.180809796670631684, 5.328980321105058593, -2.499999999999329425 ) ) ;
#202328 = CARTESIAN_POINT ( 'NONE',  ( 6.925078400183521055, 4.691537398408025972, 2.606905763235977336 ) ) ;
#202327 = CARTESIAN_POINT ( 'NONE',  ( -6.358822508390924888, 6.928531665952419871, -0.8607971499900844981 ) ) ;
#202329 = ORIENTED_EDGE ( 'NONE', *, *, #171612, .F. ) ;
#202330 = CARTESIAN_POINT ( 'NONE',  ( 3.133719265644947960, -1.383057153600345535, -1.528062560492246202 ) ) ;
#202331 = CARTESIAN_POINT ( 'NONE',  ( 1.360316468749994012, 2.265625000341386919, -1.387778780781445676E-14 ) ) ;
#202332 = UNCERTAINTY_MEASURE_WITH_UNIT (LENGTH_MEASURE( 1.000000000000000082E-05 ), #130101, 'distance_accuracy_value', 'NONE');
#202333 = CARTESIAN_POINT ( 'NONE',  ( -6.175902666224832416, 7.163973517805802160, -1.199719254218446718 ) ) ;
#202334 = CARTESIAN_POINT ( 'NONE',  ( 2.998324526916512411, 6.649795714711241423, 0.000000000000000000 ) ) ;
#202335 = CARTESIAN_POINT ( 'NONE',  ( 2.131779597171743923, -1.345384690298248698, -1.561254108789570827 ) ) ;
#202336 = CARTESIAN_POINT ( 'NONE',  ( 0.6823417656249934904, 13.19270833367473195, 1.181850606188764807 ) ) ;
#202337 = CARTESIAN_POINT ( 'NONE',  ( 4.794779880727245036, 8.745660294157122649, -0.7998128361456281477 ) ) ;
#202338 = CARTESIAN_POINT ( 'NONE',  ( 2.281615103653998666, 2.664038801896126962, 2.456549816139060649 ) ) ;
#202339 = COLOUR_RGB ( '', 0.08235294, 0.09019608, 0.10196078) ;
#202340 = CARTESIAN_POINT ( 'NONE',  ( 5.971336403843030105, 0.1662174427981797931, -2.200672837095698497 ) ) ;
#202341 = CARTESIAN_POINT ( 'NONE',  ( 1.528841242883504981, 2.082761121880230881, 0.5781018612496248155 ) ) ;
#202342 = CARTESIAN_POINT ( 'NONE',  ( -5.260200412422213923, 6.199617238323108737, -1.082531754730544860 ) ) ;
#202343 = CARTESIAN_POINT ( 'NONE',  ( 0.9894706735516716201, -0.4852629857438545691, 1.957171443305204761 ) ) ;
#202344 = ADVANCED_FACE ( 'NONE', ( #170030 ), #137561, .T. ) ;
#202345 = CARTESIAN_POINT ( 'NONE',  ( -1.734723475976807094E-15, 2.999999999999988898, -6.938893903907228378E-15 ) ) ;
#202346 = EDGE_CURVE ( 'NONE', #105328, #193413, #41134, .T. ) ;
#202347 = CARTESIAN_POINT ( 'NONE',  ( 6.235011639695051677, 1.786057601157978958, 0.6837302122261401660 ) ) ;
#202349 = VERTEX_POINT ( 'NONE', #158078 ) ;
#202348 = FACE_OUTER_BOUND ( 'NONE', #117249, .T. ) ;
#202350 = CARTESIAN_POINT ( 'NONE',  ( 2.219420098953532428, -1.815089452277141691, 0.4520615115926190919 ) ) ;
#202351 =( GEOMETRIC_REPRESENTATION_CONTEXT ( 3 ) GLOBAL_UNCERTAINTY_ASSIGNED_CONTEXT ( ( #49652 ) ) GLOBAL_UNIT_ASSIGNED_CONTEXT ( ( #51684, #1821, #88455 ) ) REPRESENTATION_CONTEXT ( 'NONE', 'WORKASPACE' ) );
#202352 = CARTESIAN_POINT ( 'NONE',  ( 3.432827581131673522, -1.645759781613131967, 1.164986487700324425 ) ) ;
#202354 = CARTESIAN_POINT ( 'NONE',  ( 5.510910596163088569E-16, 2.499999999999998668, 4.500000000000000000 ) ) ;
#202353 = CARTESIAN_POINT ( 'NONE',  ( -1.364683531250000748, 1.259375000341421469, 0.000000000000000000 ) ) ;
#202356 = CARTESIAN_POINT ( 'NONE',  ( 4.617860632714274161, -2.065554989951523535, 0.4101935312739966588 ) ) ;
#202355 = CARTESIAN_POINT ( 'NONE',  ( -7.232384877886063990, 10.52520055992070525, -1.199719254218446718 ) ) ;
#202357 = CARTESIAN_POINT ( 'NONE',  ( 7.416473721875251890, 8.611306416064660851, 1.199719254218462483 ) ) ;
#202359 = CARTESIAN_POINT ( 'NONE',  ( -6.015013705957189316, 10.16926642359206134, 0.7998128361456481317 ) ) ;
#202358 = CARTESIAN_POINT ( 'NONE',  ( 3.400062661977048428, 7.188766548940353829, -1.734723475976807094E-15 ) ) ;
#202360 = CARTESIAN_POINT ( 'NONE',  ( -0.4355862708380086046, -6.583980363594969631, -9.606148981167432765 ) ) ;
#202361 = CARTESIAN_POINT ( 'NONE',  ( 4.922131295886445379, -2.009687048479208205, 0.2019785858936548328 ) ) ;
#202362 = CARTESIAN_POINT ( 'NONE',  ( -0.7500000000000006661, -0.8604166659838472508, -1.299038105676652011 ) ) ;
#202363 = CIRCLE ( 'NONE', #109078, 0.08000000000000020983 ) ;
#202364 = CARTESIAN_POINT ( 'NONE',  ( 1.129816159781659390, 1.988900438959967376, -0.5462022044933153575 ) ) ;
#202365 = CARTESIAN_POINT ( 'NONE',  ( 8.107412671292035355, 10.48173408797264194, 1.443375672974076540 ) ) ;
#202366 = EDGE_CURVE ( 'NONE', #68875, #110911, #151611, .T. ) ;
#202367 = CARTESIAN_POINT ( 'NONE',  ( 6.011032505573889573, 1.903242638633116712, 1.024824547371510075 ) ) ;
#202368 = CARTESIAN_POINT ( 'NONE',  ( 7.700104897918568447, 7.948153567185284096, 0.000000000000000000 ) ) ;
#202369 = CARTESIAN_POINT ( 'NONE',  ( -1.364683531250000748, -0.4281249996585800854, 0.000000000000000000 ) ) ;
#202371 = FACE_OUTER_BOUND ( 'NONE', #161563, .T. ) ;
#202370 = CARTESIAN_POINT ( 'NONE',  ( 4.960304097753311936, 6.880383762169266504, 1.599625672291268286 ) ) ;
#202372 = CARTESIAN_POINT ( 'NONE',  ( 8.080296363620359301, 8.529359967086321603, 1.040834085586084257E-14 ) ) ;
#202374 = CARTESIAN_POINT ( 'NONE',  ( -3.633158051037565617, 3.497935290439206923, -2.447764745243742546 ) ) ;
#202373 = CARTESIAN_POINT ( 'NONE',  ( 3.033805354627703288, 2.062495667156949430, -0.6785788507157832772 ) ) ;
#202376 = CARTESIAN_POINT ( 'NONE',  ( 1.733694375844633706, 1.821329977863223926, 0.2691589665217360983 ) ) ;
#202375 = CARTESIAN_POINT ( 'NONE',  ( -6.724481002698138532, 6.947575379343695623, -0.7216878364870278340 ) ) ;
#202377 = CARTESIAN_POINT ( 'NONE',  ( -0.6823417656249969321, 3.217708333674754062, -1.181850606188749264 ) ) ;
#202378 = CARTESIAN_POINT ( 'NONE',  ( 2.982162443640325566, -2.159563097825706990, -0.3721831821169723775 ) ) ;
#202379 = CARTESIAN_POINT ( 'NONE',  ( 6.883263157960358924, 4.692138088316172073, 2.616388454592593504 ) ) ;
#202380 = CARTESIAN_POINT ( 'NONE',  ( 5.014671263542332724, 1.563880152264264245, -1.635232377595864595 ) ) ;
#202381 = CARTESIAN_POINT ( 'NONE',  ( -5.747767057189642870, 8.793146435774861658, -1.199719254218440723 ) ) ;
#202382 = CARTESIAN_POINT ( 'NONE',  ( -1.364683531249997417, 5.571875000341417916, 1.214306433183764966E-14 ) ) ;
#202383 = CARTESIAN_POINT ( 'NONE',  ( 5.551963943121584144, 7.421064284658021037, -1.246246109899084020 ) ) ;
#202384 = CARTESIAN_POINT ( 'NONE',  ( -1.402160292154681736E-14, 13.31250000000000000, 1.732050807568881190 ) ) ;
#202385 = CARTESIAN_POINT ( 'NONE',  ( -4.624739795592931912, 8.409630504918133909, -0.7216878364870338292 ) ) ;
#202386 = CARTESIAN_POINT ( 'NONE',  ( 6.265276383290871109, 7.442482214328385304, -1.082531754730548412 ) ) ;
#202387 = CARTESIAN_POINT ( 'NONE',  ( 5.255052661293587946, -1.495254947996208950, -0.9463502368073344329 ) ) ;
#202388 = CARTESIAN_POINT ( 'NONE',  ( 8.259941899223605333, 10.65968485389279508, -1.599625672291268286 ) ) ;
#202389 = CARTESIAN_POINT ( 'NONE',  ( 2.380028573532027458, 1.294904889207445509, 1.660730631172540495 ) ) ;
#202391 = CARTESIAN_POINT ( 'NONE',  ( -1.499999999999997780, 2.650000000000020339, 1.214306433183764966E-14 ) ) ;
#202390 = CARTESIAN_POINT ( 'NONE',  ( -1.364683531250000748, 12.10937500034139980, 0.000000000000000000 ) ) ;
#202392 = CARTESIAN_POINT ( 'NONE',  ( 2.242574321144190641, -1.930940592676654965, -0.3871509593617681322 ) ) ;
#202393 = LINE ( 'NONE', #104944, #187734 ) ;
#202394 = CARTESIAN_POINT ( 'NONE',  ( 1.499999999999990896, 5.306250000682820378, 1.214306433183764966E-14 ) ) ;
#202396 = ORIENTED_EDGE ( 'NONE', *, *, #89006, .T. ) ;
#202395 = CARTESIAN_POINT ( 'NONE',  ( 6.047087830114247886, 0.1867083960328217995, 1.801967238635309165 ) ) ;
#202397 = CARTESIAN_POINT ( 'NONE',  ( 6.982085921357777281, 7.248114451113292667, 1.040834085586084257E-14 ) ) ;
#202398 = CARTESIAN_POINT ( 'NONE',  ( -1.364683531250014514, -1.157291666325248158, 0.7879004041258379498 ) ) ;
#202399 = CARTESIAN_POINT ( 'NONE',  ( 5.383624799460786647, 1.257121276536907750, 1.385457850027263405 ) ) ;
#202400 = CIRCLE ( 'NONE', #116056, 4.000000000000000000 ) ;
#202401 = CARTESIAN_POINT ( 'NONE',  ( 5.260626886859606444, -0.6923115906582855139, -1.951227211109484383 ) ) ;
#202402 = CARTESIAN_POINT ( 'NONE',  ( -4.299344108864949554, 8.030002203735486788, -0.7216878364870338292 ) ) ;
#202403 = DIRECTION ( 'NONE',  ( -0.6507913734559627184, -0.7592566023653016805, 0.000000000000000000 ) ) ;
#202404 = CARTESIAN_POINT ( 'NONE',  ( -1.500000000000013101, 0.4208333333333572068, 0.8660254037844403729 ) ) ;
#202405 = CARTESIAN_POINT ( 'NONE',  ( 8.046927864910717432, 9.346836249606042202, 1.199719254218462483 ) ) ;
#202406 = CARTESIAN_POINT ( 'NONE',  ( -7.831806290188425557, 12.28885777186185990, -0.7998128361456281477 ) ) ;
#202407 = CARTESIAN_POINT ( 'NONE',  ( 6.866278450678116485, 6.975356045404744521, 0.000000000000000000 ) ) ;
#202408 = CARTESIAN_POINT ( 'NONE',  ( 0.6823417656249882723, -0.07395833299191079124, -1.181850606188749264 ) ) ;
#202409 = CARTESIAN_POINT ( 'NONE',  ( 0.7499999999999902300, 1.733333333333357595, 1.299038105676657340 ) ) ;
#202411 = CARTESIAN_POINT ( 'NONE',  ( 4.961394147597008697, 7.875711374583454827, -1.199719254218452047 ) ) ;
#202410 = CARTESIAN_POINT ( 'NONE',  ( 5.424254290899477304, 0.9654600744411747648, 1.707767180430696641 ) ) ;
#202412 = CARTESIAN_POINT ( 'NONE',  ( 3.181017370561005198, -0.9912469002804729090, -1.755500664876320727 ) ) ;
#202413 = EDGE_CURVE ( 'NONE', #157260, #90864, #141292, .T. ) ;
#202414 = CARTESIAN_POINT ( 'NONE',  ( 2.588968054610871317, 1.620874238694985925, 1.020808031020562501 ) ) ;
#202415 = CARTESIAN_POINT ( 'NONE',  ( -0.7500000000000006661, 2.889583334016148974, -1.299038105676652011 ) ) ;
#202416 = CARTESIAN_POINT ( 'NONE',  ( 0.9080814035550346386, -0.9900877184637231210, -1.955254813705724404 ) ) ;
#202417 = CARTESIAN_POINT ( 'NONE',  ( 0.2331713839410602396, 2.030351879425442707, -2.369071045443218004 ) ) ;
#202418 = CARTESIAN_POINT ( 'NONE',  ( 2.108475139129362574, 1.389272611029747750, -1.252756881873963168 ) ) ;
#202419 = CARTESIAN_POINT ( 'NONE',  ( 1.364683531249990311, 5.613541667008087543, 0.7879004041258500513 ) ) ;
#202420 = CARTESIAN_POINT ( 'NONE',  ( 4.131111929362305091, 1.842322257054655354, 0.8120569753113301426 ) ) ;
#202421 = CARTESIAN_POINT ( 'NONE',  ( -6.184490626128011925, 10.36698949712469364, -0.7998128361456291469 ) ) ;
#202423 = CARTESIAN_POINT ( 'NONE',  ( 4.534827772108455335, -1.699605468249162588, 1.262326912638973786 ) ) ;
#202422 = CARTESIAN_POINT ( 'NONE',  ( -5.260200412422208593, 7.159986452624450770, -1.443375672974053447 ) ) ;
#202424 = CYLINDRICAL_SURFACE ( 'NONE', #42328, 1.500000000000000222 ) ;
#202425 = CARTESIAN_POINT ( 'NONE',  ( 6.320769956279724155, -1.466918727022302971, 1.461273828345016845 ) ) ;
#202427 = DIRECTION ( 'NONE',  ( 8.638326563840814399E-31, 0.000000000000000000, 1.000000000000000000 ) ) ;
#202426 = CARTESIAN_POINT ( 'NONE',  ( 1.716468666696397971, 1.951974251796151583, 0.7495149520271927601 ) ) ;
#202429 = ORIENTED_EDGE ( 'NONE', *, *, #27277, .T. ) ;
#202428 = CARTESIAN_POINT ( 'NONE',  ( 6.088856429251793934, -0.2706771573857471580, -1.805266125362497531 ) ) ;
#202430 = CARTESIAN_POINT ( 'NONE',  ( 8.046927864910717432, 9.346836249606042202, 1.199719254218462483 ) ) ;
#202431 = DIRECTION ( 'NONE',  ( 0.000000000000000000, 0.000000000000000000, 1.000000000000000000 ) ) ;
#202432 = DIRECTION ( 'NONE',  ( 0.000000000000000000, 1.000000000000000000, 0.000000000000000000 ) ) ;
#202433 =( NAMED_UNIT ( * ) SI_UNIT ( $, .STERADIAN. ) SOLID_ANGLE_UNIT ( ) );
#202434 = CARTESIAN_POINT ( 'NONE',  ( 6.927853306458749749, 8.145212281365775908, 1.082531754730558626 ) ) ;
#202435 = CARTESIAN_POINT ( 'NONE',  ( -1.364683531250000748, 13.17187500034139980, 0.000000000000000000 ) ) ;
#202437 = CARTESIAN_POINT ( 'NONE',  ( 0.3635249777022043771, 0.5700983740567664437, -1.719507965497588220 ) ) ;
#202436 = CARTESIAN_POINT ( 'NONE',  ( 6.855582950365507244, 8.027210192628430718, -1.199719254218452047 ) ) ;
#202438 = CARTESIAN_POINT ( 'NONE',  ( -8.182509401047415309, 9.505014708432145909, 1.199719254218462483 ) ) ;
#202439 = CARTESIAN_POINT ( 'NONE',  ( 6.654354466208897811, 6.657835053532175529, 0.7998128361456341429 ) ) ;
#202440 = CARTESIAN_POINT ( 'NONE',  ( -0.08058605610039842881, -6.304485801116100241, 10.99970480911019699 ) ) ;
#202441 = CARTESIAN_POINT ( 'NONE',  ( 0.9999999999999833467, 6.468705557303653819, 4.925226524755080604 ) ) ;
#202442 = CARTESIAN_POINT ( 'NONE',  ( 4.142179624174931796, 4.791296635414242111, 1.199719254218464037 ) ) ;
#202443 = ORIENTED_EDGE ( 'NONE', *, *, #97172, .F. ) ;
#202444 = CARTESIAN_POINT ( 'NONE',  ( 5.905875104417894761, -1.122515283938491537, -1.674877678029200068 ) ) ;
#202445 = CARTESIAN_POINT ( 'NONE',  ( 0.8562900302464396818, 0.8558255631127343888, -1.940287777186230578 ) ) ;
#202446 = PRESENTATION_LAYER_ASSIGNMENT (  '', '', ( #22635 ) ) ;
#202447 = CARTESIAN_POINT ( 'NONE',  ( -3.005201095308074777, 6.378479170349286242, -0.7606738891400167679 ) ) ;
#202448 = LINE ( 'NONE', #37847, #109637 ) ;
#202449 = CARTESIAN_POINT ( 'NONE',  ( -1.567523721964583450, 8.684745761082966808, -2.500978756717645357 ) ) ;
#202450 = CARTESIAN_POINT ( 'NONE',  ( -3.633221978782290140, 6.222214161012547429, -1.082531754730549967 ) ) ;
#202451 = VECTOR ( 'NONE', #202773, 1000.000000000000000 ) ;
#202452 = CARTESIAN_POINT ( 'NONE',  ( 8.405692050792682224, 12.75046512599275772, -0.7216878364870328300 ) ) ;
#202453 = CARTESIAN_POINT ( 'NONE',  ( 2.975404341296074229, -0.1976578167360588389, 1.959527558586687146 ) ) ;
#202454 = CARTESIAN_POINT ( 'NONE',  ( 4.886342304379579282, -0.6820123065829878373, -1.897693145932321857 ) ) ;
#202455 = CARTESIAN_POINT ( 'NONE',  ( -7.206322340863467346, 8.366129804884193888, 1.199719254218450271 ) ) ;
#202456 = CARTESIAN_POINT ( 'NONE',  ( -6.042630808230841359E-15, -2.012500000000000178, 3.474999999999999645 ) ) ;
#202457 = EDGE_CURVE ( 'NONE', #144861, #129260, #58862, .T. ) ;
#202458 = CARTESIAN_POINT ( 'NONE',  ( 5.244143516318892750, 0.6338322011035132375, 2.097776330851252258 ) ) ;
#202459 = DIRECTION ( 'NONE',  ( 0.000000000000000000, 1.000000000000000000, 0.000000000000000000 ) ) ;
#202460 = CARTESIAN_POINT ( 'NONE',  ( 3.434515876041916105, 1.879162883219337665, 0.4232601004234298747 ) ) ;
#202461 = CARTESIAN_POINT ( 'NONE',  ( -6.320072162264675164, 10.52516795595079557, 0.7998128361456481317 ) ) ;
#202462 = CARTESIAN_POINT ( 'NONE',  ( -0.02948999725177046949, 0.7228889410342426158, -2.008564694272568563 ) ) ;
#202463 = DIRECTION ( 'NONE',  ( -0.7592566023652995710, 0.6507913734559650498, 0.000000000000000000 ) ) ;
#202464 = CARTESIAN_POINT ( 'NONE',  ( 5.477955196520937875, 6.401917805796054850, -1.218707208129303110 ) ) ;
#202465 =( BOUNDED_CURVE ( )  B_SPLINE_CURVE ( 2, ( #184124, #35746, #4285, #168949, #101821, #167888, #19489 ),
 .UNSPECIFIED., .F., .T. ) 
 B_SPLINE_CURVE_WITH_KNOTS ( ( 3, 2, 2, 3 ),
 ( 0.3000000000000002109, 0.3083333333333335147, 0.3166666666666667629, 0.3250000000000000666 ),
 .UNSPECIFIED. ) 
 CURVE ( )  GEOMETRIC_REPRESENTATION_ITEM ( )  RATIONAL_B_SPLINE_CURVE ( ( 0.9999999999999964473, 0.8660254037844422603, 1.000000000000000000, 0.8660254037844387076, 1.000000000000000000, 0.8660254037844378194, 1.000000000000000888 ) ) 
 REPRESENTATION_ITEM ( '' )  );
#202466 = ORIENTED_EDGE ( 'NONE', *, *, #62099, .F. ) ;
#202467 = CARTESIAN_POINT ( 'NONE',  ( 3.607878275012302627, 7.223292064240769861, 0.7216878364870257245 ) ) ;
#202468 = CARTESIAN_POINT ( 'NONE',  ( 5.155114233317533490, 1.639596689546858777, -1.090739528099492928 ) ) ;
#202469 = ORIENTED_EDGE ( 'NONE', *, *, #84925, .F. ) ;
#202471 = CARTESIAN_POINT ( 'NONE',  ( 4.283843839860628222, 1.952122219449687668, -0.4911893120533029622 ) ) ;
#202470 = CARTESIAN_POINT ( 'NONE',  ( 0.9252163604592329449, -1.233020167302405490, -1.500395619358737553 ) ) ;
#202472 = CARTESIAN_POINT ( 'NONE',  ( 5.237821733363889010, -2.161759915733433068, -0.7809387408506673900 ) ) ;
#202474 = CARTESIAN_POINT ( 'NONE',  ( 3.906960136656021376, -1.523566986099005316, 1.068299854780943692 ) ) ;
#202473 = SURFACE_STYLE_FILL_AREA ( #105023 ) ;
#202475 = CARTESIAN_POINT ( 'NONE',  ( 7.212011367826596242, 7.378711115411311638, 0.000000000000000000 ) ) ;
#202477 = EDGE_CURVE ( 'NONE', #5559, #46791, #158419, .T. ) ;
#202476 = CYLINDRICAL_SURFACE ( 'NONE', #64019, 0.09999999999999986677 ) ;
#202478 = DIRECTION ( 'NONE',  ( 0.9982742078614211811, 0.000000000000000000, 0.05872483221476467591 ) ) ;
#202479 = CARTESIAN_POINT ( 'NONE',  ( -6.344325816190970357, 9.489131654609717970, 1.199719254218452047 ) ) ;
#202480 = CARTESIAN_POINT ( 'NONE',  ( -5.045042558060949034, 6.018876084893449274, 1.082531754730549078 ) ) ;
#202481 = CARTESIAN_POINT ( 'NONE',  ( 0.3280006606478855224, 1.121390616443746602, -1.882787531365101685 ) ) ;
#202482 = CARTESIAN_POINT ( 'NONE',  ( 5.287316719649520991, 8.151991358691011769, -1.082531754730549078 ) ) ;
#202483 = ORIENTED_EDGE ( 'NONE', *, *, #43620, .F. ) ;
#202484 = CARTESIAN_POINT ( 'NONE',  ( 3.334942598837264960, 6.834590765378040444, 1.214306433183764966E-14 ) ) ;
#202485 = CARTESIAN_POINT ( 'NONE',  ( 0.000000000000000000, 9.001999999999998892, 0.000000000000000000 ) ) ;
#202486 = CARTESIAN_POINT ( 'NONE',  ( 0.2053145577999641036, -0.4904175937916722128, 1.758528939493007481 ) ) ;
#202487 = CARTESIAN_POINT ( 'NONE',  ( -3.086452525405351643, 6.752611712948207057, 0.7998128361456341429 ) ) ;
#202488 = CARTESIAN_POINT ( 'NONE',  ( 2.707300540323886562, 1.633622375412818073, 0.5822755513817943207 ) ) ;
#202489 = CARTESIAN_POINT ( 'NONE',  ( -4.913752204202785023, 4.881785571126718182, -0.5639616748225815268 ) ) ;
#202491 = CARTESIAN_POINT ( 'NONE',  ( -6.905180308061733996, 6.950465202360470052, 0.7998128361456341429 ) ) ;
#202490 = AXIS2_PLACEMENT_3D ( 'NONE', #164637, #96472, #195004 ) ;
#202492 = CARTESIAN_POINT ( 'NONE',  ( 9.083072846151447166, 12.68433652289702884, 1.199719254218450271 ) ) ;
#202493 = CARTESIAN_POINT ( 'NONE',  ( 6.111906964637446649, -1.811269838261083232, 0.2284818145076653595 ) ) ;
#202494 = CARTESIAN_POINT ( 'NONE',  ( 3.731260466781026963, 0.05263058604075031982, -1.961233346245725429 ) ) ;
#202495 = CARTESIAN_POINT ( 'NONE',  ( -9.514659125335341649E-15, -0.9999999993172007384, -1.414508159514585417 ) ) ;
#202496 = CARTESIAN_POINT ( 'NONE',  ( -9.826962411806732689, 10.35921099006301382, -0.7998128361456291469 ) ) ;
#202497 = EDGE_CURVE ( 'NONE', #48843, #51477, #102580, .T. ) ;
#202498 = CARTESIAN_POINT ( 'NONE',  ( 7.884230021546724920, 9.157022099014721306, 1.199719254218462483 ) ) ;
#202499 = CARTESIAN_POINT ( 'NONE',  ( 3.633539341399088407, -0.1543397204060332761, 2.114911865293423787 ) ) ;
#202500 = CARTESIAN_POINT ( 'NONE',  ( 5.833751235630055376, 10.02806988486892514, 0.7998128361456331437 ) ) ;
#202501 = CARTESIAN_POINT ( 'NONE',  ( -9.592557376868645846, 11.15007068022363157, -1.199719254218441611 ) ) ;
#202502 = ADVANCED_FACE ( 'NONE', ( #124583 ), #180104, .T. ) ;
#202503 = CARTESIAN_POINT ( 'NONE',  ( 1.446235060908855008, -0.9343481645287862181, 1.847524432027500385 ) ) ;
#202505 = CARTESIAN_POINT ( 'NONE',  ( -0.6823417656250246877, -0.8864583329919115684, 1.181850606188755259 ) ) ;
#202504 = DIRECTION ( 'NONE',  ( -0.9632918427306580433, 0.000000000000000000, -0.2684563758389303945 ) ) ;
#202507 = ORIENTED_EDGE ( 'NONE', *, *, #65071, .F. ) ;
#202506 = CARTESIAN_POINT ( 'NONE',  ( 4.916739609850255377, -0.7473993280511237458, -2.091895594778249379 ) ) ;
#202508 = CARTESIAN_POINT ( 'NONE',  ( 1.249136956142880894, 2.263619502511230230, -0.3993902815438779563 ) ) ;
#202509 = CARTESIAN_POINT ( 'NONE',  ( 9.300530189294644146, 10.91333531134101165, -1.082531754730543083 ) ) ;
#202511 = CARTESIAN_POINT ( 'NONE',  ( -3.285556943750000514, -1.888541666188711110, -1.896917185911906500 ) ) ;
#202510 = CARTESIAN_POINT ( 'NONE',  ( 7.241463443474815520, 8.581367117876336437, -1.082531754730548412 ) ) ;
#202512 = SURFACE_STYLE_USAGE ( .BOTH. , #199316 ) ;
#202513 = CARTESIAN_POINT ( 'NONE',  ( -8.673617379884035472E-15, 3.975067388631681187, -1.561251128379126385E-14 ) ) ;
#202515 = DIRECTION ( 'NONE',  ( -5.551115123125764829E-17, 0.000000000000000000, 1.000000000000000000 ) ) ;
#202514 = AXIS2_PLACEMENT_3D ( 'NONE', #10442, #27773, #111228 ) ;
#202516 = CARTESIAN_POINT ( 'NONE',  ( 2.689602200614676697, 1.814610489020528350, -0.6038049036062518304 ) ) ;
#202517 = CARTESIAN_POINT ( 'NONE',  ( 4.242953580973901850, -1.500179917044243139, 0.8508681493539415053 ) ) ;
#202518 = CARTESIAN_POINT ( 'NONE',  ( 2.817592499383800408, -1.357869084745389587, -1.490969456672403659 ) ) ;
#202519 = CARTESIAN_POINT ( 'NONE',  ( 3.516502792989243176, -2.123307701433849282, 0.8810689989526691024 ) ) ;
#202520 = FACE_OUTER_BOUND ( 'NONE', #188887, .T. ) ;
#202521 = CARTESIAN_POINT ( 'NONE',  ( 6.709622069694824553, -0.4604308047033068840, 2.062537096560501659 ) ) ;
#202522 = CARTESIAN_POINT ( 'NONE',  ( -6.346625304972878467, 7.537389289624049304, 1.082531754730548412 ) ) ;
#202523 = CARTESIAN_POINT ( 'NONE',  ( 4.973781575966475188, 1.018845774273930749, 1.446830399915491006 ) ) ;
#202525 = CARTESIAN_POINT ( 'NONE',  ( 1.008267258593512183, -1.035053087846869335, -2.045343892876672065 ) ) ;
#202524 = CARTESIAN_POINT ( 'NONE',  ( 6.607619761813720238, 8.802252036906432764, 1.599625672291268286 ) ) ;
#202526 = CARTESIAN_POINT ( 'NONE',  ( 6.316338248019477852, 1.719745045379994286, 0.6579504788090041467 ) ) ;
#202527 = CARTESIAN_POINT ( 'NONE',  ( -3.379006598303881059, 4.965260336153046516, -1.599625672291256295 ) ) ;
#202528 = CARTESIAN_POINT ( 'NONE',  ( 5.542994302928621053, -1.725804593724251657, -1.350479894307685225 ) ) ;
#202529 = CARTESIAN_POINT ( 'NONE',  ( -5.276058054373441664, 6.184431147304315424, -1.199719254218453823 ) ) ;
#202530 = CARTESIAN_POINT ( 'NONE',  ( -1.953008978358306879E-14, -0.5156249996585442474, 1.570758158831760287 ) ) ;
#202531 = DIRECTION ( 'NONE',  ( 0.000000000000000000, 1.000000000000000000, 0.000000000000000000 ) ) ;
#202532 = CARTESIAN_POINT ( 'NONE',  ( 6.689897370947560873, -1.349224794794257720, -1.570457413003906177 ) ) ;
#202533 = CARTESIAN_POINT ( 'NONE',  ( 0.9191581010105540628, -1.820984308097562954, 0.8666112775468015617 ) ) ;
#202534 = CARTESIAN_POINT ( 'NONE',  ( -1.364683531250010295, 5.530208333674751842, 0.7879004041258379498 ) ) ;
#202535 = CARTESIAN_POINT ( 'NONE',  ( 4.283760221956850245, 1.259274395394771817, 1.458037640750938779 ) ) ;
#202536 = CARTESIAN_POINT ( 'NONE',  ( -1.402160292154681736E-14, 11.42187500034140157, 1.575800808251682339 ) ) ;
#202537 = CARTESIAN_POINT ( 'NONE',  ( 0.8794853950937852050, -2.011299634806243741, -0.9433073274909502537 ) ) ;
#202539 = ORIENTED_EDGE ( 'NONE', *, *, #70476, .F. ) ;
#202538 = CARTESIAN_POINT ( 'NONE',  ( 10.40318394038753702, 11.03146944007395724, -0.7998128361456281477 ) ) ;
#202541 = FACE_OUTER_BOUND ( 'NONE', #149649, .T. ) ;
#202540 = FACE_OUTER_BOUND ( 'NONE', #150001, .T. ) ;
#202542 = CARTESIAN_POINT ( 'NONE',  ( 6.938893903907228378E-15, 10.64264068711930733, 1.214306433183764966E-14 ) ) ;
#202543 = CARTESIAN_POINT ( 'NONE',  ( 8.530051201292206287, 13.10347683481629488, 0.000000000000000000 ) ) ;
#202544 = DIRECTION ( 'NONE',  ( 0.000000000000000000, -1.000000000000000000, 0.000000000000000000 ) ) ;
#202545 = FACE_OUTER_BOUND ( 'NONE', #95048, .T. ) ;
#202546 = CARTESIAN_POINT ( 'NONE',  ( 4.229842819227870976, 1.707864474872609062, 0.3341882380870179192 ) ) ;
#202547 = CARTESIAN_POINT ( 'NONE',  ( 2.769914238037580745, -1.940913097850523128, 0.2850433363836765155 ) ) ;
#202549 = CARTESIAN_POINT ( 'NONE',  ( 0.6823417656249899377, 3.155208333674754062, 1.181850606188765695 ) ) ;
#202548 = CARTESIAN_POINT ( 'NONE',  ( 5.931855901178834323, 6.879252291918818152, 1.199719254218462483 ) ) ;
#202550 = CARTESIAN_POINT ( 'NONE',  ( -5.703936002245207249, 6.126809468943200443, 0.7377312291968595170 ) ) ;
#202551 = CARTESIAN_POINT ( 'NONE',  ( 10.97895254167818813, -5.212340523078044185, -0.4373349612950642729 ) ) ;
#202552 = CARTESIAN_POINT ( 'NONE',  ( 0.2036765287981847083, -1.593398458586914757, -1.309455759714562850 ) ) ;
#202553 = CARTESIAN_POINT ( 'NONE',  ( -8.667740277838301921, 9.006785167099828016, -0.7998128361456291469 ) ) ;
#202554 = CARTESIAN_POINT ( 'NONE',  ( -3.240035523541616502, 6.723865844199768738, 0.7216878364870317197 ) ) ;
#202555 = CARTESIAN_POINT ( 'NONE',  ( 5.260953973667149342, -0.05432152012316109058, -2.015980820358989511 ) ) ;
#202556 = CARTESIAN_POINT ( 'NONE',  ( 0.8137758769373629741, -0.3292158159766758185, 2.238336236828967429 ) ) ;
#202558 = EDGE_LOOP ( 'NONE', ( #61967, #198000, #9144, #69360 ) ) ;
#202557 = CARTESIAN_POINT ( 'NONE',  ( -6.417086777969760902, 6.381022750586497594, 0.7998128361456341429 ) ) ;
#202559 = CARTESIAN_POINT ( 'NONE',  ( -1.402160292154681736E-14, -0.5062499993171791779, 1.732050807568877637 ) ) ;
#202560 = CARTESIAN_POINT ( 'NONE',  ( 1.897508810457830153, -0.6348907881138059484, 1.759622905829677508 ) ) ;
#202561 = CARTESIAN_POINT ( 'NONE',  ( -0.07027205189932134166, -1.338084538058325279, -1.103043951268277478 ) ) ;
#202563 = CARTESIAN_POINT ( 'NONE',  ( 3.843468145482428877, 0.7371271433744167600, -2.064019554291535830 ) ) ;
#202562 = CARTESIAN_POINT ( 'NONE',  ( -1.360316468750056851, 1.369791667008064540, -0.7853790794159101196 ) ) ;
#202564 = CARTESIAN_POINT ( 'NONE',  ( 6.088978940744814494, -0.3304744056438710387, -2.283700556900492451 ) ) ;
#202565 = CARTESIAN_POINT ( 'NONE',  ( 6.643830136542335119, 0.7930364421293911725, -1.902288772117090687 ) ) ;
#202566 = CARTESIAN_POINT ( 'NONE',  ( 3.714730536668510830, -0.1420231480665778423, 1.936809614188730544 ) ) ;
#202567 = CARTESIAN_POINT ( 'NONE',  ( -5.409340101728186134, 5.413244328212063472, 0.7216878364870317197 ) ) ;
#202568 = CARTESIAN_POINT ( 'NONE',  ( 5.553920895479774522, 1.868435625992425742, -0.09091641586010666687 ) ) ;
#202569 = CARTESIAN_POINT ( 'NONE',  ( 0.4867935908847584314, 7.427453578140085888, -4.536604770854444801 ) ) ;
#202570 = CARTESIAN_POINT ( 'NONE',  ( 5.397554552016228691, 5.469770863539975991, 0.7216878364870328300 ) ) ;
#202571 = CARTESIAN_POINT ( 'NONE',  ( -0.6801582343749917881, 0.4322916670080681478, 1.178068619123841643 ) ) ;
#202572 = CARTESIAN_POINT ( 'NONE',  ( 4.236954046275762664, 2.015912997090345549, -0.05229627655192746472 ) ) ;
#202573 = CARTESIAN_POINT ( 'NONE',  ( -3.999292125906916073, 5.688926785023260102, 1.443375672974064550 ) ) ;
#202574 = CARTESIAN_POINT ( 'NONE',  ( -4.932134020321308654, 8.976183133675331050, 0.7998128361456291469 ) ) ;
#202575 = CARTESIAN_POINT ( 'NONE',  ( 8.880754312151170282, 10.31963377138658089, 1.199719254218453823 ) ) ;
#202577 = CARTESIAN_POINT ( 'NONE',  ( 0.000000000000000000, 0.2000000000000057288, 0.000000000000000000 ) ) ;
#202576 = CARTESIAN_POINT ( 'NONE',  ( 1.031563979315492485, -1.156294252604734396, -1.412831148817683680 ) ) ;
#202578 = CARTESIAN_POINT ( 'NONE',  ( -5.367048706163331850, 7.354919138647580290, -1.599625672291271394 ) ) ;
#202579 = CARTESIAN_POINT ( 'NONE',  ( -3.806807270387036368, 7.663301925418665839, 0.000000000000000000 ) ) ;
#202580 = CARTESIAN_POINT ( 'NONE',  ( -11.76695491367977198, 4.673720869072629291, 4.995412848167409159 ) ) ;
#202581 = ORIENTED_EDGE ( 'NONE', *, *, #116347, .F. ) ;
#202582 = CARTESIAN_POINT ( 'NONE',  ( 0.4269344243218140544, 2.069031678568326704, 0.6260965431626740463 ) ) ;
#202583 = CARTESIAN_POINT ( 'NONE',  ( -5.099275172071237705, 8.963255110809500437, 0.000000000000000000 ) ) ;
#202584 = CARTESIAN_POINT ( 'NONE',  ( -3.602716132929368875, 5.226254793216122074, 1.599625672291267398 ) ) ;
#202585 = CARTESIAN_POINT ( 'NONE',  ( -8.123306592882240551, 12.62894145833798376, 0.000000000000000000 ) ) ;
#202586 = CARTESIAN_POINT ( 'NONE',  ( 5.901037506996139825, -0.2983434833860042490, -1.997397228102874234 ) ) ;
#202588 = ORIENTED_EDGE ( 'NONE', *, *, #52718, .F. ) ;
#202587 = CARTESIAN_POINT ( 'NONE',  ( 5.848318881832833327, 1.097015000334870649, -1.931420017644119635 ) ) ;
#202589 = CARTESIAN_POINT ( 'NONE',  ( -3.923105346307911745, 5.670318552149568703, -1.599625672291283607 ) ) ;
#202590 = CARTESIAN_POINT ( 'NONE',  ( 5.952193131599331721, 6.902979060742733708, 1.199719254218462483 ) ) ;
#202591 = CARTESIAN_POINT ( 'NONE',  ( 5.155176885484381799, -1.739861089072095357, -1.104300716835506346 ) ) ;
#202592 = CARTESIAN_POINT ( 'NONE',  ( 4.166638809851969327, 1.319227567334404494, 1.525044649537968589 ) ) ;
#202593 = ORIENTED_EDGE ( 'NONE', *, *, #203566, .F. ) ;
#202594 = ORIENTED_EDGE ( 'NONE', *, *, #109243, .F. ) ;
#202595 = CARTESIAN_POINT ( 'NONE',  ( 6.961139734775133370, 5.290451655907104644, 1.214306433183764966E-14 ) ) ;
#202596 = CARTESIAN_POINT ( 'NONE',  ( 3.891353782322113375, 4.498666486585943147, -1.199719254218446718 ) ) ;
#202598 = ORIENTED_EDGE ( 'NONE', *, *, #154559, .F. ) ;
#202597 = CARTESIAN_POINT ( 'NONE',  ( -8.106849506328558164, 8.422688943663599659, 0.000000000000000000 ) ) ;
#202599 = CARTESIAN_POINT ( 'NONE',  ( 4.605689926069578277, 8.476745573306274650, -0.2140288463435610078 ) ) ;
#202600 = CARTESIAN_POINT ( 'NONE',  ( 4.130232389481975908, 0.2495678132241747338, -2.000550906993769473 ) ) ;
#202601 = CARTESIAN_POINT ( 'NONE',  ( 3.556447125109524876, -1.624355972047783148, -0.8667379164201680641 ) ) ;
#202602 = CARTESIAN_POINT ( 'NONE',  ( 0.4999999999999900080, 3.949999999999974420, 0.4999999999999640288 ) ) ;
#202603 = CARTESIAN_POINT ( 'NONE',  ( 2.245130213409586961, 0.5076759487793567338, 2.251015715305480391 ) ) ;
#202604 = CARTESIAN_POINT ( 'NONE',  ( 5.110497557708379546, 4.926945003606695295, -0.7998128361456481317 ) ) ;
#202605 = CARTESIAN_POINT ( 'NONE',  ( 4.446650332099550518, 0.5718123500428309303, 2.084546224624775679 ) ) ;
#202606 = CARTESIAN_POINT ( 'NONE',  ( 6.909851844459134362, 11.21324425184434936, -0.7998128361456291469 ) ) ;
#202608 = CARTESIAN_POINT ( 'NONE',  ( 2.729704159269104924, 0.7212915320151757070, -1.883313052590728454 ) ) ;
#202607 = CARTESIAN_POINT ( 'NONE',  ( 6.532758020889952277, -1.641319963461195464, 0.8346263169811756200 ) ) ;
#202609 = CARTESIAN_POINT ( 'NONE',  ( -4.843287188579803448, 6.673587691474970107, -1.599625672291256295 ) ) ;
#202610 = ADVANCED_FACE ( 'NONE', ( #58678 ), #94402, .F. ) ;
#202611 = CARTESIAN_POINT ( 'NONE',  ( 6.856061878569608298E-15, 0.9375000000000238698, -1.225000000000010525 ) ) ;
#202612 = AXIS2_PLACEMENT_3D ( 'NONE', #192006, #20172, #104658 ) ;
#202613 = DIRECTION ( 'NONE',  ( 0.000000000000000000, 0.000000000000000000, 1.000000000000000000 ) ) ;
#202614 = CARTESIAN_POINT ( 'NONE',  ( 2.008475284031425723, 1.387998011844304491, -1.254312187223500796 ) ) ;
#202615 = CARTESIAN_POINT ( 'NONE',  ( 6.702032618711820433, -1.971027473680329045, 0.04818573739380492549 ) ) ;
#202616 = VECTOR ( 'NONE', #124684, 1000.000000000000000 ) ;
#202618 = CARTESIAN_POINT ( 'NONE',  ( -6.291865805193673111, 9.498204651771386509, -1.199719254218452047 ) ) ;
#202617 = CARTESIAN_POINT ( 'NONE',  ( 1.499999999999987121, -0.9645833326505173222, 0.8660254037844524744 ) ) ;
#202619 = CARTESIAN_POINT ( 'NONE',  ( 1.840723031453334935, 2.183200880077686978, 0.3216222850719457349 ) ) ;
#202620 = ORIENTED_EDGE ( 'NONE', *, *, #76548, .T. ) ;
#202621 = CARTESIAN_POINT ( 'NONE',  ( -5.710235717126113109, 6.137237704801142613, 0.8101758662225978513 ) ) ;
#202622 = CARTESIAN_POINT ( 'NONE',  ( 3.032219910950674890, 6.689340329417765574, 0.7998128361456321445 ) ) ;
#202623 = CARTESIAN_POINT ( 'NONE',  ( -5.274285450916075035, 6.112086766612214284, 1.199719254218450271 ) ) ;
#202624 = CARTESIAN_POINT ( 'NONE',  ( -7.730132016633767478, -5.756136661604486449, 7.730132016633794123 ) ) ;
#202625 = CARTESIAN_POINT ( 'NONE',  ( 5.629747345311447937, -1.250075164085572954, -1.524477324586423377 ) ) ;
#202626 = CARTESIAN_POINT ( 'NONE',  ( 6.322925365441865786, 2.150718969097795696, 0.8370602354567517889 ) ) ;
#202627 = CARTESIAN_POINT ( 'NONE',  ( 0.5198770262540284293, 1.941052373433370448, -0.2841105942011297736 ) ) ;
#202628 = CARTESIAN_POINT ( 'NONE',  ( 3.748931555198372845, -0.3975983499134613242, -2.023727603370987449 ) ) ;
#202629 = CARTESIAN_POINT ( 'NONE',  ( 4.839897650398541806, 8.590371658866210680, 1.040834085586084257E-14 ) ) ;
#202630 = EDGE_CURVE ( 'NONE', #197916, #167380, #141145, .T. ) ;
#202631 = CARTESIAN_POINT ( 'NONE',  ( 7.354371980770088690, 7.544798497178720531, 0.000000000000000000 ) ) ;
#202632 = ORIENTED_EDGE ( 'NONE', *, *, #187141, .F. ) ;
#202633 = CARTESIAN_POINT ( 'NONE',  ( 8.907343734053986495, 9.494248565925552441, -0.7216878364870197293 ) ) ;
#202634 = CARTESIAN_POINT ( 'NONE',  ( 0.6823417656249899377, 3.238541667008085323, -1.181850606188754593 ) ) ;
#202635 = CARTESIAN_POINT ( 'NONE',  ( 10.45358220256315285, 1.000000000000000888, -5.892590188894412329 ) ) ;
#202636 = CARTESIAN_POINT ( 'NONE',  ( 3.660338285565247762, 7.214219066560688454, 1.040834085586084257E-14 ) ) ;
#202637 = CARTESIAN_POINT ( 'NONE',  ( 5.951682048281027981, 1.640226396406889942, 1.422642917226999426 ) ) ;
#202639 = CARTESIAN_POINT ( 'NONE',  ( 4.985823801847525161, -1.827980399782932697, -0.2200341325891697619 ) ) ;
#202638 = DIRECTION ( 'NONE',  ( 0.000000000000000000, -1.000000000000000000, 0.000000000000000000 ) ) ;
#202640 = CARTESIAN_POINT ( 'NONE',  ( 5.459907696476232530, 6.251290254602066554, -1.005486610859710472 ) ) ;
#202641 = CARTESIAN_POINT ( 'NONE',  ( -10.06283597805679975, 4.651455381798285771, -6.539173949727397961 ) ) ;
#202642 = CARTESIAN_POINT ( 'NONE',  ( 0.6142526126209288950, 1.294576594435635108, -1.350420462534522859 ) ) ;
#202643 = B_SPLINE_CURVE_WITH_KNOTS ( 'NONE', 3,
 ( #177497, #29110, #12831, #62657, #128815, #194797, #46434, #59334, #39894, #192517 ),
 .UNSPECIFIED., .F., .F.,
 ( 4, 2, 2, 2, 4 ),
 ( 0.000000000000000000, 0.2499999999999999445, 0.4999999999999998890, 0.7499999999999997780, 1.000000000000000000 ),
 .UNSPECIFIED. ) ;
#202644 = CARTESIAN_POINT ( 'NONE',  ( -4.432018112209435756, 7.309502936831247411, 1.252451368452773384 ) ) ;
#202645 = CARTESIAN_POINT ( 'NONE',  ( -10.86205067566995730, -6.804704122739859251, 0.3107038660269559327 ) ) ;
#202646 = CARTESIAN_POINT ( 'NONE',  ( 6.053423048675670159, 7.145495228771222784, -1.160209803801291795 ) ) ;
#202647 = CARTESIAN_POINT ( 'NONE',  ( 11.89942855770814312, 13.79999999999999893, 0.6999999999999992895 ) ) ;
#202648 = CARTESIAN_POINT ( 'NONE',  ( 2.324752472428833983, -0.002986221762550990942, 1.770032028303660576 ) ) ;
#202649 = AXIS2_PLACEMENT_3D ( 'NONE', #157923, #58272, #88648 ) ;
#202650 = CARTESIAN_POINT ( 'NONE',  ( 6.164703283132928924, 0.6335332109005767931, 1.910856914995302303 ) ) ;
#202652 = CARTESIAN_POINT ( 'NONE',  ( 4.534732036847580083, -1.536008458380673458, 1.144414559590371638 ) ) ;
#202651 = CARTESIAN_POINT ( 'NONE',  ( -7.804689982961090955, 12.25722208009664094, 0.7998128361456481317 ) ) ;
#202653 = CARTESIAN_POINT ( 'NONE',  ( -2.974866045527320590, 6.692355909712924600, 0.04048647387576057716 ) ) ;
#202654 = CARTESIAN_POINT ( 'NONE',  ( 5.564895475732142494, 1.492515675241333772, -1.285245034736775649 ) ) ;
#202655 = CARTESIAN_POINT ( 'NONE',  ( 0.1059362375676886209, 1.575662574916199210, 1.419458935296296520 ) ) ;
#202656 = CARTESIAN_POINT ( 'NONE',  ( -3.541704441667874903, 5.155074486744371853, -1.599625672291256295 ) ) ;
#202657 = CARTESIAN_POINT ( 'NONE',  ( 3.063207453921251489, 0.2760179531714930246, -1.850060308400132358 ) ) ;
#202659 = ORIENTED_EDGE ( 'NONE', *, *, #148379, .F. ) ;
#202658 = CARTESIAN_POINT ( 'NONE',  ( 6.463511695382619493, 0.2867160277617316622, -1.700725516685620553 ) ) ;
#202660 = CARTESIAN_POINT ( 'NONE',  ( 3.545738602337618506, -1.670889076328873069, -1.441789439710974063 ) ) ;
#202661 = CARTESIAN_POINT ( 'NONE',  ( 1.364683531249990311, 3.196875000341416140, 1.214306433183764966E-14 ) ) ;
#202662 = CARTESIAN_POINT ( 'NONE',  ( 0.3618804954101816906, -0.5516051106895186740, 1.987472385349927428 ) ) ;
#202663 = CARTESIAN_POINT ( 'NONE',  ( 5.913327553854682783, 10.05063257947248800, -0.7998128361456291469 ) ) ;
#202664 = CARTESIAN_POINT ( 'NONE',  ( -8.696665468161981494, 12.23352791524263239, -1.199719254218446718 ) ) ;
#202665 = CARTESIAN_POINT ( 'NONE',  ( 5.885648082108208889, 6.039213315313944896, 0.7216878364870273899 ) ) ;
#202666 = CARTESIAN_POINT ( 'NONE',  ( -4.711622075948912247, 5.455646162483875017, -1.199719254218446718 ) ) ;
#202667 =( GEOMETRIC_REPRESENTATION_CONTEXT ( 3 ) GLOBAL_UNCERTAINTY_ASSIGNED_CONTEXT ( ( #77635 ) ) GLOBAL_UNIT_ASSIGNED_CONTEXT ( ( #87687, #69277, #153761 ) ) REPRESENTATION_CONTEXT ( 'NONE', 'WORKASPACE' ) );
#202668 = CARTESIAN_POINT ( 'NONE',  ( -5.593777659986292505, 7.397990072842402398, -1.241664499109219166 ) ) ;
#202669 = ORIENTED_EDGE ( 'NONE', *, *, #28369, .F. ) ;
#202670 = B_SPLINE_CURVE_WITH_KNOTS ( 'NONE', 3,
 ( #35847, #100849, #181041, #199399, #33718, #51046 ),
 .UNSPECIFIED., .F., .F.,
 ( 4, 2, 4 ),
 ( 0.000000000000000000, 0.002109688543090479894, 0.004219377086180959788 ),
 .UNSPECIFIED. ) ;
#202671 = CARTESIAN_POINT ( 'NONE',  ( 2.787621587699981696, -1.932700977737045633, 0.7428295258242522126 ) ) ;
#202672 = CARTESIAN_POINT ( 'NONE',  ( -1.001543065824772872E-14, 4.462500000000024336, 1.732050807568877637 ) ) ;
#202673 = CARTESIAN_POINT ( 'NONE',  ( 6.010342169559767633, 5.906487374108181143, -0.7998128361456281477 ) ) ;
#202674 = CARTESIAN_POINT ( 'NONE',  ( -6.612576056032890115, 6.759750829040511277, 0.1256891304984939506 ) ) ;
#202675 = CARTESIAN_POINT ( 'NONE',  ( 1.102219918440990876, -0.9059408578524772437, 1.805149201161629025 ) ) ;
#202676 = SURFACE_SIDE_STYLE ('',( #53253 ) ) ;
#202677 = CARTESIAN_POINT ( 'NONE',  ( -0.6823417656249969321, 3.467708333674754506, -1.181850606188749264 ) ) ;
#202678 = VERTEX_POINT ( 'NONE', #92280 ) ;
#202679 = VECTOR ( 'NONE', #22918, 1000.000000000000000 ) ;
#202681 = CARTESIAN_POINT ( 'NONE',  ( 8.866669273657322492, 12.32790267170016207, -1.082531754730543083 ) ) ;
#202680 = CARTESIAN_POINT ( 'NONE',  ( 0.1747926744264677590, 2.047238405490480861, -2.272669950590770149 ) ) ;
#202682 = CARTESIAN_POINT ( 'NONE',  ( 6.098982473628085543, 0.9961464269193781584, -1.752763620266280187 ) ) ;
#202683 = CARTESIAN_POINT ( 'NONE',  ( 6.227746030346171580, 0.7262518248569529433, -1.772935525165220128 ) ) ;
#202684 = CARTESIAN_POINT ( 'NONE',  ( -1.500000000000039524, 7.064371086078061523, -10.89416074946469770 ) ) ;
#202685 = CARTESIAN_POINT ( 'NONE',  ( 3.456733517523990606, -1.933646301634945885, -1.031433503814835007 ) ) ;
#202686 = CARTESIAN_POINT ( 'NONE',  ( -1.402160292154681736E-14, 2.118750000682816825, -1.732050807568863648 ) ) ;
#202687 = CARTESIAN_POINT ( 'NONE',  ( 2.513799616133075343, -0.5961229146635020903, 1.817204401178821760 ) ) ;
#202688 = CARTESIAN_POINT ( 'NONE',  ( -5.416646063859567484, 6.278174148379618735, 1.199719254218450271 ) ) ;
#202689 = CARTESIAN_POINT ( 'NONE',  ( 4.161989969270895706, 5.878740935614591656, 1.443375672974062551 ) ) ;
#202691 = CARTESIAN_POINT ( 'NONE',  ( 1.230092461119953517, 2.014234866427236259, 0.09611455020034495589 ) ) ;
#202690 = CARTESIAN_POINT ( 'NONE',  ( 10.14641618983893068, 3.870538056096204826, -5.683069686889757222 ) ) ;
#202692 = CARTESIAN_POINT ( 'NONE',  ( 1.364683531249997417, 10.79687500034139802, 2.602085213965210642E-15 ) ) ;
#202694 = CARTESIAN_POINT ( 'NONE',  ( -6.479871072688648148, 6.524547437750345402, 0.000000000000000000 ) ) ;
#202693 = CARTESIAN_POINT ( 'NONE',  ( 6.146043800834426918, 0.6857851511376764631, 2.081541312870714311 ) ) ;
#202696 = ORIENTED_EDGE ( 'NONE', *, *, #18997, .F. ) ;
#202695 = CARTESIAN_POINT ( 'NONE',  ( 3.276077977556953513, -1.028358954114884094, 1.384488693430762085 ) ) ;
#202697 = CARTESIAN_POINT ( 'NONE',  ( 0.1394461523057137220, 2.891244824116427470, -2.208899952336295325 ) ) ;
#202698 = CARTESIAN_POINT ( 'NONE',  ( 8.294891053462476904, 8.571794405328034827, 1.040834085586084257E-14 ) ) ;
#202699 = CARTESIAN_POINT ( 'NONE',  ( 3.310162060030825248, 7.013606170011280838, -0.7998128361456291469 ) ) ;
#202700 = SURFACE_STYLE_USAGE ( .BOTH. , #170218 ) ;
#202701 = CARTESIAN_POINT ( 'NONE',  ( 0.9769180011504545735, 1.811320799089161993, 0.7541596914439269161 ) ) ;
#202702 = CARTESIAN_POINT ( 'NONE',  ( -3.673896439623305810, 4.156855427197417185, -7.499999999999991118 ) ) ;
#202703 = CARTESIAN_POINT ( 'NONE',  ( 3.520313441042647540, 7.258782781191745137, 0.7998128361456321445 ) ) ;
#202704 = CARTESIAN_POINT ( 'NONE',  ( 0.1399997263886037790, 2.025166351305721868, -2.415484119839182320 ) ) ;
#202705 = ORIENTED_EDGE ( 'NONE', *, *, #156690, .F. ) ;
#202706 = VERTEX_POINT ( 'NONE', #158325 ) ;
#202707 = CARTESIAN_POINT ( 'NONE',  ( 4.266123773889715309, 1.810994338341217480, -0.04873877536224096446 ) ) ;
#202708 = ORIENTED_EDGE ( 'NONE', *, *, #104440, .T. ) ;
#202709 = CARTESIAN_POINT ( 'NONE',  ( 9.836604141914616406, 11.43479190611061647, 1.199719254218452047 ) ) ;
#202710 = CARTESIAN_POINT ( 'NONE',  ( 5.096939404094710468, 4.911127157724081371, 0.000000000000000000 ) ) ;
#202711 = CARTESIAN_POINT ( 'NONE',  ( 4.617698128633199062, -0.4785133679615029556, 1.747060762061508621 ) ) ;
#202712 = CARTESIAN_POINT ( 'NONE',  ( 0.4373225248172820656, -7.723431457505077979, -10.96785329849813273 ) ) ;
#202713 = DIRECTION ( 'NONE',  ( 0.7347175152297780176, 0.000000000000000000, -0.6783731810844091381 ) ) ;
#202714 = CARTESIAN_POINT ( 'NONE',  ( 5.888650760256147088, 5.979308965038350188, -0.1076000636002025918 ) ) ;
#202716 = CARTESIAN_POINT ( 'NONE',  ( 9.541187415715040032, 12.15447128979948310, -1.599625672291262513 ) ) ;
#202715 = CARTESIAN_POINT ( 'NONE',  ( 5.529708137783917898, 1.793509118821761561, -0.4966223845426844252 ) ) ;
#202717 = CARTESIAN_POINT ( 'NONE',  ( 2.530754833220005384, -1.591195339209892312, 1.066270812275710966 ) ) ;
#202718 = DIRECTION ( 'NONE',  ( 5.578564026256490882E-16, 1.000000000000000000, 9.066213480720158442E-32 ) ) ;
#202719 = CARTESIAN_POINT ( 'NONE',  ( -5.314433026876900001, 6.262888621853549331, 1.082531754730548412 ) ) ;
#202720 = ADVANCED_FACE ( 'NONE', ( #145302 ), #20002, .T. ) ;
#202721 = CARTESIAN_POINT ( 'NONE',  ( 9.499717950937025535, -9.918872507113817960, -0.07320418461264667498 ) ) ;
#202722 = CARTESIAN_POINT ( 'NONE',  ( 6.887178846062110615, 9.058127958537705027, -1.443375672974057666 ) ) ;
#202723 = CARTESIAN_POINT ( 'NONE',  ( -2.981903720001798597, 5.566305875722335372, -1.199719254218446718 ) ) ;
#202724 = CARTESIAN_POINT ( 'NONE',  ( 0.000000000000000000, 13.49999999999999822, 0.000000000000000000 ) ) ;
#202725 = CARTESIAN_POINT ( 'NONE',  ( 1.166094707548096965, -1.325134400199390550, 1.617025002462493921 ) ) ;
#202726 = CARTESIAN_POINT ( 'NONE',  ( 5.499767588998890844, 6.445425604367387429, 1.199719254218451159 ) ) ;
#202727 = CARTESIAN_POINT ( 'NONE',  ( 6.018570082959111112, 1.293320673360508488, -1.427839425051903532 ) ) ;
#202728 = CARTESIAN_POINT ( 'NONE',  ( -4.741601036477307574, 6.554953847355395880, 1.599625672291267398 ) ) ;
#202729 = CARTESIAN_POINT ( 'NONE',  ( 2.959763373685084353, 1.816946311034864703, -0.1772020141349931188 ) ) ;
#202730 = CARTESIAN_POINT ( 'NONE',  ( -3.642287698956932829, 3.120124397464415278, 2.500000000000464961 ) ) ;
#202731 = CARTESIAN_POINT ( 'NONE',  ( 2.250135261179100343, 0.8981609309555339538, -1.688322754368525747 ) ) ;
#202732 = EDGE_CURVE ( 'NONE', #193316, #129112, #213815, .T. ) ;
#202733 = CARTESIAN_POINT ( 'NONE',  ( 1.328490337915340991, -1.252144239891037403, 1.520259730874585768 ) ) ;
#202734 = CARTESIAN_POINT ( 'NONE',  ( 3.368632357871951033, 0.04486925901568206143, -1.941695523777670740 ) ) ;
#202735 = ORIENTED_EDGE ( 'NONE', *, *, #177319, .F. ) ;
#202736 = LINE ( 'NONE', #104207, #202679 ) ;
#202737 = CARTESIAN_POINT ( 'NONE',  ( -3.871735385154307263, 6.674719161725423788, -1.199719254218450271 ) ) ;
#202739 = CARTESIAN_POINT ( 'NONE',  ( 4.412424163657523657, -2.120181911468725033, -0.04909571644767100895 ) ) ;
#202738 = CARTESIAN_POINT ( 'NONE',  ( 4.760848217054122422, 5.583353003765119560, -1.199719254218452047 ) ) ;
#202741 = EDGE_CURVE ( 'NONE', #142717, #200044, #190420, .T. ) ;
#202740 = DIRECTION ( 'NONE',  ( 0.000000000000000000, 0.000000000000000000, -1.000000000000000000 ) ) ;
#202742 = CARTESIAN_POINT ( 'NONE',  ( 9.433775957010412938, 9.900493459467314850, 0.000000000000000000 ) ) ;
#202743 = CARTESIAN_POINT ( 'NONE',  ( 5.714115171586898079, 6.274818061858235652, 1.066218439657661721 ) ) ;
#202744 = CARTESIAN_POINT ( 'NONE',  ( 7.201315867513990554, 8.430565262634994284, -1.199719254218452047 ) ) ;
#202745 = CARTESIAN_POINT ( 'NONE',  ( 11.88234649872613602, 12.34339217083249096, -0.9090484974825243647 ) ) ;
#202746 = CARTESIAN_POINT ( 'NONE',  ( 4.178209475066913647, -1.049361115903378883, 1.493786327181771068 ) ) ;
#202747 = CARTESIAN_POINT ( 'NONE',  ( 0.1861046438572169226, -1.272802160389638892, -1.633586439835111648 ) ) ;
#202748 = CARTESIAN_POINT ( 'NONE',  ( -4.302014814237876017, 3.913438792899272212, 0.7998128361456341429 ) ) ;
#202749 = CARTESIAN_POINT ( 'NONE',  ( -4.900510728191886933, 8.135641830034209931, 1.034109914766440541 ) ) ;
#202750 = DIRECTION ( 'NONE',  ( -0.03984146075563027578, 0.000000000000000000, -0.9992060137953822085 ) ) ;
#202751 = CARTESIAN_POINT ( 'NONE',  ( 4.926551758443064699, 1.790249073151507497, 0.5424879929923772659 ) ) ;
#202752 = CARTESIAN_POINT ( 'NONE',  ( 8.263858322729371153, 9.599921783727809910, -1.199719254218446718 ) ) ;
#202753 = CARTESIAN_POINT ( 'NONE',  ( 2.596214140771450296, -1.921342217666447860, -0.1417109463846803752 ) ) ;
#202754 = DIRECTION ( 'NONE',  ( -0.7592566023652995710, -0.6507913734559652719, 0.000000000000000000 ) ) ;
#202755 = CARTESIAN_POINT ( 'NONE',  ( -8.012344526598182026E-15, 8.609375000341403350, -1.575800808251669460 ) ) ;
#202756 = CARTESIAN_POINT ( 'NONE',  ( -6.413170354464012846, 7.440785820751486312, 1.199719254218450271 ) ) ;
#202757 = CARTESIAN_POINT ( 'NONE',  ( 5.820528018968444961, 5.685037531751635953, 0.7998128361456341429 ) ) ;
#202758 = CARTESIAN_POINT ( 'NONE',  ( -3.648552735408985725, 7.270745601370182776, -0.7216878364870458196 ) ) ;
#202759 = COLOUR_RGB ( '', 0.72549020, 0.75294118, 0.79215686) ;
#202760 = ADVANCED_FACE ( 'NONE', ( #43517 ), #44580, .T. ) ;
#202761 = CARTESIAN_POINT ( 'NONE',  ( 1.599367111750239934, -0.2554771505851380908, 2.101684664062503316 ) ) ;
#202762 = FACE_OUTER_BOUND ( 'NONE', #26764, .T. ) ;
#202763 = CARTESIAN_POINT ( 'NONE',  ( 0.5155926040970099100, 6.713058329651131473, 3.584077772868219380 ) ) ;
#202764 = CARTESIAN_POINT ( 'NONE',  ( 4.891501605334720004, -1.894957309059261297, 0.8341102180390786991 ) ) ;
#202766 = CARTESIAN_POINT ( 'NONE',  ( 4.313480937648101587, 7.206793636360196764, -1.001376897629567830 ) ) ;
#202765 = CARTESIAN_POINT ( 'NONE',  ( 0.6613494997313728030, 0.9071737413179328247, 1.602200521169500957 ) ) ;
#202767 = EDGE_LOOP ( 'NONE', ( #42118, #43895, #44007, #127672 ) ) ;
#202768 = CARTESIAN_POINT ( 'NONE',  ( 5.906922434318937931, -1.273882657197453305, -1.913274281643152941 ) ) ;
#202769 = CARTESIAN_POINT ( 'NONE',  ( 4.799223189557548785, 7.582548906917042864, -1.082531754730549078 ) ) ;
#202771 = CARTESIAN_POINT ( 'NONE',  ( 1.220146605508150803E-14, 9.718750000682797818, -1.499999999999998446 ) ) ;
#202770 = CARTESIAN_POINT ( 'NONE',  ( 3.390947817193682656, 6.009837315817661008, -1.082531754730549967 ) ) ;
#202772 = CARTESIAN_POINT ( 'NONE',  ( 1.183963288966838334, -1.026766722195756376, 2.049517438521175183 ) ) ;
#202773 = DIRECTION ( 'NONE',  ( -5.578564026256490882E-16, -1.000000000000000000, -9.066213480720158442E-32 ) ) ;
#202774 = CARTESIAN_POINT ( 'NONE',  ( -5.529746549527323474, 7.544733289238903851, -1.599625672291271394 ) ) ;
#202775 = CARTESIAN_POINT ( 'NONE',  ( 6.087830645824786835, -1.932811661901209010, -0.1881662411436606785 ) ) ;
#202776 = ORIENTED_EDGE ( 'NONE', *, *, #206253, .T. ) ;
#202777 = CARTESIAN_POINT ( 'NONE',  ( 9.219181267168295335, 9.858059021225592744, 1.040834085586084257E-14 ) ) ;
#202778 = ORIENTED_EDGE ( 'NONE', *, *, #139330, .F. ) ;
#202779 = CARTESIAN_POINT ( 'NONE',  ( 6.486579876843341808, -1.171037552013409089, 1.512559164390047783 ) ) ;
#202780 = CARTESIAN_POINT ( 'NONE',  ( 0.1335669894368500532, -0.0009366757763962071850, -2.153671288142432694 ) ) ;
#202781 =( REPRESENTATION_RELATIONSHIP ('NONE','NONE', #84563, #11178 ) REPRESENTATION_RELATIONSHIP_WITH_TRANSFORMATION ( #9178 )SHAPE_REPRESENTATION_RELATIONSHIP( ) );
#202783 = CARTESIAN_POINT ( 'NONE',  ( 11.04536101718726293, 12.69999999999999929, 1.099999999999996758 ) ) ;
#202782 = CARTESIAN_POINT ( 'NONE',  ( -7.395082721250053837, 10.71501471051202614, -1.199719254218446718 ) ) ;
#202784 = CARTESIAN_POINT ( 'NONE',  ( -6.615342224808819616, 6.750480251133848419, 0.3470571717737805373 ) ) ;
#202786 = CARTESIAN_POINT ( 'NONE',  ( 1.568863545881917343, 0.1344791104000986337, -1.764800092583326929 ) ) ;
#202785 = CARTESIAN_POINT ( 'NONE',  ( 3.046908718545093819, -1.709425224762064266, -1.203301715110078662 ) ) ;
#202787 = DIRECTION ( 'NONE',  ( -0.9632918427306580433, 0.000000000000000000, 0.2684563758389303945 ) ) ;
#202789 = CARTESIAN_POINT ( 'NONE',  ( 3.978722188455630082, -0.2232912938500397904, -2.281366727860510313 ) ) ;
#202788 = CARTESIAN_POINT ( 'NONE',  ( 5.083381250481017410, 4.895309311841474553, 0.7998128361456352531 ) ) ;
#202790 = CARTESIAN_POINT ( 'NONE',  ( 3.011345489304529277, -0.8582029173807427247, -1.513924679874333767 ) ) ;
#202791 = CARTESIAN_POINT ( 'NONE',  ( 9.836604141914616406, 11.43479190611061647, 1.199719254218452047 ) ) ;
#202792 = DIRECTION ( 'NONE',  ( 0.9885327375000381167, 0.000000000000000000, -0.1510067114093955609 ) ) ;
#202793 = CARTESIAN_POINT ( 'NONE',  ( 3.374086008222790589, -0.3405263371191130095, 1.699849027820112823 ) ) ;
#202794 = CARTESIAN_POINT ( 'NONE',  ( 3.385384905382606391, 0.05040654291960967176, 2.170743301239473233 ) ) ;
#202795 = CARTESIAN_POINT ( 'NONE',  ( 3.635557746758808495, 7.393234471193928847, -0.7998128361456291469 ) ) ;
#202796 = CARTESIAN_POINT ( 'NONE',  ( 5.102750050473856547, 1.865045247124358818, 0.7672954931761333253 ) ) ;
#202798 = STYLED_ITEM ( 'NONE', ( #74865 ), #98352 ) ;
#202797 = CARTESIAN_POINT ( 'NONE',  ( 2.406250000000001776, 1.895863743164033277, -0.7852924748301132185 ) ) ;
#202799 = CARTESIAN_POINT ( 'NONE',  ( -1.201851678989727383E-14, 2.243750000682818158, 1.732050807568877637 ) ) ;
#202800 = CARTESIAN_POINT ( 'NONE',  ( 0.9383530073892000223, 1.897354475554638320, 0.3323884044314562858 ) ) ;
#202801 = CARTESIAN_POINT ( 'NONE',  ( -0.7500000000000006661, 8.989583334016129967, -1.299038105676657340 ) ) ;
#202802 = CARTESIAN_POINT ( 'NONE',  ( 3.990652734535464319, -1.277060150153148221, 1.817470393784472948 ) ) ;
#202803 = ORIENTED_EDGE ( 'NONE', *, *, #154706, .F. ) ;
#202804 = CARTESIAN_POINT ( 'NONE',  ( 6.883263157960364254, 2.447565407927353220, 2.329071302269662080 ) ) ;
#202805 = CARTESIAN_POINT ( 'NONE',  ( -1.500000000000013101, 1.170833333333352710, 0.8660254037844403729 ) ) ;
#202806 = CARTESIAN_POINT ( 'NONE',  ( 7.558834334818744338, 8.777393797832065303, 1.199719254218462483 ) ) ;
#202807 = CARTESIAN_POINT ( 'NONE',  ( 4.243338890952890630, 5.973648010910253880, -1.443375672974051449 ) ) ;
#202808 = CARTESIAN_POINT ( 'NONE',  ( -1.642778471874998480, -1.101041666188708801, 2.845375778867863303 ) ) ;
#202809 = CARTESIAN_POINT ( 'NONE',  ( 0.9970955524637573619, -2.168350899310825586, -0.4814931055744512411 ) ) ;
#202810 = CARTESIAN_POINT ( 'NONE',  ( 5.424254290899477304, 0.9654600744411747648, 1.707767180430696641 ) ) ;
#202811 = CARTESIAN_POINT ( 'NONE',  ( 8.270110514656021650, 11.63191745286530576, 1.082531754730557072 ) ) ;
#202812 = CARTESIAN_POINT ( 'NONE',  ( -0.3857294007042892936, 3.105957228677906024, 1.963430320088064063 ) ) ;
#202813 = CARTESIAN_POINT ( 'NONE',  ( 0.5444778865218368180, 2.155786741090206959, 0.1595364878888144988 ) ) ;
#202814 = CARTESIAN_POINT ( 'NONE',  ( -3.512971199716682591, 7.112567143062499930, 0.000000000000000000 ) ) ;
#202815 = CARTESIAN_POINT ( 'NONE',  ( 3.350102204537624306, -0.8385132117052511713, 1.884735577694598430 ) ) ;
#202816 = CARTESIAN_POINT ( 'NONE',  ( -5.687809136132860210, 6.594531066031826150, -1.199719254218446718 ) ) ;
#202817 = CARTESIAN_POINT ( 'NONE',  ( -1.201851678989727383E-14, 4.368750000682820378, -1.732050807568863648 ) ) ;
#202818 = CARTESIAN_POINT ( 'NONE',  ( 0.6823417656249917140, 4.905208333674755394, 1.181850606188765695 ) ) ;
#202819 = CARTESIAN_POINT ( 'NONE',  ( 4.551927186349598031, 1.870183863439809357, -0.04390777100237578529 ) ) ;
#202820 = CARTESIAN_POINT ( 'NONE',  ( 3.850049338483009009, 0.2070581644968480517, -1.721641829124469059 ) ) ;
#202821 = CARTESIAN_POINT ( 'NONE',  ( 3.104748464929545371, -0.3365338927540823533, 1.707397895346264738 ) ) ;
#202822 = CARTESIAN_POINT ( 'NONE',  ( 1.277341847617214476, 2.115720621435190907, -0.8829085993839781432 ) ) ;
#202823 = CARTESIAN_POINT ( 'NONE',  ( -1.201851678989727383E-14, 4.509375000341417916, -1.575800808251660134 ) ) ;
#202824 = CARTESIAN_POINT ( 'NONE',  ( 4.669523271137602904, 1.205110262999141701, 1.708276167780866661 ) ) ;
#202825 = CARTESIAN_POINT ( 'NONE',  ( 0.4976878544296211015, -0.6176706345307936274, -1.734562967469073236 ) ) ;
#202826 = DIRECTION ( 'NONE',  ( 0.000000000000000000, 0.000000000000000000, -1.000000000000000000 ) ) ;
#202827 =( LENGTH_UNIT ( ) NAMED_UNIT ( * ) SI_UNIT ( .MILLI., .METRE. ) );
#202828 = CARTESIAN_POINT ( 'NONE',  ( 1.705704151892040832, 1.882474636155605507, 0.7231385473688843879 ) ) ;
#202829 = CARTESIAN_POINT ( 'NONE',  ( -4.243338890952901288, 6.934017225211593249, -1.082531754730548412 ) ) ;
#202830 = CARTESIAN_POINT ( 'NONE',  ( 8.312826421212609063, 13.22328045796207086, -8.547122492678219885 ) ) ;
#202831 = CARTESIAN_POINT ( 'NONE',  ( -6.516665389662827934, 10.75452672124865217, 0.000000000000000000 ) ) ;
#202832 = CARTESIAN_POINT ( 'NONE',  ( 7.305145839664861640, 7.417091655897478653, 0.7998128361456341429 ) ) ;
#202833 = CARTESIAN_POINT ( 'NONE',  ( 2.649219347560148208, 0.2619616101627724736, 2.104190563435456518 ) ) ;
#202834 = DIRECTION ( 'NONE',  ( 3.347138415753902517E-16, 0.6000000000000018652, 0.7999999999999984901 ) ) ;
#202835 = CARTESIAN_POINT ( 'NONE',  ( 5.865807274569020180, 1.797851641234180509, -0.3166982042408575948 ) ) ;
#202836 = ORIENTED_EDGE ( 'NONE', *, *, #23138, .T. ) ;
#202837 = B_SPLINE_CURVE_WITH_KNOTS ( 'NONE', 3,
 ( #183573, #101255, #15732, #151100, #86079, #16791 ),
 .UNSPECIFIED., .F., .F.,
 ( 4, 2, 4 ),
 ( 0.000000000000000000, 0.0006594656818133617666, 0.001318931363626723533 ),
 .UNSPECIFIED. ) ;
#202838 = CARTESIAN_POINT ( 'NONE',  ( -7.293360289508603600, 7.473618190706972086, 0.000000000000000000 ) ) ;
#202839 = FACE_OUTER_BOUND ( 'NONE', #137664, .T. ) ;
#202840 = CARTESIAN_POINT ( 'NONE',  ( 3.285556943749998737, -1.392708332855375764, -1.896917185911906500 ) ) ;
#202841 = CARTESIAN_POINT ( 'NONE',  ( -7.555971681517696936, 7.709721804725773175, 0.7998128361456462443 ) ) ;
#202842 = CARTESIAN_POINT ( 'NONE',  ( 1.898700399197379651, -1.981625571768164340, -0.3898374508689693152 ) ) ;
#202843 = CARTESIAN_POINT ( 'NONE',  ( 0.1300960903409088820, -1.296115720595720333, -1.660425602283533308 ) ) ;
#202844 = CARTESIAN_POINT ( 'NONE',  ( -4.981695098378565945, 4.776675467721892332, -0.7998128361456362523 ) ) ;
#202845 = CARTESIAN_POINT ( 'NONE',  ( 4.574962676454192412, 1.700228875758927671, 0.7569903647998057483 ) ) ;
#202846 = CARTESIAN_POINT ( 'NONE',  ( 9.738834413317897898, 10.25639499182604730, 0.000000000000000000 ) ) ;
#202847 = CARTESIAN_POINT ( 'NONE',  ( -4.858757509019071996, 5.629766575900002401, 7.500000000000000000 ) ) ;
#202848 = VERTEX_POINT ( 'NONE', #13110 ) ;
#202849 = CARTESIAN_POINT ( 'NONE',  ( -4.497554271431319250, 6.270232621468402989, -1.599625672291256295 ) ) ;
#202850 = CARTESIAN_POINT ( 'NONE',  ( -6.170932472514347289, 10.35117165124207972, 0.000000000000000000 ) ) ;
#202851 = CARTESIAN_POINT ( 'NONE',  ( 4.793472150574508817, 1.354911484294840429, 1.223852735664505698 ) ) ;
#202853 = CARTESIAN_POINT ( 'NONE',  ( -3.990254785474510513, 7.829054500403880290, -0.2746884413801879976 ) ) ;
#202852 = CARTESIAN_POINT ( 'NONE',  ( -2.993318053567081360, 6.714231172462041819, 0.000000000000000000 ) ) ;
#202854 = CARTESIAN_POINT ( 'NONE',  ( 5.253852870291571442, 7.792406146126436006, -1.285611862062207011 ) ) ;
#202855 = CARTESIAN_POINT ( 'NONE',  ( 0.5613444508567478897, 1.446164810419462432, -0.9560955100236142590 ) ) ;
#202856 = CARTESIAN_POINT ( 'NONE',  ( 0.04040834310030903126, -1.341606091951352164, -1.108378290077848494 ) ) ;
#202857 = CARTESIAN_POINT ( 'NONE',  ( 4.987122935671228774, -0.2785958505117277495, -2.290767236937583995 ) ) ;
#202858 = CARTESIAN_POINT ( 'NONE',  ( 3.390420931869152721, 6.113185632892752075, -1.199719254218452047 ) ) ;
#202859 = CARTESIAN_POINT ( 'NONE',  ( 1.264995835974036975, -1.861883480270887903, -0.8836341380922418942 ) ) ;
#202860 = CARTESIAN_POINT ( 'NONE',  ( 5.035963992472171746, 7.962709526937818083, 1.199719254218462483 ) ) ;
#202861 = ADVANCED_FACE ( 'NONE', ( #77045 ), #193995, .T. ) ;
#202862 = CARTESIAN_POINT ( 'NONE',  ( 0.5267199648841465187, 1.994564833640038781, -0.2930222482238133419 ) ) ;
#202863 = CARTESIAN_POINT ( 'NONE',  ( 7.853188201116851452, 15.31763947413069715, -9.016399092843794705 ) ) ;
#202864 = CARTESIAN_POINT ( 'NONE',  ( -5.315678745009726924, 8.359319748223434487, -1.199719254218453823 ) ) ;
#202865 = CARTESIAN_POINT ( 'NONE',  ( 5.594569530875262764, -0.4557361262383100020, -1.814172972432124720 ) ) ;
#202867 = CARTESIAN_POINT ( 'NONE',  ( -5.093022980588950865, 5.970890227889075419, -1.199719254218453823 ) ) ;
#202866 = CARTESIAN_POINT ( 'NONE',  ( 3.832203377193269755, -0.9874410831685247469, -1.637625244210038300 ) ) ;
#202868 = CARTESIAN_POINT ( 'NONE',  ( 4.547634279845023109, -1.704780727694398479, -1.401453192282381188 ) ) ;
#202869 = CARTESIAN_POINT ( 'NONE',  ( 0.6125000000000071498, 2.395833334016134408, 1.060881119635924019 ) ) ;
#202870 = DIRECTION ( 'NONE',  ( -0.000000000000000000, 1.000000000000000000, -0.000000000000000000 ) ) ;
#202871 = CARTESIAN_POINT ( 'NONE',  ( 3.540087506499646874, 7.144202834309300698, -0.7216878364870338292 ) ) ;
#202872 = CARTESIAN_POINT ( 'NONE',  ( -4.448483798615272100, 8.203998508444197313, 0.000000000000000000 ) ) ;
#202873 = CARTESIAN_POINT ( 'NONE',  ( 6.024112365460934981, -2.104525519549589330, 0.2592714029671301934 ) ) ;
#202874 = EDGE_LOOP ( 'NONE', ( #76006, #27704, #138508, #168928 ) ) ;
#202875 = CARTESIAN_POINT ( 'NONE',  ( 3.751255533806226339, -1.888273344036644819, 1.326175916821286105 ) ) ;
#202876 = CARTESIAN_POINT ( 'NONE',  ( 3.560947883890089649, 1.548132398191165882, -1.204989647596923508 ) ) ;
#202877 = CARTESIAN_POINT ( 'NONE',  ( -4.098307573080856692, 8.003385611894792362, 0.7998128361456350310 ) ) ;
#202878 = CARTESIAN_POINT ( 'NONE',  ( 1.059338230090471011, 1.600537254139059673, 1.134074526779847769 ) ) ;
#202879 = CARTESIAN_POINT ( 'NONE',  ( 8.944921657900962941, 14.55297637781186637, 7.932298026445150363 ) ) ;
#202880 = CARTESIAN_POINT ( 'NONE',  ( 4.184706906422049677, 7.590773377626947038, -0.8858016570119742195 ) ) ;
#202881 = ORIENTED_EDGE ( 'NONE', *, *, #175529, .T. ) ;
#202882 = CARTESIAN_POINT ( 'NONE',  ( 5.911342272548038679, -1.897112096406332382, 0.6839327336411115121 ) ) ;
#202883 = CARTESIAN_POINT ( 'NONE',  ( -8.123306592882240551, 12.62894145833798376, 0.000000000000000000 ) ) ;
#202884 = SURFACE_STYLE_USAGE ( .BOTH. , #136860 ) ;
#202886 = VECTOR ( 'NONE', #93521, 1000.000000000000114 ) ;
#202885 = CARTESIAN_POINT ( 'NONE',  ( 2.694371920525945097, 1.027083080403013993, -1.912793749723267211 ) ) ;
#202887 = CARTESIAN_POINT ( 'NONE',  ( 5.554000203453580475, 6.508696987897830688, -1.199719254218452047 ) ) ;
#202888 = CARTESIAN_POINT ( 'NONE',  ( 1.019968326173793960, -0.5097545255977399270, 2.058319881341897695 ) ) ;
#202889 = B_SPLINE_CURVE_WITH_KNOTS ( 'NONE', 3,
 ( #161295, #80028, #130988, #127821 ),
 .UNSPECIFIED., .F., .F.,
 ( 4, 4 ),
 ( 4.470280076681866734E-19, 0.0001925329755551839501 ),
 .UNSPECIFIED. ) ;
#202890 = CARTESIAN_POINT ( 'NONE',  ( -1.201851678989727383E-14, 1.493750000682814383, 1.732050807568877637 ) ) ;
#202891 = CARTESIAN_POINT ( 'NONE',  ( 7.879259827836241570, 12.34422023245099176, 1.040834085586084257E-14 ) ) ;
#202892 = FILL_AREA_STYLE_COLOUR ( '', #180995 ) ;
#202893 = CARTESIAN_POINT ( 'NONE',  ( 5.004104291928844539, 8.031804922028364047, 1.127571413376940335 ) ) ;
#202894 = CARTESIAN_POINT ( 'NONE',  ( 0.5618817370758311114, 2.038728707766800596, -0.2996719410968719521 ) ) ;
#202896 = CARTESIAN_POINT ( 'NONE',  ( 6.827182134110195477, 7.052946558436035573, 2.509100386683714490 ) ) ;
#202895 = CARTESIAN_POINT ( 'NONE',  ( -8.631737353394710155, 13.22211067893587533, 1.040834085586084257E-14 ) ) ;
#202897 = CARTESIAN_POINT ( 'NONE',  ( -1.364683531250012516, 2.280208333674751842, 0.7879004041258379498 ) ) ;
#202898 = CARTESIAN_POINT ( 'NONE',  ( 5.900277318768097246, 7.249539301847896411, -1.301905728482563251 ) ) ;
#202899 =( BOUNDED_CURVE ( )  B_SPLINE_CURVE ( 2, ( #36466, #3941, #153435, #1809, #150240, #54865, #168604, #166473, #20206 ),
 .UNSPECIFIED., .F., .T. ) 
 B_SPLINE_CURVE_WITH_KNOTS ( ( 3, 2, 2, 2, 3 ),
 ( 0.8303571428571429047, 0.8333333333333333703, 0.8392857142857143016, 0.8452380952380952328, 0.8482142857142856984 ),
 .UNSPECIFIED. ) 
 CURVE ( )  GEOMETRIC_REPRESENTATION_ITEM ( )  RATIONAL_B_SPLINE_CURVE ( ( 0.9330127018922194093, 0.9330127018922206306, 1.000000000000000000, 0.8660254037844387076, 1.000000000000000000, 0.8660254037844387076, 1.000000000000000000, 0.9330127018922194093, 0.9330127018922194093 ) ) 
 REPRESENTATION_ITEM ( '' )  );
#202900 = VERTEX_POINT ( 'NONE', #176693 ) ;
#202901 = CARTESIAN_POINT ( 'NONE',  ( 4.723256143441832755, 1.665581346147155806, 0.9393396248940298898 ) ) ;
#202902 = CARTESIAN_POINT ( 'NONE',  ( 5.207753166488873653, -1.761066459785052274, 0.1758167199723305041 ) ) ;
#202903 = CARTESIAN_POINT ( 'NONE',  ( 7.225569521440261767, 7.394528961293920233, -0.7998128361456341429 ) ) ;
#202904 = CARTESIAN_POINT ( 'NONE',  ( -8.649738815838677652, 13.03518635187974262, 0.7216878364870357165 ) ) ;
#202906 = EDGE_CURVE ( 'NONE', #101986, #179040, #99653, .T. ) ;
#202905 = CARTESIAN_POINT ( 'NONE',  ( -0.05289022600267567070, -1.656485410061825592, 0.7338673832079073422 ) ) ;
#202908 = CARTESIAN_POINT ( 'NONE',  ( 1.376049117821566137, -1.906831126389372022, -0.1839060664316337634 ) ) ;
#202907 = CARTESIAN_POINT ( 'NONE',  ( 6.928203230275522095, 15.51887838114830132, 9.797958971132704420 ) ) ;
#202909 = CARTESIAN_POINT ( 'NONE',  ( 1.943885480841448965, 1.426152643941134501, 1.501071833787496645 ) ) ;
#202910 = CARTESIAN_POINT ( 'NONE',  ( 0.6823417656249899377, 0.6552083336747518416, 1.181850606188755259 ) ) ;
#202911 = CARTESIAN_POINT ( 'NONE',  ( 0.2507688454781953902, -1.584965806562924628, 1.172240258958085146 ) ) ;
#202912 = CARTESIAN_POINT ( 'NONE',  ( 2.631258204695927194, -1.703542010001803275, 0.6570300758180421807 ) ) ;
#202914 = CARTESIAN_POINT ( 'NONE',  ( 5.510920874727778696, 7.454463421478725316, 1.249874847645112697 ) ) ;
#202913 = CARTESIAN_POINT ( 'NONE',  ( 0.5754005350990994971, -2.174928102591418888, -0.7718245971977951703 ) ) ;
#202915 = CARTESIAN_POINT ( 'NONE',  ( -1.364683531250014514, 0.2385416670080863499, -0.7879004041258359514 ) ) ;
#202916 = VECTOR ( 'NONE', #39020, 1000.000000000000114 ) ;
#202917 = CARTESIAN_POINT ( 'NONE',  ( 4.580570881008502404, 1.271380961112581032, -1.624167499240388057 ) ) ;
#202918 = CARTESIAN_POINT ( 'NONE',  ( -5.065942953000576843, 9.062017211809330064, -0.7998128361456231517 ) ) ;
#202919 = CARTESIAN_POINT ( 'NONE',  ( 8.911787042884274257, 9.291506392986812912, 0.7998128361456462443 ) ) ;
#202920 = CARTESIAN_POINT ( 'NONE',  ( -11.86239285000045918, 11.37999999999998302, 1.812080536912751061 ) ) ;
#202921 = CARTESIAN_POINT ( 'NONE',  ( 6.654354466208897811, 6.657835053532175529, 0.7998128361456341429 ) ) ;
#202923 = CARTESIAN_POINT ( 'NONE',  ( 0.7499999999999902300, 3.233333333333352044, 1.299038105676669330 ) ) ;
#202922 = CARTESIAN_POINT ( 'NONE',  ( 5.508848719172433128, 1.596710022150628294, -1.373279487321391379 ) ) ;
#202924 = STYLED_ITEM ( 'NONE', ( #61112 ), #196848 ) ;
#202925 = EDGE_CURVE ( 'NONE', #31219, #10132, #113024, .T. ) ;
#202926 = CARTESIAN_POINT ( 'NONE',  ( 6.268043187460373922, -2.055199631210803624, 0.2494731385529954104 ) ) ;
#202927 = CARTESIAN_POINT ( 'NONE',  ( -1.364683531250012516, 1.092708333674754506, 0.7879004041258379498 ) ) ;
#202928 = CARTESIAN_POINT ( 'NONE',  ( 4.077527805175058973, 2.036875575534887961, -0.7240464584713502960 ) ) ;
#202929 = CARTESIAN_POINT ( 'NONE',  ( 4.072919328976184694, -1.495020084728536203, 1.358112258667160344 ) ) ;
#202932 = CARTESIAN_POINT ( 'NONE',  ( 4.989037340148863464, 8.764367963574922982, -0.7216878364870257245 ) ) ;
#202931 = CARTESIAN_POINT ( 'NONE',  ( -3.285556943750000070, -2.909374999522040817, 0.000000000000000000 ) ) ;
#202930 = CARTESIAN_POINT ( 'NONE',  ( -3.486133158594716510E-16, 2.687500000000001332, -1.225000000000008749 ) ) ;
#202933 = CARTESIAN_POINT ( 'NONE',  ( -6.306477729012051725, 7.386587434382707151, 1.199719254218452047 ) ) ;
#202934 = CARTESIAN_POINT ( 'NONE',  ( 2.624232735793774030, 2.001858099149746550, 0.2420302859193757539 ) ) ;
#202935 = CARTESIAN_POINT ( 'NONE',  ( -8.636707547105197946, 10.03491254549959777, -1.199719254218446718 ) ) ;
#202937 = CARTESIAN_POINT ( 'NONE',  ( -10.99970480893081337, -5.907420853759282053, -0.08058608058607207025 ) ) ;
#202936 = CARTESIAN_POINT ( 'NONE',  ( -2.754277761870538299, 6.365074488824250309, 1.040834085586084257E-14 ) ) ;
#202938 = CARTESIAN_POINT ( 'NONE',  ( -0.6823417656250039265, 8.567708333674733723, -1.181850606188755259 ) ) ;
#202939 = CARTESIAN_POINT ( 'NONE',  ( 5.308822938259078583, -0.4706598425541131947, -1.853433239416848677 ) ) ;
#202940 = DIRECTION ( 'NONE',  ( -7.387867266669436732E-31, 1.000000000000000000, 8.546850786086424434E-32 ) ) ;
#202942 = CARTESIAN_POINT ( 'NONE',  ( 4.200796113533305842, 1.844717850457804120, 0.8146114232021259838 ) ) ;
#202941 = CARTESIAN_POINT ( 'NONE',  ( -9.137832345486311070, 9.763151945929928743, 1.040834085586084257E-14 ) ) ;
#202943 = CARTESIAN_POINT ( 'NONE',  ( -1.001543065824772872E-14, 5.712500000000021672, 1.732050807568877637 ) ) ;
#202944 = CARTESIAN_POINT ( 'NONE',  ( 1.364683531250000303, 15.31770833367473017, -0.7879004041258355073 ) ) ;
#202945 = CARTESIAN_POINT ( 'NONE',  ( 6.827182134110228340, 0.006757161851634120239, 1.710856279483467191 ) ) ;
#202946 = CARTESIAN_POINT ( 'NONE',  ( 5.737035277238070385, 6.722237907313067140, -1.199719254218452047 ) ) ;
#202948 = CARTESIAN_POINT ( 'NONE',  ( 9.243516698675458443, 13.40993305631030985, 7.925370479070547702 ) ) ;
#202947 = CARTESIAN_POINT ( 'NONE',  ( 7.782016984564043227, 12.02284421539267356, 0.7216878364870438212 ) ) ;
#202949 = CARTESIAN_POINT ( 'NONE',  ( -4.785665035499573783, 5.645992631913323123, 1.082531754730558626 ) ) ;
#202950 = CARTESIAN_POINT ( 'NONE',  ( 5.747288119592351308, -1.474170506619469023, -1.151262835514428540 ) ) ;
#202951 = CARTESIAN_POINT ( 'NONE',  ( 6.310797300923185915, -0.5409384057308598281, -1.939081195975641769 ) ) ;
#202952 = CARTESIAN_POINT ( 'NONE',  ( -0.3000000000000155320, 3.999999999999955147, 1.007084189318345757 ) ) ;
#202953 = COLOUR_RGB ( '', 0.08235294, 0.09019608, 0.10196078) ;
#202955 =( BOUNDED_CURVE ( )  B_SPLINE_CURVE ( 2, ( #56952, #173935, #91616, #124178, #137145, #120966, #25507, #186937, #157666 ),
 .UNSPECIFIED., .F., .T. ) 
 B_SPLINE_CURVE_WITH_KNOTS ( ( 3, 2, 2, 2, 3 ),
 ( 0.9017857142857143016, 0.9047619047619047672, 0.9107142857142856984, 0.9166666666666666297, 0.9196428571428570953 ),
 .UNSPECIFIED. ) 
 CURVE ( )  GEOMETRIC_REPRESENTATION_ITEM ( )  RATIONAL_B_SPLINE_CURVE ( ( 0.9330127018922194093, 0.9330127018922194093, 1.000000000000000000, 0.8660254037844387076, 1.000000000000000000, 0.8660254037844387076, 1.000000000000000000, 0.9330127018922206306, 0.9330127018922194093 ) ) 
 REPRESENTATION_ITEM ( '' )  );
#202954 = CARTESIAN_POINT ( 'NONE',  ( 1.903268718874175480, -1.751121435885591548, 1.104011288380807532 ) ) ;
#202956 = CARTESIAN_POINT ( 'NONE',  ( -2.276824562219559311E-15, -8.030730635398800388, -11.29670623088187398 ) ) ;
#202957 = ORIENTED_EDGE ( 'NONE', *, *, #47152, .F. ) ;
#202958 = CARTESIAN_POINT ( 'NONE',  ( 0.7554827284574801016, 1.942536278707338360, -0.5405140857882018146 ) ) ;
#202959 = CARTESIAN_POINT ( 'NONE',  ( 1.001899194773261170, -0.8131845483106721062, 1.618847804792804324 ) ) ;
#202960 = CARTESIAN_POINT ( 'NONE',  ( 3.540087506499646874, 7.144202834309300698, -0.7216878364870338292 ) ) ;
#202961 = DIRECTION ( 'NONE',  ( -1.000000000000000000, 0.000000000000000000, -8.638326563840826660E-31 ) ) ;
#202962 = AXIS2_PLACEMENT_3D ( 'NONE', #149330, #133116, #199114 ) ;
#202963 = CARTESIAN_POINT ( 'NONE',  ( 8.717529583462654941, 9.272798723569005475, 0.7216878364870458196 ) ) ;
#202964 = CARTESIAN_POINT ( 'NONE',  ( 7.613066949273408213, 8.840665181362512115, -1.199719254218441611 ) ) ;
#202966 = CARTESIAN_POINT ( 'NONE',  ( 6.081633583971849610, -0.6405020660514448849, 1.805506905929341821 ) ) ;
#202965 = CARTESIAN_POINT ( 'NONE',  ( -5.259673527097670664, 8.223703984000886535, -1.199719254218446718 ) ) ;
#202967 = SURFACE_STYLE_USAGE ( .BOTH. , #100159 ) ;
#202968 = CARTESIAN_POINT ( 'NONE',  ( -4.103031383223492590, 3.978538327596326862, -0.5488639320762221940 ) ) ;
#202969 = CARTESIAN_POINT ( 'NONE',  ( 1.364683531249986537, -0.8239583329919186738, 0.7879004041258500513 ) ) ;
#202971 = ORIENTED_EDGE ( 'NONE', *, *, #31468, .T. ) ;
#202970 = CARTESIAN_POINT ( 'NONE',  ( 3.389175213736292047, 5.937492935125556315, 1.082531754730558626 ) ) ;
#202972 = CARTESIAN_POINT ( 'NONE',  ( -2.785310492603665367, 5.336947110424484109, 1.199719254218462483 ) ) ;
#202973 = CARTESIAN_POINT ( 'NONE',  ( 3.362350911093567873, 0.9703303321016673033, 1.931748911306984784 ) ) ;
#202974 = CARTESIAN_POINT ( 'NONE',  ( -7.932929277771797238, 8.427708043588125975, 0.000000000000000000 ) ) ;
#202975 = CARTESIAN_POINT ( 'NONE',  ( 7.214347136247488912, 7.589362211809770997, -0.7216878364870317197 ) ) ;
#202976 = CARTESIAN_POINT ( 'NONE',  ( 0.8793290508635929204, -1.919567575575848339, -0.9014759086384204201 ) ) ;
#202977 = CARTESIAN_POINT ( 'NONE',  ( 6.194357462883205656, -1.817092693925309810, -0.1759843941628037312 ) ) ;
#202978 = CARTESIAN_POINT ( 'NONE',  ( 1.809780422520257170, -1.956919260803160032, 0.2374922769308157044 ) ) ;
#202979 = CARTESIAN_POINT ( 'NONE',  ( 5.133030909251353968, 1.769313487831367659, 0.7262901588861517821 ) ) ;
#202980 = VERTEX_POINT ( 'NONE', #196148 ) ;
#202981 = PLANE ( 'NONE',  #163525 ) ;
#202982 = CARTESIAN_POINT ( 'NONE',  ( 5.336368261742150843, -1.095693791129894956, 1.636418990172120003 ) ) ;
#202984 = B_SPLINE_CURVE_WITH_KNOTS ( 'NONE', 3,
 ( #30562, #176797, #31626, #196252 ),
 .UNSPECIFIED., .F., .F.,
 ( 4, 4 ),
 ( 0.000000000000000000, 0.0005592965258961650823 ),
 .UNSPECIFIED. ) ;
#202983 = CARTESIAN_POINT ( 'NONE',  ( 0.4627034902389154936, 0.1913720229725413835, -1.932491135362510715 ) ) ;
#202985 = EDGE_LOOP ( 'NONE', ( #117304, #68259, #48884, #56770 ) ) ;
#202986 = CARTESIAN_POINT ( 'NONE',  ( -6.147696309153835692, 6.137010213626392208, 0.7998128361456281477 ) ) ;
#202987 = CARTESIAN_POINT ( 'NONE',  ( -3.284818356260900796, 7.054314858938165678, 0.7998128361456352531 ) ) ;
#202990 = EDGE_CURVE ( 'NONE', #67257, #143616, #166841, .T. ) ;
#202989 = CARTESIAN_POINT ( 'NONE',  ( 5.139949632912227173, 8.050339434155988627, -1.082531754730548412 ) ) ;
#202988 = CARTESIAN_POINT ( 'NONE',  ( 6.909851844459134362, 11.21324425184434936, -0.7998128361456291469 ) ) ;
#202992 = ORIENTED_EDGE ( 'NONE', *, *, #186024, .F. ) ;
#202991 = CARTESIAN_POINT ( 'NONE',  ( 5.057238878282278804, -1.638088962530854786, 0.9864336689310859718 ) ) ;
#202993 = CARTESIAN_POINT ( 'NONE',  ( 1.378255502416311895, 1.315327575222959622, 1.771799650011764538 ) ) ;
#202994 = CARTESIAN_POINT ( 'NONE',  ( 1.445103857048099405, 8.688264192037884470, 2.625611233228254626 ) ) ;
#202995 = CARTESIAN_POINT ( 'NONE',  ( 6.094395157121155648, -1.075028013068216604, 1.701836141867618446 ) ) ;
#202996 = CARTESIAN_POINT ( 'NONE',  ( 4.367134876933267407, 8.109091433148536865, 0.000000000000000000 ) ) ;
#202997 = CARTESIAN_POINT ( 'NONE',  ( 10.99526901688165026, -7.794005300192742069, -0.3296348669024388722 ) ) ;
#202998 = DIRECTION ( 'NONE',  ( 1.908195823574487804E-17, 1.000000000000000000, -3.097714438736600596E-15 ) ) ;
#202999 = CARTESIAN_POINT ( 'NONE',  ( 2.523957353938070192, 2.030885678308389952, -0.4015143504868187718 ) ) ;
#203000 = CARTESIAN_POINT ( 'NONE',  ( -5.168682875307782254, 7.053215992657626110, -1.599625672291256295 ) ) ;
#203001 = CARTESIAN_POINT ( 'NONE',  ( -4.638545736399841246, 8.340143690112583386, 0.3695662286686048903 ) ) ;
#203003 = CARTESIAN_POINT ( 'NONE',  ( 0.1984014031938194922, -2.161264429664040421, -0.05129915172277095536 ) ) ;
#203002 = CARTESIAN_POINT ( 'NONE',  ( -4.928552533767591726, 5.708731696605642725, 1.199719254218462483 ) ) ;
#203004 = CARTESIAN_POINT ( 'NONE',  ( -10.64364919647040786, 5.928722196471193584, -5.549781512408035411 ) ) ;
#203005 = FILL_AREA_STYLE_COLOUR ( '', #156337 ) ;
#203006 = CARTESIAN_POINT ( 'NONE',  ( 0.2039282260587823581, -6.674536912880641104, 9.612297698795920553 ) ) ;
#203007 = CARTESIAN_POINT ( 'NONE',  ( -1.364683531250010295, 12.44270833367473372, 0.7879004041258445001 ) ) ;
#203009 = CARTESIAN_POINT ( 'NONE',  ( -4.457598643843001973, 8.422558527783969851, 0.000000000000000000 ) ) ;
#203008 = CARTESIAN_POINT ( 'NONE',  ( 6.925078400183546812, 3.702220002068328242, 2.370079373711677206 ) ) ;
#203010 = CARTESIAN_POINT ( 'NONE',  ( 5.432138663567621428, -1.371958567392589146, -1.060553414760868618 ) ) ;
#203011 = CARTESIAN_POINT ( 'NONE',  ( -4.776550190716183586, 4.467063398790632966, 1.214306433183764966E-14 ) ) ;
#203012 = CARTESIAN_POINT ( 'NONE',  ( 3.098552089154332556, 2.054082100768514607, 0.2579794602402472603 ) ) ;
#203013 = CARTESIAN_POINT ( 'NONE',  ( 4.288735948182021751, 1.635604132441673020, -1.344385869115312770 ) ) ;
#203014 = CARTESIAN_POINT ( 'NONE',  ( 8.274553823041976841, 8.548067636504127265, 1.040834085586084257E-14 ) ) ;
#203015 = CARTESIAN_POINT ( 'NONE',  ( -1.364683531250012516, 4.238541667008089320, -0.7879004041258300672 ) ) ;
#203016 = CARTESIAN_POINT ( 'NONE',  ( 2.817198160248539196, -1.711224680871022086, -0.9748066430285988737 ) ) ;
#203017 = CARTESIAN_POINT ( 'NONE',  ( 0.5625819312903357350, 0.5574351770905332515, 1.829310545699929458 ) ) ;
#203018 = CARTESIAN_POINT ( 'NONE',  ( 5.085981902069889315, -2.274473487728204013, -0.2844877896996683142 ) ) ;
#203019 = CARTESIAN_POINT ( 'NONE',  ( 1.875362892791394787, 1.747422460009705913, -0.5287960245906262458 ) ) ;
#203020 = CARTESIAN_POINT ( 'NONE',  ( 4.878955176071345434, 6.785476686873604280, -1.599625672291269396 ) ) ;
#203021 = CARTESIAN_POINT ( 'NONE',  ( 4.785665035499516051, 8.527100274817353665, -0.7216878364870207285 ) ) ;
#203022 = CARTESIAN_POINT ( 'NONE',  ( -6.347188469492005325, 10.55680364771601809, -0.7998128361456291469 ) ) ;
#203023 = CARTESIAN_POINT ( 'NONE',  ( 2.373293634344127767, -1.753592693251155632, -0.9887173157705446691 ) ) ;
#203024 = CARTESIAN_POINT ( 'NONE',  ( 3.678520109711844732, 1.247982904293298168, -1.513573691770610186 ) ) ;
#203025 = CARTESIAN_POINT ( 'NONE',  ( -8.342344591110322227, 8.627156865917170236, -0.7998128361456291469 ) ) ;
#203026 = VECTOR ( 'NONE', #48657, 1000.000000000000000 ) ;
#203027 = CARTESIAN_POINT ( 'NONE',  ( -5.599681137644054729, 6.491715067794862293, 1.199719254218450271 ) ) ;
#203028 = CARTESIAN_POINT ( 'NONE',  ( 0.07556134207192634344, 1.307170157424314638, -2.493659143521540500 ) ) ;
#203030 = CARTESIAN_POINT ( 'NONE',  ( 5.102326758870145973, -0.5985492928855026262, -1.665706573615277852 ) ) ;
#203029 = CARTESIAN_POINT ( 'NONE',  ( 6.105435528804215473, -2.075010666747591159, 0.2545828925317530911 ) ) ;
#203031 = CARTESIAN_POINT ( 'NONE',  ( 3.946537740505243974, 2.817530495244580102, -0.7749999999999935829 ) ) ;
#203032 = CARTESIAN_POINT ( 'NONE',  ( 1.289316216709124996, 1.661312375189183399, 1.429258102917586815 ) ) ;
#203033 = CARTESIAN_POINT ( 'NONE',  ( 6.456985410506528744, 0.2896317775202154610, -1.715898445072817413 ) ) ;
#203034 = CARTESIAN_POINT ( 'NONE',  ( 7.100719765255169236, 9.307259030929609267, -1.599625672291262513 ) ) ;
#203035 = DIRECTION ( 'NONE',  ( 0.000000000000000000, 0.000000000000000000, 1.000000000000000000 ) ) ;
#203036 = CARTESIAN_POINT ( 'NONE',  ( 0.3866022076702098076, -0.1098403002397010941, 2.295889243394435564 ) ) ;
#203037 = CARTESIAN_POINT ( 'NONE',  ( -0.005964567173097347699, -2.191213315851054944, -0.04726126812268362232 ) ) ;
#203038 = CARTESIAN_POINT ( 'NONE',  ( 6.380242484794338864, -0.2077342984398328762, 1.721287130621736772 ) ) ;
#203039 = CARTESIAN_POINT ( 'NONE',  ( 2.842613246588860942, 2.190307313262893185, 0.2694104812042824038 ) ) ;
#203040 = CARTESIAN_POINT ( 'NONE',  ( 0.3741910912563637948, -2.129432730031981080, 0.4223156635175562279 ) ) ;
#203041 = DIRECTION ( 'NONE',  ( -7.993605777301127091E-15, 0.000000000000000000, 1.000000000000000000 ) ) ;
#203042 = CARTESIAN_POINT ( 'NONE',  ( 1.059931528796464129, 1.266109226500349960, 1.696929307225014449 ) ) ;
#203043 = CARTESIAN_POINT ( 'NONE',  ( 3.375000000000002665, 2.052068128417946724, -1.927395870058053847E-13 ) ) ;
#203044 = CARTESIAN_POINT ( 'NONE',  ( 6.827182134110194589, 2.412578537245218424, 2.569476350730160785 ) ) ;
#203045 = CARTESIAN_POINT ( 'NONE',  ( 5.754890659886483739, -1.518548266084504439, 1.185242666505934572 ) ) ;
#203046 = ORIENTED_EDGE ( 'NONE', *, *, #83250, .F. ) ;
#203048 = CARTESIAN_POINT ( 'NONE',  ( -1.001543065824772872E-14, 5.462500000000020783, 1.732050807568877637 ) ) ;
#203047 = CARTESIAN_POINT ( 'NONE',  ( 1.962814135067984411, -2.097685689255949448, -0.9248770880663819138 ) ) ;
#203049 = CARTESIAN_POINT ( 'NONE',  ( 3.174580523894166006, 6.855427711185178019, 0.7998128361456341429 ) ) ;
#203050 = CARTESIAN_POINT ( 'NONE',  ( 5.494078562035752178, 7.432844293840273231, -1.599625672291262513 ) ) ;
#203051 = CARTESIAN_POINT ( 'NONE',  ( 3.176664282717697851, 1.000473465829452735, 1.983322933999843052 ) ) ;
#203052 = CARTESIAN_POINT ( 'NONE',  ( -7.375272376154077492, 11.54830883891436422, -0.7216878364870267237 ) ) ;
#203053 = CARTESIAN_POINT ( 'NONE',  ( 5.910991785878156435, 7.919243054989755670, -1.443375672974057666 ) ) ;
#203054 = CARTESIAN_POINT ( 'NONE',  ( -7.280365300414089802, 10.47721470291632784, 1.082531754730549967 ) ) ;
#203055 = CARTESIAN_POINT ( 'NONE',  ( 4.258669648468268676, 7.982548666606070320, 0.7216878364870257245 ) ) ;
#203057 = VERTEX_POINT ( 'NONE', #117079 ) ;
#203056 = VECTOR ( 'NONE', #182694, 1000.000000000000000 ) ;
#203058 = CARTESIAN_POINT ( 'NONE',  ( 1.424454163599726320, -1.462446849824734274, -1.388484543128357229 ) ) ;
#203060 = CARTESIAN_POINT ( 'NONE',  ( 6.268047042621852860, -2.047536660891946525, 0.2488583125946699504 ) ) ;
#203059 = CARTESIAN_POINT ( 'NONE',  ( 8.450809820019639318, 8.753699632978056755, -0.7998128361456291469 ) ) ;
#203061 = CARTESIAN_POINT ( 'NONE',  ( 5.519577934094852978, 7.532869904567736974, 1.443375672974064550 ) ) ;
#203062 = CARTESIAN_POINT ( 'NONE',  ( 6.022986557963563747, -1.635662919198093812, 0.5951793741951169059 ) ) ;
#203063 = CARTESIAN_POINT ( 'NONE',  ( -10.95308175811721085, 13.79999999999999893, -1.800000000000001155 ) ) ;
#203064 = CARTESIAN_POINT ( 'NONE',  ( -1.201851678989727383E-14, 2.321875000341416584, 1.575800808251672791 ) ) ;
#203065 = CARTESIAN_POINT ( 'NONE',  ( 1.580939025779507956, 1.637719487297364163, -0.6712238910871449749 ) ) ;
#203066 = CARTESIAN_POINT ( 'NONE',  ( -0.01695367945527340853, -2.016028864686558730, -0.04667425414178058563 ) ) ;
#203067 = CARTESIAN_POINT ( 'NONE',  ( 6.444851825500396814, -1.403812859381381895, -1.028626497576446086 ) ) ;
#203068 = CARTESIAN_POINT ( 'NONE',  ( 4.687240393977892161, 1.697883010200517129, 1.540384229137826466 ) ) ;
#203069 = CARTESIAN_POINT ( 'NONE',  ( 3.503688343963583307, -0.7473321665184139428, -1.682825604429179833 ) ) ;
#203070 = CARTESIAN_POINT ( 'NONE',  ( 7.964525173024008531, 11.37936423758166526, 1.199719254218460707 ) ) ;
#203071 = DIRECTION ( 'NONE',  ( 0.000000000000000000, -1.000000000000000000, 0.000000000000000000 ) ) ;
#203072 = CARTESIAN_POINT ( 'NONE',  ( 3.786012796616508247, -0.9002957760516903107, 1.588078298607284111 ) ) ;
#203073 = CARTESIAN_POINT ( 'NONE',  ( 4.799454022740247794, 1.388487131293577592, -1.462444391756134943 ) ) ;
#203074 = CARTESIAN_POINT ( 'NONE',  ( -9.341731535015849630, 10.85744053139533349, 1.199719254218462483 ) ) ;
#203076 = CARTESIAN_POINT ( 'NONE',  ( -7.930593509350902792, 8.217056947189661287, -0.7998128361456362523 ) ) ;
#203075 = CARTESIAN_POINT ( 'NONE',  ( 3.643696890507712283, -1.711652922788420739, -1.479685619365896265 ) ) ;
#203077 = CARTESIAN_POINT ( 'NONE',  ( 6.563511373971260277, 0.3638278135829931537, -2.074131770586047363 ) ) ;
#203078 = CARTESIAN_POINT ( 'NONE',  ( 3.877443546529443452, -0.1552652338182025915, 2.064615508632794860 ) ) ;
#203079 = CARTESIAN_POINT ( 'NONE',  ( 3.704402285031850539, 5.344888637335695414, -1.599625672291262513 ) ) ;
#203080 = CARTESIAN_POINT ( 'NONE',  ( 1.360316468749955598, 1.526041667008097180, 0.7853790794158861388 ) ) ;
#203081 = CARTESIAN_POINT ( 'NONE',  ( 5.654972079148370412, 0.4136758123431219514, 2.079573305287989893 ) ) ;
#203083 = CARTESIAN_POINT ( 'NONE',  ( 1.699704897782030377, -0.6493637136964022227, 1.813892859743936103 ) ) ;
#203082 = CARTESIAN_POINT ( 'NONE',  ( -7.818248136574758256, 12.27303992597924420, 0.000000000000000000 ) ) ;
#203084 = UNCERTAINTY_MEASURE_WITH_UNIT (LENGTH_MEASURE( 1.000000000000000082E-05 ), #160485, 'distance_accuracy_value', 'NONE');
#203085 = DIRECTION ( 'NONE',  ( 0.5994789404140898892, -1.444427003850258927E-16, 0.8003905296791063995 ) ) ;
#203086 = CARTESIAN_POINT ( 'NONE',  ( 6.737161338948785883, -0.09310609838950174855, -1.967343120315911298 ) ) ;
#203087 = CARTESIAN_POINT ( 'NONE',  ( 5.356880090730872013, 6.382686539675070492, 1.082531754730549078 ) ) ;
#203088 = CARTESIAN_POINT ( 'NONE',  ( 5.421662447778366811, 6.277071961296246450, 1.037714289653376198 ) ) ;
#203089 = CARTESIAN_POINT ( 'NONE',  ( -0.7500000000000006661, 10.98958333401613174, -1.299038105676657340 ) ) ;
#203090 = CARTESIAN_POINT ( 'NONE',  ( -4.660252114795309097, 6.460046772059735432, -1.599625672291256295 ) ) ;
#203091 = CARTESIAN_POINT ( 'NONE',  ( 0.4225341819744453664, -2.209939313495157265, 0.2258247597332131984 ) ) ;
#203092 = CARTESIAN_POINT ( 'NONE',  ( 2.995255089933103854, 1.807040913553149997, -1.081249443666182808 ) ) ;
#203093 = CARTESIAN_POINT ( 'NONE',  ( -5.015590482412729756, 4.816220082428420923, 0.000000000000000000 ) ) ;
#203094 = CARTESIAN_POINT ( 'NONE',  ( 5.750629710490689384, 9.860818428881154674, -0.7998128361456291469 ) ) ;
#203095 = CARTESIAN_POINT ( 'NONE',  ( 0.8361097980106885208, -1.038377568841988063, 1.544222109484013172 ) ) ;
#203096 = CARTESIAN_POINT ( 'NONE',  ( 6.368579470117202490, 8.453095353268645695, 1.599625672291281386 ) ) ;
#203097 = CARTESIAN_POINT ( 'NONE',  ( 4.985647801523278133, 6.839675073242382553, -1.599625672291256295 ) ) ;
#203098 = CARTESIAN_POINT ( 'NONE',  ( -6.238160076063538284, 9.331584951165851294, 1.082531754730549967 ) ) ;
#203099 = CARTESIAN_POINT ( 'NONE',  ( -7.348156068926747331, 11.51667314714914347, 0.7216878364870458196 ) ) ;
#203100 = CARTESIAN_POINT ( 'NONE',  ( 1.178162429063234207, 2.088287186665960693, -0.3679680078583212333 ) ) ;
#203101 = CARTESIAN_POINT ( 'NONE',  ( -7.584860592202423035, 7.813701877183096833, -0.7998128361456362523 ) ) ;
#203103 = CARTESIAN_POINT ( 'NONE',  ( 3.314850587115983238, -1.487306837207631238, 1.279512770686676681 ) ) ;
#203102 = CARTESIAN_POINT ( 'NONE',  ( -0.6125000000000089262, 0.7083333333333317050, -1.060881119635948444 ) ) ;
#203104 = CARTESIAN_POINT ( 'NONE',  ( 1.885829143180400624, 1.490600019384461072, 1.565824011241300440 ) ) ;
#203105 = CARTESIAN_POINT ( 'NONE',  ( 1.259045258496578557, 1.813921241667546758, -0.3151448728593714277 ) ) ;
#203107 = CARTESIAN_POINT ( 'NONE',  ( -5.343048727742272241, 6.363526295613923800, -1.106837213068444292 ) ) ;
#203106 = CARTESIAN_POINT ( 'NONE',  ( -4.442231607132987925, 5.211633625523774960, -1.199719254218453823 ) ) ;
#203108 = ADVANCED_FACE ( 'NONE', ( #133304 ), #37333, .T. ) ;
#203109 = CARTESIAN_POINT ( 'NONE',  ( 3.995860056160570384, -0.5486252962480555606, -1.651658045138884257 ) ) ;
#203110 = FACE_OUTER_BOUND ( 'NONE', #166879, .T. ) ;
#203111 = CARTESIAN_POINT ( 'NONE',  ( 5.992340707560160240, 7.053780915984068756, 1.082531754730558626 ) ) ;
#203112 = CARTESIAN_POINT ( 'NONE',  ( -10.84558554699185784, 5.653278704827924273, 6.476092148523931336 ) ) ;
#203113 = CARTESIAN_POINT ( 'NONE',  ( 9.368847842243145152, 10.88907622316056312, 1.199719254218453823 ) ) ;
#203114 = AXIS2_PLACEMENT_3D ( 'NONE', #190606, #27041, #61692 ) ;
#203115 = CARTESIAN_POINT ( 'NONE',  ( 0.5675189469334164238, 0.2105291993744831114, -2.151437729447757796 ) ) ;
#203116 = ADVANCED_FACE ( 'NONE', ( #212366 ), #113902, .T. ) ;
#203117 = CARTESIAN_POINT ( 'NONE',  ( 3.391953724946984661, 0.04666865176591524639, 2.015725201127672506 ) ) ;
#203118 = CARTESIAN_POINT ( 'NONE',  ( -10.42585693878457853, 11.26584730477792284, -0.7216878364870267237 ) ) ;
#203119 = CARTESIAN_POINT ( 'NONE',  ( -5.008811405605897882, 4.808311159487113073, 0.7998128361456281477 ) ) ;
#203120 = CARTESIAN_POINT ( 'NONE',  ( 3.643400374902918681, -1.492087795311855425, -1.288628176122036839 ) ) ;
#203121 = CARTESIAN_POINT ( 'NONE',  ( 6.509000000000037645, 2.054060622569788386, 2.307050226316338382 ) ) ;
#203122 = CARTESIAN_POINT ( 'NONE',  ( 2.647912457843327960, 0.6564901929842799078, 1.827849683178353057 ) ) ;
#203125 = ORIENTED_EDGE ( 'NONE', *, *, #165463, .T. ) ;
#203124 = CARTESIAN_POINT ( 'NONE',  ( -4.177320726786315497, 7.887641591310407208, -0.7216878364870458196 ) ) ;
#203123 = CARTESIAN_POINT ( 'NONE',  ( 10.97011102005664185, 11.29999999999997939, 1.696376167609456198 ) ) ;
#203126 = AXIS2_PLACEMENT_3D ( 'NONE', #55229, #75741, #189489 ) ;
#203127 = CARTESIAN_POINT ( 'NONE',  ( -6.089020385868876062, 6.276481003034692030, -0.7216878364870338292 ) ) ;
#203128 = CARTESIAN_POINT ( 'NONE',  ( -0.2106854629475425067, 4.089057744811007922, -2.552070079120628776 ) ) ;
#203129 = CARTESIAN_POINT ( 'NONE',  ( 4.224247379109608680, 7.085983154673295203, -1.199719254218452047 ) ) ;
#203130 = EDGE_CURVE ( 'NONE', #40830, #96770, #71470, .T. ) ;
#203131 = CARTESIAN_POINT ( 'NONE',  ( -4.457598643843001973, 8.422558527783969851, 0.000000000000000000 ) ) ;
#203132 = CARTESIAN_POINT ( 'NONE',  ( -5.420227550413282636, 9.545625585449309725, 0.7998128361456291469 ) ) ;
#203133 = CARTESIAN_POINT ( 'NONE',  ( -6.615342224808818727, 6.750480251133849308, 0.3470571717737805373 ) ) ;
#203134 = CARTESIAN_POINT ( 'NONE',  ( 0.2005908178989434243, -2.206344910233990486, -0.05143828380192031619 ) ) ;
#203135 = DIRECTION ( 'NONE',  ( -0.7927788072572178324, 0.000000000000000000, 0.6095094443598253475 ) ) ;
#203136 = CARTESIAN_POINT ( 'NONE',  ( 4.539869136473917877, 1.278287603951251183, 1.488235606430035274 ) ) ;
#203137 = CARTESIAN_POINT ( 'NONE',  ( 6.934105498385400246, 10.17720795050327354, -1.199719254218441611 ) ) ;
#203138 = CARTESIAN_POINT ( 'NONE',  ( 2.074842474778653578, -0.8596299393073092432, 1.824119475507138821 ) ) ;
#203139 = ORIENTED_EDGE ( 'NONE', *, *, #130231, .T. ) ;
#203140 = CARTESIAN_POINT ( 'NONE',  ( 2.290374991995058895, -0.8151648431981967091, -1.954327666539334762 ) ) ;
#203141 = CARTESIAN_POINT ( 'NONE',  ( 0.7499999999999902300, 1.514583334016148086, 1.299038105676657340 ) ) ;
#203143 = CARTESIAN_POINT ( 'NONE',  ( -4.218558352146454915, 8.073401844146177453, 1.040834085586084257E-14 ) ) ;
#203142 = CARTESIAN_POINT ( 'NONE',  ( -3.379006598303881059, 4.965260336153046516, -1.599625672291256295 ) ) ;
#203144 = CARTESIAN_POINT ( 'NONE',  ( 3.116968920156853340, -1.774181764490849744, 0.4917334186493869108 ) ) ;
#203145 = ORIENTED_EDGE ( 'NONE', *, *, #204483, .F. ) ;
#203146 = CARTESIAN_POINT ( 'NONE',  ( -8.622095623286845978, 12.14652976288826913, 1.199719254218462483 ) ) ;
#203147 = CARTESIAN_POINT ( 'NONE',  ( 0.000000000000000000, 11.37999999999999901, 0.000000000000000000 ) ) ;
#203148 = CARTESIAN_POINT ( 'NONE',  ( 4.113620189327307664, 1.705085180707970771, 1.260635662952174663 ) ) ;
#203149 = CARTESIAN_POINT ( 'NONE',  ( -0.7499999999999972244, 5.639583334016151639, -1.299038105676652899 ) ) ;
#203150 = CARTESIAN_POINT ( 'NONE',  ( 5.587931867126699537, 9.671004278289832001, -0.7998128361456291469 ) ) ;
#203151 = CARTESIAN_POINT ( 'NONE',  ( 4.569639033146696505, 1.999850647628642175, -0.4969485059727016263 ) ) ;
#203153 = CARTESIAN_POINT ( 'NONE',  ( 2.138008341990283778, 0.4048980806483238326, 1.796005048712509655 ) ) ;
#203152 = CARTESIAN_POINT ( 'NONE',  ( -6.015013705957189316, 10.16926642359206134, 0.7998128361456481317 ) ) ;
#203154 = CARTESIAN_POINT ( 'NONE',  ( 7.248805684800777804, 11.60869039890961218, 1.040834085586084257E-14 ) ) ;
#203155 = CARTESIAN_POINT ( 'NONE',  ( 6.039269195634717313, 6.063090950291412540, -0.5025354473536098876 ) ) ;
#203156 = CARTESIAN_POINT ( 'NONE',  ( 0.4170821662628915183, 3.033599471985643170, 0.4170821662628724225 ) ) ;
#203157 =( NAMED_UNIT ( * ) SI_UNIT ( $, .STERADIAN. ) SOLID_ANGLE_UNIT ( ) );
#203158 = CARTESIAN_POINT ( 'NONE',  ( 0.000000000000000000, 0.5999999999999998668, 0.000000000000000000 ) ) ;
#203159 = CARTESIAN_POINT ( 'NONE',  ( 2.174722684859807575, -1.356406721008751814, 1.740749382485320407 ) ) ;
#203160 = CARTESIAN_POINT ( 'NONE',  ( 3.216390312923810502, -1.112095606969863759, -1.970117241612897363 ) ) ;
#203161 = CARTESIAN_POINT ( 'NONE',  ( -6.236387472606141458, 10.21960978477508952, -0.7216878364870278340 ) ) ;
#203162 = CARTESIAN_POINT ( 'NONE',  ( 4.043061577595566725, 0.09493798274137112136, 1.809245059475625750 ) ) ;
#203163 = CARTESIAN_POINT ( 'NONE',  ( 3.889770295363860431, -1.910208526776317806, 0.1464741861031873538 ) ) ;
#203164 = CARTESIAN_POINT ( 'NONE',  ( 5.652806998763869828, -0.4994405740583847675, -2.009109930559597856 ) ) ;
#203165 = CARTESIAN_POINT ( 'NONE',  ( 0.6823417656249917140, 4.155208333674755394, 1.181850606188765695 ) ) ;
#203166 = CARTESIAN_POINT ( 'NONE',  ( 3.555508008102294060, 0.4801912113073670829, -1.911968381370426684 ) ) ;
#203167 = CARTESIAN_POINT ( 'NONE',  ( 1.131717742382963632, -1.219707097817297692, -1.491085513105432581 ) ) ;
#203168 = CARTESIAN_POINT ( 'NONE',  ( 3.696050037196423332, -1.868490534004090931, -0.09263902202472777681 ) ) ;
#203169 = CARTESIAN_POINT ( 'NONE',  ( 3.088805445243738568, -2.273621702497233166, -0.3942619731671925254 ) ) ;
#203170 = CARTESIAN_POINT ( 'NONE',  ( 4.721077684499490168, -1.662108436276054091, -0.8373904101051653504 ) ) ;
#203171 = CARTESIAN_POINT ( 'NONE',  ( -1.378881877344243945, 4.087185210397143109, 0.5904953584335903560 ) ) ;
#203172 = CARTESIAN_POINT ( 'NONE',  ( 6.511381374296898450, -8.144978210217303172, 6.953912913643685023 ) ) ;
#203173 = CARTESIAN_POINT ( 'NONE',  ( 1.717544045074904213, -0.2563126921724939167, 2.090340884163774948 ) ) ;
#203174 = EDGE_CURVE ( 'NONE', #139889, #210054, #48833, .T. ) ;
#203175 = CARTESIAN_POINT ( 'NONE',  ( 3.999292125906911188, 4.728557570721922509, 1.082531754730560403 ) ) ;
#203177 = CARTESIAN_POINT ( 'NONE',  ( -9.561524646135538319, 12.17819805862340310, -1.599625672291263179 ) ) ;
#203176 = FACE_OUTER_BOUND ( 'NONE', #110913, .T. ) ;
#203178 = CARTESIAN_POINT ( 'NONE',  ( 7.015401035077362124, 6.062865449010540253, -2.437084766375293476 ) ) ;
#203179 = CARTESIAN_POINT ( 'NONE',  ( 0.6506561817731060238, 1.990614601344290691, 0.3409984238087642727 ) ) ;
#203180 = CARTESIAN_POINT ( 'NONE',  ( 1.364683531249986537, 0.8635416670080893198, 0.7879004041258500513 ) ) ;
#203181 = CARTESIAN_POINT ( 'NONE',  ( -4.799223189557577207, 4.701441264013013210, 0.7216878364870317197 ) ) ;
#203182 = EDGE_CURVE ( 'NONE', #62943, #95548, #185446, .T. ) ;
#203183 = CARTESIAN_POINT ( 'NONE',  ( 5.335297142177534369, 6.183267073083954735, -1.199719254218452047 ) ) ;
#203184 = ORIENTED_EDGE ( 'NONE', *, *, #44491, .T. ) ;
#203185 = CARTESIAN_POINT ( 'NONE',  ( 1.616726252867954683, 1.452999108549270169, -1.600537328674697779 ) ) ;
#203186 = CARTESIAN_POINT ( 'NONE',  ( 6.610000000000001208, 3.709748940453510446, 2.234587373521100151 ) ) ;
#203189 = CARTESIAN_POINT ( 'NONE',  ( 6.938893903907228378E-15, 10.64264068711930733, 1.214306433183764966E-14 ) ) ;
#203188 = CARTESIAN_POINT ( 'NONE',  ( 6.825078400183584471, 2.055285645424239416, 2.261848697290469445 ) ) ;
#203187 = CARTESIAN_POINT ( 'NONE',  ( 5.845500506147374153, 6.848780674373954547, 1.199719254218453823 ) ) ;
#203190 = DIRECTION ( 'NONE',  ( 0.000000000000000000, 1.000000000000000000, 0.000000000000000000 ) ) ;
#203191 = CARTESIAN_POINT ( 'NONE',  ( 5.594935472981866553, 1.780666063871166882, 0.9463038388278843804 ) ) ;
#203192 = CARTESIAN_POINT ( 'NONE',  ( -8.839552966430012759, 10.37552855133225904, -1.082531754730543971 ) ) ;
#203193 = CARTESIAN_POINT ( 'NONE',  ( 6.427293192253748622, -1.366186911818557226, -1.582700853868714397 ) ) ;
#203194 = DIRECTION ( 'NONE',  ( -0.000000000000000000, 1.000000000000000000, -0.000000000000000000 ) ) ;
#203196 = CARTESIAN_POINT ( 'NONE',  ( -0.6823417656250003738, 11.65104166700806765, 1.181850606188754593 ) ) ;
#203195 = CARTESIAN_POINT ( 'NONE',  ( 0.6732104281652334654, -2.131434628316424273, -0.7592435237872022791 ) ) ;
#203197 = CARTESIAN_POINT ( 'NONE',  ( -7.458957065812611198, 11.85386701009007204, 0.7998128361456481317 ) ) ;
#203198 = CARTESIAN_POINT ( 'NONE',  ( -4.080641047588902559, 7.704572288921609058, -0.7216878364870257245 ) ) ;
#203199 = CARTESIAN_POINT ( 'NONE',  ( 1.364683531249988535, 2.676041667008082214, 0.7879004041258500513 ) ) ;
#203200 = CARTESIAN_POINT ( 'NONE',  ( -0.7500000000000215383, 4.441666666666691299, 1.299038105676671107 ) ) ;
#203201 = CARTESIAN_POINT ( 'NONE',  ( -1.500000000000001110, 10.27083333333332860, 0.8660254037844419273 ) ) ;
#203202 = CARTESIAN_POINT ( 'NONE',  ( 2.508071618744921238, -0.6595455166902574051, -1.594007932167235131 ) ) ;
#203203 = CARTESIAN_POINT ( 'NONE',  ( 3.718679271898170491, 7.560485927181699317, 0.7998128361456271485 ) ) ;
#203204 = CARTESIAN_POINT ( 'NONE',  ( 2.389615768203833479, -0.7611923103308501082, 1.597832513397597021 ) ) ;
#203205 = CARTESIAN_POINT ( 'NONE',  ( 2.649090073008007362, 0.2487567141898557876, 1.997615136964459470 ) ) ;
#203206 = CARTESIAN_POINT ( 'NONE',  ( 5.315527377757141458, -0.3284926246858720922, 2.182075488366498117 ) ) ;
#203207 = ORIENTED_EDGE ( 'NONE', *, *, #204467, .F. ) ;
#203208 = CARTESIAN_POINT ( 'NONE',  ( 4.447524238883529435, -1.845004865869297905, 0.8223427699834483517 ) ) ;
#203209 = CARTESIAN_POINT ( 'NONE',  ( -7.584860592202423035, 7.813701877183096833, -0.7998128361456362523 ) ) ;
#203211 = CARTESIAN_POINT ( 'NONE',  ( 4.499625164952708367, -1.976952908697379607, 0.3961224619316304763 ) ) ;
#203210 = CARTESIAN_POINT ( 'NONE',  ( 4.477262591527907176, -1.894555094343739476, -0.9525379817736513433 ) ) ;
#203213 = ORIENTED_EDGE ( 'NONE', *, *, #73284, .F. ) ;
#203212 = CARTESIAN_POINT ( 'NONE',  ( 4.078215212670958323, 0.8593412415473808963, 1.594818892651229891 ) ) ;
#203214 = B_SPLINE_CURVE_WITH_KNOTS ( 'NONE', 3,
 ( #57587, #123744, #105286, #189705 ),
 .UNSPECIFIED., .F., .F.,
 ( 4, 4 ),
 ( 1.890032774489904948E-16, 0.0001045641765545081658 ),
 .UNSPECIFIED. ) ;
#203215 = CARTESIAN_POINT ( 'NONE',  ( 6.398522151006641678, 6.429640362454684954, 0.000000000000000000 ) ) ;
#203216 = EDGE_LOOP ( 'NONE', ( #26246, #65775, #52027, #110073, #46640, #183241, #86888, #80491, #37719, #196079, #206975, #4991, #50430, #73189, #69785, #180581, #4299, #54122, #185676, #118687, #105133 ) ) ;
#203217 = CARTESIAN_POINT ( 'NONE',  ( 1.234984068473435670, -1.692697435815498919, 0.7966027930108382504 ) ) ;
#203218 = DIRECTION ( 'NONE',  ( -1.276756478318932585E-15, 1.000000000000000000, -1.665334536937738262E-16 ) ) ;
#203219 = CARTESIAN_POINT ( 'NONE',  ( 5.654893700716965732, 0.3597771647365927694, 1.775199357419085411 ) ) ;
#203220 = DIRECTION ( 'NONE',  ( -0.7592566023653004592, 0.6507913734559639396, 0.000000000000000000 ) ) ;
#203221 = VECTOR ( 'NONE', #151313, 1000.000000000000000 ) ;
#203222 = CARTESIAN_POINT ( 'NONE',  ( -11.25771003949915539, 3.534410846742664702, -5.930344140359695260 ) ) ;
#203223 = SURFACE_STYLE_FILL_AREA ( #52722 ) ;
#203224 = CARTESIAN_POINT ( 'NONE',  ( -1.364683531250012516, 2.842708333674754506, 0.7879004041258379498 ) ) ;
#203225 = CARTESIAN_POINT ( 'NONE',  ( 0.3164790345465406385, -0.6463921985436007489, -1.799943259716822341 ) ) ;
#203226 = CARTESIAN_POINT ( 'NONE',  ( 7.702440666339465558, 8.158804663583751449, -0.7216878364870317197 ) ) ;
#203227 = CARTESIAN_POINT ( 'NONE',  ( 2.260140581184489239, -1.961506502764579052, 0.04509734162668613960 ) ) ;
#203228 = CARTESIAN_POINT ( 'NONE',  ( -3.038435823238377687, 6.558942537171132514, -0.7216878364870458196 ) ) ;
#203229 = CARTESIAN_POINT ( 'NONE',  ( -4.936050443827081580, 7.916420063510339666, 1.199719254218452935 ) ) ;
#203230 = CARTESIAN_POINT ( 'NONE',  ( 4.271814301144261528, 0.4616217191124799002, -2.069597271375968273 ) ) ;
#203232 = CARTESIAN_POINT ( 'NONE',  ( -10.47476631618627252, 5.237304525980054137, 5.169966676860812349 ) ) ;
#203231 = CARTESIAN_POINT ( 'NONE',  ( -0.02968770228137588424, 4.095675376368371090, -2.381331788581673159 ) ) ;
#203233 = CARTESIAN_POINT ( 'NONE',  ( 5.325445421541009416, -1.872857986210634484, 0.6156230612282005410 ) ) ;
#203234 = CARTESIAN_POINT ( 'NONE',  ( -0.6823417656250212460, 1.551041667008083769, 1.181850606188755259 ) ) ;
#203235 = CARTESIAN_POINT ( 'NONE',  ( 1.230727935554910557, 1.348888731755660153, -1.494678444409401896 ) ) ;
#203236 = ORIENTED_EDGE ( 'NONE', *, *, #42629, .T. ) ;
#203237 = CARTESIAN_POINT ( 'NONE',  ( 1.529080078018136390, -1.786526079506415288, 1.135962973836294854 ) ) ;
#203238 = CARTESIAN_POINT ( 'NONE',  ( 11.35349642860619390, 7.539003845593507336, 3.753059129874396493 ) ) ;
#203239 = CARTESIAN_POINT ( 'NONE',  ( 2.242711981562468093, -2.029969483702593003, -0.4061203719310027549 ) ) ;
#203240 = CARTESIAN_POINT ( 'NONE',  ( 5.252858170651868441, 5.093032385374103299, -0.7998128361456481317 ) ) ;
#203241 = CARTESIAN_POINT ( 'NONE',  ( 6.222266154028957885, 6.224008365980749247, 0.7998128361456352531 ) ) ;
#203242 = ORIENTED_EDGE ( 'NONE', *, *, #183755, .F. ) ;
#203244 = CARTESIAN_POINT ( 'NONE',  ( 3.669453130792974971, 7.432779085900453886, 1.040834085586084257E-14 ) ) ;
#203243 = CARTESIAN_POINT ( 'NONE',  ( 4.277343952648727132, 1.365583793738689655, 1.583094835029410063 ) ) ;
#203247 = ORIENTED_EDGE ( 'NONE', *, *, #86107, .T. ) ;
#203246 = CARTESIAN_POINT ( 'NONE',  ( 1.646807439477548707, 0.1776336960073976179, 1.802747333403993402 ) ) ;
#203245 = CARTESIAN_POINT ( 'NONE',  ( 2.924607851032960504, 1.718362407962298333, 0.6167639819729958672 ) ) ;
#203248 = CARTESIAN_POINT ( 'NONE',  ( 6.322910218073367616, 2.057572540570989261, 0.7984293639632376038 ) ) ;
#203249 = CARTESIAN_POINT ( 'NONE',  ( 3.686212053427321056, 6.121915856213854923, 1.284222742053100941 ) ) ;
#203250 = CARTESIAN_POINT ( 'NONE',  ( 3.962124768131184638, 2.190450126196175074, -0.2673064950309556043 ) ) ;
#203251 = CARTESIAN_POINT ( 'NONE',  ( 6.286176778230493589, 10.48562334124426698, 0.7998128361456462443 ) ) ;
#203252 = CARTESIAN_POINT ( 'NONE',  ( 1.364683531249997417, 9.046875000341403350, 2.602085213965210642E-15 ) ) ;
#203253 = CARTESIAN_POINT ( 'NONE',  ( 2.877492880751183257, 0.2784179829431778219, -1.891769048003589138 ) ) ;
#203255 = CARTESIAN_POINT ( 'NONE',  ( -4.946027110887008860, 4.664786472323266153, -0.7998128361456221525 ) ) ;
#203254 = VECTOR ( 'NONE', #192733, 1000.000000000000000 ) ;
#203256 = CARTESIAN_POINT ( 'NONE',  ( 9.257519960032755790, 9.694861462993381807, 0.7998128361456462443 ) ) ;
#203257 = CARTESIAN_POINT ( 'NONE',  ( 6.478973898625433492, 1.930320082341809629, 0.7489585856828018251 ) ) ;
#203258 = CARTESIAN_POINT ( 'NONE',  ( -0.4019237886466871523, 10.22991455036742714, -1.499999999999998668 ) ) ;
#203259 = CARTESIAN_POINT ( 'NONE',  ( 5.864808805604324604, 0.1626094438406736342, -2.185560445749204828 ) ) ;
#203260 = CARTESIAN_POINT ( 'NONE',  ( 5.561552386509557522, 7.525632394756676113, -1.337405013919689800 ) ) ;
#203261 = CARTESIAN_POINT ( 'NONE',  ( -9.333041836229160282, 15.44694763439141205, -7.472413793097630652 ) ) ;
#203262 = COLOUR_RGB ( '', 0.09019608, 0.27058824, 0.51372549) ;
#203263 = CARTESIAN_POINT ( 'NONE',  ( 11.40591166468351503, 3.507114751586604129, -3.706005353348470255 ) ) ;
#203264 = CARTESIAN_POINT ( 'NONE',  ( 3.637841704585748293, 0.8437669887123750989, -1.669527271503386201 ) ) ;
#203265 = DIRECTION ( 'NONE',  ( 0.000000000000000000, 7.228014483236694583E-17, -1.000000000000000000 ) ) ;
#203266 = DIRECTION ( 'NONE',  ( 1.000000000000000000, 0.000000000000000000, 0.000000000000000000 ) ) ;
#203267 = CARTESIAN_POINT ( 'NONE',  ( -7.754900677336769022, 9.110100880723427608, 1.082531754730558626 ) ) ;
#203268 = CARTESIAN_POINT ( 'NONE',  ( 4.817943484809818600, 6.714296380401858499, 1.599625672291269396 ) ) ;
#203269 = CARTESIAN_POINT ( 'NONE',  ( 6.895378825052528526, -1.852007112603266670, 0.9253362530580526712 ) ) ;
#203270 = CARTESIAN_POINT ( 'NONE',  ( 1.247672978039487734, 1.986097573956084439, -0.3474914183895366215 ) ) ;
#203271 = CARTESIAN_POINT ( 'NONE',  ( -7.621654909176601045, 12.04368116068139472, 0.7998128361456481317 ) ) ;
#203272 = CARTESIAN_POINT ( 'NONE',  ( 8.167861197590044142, 8.493869250135347215, 0.000000000000000000 ) ) ;
#203273 = CARTESIAN_POINT ( 'NONE',  ( 1.552940555598739891, -1.880887156831068552, -1.124362282834884263 ) ) ;
#203274 = CARTESIAN_POINT ( 'NONE',  ( 6.709597972018079837, -0.3944863986210072060, 1.789098616620278470 ) ) ;
#203275 = CARTESIAN_POINT ( 'NONE',  ( -2.785310492603665367, 5.336947110424484109, 1.199719254218462483 ) ) ;
#203276 = ADVANCED_FACE ( 'NONE', ( #66099 ), #61608, .T. ) ;
#203277 = CARTESIAN_POINT ( 'NONE',  ( 5.072158865288222351, 8.931619419562697004, 0.7216878364870317197 ) ) ;
#203278 = CARTESIAN_POINT ( 'NONE',  ( 9.398826802771546696, 11.98838390803207865, -1.599625672291262513 ) ) ;
#203279 = CARTESIAN_POINT ( 'NONE',  ( 2.693266070609028784, 6.293894182352508970, 0.000000000000000000 ) ) ;
#203280 = CARTESIAN_POINT ( 'NONE',  ( 3.067887898442204442, 6.801229324816399746, 0.7998128361456271485 ) ) ;
#203281 = EDGE_LOOP ( 'NONE', ( #101870, #177071, #145248, #79202 ) ) ;
#203283 = CARTESIAN_POINT ( 'NONE',  ( 0.9967404297962767501, -1.964529542677856622, -0.4388597091333420463 ) ) ;
#203282 = CARTESIAN_POINT ( 'NONE',  ( 3.860763913883006992, 0.2215400755124704024, -1.827792592973469743 ) ) ;
#203284 = CARTESIAN_POINT ( 'NONE',  ( 2.407932310410058285, 0.5022953597978959683, 2.242707597164790734 ) ) ;
#203286 = CARTESIAN_POINT ( 'NONE',  ( 0.2680791809135505410, -0.7890318081985218113, -1.684091100025336463 ) ) ;
#203285 = CARTESIAN_POINT ( 'NONE',  ( 4.704316114261903436, 4.590716342834741504, 1.214306433183764966E-14 ) ) ;
#203287 = CARTESIAN_POINT ( 'NONE',  ( -5.416646063859567484, 6.278174148379618735, 1.199719254218450271 ) ) ;
#203288 = CARTESIAN_POINT ( 'NONE',  ( 3.929058411375439874, -1.000000000000000888, 0.7500000000000006661 ) ) ;
#203289 = CARTESIAN_POINT ( 'NONE',  ( 3.797043250571481732, -0.1924442655423033721, -1.902711443722324258 ) ) ;
#203290 = CARTESIAN_POINT ( 'NONE',  ( -10.29471871147821282, 10.90492667301307605, -0.7998128361456291469 ) ) ;
#203291 = CARTESIAN_POINT ( 'NONE',  ( 6.423677080210483226, 6.791898735554919853, -0.4454198846488600649 ) ) ;
#203292 = CARTESIAN_POINT ( 'NONE',  ( -3.311934663488232733, 7.085950550703385531, -0.7998128361456481317 ) ) ;
#203294 = CARTESIAN_POINT ( 'NONE',  ( 0.8658264364783776479, 0.9185255527898968930, 1.629538061279064642 ) ) ;
#203293 = CARTESIAN_POINT ( 'NONE',  ( 2.384421550557855429, -0.3601958963256215451, -2.059324561056875336 ) ) ;
#203295 = CARTESIAN_POINT ( 'NONE',  ( 2.460314346279086628, 1.556669099887195484, 1.281166478716524670 ) ) ;
#203296 = CARTESIAN_POINT ( 'NONE',  ( 7.727784370109387346, 10.99920361756089093, -1.082531754730543083 ) ) ;
#203297 = CARTESIAN_POINT ( 'NONE',  ( 1.364683531249988535, 4.217708333674753618, -0.7879004041258239610 ) ) ;
#203298 = CARTESIAN_POINT ( 'NONE',  ( 3.684860642351639903, 1.263529365103865709, 1.197186439443503003 ) ) ;
#203299 = CARTESIAN_POINT ( 'NONE',  ( 3.323720213644492993, 7.029424015893889433, 1.040834085586084257E-14 ) ) ;
#203300 = CARTESIAN_POINT ( 'NONE',  ( 11.89942855770814312, 13.79999999999999893, -0.7000000000000009548 ) ) ;
#203301 = CARTESIAN_POINT ( 'NONE',  ( 4.336358584672225902, 1.692218828317056278, 0.3330917469099390904 ) ) ;
#203302 = CARTESIAN_POINT ( 'NONE',  ( 3.368858348882136422, 0.05182064297618373117, -2.191103300807801801 ) ) ;
#203303 = CARTESIAN_POINT ( 'NONE',  ( 5.953802724510455668, 0.6443607167232848765, -2.110727517106169682 ) ) ;
#203304 = CARTESIAN_POINT ( 'NONE',  ( -10.41986968326957808, 5.020773655391575829, -5.279272669861445166 ) ) ;
#203305 = CARTESIAN_POINT ( 'NONE',  ( 3.784171691162826701, -1.288926714175726129, -1.746948845794197958 ) ) ;
#203306 = CARTESIAN_POINT ( 'NONE',  ( 2.719161800852238464, -0.1789327596440904167, 1.816892639718168390 ) ) ;
#203307 = CARTESIAN_POINT ( 'NONE',  ( 1.499999999999996891, 12.39583333333333037, -0.8660254037844378194 ) ) ;
#203308 = CARTESIAN_POINT ( 'NONE',  ( 4.891875743818586919, -2.106850654347144580, 0.2108507618673941542 ) ) ;
#203309 = CARTESIAN_POINT ( 'NONE',  ( -1.500000000000001110, 9.802083334016129967, 0.8660254037844418162 ) ) ;
#203310 = ORIENTED_EDGE ( 'NONE', *, *, #205165, .F. ) ;
#203312 = CARTESIAN_POINT ( 'NONE',  ( 1.364683531249986537, 2.217708333674751398, -0.7879004041258239610 ) ) ;
#203311 = CARTESIAN_POINT ( 'NONE',  ( 4.757543194620796889, 2.267657608012829673, -0.3350592807548398722 ) ) ;
#203313 = CARTESIAN_POINT ( 'NONE',  ( -1.115562610750309283E-14, 8.343750000682796042, 1.500000000000001554 ) ) ;
#203314 = CARTESIAN_POINT ( 'NONE',  ( 10.22692794340986921, 10.82583744360002243, 0.000000000000000000 ) ) ;
#203315 = CARTESIAN_POINT ( 'NONE',  ( 0.5223349339509277822, -2.109880975928311031, 0.2119513895993754005 ) ) ;
#203316 = CARTESIAN_POINT ( 'NONE',  ( -5.422898255786198440, 7.349800603215774331, -1.443375672974052559 ) ) ;
#203317 = ADVANCED_FACE ( 'NONE', ( #165775 ), #85892, .T. ) ;
#203318 = CARTESIAN_POINT ( 'NONE',  ( -4.731432421044873493, 7.503459676985569260, -1.082531754730548412 ) ) ;
#203319 = CARTESIAN_POINT ( 'NONE',  ( 6.883263157960381129, 0.5832772681763243039, 2.006853359411898463 ) ) ;
#203320 = ORIENTED_EDGE ( 'NONE', *, *, #163044, .F. ) ;
#203321 = CARTESIAN_POINT ( 'NONE',  ( 5.080704010962952211, -0.7231418808758652839, 1.882473355234378865 ) ) ;
#203323 = CARTESIAN_POINT ( 'NONE',  ( 3.116140835343351956, 2.053043485406472080, -0.1977005638095686579 ) ) ;
#203322 = CARTESIAN_POINT ( 'NONE',  ( 5.281064527722868718, 6.119995689553514140, 1.199719254218462483 ) ) ;
#203324 = CARTESIAN_POINT ( 'NONE',  ( 6.855582950365507244, 8.027210192628430718, -1.199719254218452047 ) ) ;
#203325 = CARTESIAN_POINT ( 'NONE',  ( 7.049313524462606395, 7.188896964819984525, 0.000000000000000000 ) ) ;
#203326 = CARTESIAN_POINT ( 'NONE',  ( 0.000000000000000000, -1.946874999522044014, -3.793834371823813001 ) ) ;
#203327 = CARTESIAN_POINT ( 'NONE',  ( 6.105464321129510097, -2.175355461714892691, 0.2646407054325700670 ) ) ;
#203328 = CARTESIAN_POINT ( 'NONE',  ( 4.922500090287251773, -1.427935867408920645, -1.423962988533589158 ) ) ;
#203329 = CARTESIAN_POINT ( 'NONE',  ( 3.772867777003403589, 1.732451475078290448, -0.6238847238279123797 ) ) ;
#203330 = CARTESIAN_POINT ( 'NONE',  ( 4.320244504248938355, 8.192035688265757898, 1.040834085586084257E-14 ) ) ;
#203331 =( NAMED_UNIT ( * ) SI_UNIT ( $, .STERADIAN. ) SOLID_ANGLE_UNIT ( ) );
#203332 = CARTESIAN_POINT ( 'NONE',  ( 0.8501349688851227437, 0.4944664728778884744, 1.652377535151504206 ) ) ;
#203333 = FACE_OUTER_BOUND ( 'NONE', #173738, .T. ) ;
#203334 = CARTESIAN_POINT ( 'NONE',  ( 0.9502802867703894485, -2.080962668894706269, -0.9767702978288366200 ) ) ;
#203335 = CARTESIAN_POINT ( 'NONE',  ( -5.331380718671772101, 7.243030143248949670, -1.599625672291256295 ) ) ;
#203336 = CARTESIAN_POINT ( 'NONE',  ( 0.6676899448993807162, 0.2205636587761065359, -2.251657551468993379 ) ) ;
#203337 = CARTESIAN_POINT ( 'NONE',  ( 3.334694542603059642, 2.054772597177223936, 0.4612437286577449891 ) ) ;
#203338 = CARTESIAN_POINT ( 'NONE',  ( -4.339491684825780737, 7.220434844675483355, -1.199719254218455378 ) ) ;
#203339 = CARTESIAN_POINT ( 'NONE',  ( 6.265839547809997079, 10.46189657242035587, 0.7998128361456462443 ) ) ;
#203340 = CARTESIAN_POINT ( 'NONE',  ( 6.224601922005513543, 7.395028676162137771, -1.082531754730548412 ) ) ;
#203341 = CARTESIAN_POINT ( 'NONE',  ( 6.250000000000084377, 2.349784478886278158E-12, 2.052068128417940063 ) ) ;
#203342 = CARTESIAN_POINT ( 'NONE',  ( -5.052384799386910430, 9.046199365926717917, 1.214306433183764966E-14 ) ) ;
#203343 = ADVANCED_FACE ( 'NONE', ( #89873 ), #130204, .T. ) ;
#203344 = CARTESIAN_POINT ( 'NONE',  ( 5.775410249297131315, 9.681803024247919609, 1.040834085586084257E-14 ) ) ;
#203345 = CARTESIAN_POINT ( 'NONE',  ( 4.849937260509308956, 6.926242028416789154, 1.417063245053858722 ) ) ;
#203346 = CARTESIAN_POINT ( 'NONE',  ( -4.517891501851816649, 6.293959390292322986, -1.599625672291256295 ) ) ;
#203347 = CARTESIAN_POINT ( 'NONE',  ( 4.517978939158282969, -0.5908935252547321548, 2.141346583060988351 ) ) ;
#203348 = CARTESIAN_POINT ( 'NONE',  ( 2.695491272475036837, -0.6865090956127660737, 2.081212476921667776 ) ) ;
#203350 = EDGE_CURVE ( 'NONE', #48473, #144017, #186069, .T. ) ;
#203349 = CARTESIAN_POINT ( 'NONE',  ( -5.215082642750900277, 9.236013516518044142, 0.000000000000000000 ) ) ;
#203351 = CARTESIAN_POINT ( 'NONE',  ( -3.474632506852224356, 7.275764701294714420, -0.7998128361456481317 ) ) ;
#203352 = CARTESIAN_POINT ( 'NONE',  ( 5.230891786122516152, -1.846674803186045821, -0.6626716404555529349 ) ) ;
#203353 = CARTESIAN_POINT ( 'NONE',  ( -0.6823417656250212460, 2.051041667008083991, 1.181850606188767472 ) ) ;
#203354 = CARTESIAN_POINT ( 'NONE',  ( 6.609999999999995879, 0.01081285896096205283, 1.720159828161060833 ) ) ;
#203356 = ORIENTED_EDGE ( 'NONE', *, *, #112616, .T. ) ;
#203355 = CARTESIAN_POINT ( 'NONE',  ( -5.585596099150193616, 6.579245539505756746, -1.082531754730544860 ) ) ;
#203358 = CARTESIAN_POINT ( 'NONE',  ( 4.465154236216789307, -1.701427117168831549, 1.265499569954648962 ) ) ;
#203357 = AXIS2_PLACEMENT_3D ( 'NONE', #46695, #79171, #131192 ) ;
#203359 = CARTESIAN_POINT ( 'NONE',  ( -5.646044625448194410, 5.551749915969804938, 0.000000000000000000 ) ) ;
#203360 = EDGE_LOOP ( 'NONE', ( #28202, #189927, #46405, #185662 ) ) ;
#203361 = CARTESIAN_POINT ( 'NONE',  ( 5.102478102407745908, -0.7247817745383768884, -2.036717088958202471 ) ) ;
#203362 = CARTESIAN_POINT ( 'NONE',  ( 5.656776405399742025, 7.622658444431597680, -1.599625672291262513 ) ) ;
#203363 = CARTESIAN_POINT ( 'NONE',  ( 5.478019777291557979, -1.797689181224306321, -0.3974485807837144224 ) ) ;
#203364 = CARTESIAN_POINT ( 'NONE',  ( -5.811497925844209433, 6.060560459143458978, 0.5261113891226586459 ) ) ;
#203365 = CARTESIAN_POINT ( 'NONE',  ( -0.6823417656250212460, 1.863541667008083991, 1.181850606188755259 ) ) ;
#203366 = CARTESIAN_POINT ( 'NONE',  ( 6.404260164931634414, 1.284261220195097808, -1.174706115135275342 ) ) ;
#203367 = CARTESIAN_POINT ( 'NONE',  ( -9.499606442108966320, -9.900000000000019895, 0.08647222121522583904 ) ) ;
#203368 = CARTESIAN_POINT ( 'NONE',  ( -0.006800380015319074101, 7.009756401597622144, 1.999988438674507485 ) ) ;
#203369 = CARTESIAN_POINT ( 'NONE',  ( 3.942369626403975147, 2.151062187213080623, 0.2142938780915065733 ) ) ;
#203370 = CARTESIAN_POINT ( 'NONE',  ( -4.436542580169821726, 6.199052314996659874, 1.599625672291267398 ) ) ;
#203371 = CARTESIAN_POINT ( 'NONE',  ( -6.954969613686107444, 10.09758640173367894, 1.082531754730549967 ) ) ;
#203373 = AXIS2_PLACEMENT_3D ( 'NONE', #38700, #156730, #106957 ) ;
#203372 = AXIS2_PLACEMENT_3D ( 'NONE', #105066, #92020, #87724 ) ;
#203374 = CARTESIAN_POINT ( 'NONE',  ( 3.379894511112140787, 1.369989894601089775, 1.672159933133889442 ) ) ;
#203375 = CARTESIAN_POINT ( 'NONE',  ( 4.552002736099131752, 1.970983365533407694, -0.04540313215006633318 ) ) ;
#203376 = CARTESIAN_POINT ( 'NONE',  ( 3.778401656274816389, -1.708383637232064878, 0.2947856008331130040 ) ) ;
#203377 = CARTESIAN_POINT ( 'NONE',  ( 0.9080814035550346386, -0.9900877184637231210, -1.955254813705724404 ) ) ;
#203378 = CARTESIAN_POINT ( 'NONE',  ( 1.729934149615200312, -2.172323606337727142, 0.7788181121253530126 ) ) ;
#203379 = CARTESIAN_POINT ( 'NONE',  ( 3.919256602636957076, -0.1552153454438681413, 2.055015938418188526 ) ) ;
#203380 = CARTESIAN_POINT ( 'NONE',  ( 5.460475975554013317, -1.757383149004720924, -0.8268225932778446863 ) ) ;
#203381 = CARTESIAN_POINT ( 'NONE',  ( -6.521108698048767138, 10.55178454779148289, -0.7216878364870267237 ) ) ;
#203382 = CARTESIAN_POINT ( 'NONE',  ( -6.805266759416629618, 6.904175738932996964, 0.000000000000000000 ) ) ;
#203383 = DIRECTION ( 'NONE',  ( 0.000000000000000000, 1.000000000000000000, 0.000000000000000000 ) ) ;
#203384 = ADVANCED_FACE ( 'NONE', ( #52024 ), #170021, .F. ) ;
#203385 = CARTESIAN_POINT ( 'NONE',  ( -7.497295758232724872, 9.769931022736756177, -1.443375672974058777 ) ) ;
#203386 = CARTESIAN_POINT ( 'NONE',  ( 3.065657736429776126, 0.3252250816505456998, -2.182562984848686938 ) ) ;
#203387 = CARTESIAN_POINT ( 'NONE',  ( 1.001543065824772753E-15, -2.909374999522043925, 3.793834371823811669 ) ) ;
#203388 = ORIENTED_EDGE ( 'NONE', *, *, #19860, .F. ) ;
#203389 = CARTESIAN_POINT ( 'NONE',  ( 0.9361096364171941353, -1.039984170849604039, 1.543015978488631923 ) ) ;
#203390 = CARTESIAN_POINT ( 'NONE',  ( -0.1290005225502675879, -0.006633637972621592160, -2.173875058097324064 ) ) ;
#203391 = DIRECTION ( 'NONE',  ( -0.000000000000000000, 1.000000000000000000, -0.000000000000000000 ) ) ;
#203393 = DIRECTION ( 'NONE',  ( 3.330669073875478989E-16, -3.540251991789410786E-16, -1.000000000000000000 ) ) ;
#203392 = CARTESIAN_POINT ( 'NONE',  ( -6.594145116354495961, 6.771750247812114765, -0.2697605348319087604 ) ) ;
#203394 = CARTESIAN_POINT ( 'NONE',  ( 6.386648935047418263, 1.599332519906123462, -0.9119682274050244786 ) ) ;
#203395 = ORIENTED_EDGE ( 'NONE', *, *, #35195, .T. ) ;
#203396 = CARTESIAN_POINT ( 'NONE',  ( 2.694271958740936945, -2.055289539400024790, -0.1528356987768857700 ) ) ;
#203397 = CARTESIAN_POINT ( 'NONE',  ( 0.6801582343749935644, 0.9739583336747514863, 1.178068619123805227 ) ) ;
#203398 = CARTESIAN_POINT ( 'NONE',  ( -7.206322340863467346, 8.366129804884193888, 1.199719254218450271 ) ) ;
#203399 = FACE_OUTER_BOUND ( 'NONE', #107873, .T. ) ;
#203400 = CARTESIAN_POINT ( 'NONE',  ( 3.334415713957098681, 5.977569868670206787, -1.199719254218446718 ) ) ;
#203401 = CARTESIAN_POINT ( 'NONE',  ( 1.903268112024224523, 1.712809940758196259, 1.145777703309367457 ) ) ;
#203402 = EDGE_CURVE ( 'NONE', #183550, #102475, #92726, .T. ) ;
#203404 = CARTESIAN_POINT ( 'NONE',  ( -1.364683531250000748, 13.85937500034140157, 0.000000000000000000 ) ) ;
#203403 = CARTESIAN_POINT ( 'NONE',  ( 4.893868406069843857, 4.891356491275733909, 0.6526265993265610854 ) ) ;
#203405 = CARTESIAN_POINT ( 'NONE',  ( 7.169564303528210836, 7.258913197071374945, -0.7998128361456281477 ) ) ;
#203406 = STYLED_ITEM ( 'NONE', ( #63680 ), #105592 ) ;
#203407 = DIRECTION ( 'NONE',  ( 0.000000000000000000, -1.000000000000000000, 0.000000000000000000 ) ) ;
#203408 = CARTESIAN_POINT ( 'NONE',  ( 6.076841795016812320, -2.094286673724785164, -0.6961510500591641115 ) ) ;
#203409 = CARTESIAN_POINT ( 'NONE',  ( 6.766858430912646938, -2.064281441484459023, -0.9263300772878214628 ) ) ;
#203410 = CARTESIAN_POINT ( 'NONE',  ( -4.067082894419624672, 6.728385229256075739, 1.082531754730560403 ) ) ;
#203411 = CARTESIAN_POINT ( 'NONE',  ( 6.433875545303581411, -1.754733077360526972, 0.4498553729834730008 ) ) ;
#203412 = CARTESIAN_POINT ( 'NONE',  ( 0.8136858238772455287, -1.282993010278702606, -1.555696519147983459 ) ) ;
#203413 = VECTOR ( 'NONE', #61298, 1000.000000000000000 ) ;
#203414 = CARTESIAN_POINT ( 'NONE',  ( 4.588833619725765978, 8.479441126791286365, 0.4148976642893330014 ) ) ;
#203415 = CARTESIAN_POINT ( 'NONE',  ( -0.1099460098626957039, 6.494484681433106310, 3.110387376256865011 ) ) ;
#203416 = CARTESIAN_POINT ( 'NONE',  ( 2.078771448894382701, -0.08914341469279044028, -1.868647664167771616 ) ) ;
#203417 = CARTESIAN_POINT ( 'NONE',  ( 3.960172920142067898, -1.157100329752266621, 1.651342637023434090 ) ) ;
#203419 = CARTESIAN_POINT ( 'NONE',  ( 2.294141167727915320, 5.518260410454753462, -0.5312303208429024481 ) ) ;
#203418 = CARTESIAN_POINT ( 'NONE',  ( -1.364683531250000748, 0.7593750003414210248, 0.000000000000000000 ) ) ;
#203421 = CARTESIAN_POINT ( 'NONE',  ( 5.408848747418643299, 1.595474064493606514, -1.374861248814135628 ) ) ;
#203420 = CARTESIAN_POINT ( 'NONE',  ( -7.492852449846775897, 11.89341162479659531, 0.000000000000000000 ) ) ;
#203422 = EDGE_CURVE ( 'NONE', #139360, #113025, #136368, .T. ) ;
#203423 = CARTESIAN_POINT ( 'NONE',  ( 7.446452682403650769, 9.710614100936176385, -1.599625672291262513 ) ) ;
#203425 = CARTESIAN_POINT ( 'NONE',  ( -7.039708073993679704, 9.236078724457858158, 1.599625672291283607 ) ) ;
#203424 = CARTESIAN_POINT ( 'NONE',  ( 3.953084306836263995, 6.769626237021087789, 1.199719254218452047 ) ) ;
#203426 = CARTESIAN_POINT ( 'NONE',  ( -0.4294077647110585150, -6.532648833121148968, -9.469892045836655114 ) ) ;
#203427 = CARTESIAN_POINT ( 'NONE',  ( 3.709244008563481465, 1.704072514596865817, -1.083995235011512515 ) ) ;
#203428 = CARTESIAN_POINT ( 'NONE',  ( 1.364683531249990311, 4.634375000341417916, 1.214306433183764966E-14 ) ) ;
#203429 = ADVANCED_FACE ( 'NONE', ( #186266 ), #152267, .F. ) ;
#203430 = CARTESIAN_POINT ( 'NONE',  ( 6.057095868330090838, 1.688466812627244185, -1.184547966247089912 ) ) ;
#203431 = CARTESIAN_POINT ( 'NONE',  ( 10.07334494527360569, 10.85458331234846696, 0.000000000000000000 ) ) ;
#203432 = CARTESIAN_POINT ( 'NONE',  ( 5.114612887932482366, 1.494710344919391476, -1.561737693111686642 ) ) ;
#203433 = CARTESIAN_POINT ( 'NONE',  ( 6.607619761813720238, 8.802252036906432764, 1.599625672291268286 ) ) ;
#203434 = CARTESIAN_POINT ( 'NONE',  ( 0.6823417656249864960, -1.011458332991911568, -1.181850606188749264 ) ) ;
#203436 = CARTESIAN_POINT ( 'NONE',  ( 9.681421036508346845, 3.864712292056655230, -7.090140105714071161 ) ) ;
#203435 = CARTESIAN_POINT ( 'NONE',  ( 6.879836604291781121, 6.991173891287354003, -0.7998128361456341429 ) ) ;
#203437 = CARTESIAN_POINT ( 'NONE',  ( 6.114364089638775646, 10.07724917131317355, 0.7216878364870438212 ) ) ;
#203439 = CARTESIAN_POINT ( 'NONE',  ( -0.1370650511771418500, -7.902328468025382691, 10.96100467917833399 ) ) ;
#203438 = CARTESIAN_POINT ( 'NONE',  ( 2.805323142837768291, -1.806386208845015995, 1.204286856753070456 ) ) ;
#203441 = CARTESIAN_POINT ( 'NONE',  ( 1.663359199420410883, 0.9473472845980964729, 1.578708189602283873 ) ) ;
#203440 = CARTESIAN_POINT ( 'NONE',  ( -6.236387472606166327, 6.378132927569716060, -0.7216878364870278340 ) ) ;
#203442 = CARTESIAN_POINT ( 'NONE',  ( -1.201851678989727383E-14, 3.071875000341420137, 1.575800808251672791 ) ) ;
#203443 = CARTESIAN_POINT ( 'NONE',  ( 3.509492838045696672, -2.158849082856160173, 0.3763758916049686487 ) ) ;
#203444 = CARTESIAN_POINT ( 'NONE',  ( 6.883263157960358924, 7.052235917045241997, 2.651962373728885325 ) ) ;
#203445 = CARTESIAN_POINT ( 'NONE',  ( 4.012777769421401963, 1.602246665114055002, -1.597678914196493771 ) ) ;
#203446 = CARTESIAN_POINT ( 'NONE',  ( -6.501298352952815662, 7.543601818988450169, -1.199719254218446718 ) ) ;
#203447 = CARTESIAN_POINT ( 'NONE',  ( -1.001543065824772872E-14, 5.634375000341415252, 1.575800808251672791 ) ) ;
#203448 = CARTESIAN_POINT ( 'NONE',  ( 6.321627859881460587, 6.858947107989728842, -0.6823232096292205506 ) ) ;
#203449 = CARTESIAN_POINT ( 'NONE',  ( 1.500000000000001332, 13.62499999999999822, 0.000000000000000000 ) ) ;
#203450 = CARTESIAN_POINT ( 'NONE',  ( 4.556949027968946631, 8.330541276023501140, -0.7216878364870357165 ) ) ;
#203451 = CARTESIAN_POINT ( 'NONE',  ( 5.852768638770064591, -1.394116391329143667, 1.090054309861036241 ) ) ;
#203452 = CARTESIAN_POINT ( 'NONE',  ( 3.369792252087350892, 0.4868432662692974144, -1.953231169037449533 ) ) ;
#203453 = CARTESIAN_POINT ( 'NONE',  ( 8.620286740190458374, 8.951422706510690830, 1.040834085586084257E-14 ) ) ;
#203454 = CARTESIAN_POINT ( 'NONE',  ( 1.342952632442768302, 0.4104956981533373628, 2.065382446648211801 ) ) ;
#203456 = CARTESIAN_POINT ( 'NONE',  ( -1.499999999999997780, 2.900000000000020783, 1.214306433183764966E-14 ) ) ;
#203455 = CARTESIAN_POINT ( 'NONE',  ( -1.364683531250014514, 11.58854166700806410, -0.7879004041258335089 ) ) ;
#203457 = CARTESIAN_POINT ( 'NONE',  ( 0.9066264771708797410, 0.5685364763899096729, 1.885722953041415906 ) ) ;
#203458 = AXIS2_PLACEMENT_3D ( 'NONE', #188050, #8240, #172900 ) ;
#203459 = CARTESIAN_POINT ( 'NONE',  ( -3.984117037569407938, 5.741498858621315371, 1.599625672291270506 ) ) ;
#203460 = CARTESIAN_POINT ( 'NONE',  ( -9.361980464089038279, 15.42898634278301628, -7.422930886903965408 ) ) ;
#203462 = EDGE_LOOP ( 'NONE', ( #27303, #191441, #158327, #131258, #1194 ) ) ;
#203461 = CARTESIAN_POINT ( 'NONE',  ( 5.572461477490294968, 0.7419763400571472989, 1.652881490725614189 ) ) ;
#203463 = CARTESIAN_POINT ( 'NONE',  ( 5.748293942514166588, 7.729428904398431222, -1.443375672974057666 ) ) ;
#203464 = CARTESIAN_POINT ( 'NONE',  ( -1.402160292154681736E-14, -0.6156249996585817508, 1.575800808251672791 ) ) ;
#203465 = CARTESIAN_POINT ( 'NONE',  ( 4.451927283622527654, 1.870250842541102410, -0.04591718433973044494 ) ) ;
#203466 = CARTESIAN_POINT ( 'NONE',  ( 5.067269747081383890, 1.798595138155818063, 1.025117745595036656 ) ) ;
#203467 = CARTESIAN_POINT ( 'NONE',  ( -1.225000000000044276, 1.729166666666672292, -0.7072540797572958171 ) ) ;
#203468 = SHAPE_REPRESENTATION ( 'base', ( #200407 ), #13653 ) ;
#203469 = CARTESIAN_POINT ( 'NONE',  ( -5.275531169048911728, 6.287779464379406491, -1.082531754730549967 ) ) ;
#203470 = CARTESIAN_POINT ( 'NONE',  ( 2.218196896764117909, -0.9619707940356122533, 2.597613648450887158 ) ) ;
#203471 = CARTESIAN_POINT ( 'NONE',  ( -1.500000000000001332, 0.4000000000000253353, 0.000000000000000000 ) ) ;
#203472 = CARTESIAN_POINT ( 'NONE',  ( 7.100719765255169236, 9.307259030929609267, -1.599625672291262513 ) ) ;
#203473 = CARTESIAN_POINT ( 'NONE',  ( -9.989660255170729641, 10.54902514065433827, -0.7998128361456291469 ) ) ;
#203474 = CARTESIAN_POINT ( 'NONE',  ( 5.071631979963703962, 8.074598522336444262, 1.199719254218451159 ) ) ;
#203475 = B_SPLINE_CURVE_WITH_KNOTS ( 'NONE', 3,
 ( #84113, #136079, #181605, #100365, #150201, #166435, #1772 ),
 .UNSPECIFIED., .F., .F.,
 ( 4, 3, 4 ),
 ( 3.104682540412456132E-18, 8.743668306901165302E-05, 0.0001748766834010605654 ),
 .UNSPECIFIED. ) ;
#203476 = CARTESIAN_POINT ( 'NONE',  ( -1.402160292154681736E-14, 0.4468750003414233563, -1.575800808251665908 ) ) ;
#203477 = CARTESIAN_POINT ( 'NONE',  ( -1.500000000000013101, 0.9208333333333594828, 0.8660254037844403729 ) ) ;
#203479 = CARTESIAN_POINT ( 'NONE',  ( 4.364835388595708743, 7.179726155748598515, 1.199719254218462483 ) ) ;
#203478 = CARTESIAN_POINT ( 'NONE',  ( 4.668382477721988444, -0.8370036265390871089, -1.774476930476886594 ) ) ;
#203480 = CARTESIAN_POINT ( 'NONE',  ( 2.513045873335067792, 2.015604327017831654, 0.05229110803010170866 ) ) ;
#203481 = CARTESIAN_POINT ( 'NONE',  ( 0.7499999999999885647, 2.847916667349487341, -1.299038105676658228 ) ) ;
#203482 = CARTESIAN_POINT ( 'NONE',  ( -0.02351032182101517320, -2.127384168920816165, -0.5261613093957145937 ) ) ;
#203483 = CARTESIAN_POINT ( 'NONE',  ( -11.86239285000045918, 9.719999999999982876, 1.812080536912751283 ) ) ;
#203484 = CARTESIAN_POINT ( 'NONE',  ( 2.460033746253722065, 0.7958763861501785275, 1.692906160045657860 ) ) ;
#203485 = CARTESIAN_POINT ( 'NONE',  ( 1.364683531249992088, 5.634375000341417916, 1.214306433183764966E-14 ) ) ;
#203486 = CARTESIAN_POINT ( 'NONE',  ( 4.552993993533384298, 0.3484205210483002357, 1.982688671860346252 ) ) ;
#203487 = CARTESIAN_POINT ( 'NONE',  ( -8.941766003412679353, 10.39081407785832845, -1.199719254218446718 ) ) ;
#203489 = CARTESIAN_POINT ( 'NONE',  ( 4.025106843427800563, -1.841118617500647314, 1.045351873429276601 ) ) ;
#203488 = CARTESIAN_POINT ( 'NONE',  ( -4.284013352238255301, 6.981470763377843447, -1.082531754730549967 ) ) ;
#203490 = CARTESIAN_POINT ( 'NONE',  ( -2.795860172527854903, 2.967839529530329479, -2.452799336324934742 ) ) ;
#203491 = CARTESIAN_POINT ( 'NONE',  ( 6.127406499145813257, 0.1562011534181114436, -2.064545280851529885 ) ) ;
#203493 = CARTESIAN_POINT ( 'NONE',  ( 6.720655732516647163, 1.258879151752972048, 2.189434846530075252 ) ) ;
#203492 = CARTESIAN_POINT ( 'NONE',  ( 1.083664105429899216, -0.9366695517310281716, 1.869248094466950949 ) ) ;
#203495 = VERTEX_POINT ( 'NONE', #206787 ) ;
#203494 = CARTESIAN_POINT ( 'NONE',  ( 0.08252656676070461994, -0.1270158569062987686, -1.696106202995291357 ) ) ;
#203496 = CARTESIAN_POINT ( 'NONE',  ( 6.591235234537977661, 10.84152487360300299, 0.7998128361456462443 ) ) ;
#203497 = CARTESIAN_POINT ( 'NONE',  ( -4.510196435976065565, 7.040407170307378060, -1.149263043085164915 ) ) ;
#203498 = CARTESIAN_POINT ( 'NONE',  ( 2.859846416572967343, 6.488237919310435586, 0.2290337979853694639 ) ) ;
#203499 = CARTESIAN_POINT ( 'NONE',  ( -9.348561386651960348, 4.000000000000000888, 7.001914024036569373 ) ) ;
#203500 = CARTESIAN_POINT ( 'NONE',  ( 5.734735788456138295, 8.673980272298743799, -1.082531754730537976 ) ) ;
#203501 = CARTESIAN_POINT ( 'NONE',  ( 0.6823417656249934904, 13.25520833367473195, 1.181850606188764807 ) ) ;
#203502 = EDGE_CURVE ( 'NONE', #105963, #177940, #207098, .T. ) ;
#203503 = CARTESIAN_POINT ( 'NONE',  ( 6.129550632656369125, -0.2293275368827427663, 1.898405681093485953 ) ) ;
#203504 = CARTESIAN_POINT ( 'NONE',  ( -7.263417608619167076, 9.497073181520933716, -1.599625672291263179 ) ) ;
#203505 = CIRCLE ( 'NONE', #6534, 0.07999999999999998779 ) ;
#203506 = CARTESIAN_POINT ( 'NONE',  ( 5.626797444871351139, 6.523350759560078593, 1.199719254218462483 ) ) ;
#203507 = CARTESIAN_POINT ( 'NONE',  ( -6.845108005540232021, -7.986884274785872151, 6.643335646896343150 ) ) ;
#203508 = CARTESIAN_POINT ( 'NONE',  ( 0.000000000000000000, 8.600000000000017408, -0.3999999999999819811 ) ) ;
#203509 = CARTESIAN_POINT ( 'NONE',  ( 2.846322183865124700, 5.408127416896231665, -1.199719254218446718 ) ) ;
#203510 = ORIENTED_EDGE ( 'NONE', *, *, #150811, .T. ) ;
#203511 = CARTESIAN_POINT ( 'NONE',  ( 5.607046053289695742, -0.04666138757647777385, 2.016035322322209389 ) ) ;
#203512 = LINE ( 'NONE', #195573, #169960 ) ;
#203513 = CARTESIAN_POINT ( 'NONE',  ( 1.311466561510864937, 4.574475816212405313E-14, -0.2054205618200592443 ) ) ;
#203514 = AXIS2_PLACEMENT_3D ( 'NONE', #87334, #1785, #138232 ) ;
#203515 = DIRECTION ( 'NONE',  ( -5.578564026256490882E-16, -1.000000000000000000, -9.066213480720158442E-32 ) ) ;
#203516 = CARTESIAN_POINT ( 'NONE',  ( -5.178851490740209229, 7.065079377328788546, 1.443375672974064550 ) ) ;
#203517 = CARTESIAN_POINT ( 'NONE',  ( 8.242994207428692377, 12.56065097540143327, -0.7216878364870328300 ) ) ;
#203518 = CARTESIAN_POINT ( 'NONE',  ( 4.012523933672189180, 0.7048025691861439235, 1.839212210364450151 ) ) ;
#203519 = CARTESIAN_POINT ( 'NONE',  ( 4.271111354109316416, 1.799915745204151429, -0.9091612155255476280 ) ) ;
#203520 = CARTESIAN_POINT ( 'NONE',  ( -7.705111371268023923, 7.883718109434487253, 1.040834085586084257E-14 ) ) ;
#203521 = CARTESIAN_POINT ( 'NONE',  ( 11.33772463945036790, 13.40000000000000036, -3.600000000000002309 ) ) ;
#203522 = CARTESIAN_POINT ( 'NONE',  ( 4.769572470968366673, 1.260305947291120221, 1.792593939366843303 ) ) ;
#203523 = CARTESIAN_POINT ( 'NONE',  ( 3.189213936345665523, 2.817530495244580102, 2.450448857954567572 ) ) ;
#203524 = CARTESIAN_POINT ( 'NONE',  ( 3.680616551068579767, -1.856277683350136432, -0.5147254836462693550 ) ) ;
#203525 = CARTESIAN_POINT ( 'NONE',  ( -6.995117189646935962, 10.24838825697502109, 1.199719254218453823 ) ) ;
#203526 = CARTESIAN_POINT ( 'NONE',  ( -0.1294898018152383368, 5.723764454335155349, -2.520545915250469893 ) ) ;
#203527 = CARTESIAN_POINT ( 'NONE',  ( 0.4345545588612038101, 1.130843733186673639, -1.894998796914903139 ) ) ;
#203528 = SURFACE_SIDE_STYLE ('',( #73553 ) ) ;
#203529 = CARTESIAN_POINT ( 'NONE',  ( 4.394251184604942573, 8.140727125432185574, -0.7216878364870246143 ) ) ;
#203530 = ORIENTED_EDGE ( 'NONE', *, *, #72282, .T. ) ;
#203531 = CARTESIAN_POINT ( 'NONE',  ( 3.445180431648313224, 7.033477913649446300, 0.7216878364870257245 ) ) ;
#203532 = CARTESIAN_POINT ( 'NONE',  ( 4.768383308330760961, -0.8382467442454040185, -1.782262242837754807 ) ) ;
#203533 = ORIENTED_EDGE ( 'NONE', *, *, #69586, .T. ) ;
#203535 = CARTESIAN_POINT ( 'NONE',  ( 4.582685675920167512, -1.313125608480088635, 1.525959163679012187 ) ) ;
#203534 = CARTESIAN_POINT ( 'NONE',  ( -0.02402099761080173090, -1.884047281740467872, -0.4708274727777494451 ) ) ;
#203536 = CARTESIAN_POINT ( 'NONE',  ( 5.255319057710332586, -2.280117823540278366, -0.2889680969316887893 ) ) ;
#203538 = CARTESIAN_POINT ( 'NONE',  ( 3.133497910287503796, 1.768579976953125632, -0.5793101531420452588 ) ) ;
#203537 = CARTESIAN_POINT ( 'NONE',  ( -8.120407659942227241, 8.438506789546210030, 0.7998128361456341429 ) ) ;
#203539 = CARTESIAN_POINT ( 'NONE',  ( 7.147083253059300922, 8.367293879104554577, 1.199719254218452935 ) ) ;
#203540 = DIRECTION ( 'NONE',  ( 0.000000000000000000, 1.084202172485501594E-14, -1.000000000000000000 ) ) ;
#203541 = CARTESIAN_POINT ( 'NONE',  ( -5.859094939400033120, 9.987361195942037639, -0.7998128361456231517 ) ) ;
#203542 = CARTESIAN_POINT ( 'NONE',  ( -4.014622883422322985, 7.697827440719083647, -0.7216878364870458196 ) ) ;
#203543 = CARTESIAN_POINT ( 'NONE',  ( 6.321832389622432657, 1.203313566387714584, -1.709558936785739780 ) ) ;
#203544 = CARTESIAN_POINT ( 'NONE',  ( 4.690757960648221037, 7.456006139856155457, 1.082531754730558626 ) ) ;
#203545 = EDGE_LOOP ( 'NONE', ( #111763, #189670, #149300, #202469 ) ) ;
#203546 =( NAMED_UNIT ( * ) PLANE_ANGLE_UNIT ( ) SI_UNIT ( $, .RADIAN. ) );
#203547 = CYLINDRICAL_SURFACE ( 'NONE', #44461, 1.250000000000000000 ) ;
#203548 = CARTESIAN_POINT ( 'NONE',  ( 0.2756506080626683342, 1.048234779247591453, 1.494575289200591239 ) ) ;
#203549 = CARTESIAN_POINT ( 'NONE',  ( -5.762378981008047241, 6.681529218386182301, 1.199719254218450271 ) ) ;
#203550 = B_SPLINE_CURVE_WITH_KNOTS ( 'NONE', 1,
 ( #113551, #213088 ),
 .UNSPECIFIED., .F., .F.,
 ( 2, 2 ),
 ( 0.2265555213262060719, 0.4428258268412425536 ),
 .UNSPECIFIED. ) ;
#203551 =( BOUNDED_SURFACE ( )  B_SPLINE_SURFACE ( 3, 2, ( 
 ( #193140, #111975, #44788 ),
 ( #197400, #177976, #28514 ),
 ( #94605, #131403, #95677 ),
 ( #161731, #80464, #145514 ) ),
 .UNSPECIFIED., .F., .F., .F. ) 
 B_SPLINE_SURFACE_WITH_KNOTS ( ( 4, 4 ),
 ( 3, 3 ),
 ( -4.336808689942017736E-18, 0.002003486994853882937 ),
 ( 0.000000000000000000, 1.000000000000000000 ),
 .UNSPECIFIED. ) 
 GEOMETRIC_REPRESENTATION_ITEM ( )  RATIONAL_B_SPLINE_SURFACE ( (
 ( 1.000000000000000000, 0.7779734834199527604, 1.000000000000000000),
 ( 1.000000000000000000, 0.7856061901475716036, 1.000000000000000000),
 ( 1.000000000000000000, 0.7951961705782252254, 1.000000000000000000),
 ( 1.000000000000000000, 0.8104931255419017821, 1.000000000000000000) ) ) 
 REPRESENTATION_ITEM ( '' )  SURFACE ( )  );
#203552 = CARTESIAN_POINT ( 'NONE',  ( 2.285452750267936484, 1.391693986029099772, -1.034342955966370603 ) ) ;
#203553 = DIRECTION ( 'NONE',  ( 0.000000000000000000, 1.000000000000000000, 0.000000000000000000 ) ) ;
#203554 = CARTESIAN_POINT ( 'NONE',  ( 6.509000000000035868, 7.629137130509092479, 2.600000000000000977 ) ) ;
#203555 = CARTESIAN_POINT ( 'NONE',  ( -5.422371370461663176, 8.413518134592214537, -1.199719254218446718 ) ) ;
#203556 = CARTESIAN_POINT ( 'NONE',  ( 0.7499999999999885647, 3.316666666666689967, -1.299038105676658228 ) ) ;
#203557 = CARTESIAN_POINT ( 'NONE',  ( 0.6552395816744536194, 1.723207459482085202, -1.147090658606984892 ) ) ;
#203558 = CARTESIAN_POINT ( 'NONE',  ( 5.074738461036464088, -1.720261882950037124, -0.6118011564382742629 ) ) ;
#203559 = CARTESIAN_POINT ( 'NONE',  ( 3.028120845615461132, 1.045410262836780069, 1.659804706804830277 ) ) ;
#203560 = EDGE_CURVE ( 'NONE', #138365, #33049, #213877, .T. ) ;
#203561 = CARTESIAN_POINT ( 'NONE',  ( 1.224999999999999201, -0.5416666659838705877, -0.7072540797572937077 ) ) ;
#203562 = CARTESIAN_POINT ( 'NONE',  ( -9.677822722056413696, 10.18521468535430685, 1.040834085586084257E-14 ) ) ;
#203563 = CARTESIAN_POINT ( 'NONE',  ( 5.913327553854682783, 10.05063257947248800, -0.7998128361456291469 ) ) ;
#203564 = CARTESIAN_POINT ( 'NONE',  ( 4.160867320283115234, 0.5667376361006767338, 2.043264482828925033 ) ) ;
#203565 = CARTESIAN_POINT ( 'NONE',  ( 6.749980374757213575, 8.968339418673846097, 1.599625672291268286 ) ) ;
#203566 = EDGE_CURVE ( 'NONE', #78601, #45420, #186215, .T. ) ;
#203567 = CARTESIAN_POINT ( 'NONE',  ( -9.969323024750229578, 10.52529837183042716, -0.7998128361456291469 ) ) ;
#203568 = CARTESIAN_POINT ( 'NONE',  ( 1.270471156847551075, -0.9273748054965322840, -1.850965650132020635 ) ) ;
#203570 = CARTESIAN_POINT ( 'NONE',  ( -0.6823417656250003738, -0.9697916663252494907, -1.181850606188749264 ) ) ;
#203569 = PRESENTATION_STYLE_ASSIGNMENT (( #168959 ) ) ;
#203572 = ORIENTED_EDGE ( 'NONE', *, *, #29169, .F. ) ;
#203571 = CARTESIAN_POINT ( 'NONE',  ( 4.723389051577030706, 1.932298245749045629, 1.095468883668549553 ) ) ;
#203573 = CARTESIAN_POINT ( 'NONE',  ( 1.284255082537180570, 1.875723515222413207, -1.328569176028525645 ) ) ;
#203575 = CARTESIAN_POINT ( 'NONE',  ( 1.164813196467245904, 1.489159823276710926, -1.277213275948145599 ) ) ;
#203574 = CARTESIAN_POINT ( 'NONE',  ( 7.917598520700710019, 12.18102267421877727, -0.7216878364870328300 ) ) ;
#203577 = CARTESIAN_POINT ( 'NONE',  ( 3.475000000000000533, -0.8750000000000007772, 0.000000000000000000 ) ) ;
#203576 = CARTESIAN_POINT ( 'NONE',  ( 6.482206841109512396, 9.616306177052839743, -1.082531754730548412 ) ) ;
#203578 = DIRECTION ( 'NONE',  ( 0.000000000000000000, -0.000000000000000000, 1.000000000000000000 ) ) ;
#203579 = CARTESIAN_POINT ( 'NONE',  ( -11.04536101718726293, 10.90000000000000036, 1.099999999999996758 ) ) ;
#203580 = DIRECTION ( 'NONE',  ( 0.000000000000000000, -1.000000000000000000, 0.000000000000000000 ) ) ;
#203581 = CARTESIAN_POINT ( 'NONE',  ( 2.584119536544440265, 1.026460374567798484, 1.613398670029235538 ) ) ;
#203582 = CARTESIAN_POINT ( 'NONE',  ( -0.04202953795663257053, 6.478538335026032158, -3.086709765070265288 ) ) ;
#203583 = CARTESIAN_POINT ( 'NONE',  ( 3.645241786196154354, -1.305741510076625644, -1.126962775032739339 ) ) ;
#203584 = CARTESIAN_POINT ( 'NONE',  ( 2.202361591730035428, 1.313542931311746598, -1.530159205979222392 ) ) ;
#203585 = CARTESIAN_POINT ( 'NONE',  ( 4.360180292246352174, 0.0003893357360621601550, -2.298851035006874266 ) ) ;
#203586 = CARTESIAN_POINT ( 'NONE',  ( 3.761208288054026738, -1.993080904335465142, -1.070619287061522318 ) ) ;
#203587 = CARTESIAN_POINT ( 'NONE',  ( 6.129533150132032482, -1.983608965904083421, 0.7080540597134558078 ) ) ;
#203588 = CARTESIAN_POINT ( 'NONE',  ( -6.021229618244897885, 7.157760988441397743, 1.082531754730548412 ) ) ;
#203589 = ORIENTED_EDGE ( 'NONE', *, *, #197651, .T. ) ;
#203590 = CARTESIAN_POINT ( 'NONE',  ( 5.255052661293587946, -1.495254947996208950, -0.9463502368073344329 ) ) ;
#203592 = CARTESIAN_POINT ( 'NONE',  ( 0.9379084653730703769, 0.9244841788896654977, -2.097747560502453812 ) ) ;
#203591 = CARTESIAN_POINT ( 'NONE',  ( 7.876360894896227371, 8.153785563659219804, -0.7998128361456341429 ) ) ;
#203593 = CARTESIAN_POINT ( 'NONE',  ( 5.876868881424701208, 1.699447150514224125, -0.7087742222662285485 ) ) ;
#203594 = CARTESIAN_POINT ( 'NONE',  ( -2.625475302540713152, 6.214804952939456228, -0.7998128361456281477 ) ) ;
#203595 = CARTESIAN_POINT ( 'NONE',  ( 5.859372887940716090, 2.159598860408561194, -0.3713886045505072619 ) ) ;
#203596 = CARTESIAN_POINT ( 'NONE',  ( -4.655245641445871385, 6.524482229810530498, 1.599625672291263179 ) ) ;
#203597 = CARTESIAN_POINT ( 'NONE',  ( -4.308793891044708779, 3.921347715840572956, 1.214306433183764966E-14 ) ) ;
#203598 = CARTESIAN_POINT ( 'NONE',  ( -4.767738813365186346, 15.46911576196198901, 11.02133430360666644 ) ) ;
#203599 = CARTESIAN_POINT ( 'NONE',  ( 5.336411075974297979, -1.153114810915600641, 1.719314882265559286 ) ) ;
#203600 = CARTESIAN_POINT ( 'NONE',  ( 1.710173085450257924, 1.157096902994741772, -1.651345047625000007 ) ) ;
#203601 = CARTESIAN_POINT ( 'NONE',  ( -0.7500000000000006661, -1.110416665983847473, -1.299038105676652011 ) ) ;
#203602 = CARTESIAN_POINT ( 'NONE',  ( 3.984924265943972532, -0.1901312170250069600, -1.917098255223735004 ) ) ;
#203603 = CARTESIAN_POINT ( 'NONE',  ( -1.364683531250014514, 10.33854166700806765, -0.7879004041258335089 ) ) ;
#203604 = CARTESIAN_POINT ( 'NONE',  ( 0.9322285317887604172, -2.165714743787349406, 0.4936765188615526712 ) ) ;
#203606 = ORIENTED_EDGE ( 'NONE', *, *, #15247, .F. ) ;
#203605 = CARTESIAN_POINT ( 'NONE',  ( 2.878073747850912412, 6.579779482459851003, -0.7998128361456362523 ) ) ;
#203608 = CARTESIAN_POINT ( 'NONE',  ( -1.127943160727153060, 2.800000000000024691, -0.7749999999999935829 ) ) ;
#203607 = CARTESIAN_POINT ( 'NONE',  ( 1.419999999999820961, 7.176846818246208848, -4.202462424328213153 ) ) ;
#203609 = CARTESIAN_POINT ( 'NONE',  ( 4.216749469050096621, 4.878294787768598262, -1.199719254218452047 ) ) ;
#203610 = CARTESIAN_POINT ( 'NONE',  ( -3.475000000000000533, -2.479166666666667851, -2.006292185433948827 ) ) ;
#203611 = CARTESIAN_POINT ( 'NONE',  ( -10.97011102005664185, 9.799999999999982947, 1.696376167609455310 ) ) ;
#203612 = CARTESIAN_POINT ( 'NONE',  ( 1.499999999999821032, 10.00000000000000178, -4.154462424328206893 ) ) ;
#203613 = B_SPLINE_CURVE_WITH_KNOTS ( 'NONE', 3,
 ( #73041, #207325, #140229, #120820, #23215, #187862, #119741, #39489, #204085, #186797 ),
 .UNSPECIFIED., .F., .F.,
 ( 4, 3, 3, 4 ),
 ( 0.000000000000000000, 3.125155738325145446E-05, 5.612058060597180007E-05, 8.099573230367171513E-05 ),
 .UNSPECIFIED. ) ;
#203614 = CARTESIAN_POINT ( 'NONE',  ( 1.943732651021431224, 1.350599318427040840, 1.423195245143428433 ) ) ;
#203616 = CARTESIAN_POINT ( 'NONE',  ( 0.6823417656249899377, 2.155208333674753174, 1.181850606188767472 ) ) ;
#203615 = CARTESIAN_POINT ( 'NONE',  ( 3.960953433486789521, 7.772862772376584850, -0.7998128361456221525 ) ) ;
#203617 = CARTESIAN_POINT ( 'NONE',  ( -4.344470927813957495, 7.211826089590096522, 1.015455228366731966 ) ) ;
#203618 = DIRECTION ( 'NONE',  ( -0.000000000000000000, 1.000000000000000000, -0.000000000000000000 ) ) ;
#203619 = CARTESIAN_POINT ( 'NONE',  ( 6.514115657861259123, 1.956686900881845714, -0.1430618042221123987 ) ) ;
#203620 = CARTESIAN_POINT ( 'NONE',  ( -7.648771216403934758, 12.07531685244661723, -0.7998128361456291469 ) ) ;
#203621 = CARTESIAN_POINT ( 'NONE',  ( -4.812781342726871969, 6.637997537979888563, 1.443375672974064550 ) ) ;
#203622 = CARTESIAN_POINT ( 'NONE',  ( 6.332923096303629151, 0.2067577541180857514, 2.151790036905242953 ) ) ;
#203624 = VERTEX_POINT ( 'NONE', #190533 ) ;
#203623 = CARTESIAN_POINT ( 'NONE',  ( -5.205440912643032547, 8.160432600470439723, 1.199719254218452047 ) ) ;
#203625 = CARTESIAN_POINT ( 'NONE',  ( -1.402160292154681736E-14, -1.256249999317182953, 1.732050807568877637 ) ) ;
#203626 = CARTESIAN_POINT ( 'NONE',  ( 1.229531971273215341, -1.182229855178434930, -1.449605969065965949 ) ) ;
#203627 = CARTESIAN_POINT ( 'NONE',  ( 6.889999999999967706, 0.005249217920031550542, 1.719840535937327664 ) ) ;
#203629 = CARTESIAN_POINT ( 'NONE',  ( 4.528971853086540378, -2.003544689622422936, 0.8885388601788182239 ) ) ;
#203628 = CARTESIAN_POINT ( 'NONE',  ( -0.6801582343750282034, 2.432291667008048996, 1.178068619123807004 ) ) ;
#203630 = CARTESIAN_POINT ( 'NONE',  ( 6.001056180859140277, 1.891180833080384982, -1.322043635676501072 ) ) ;
#203631 = CARTESIAN_POINT ( 'NONE',  ( 6.819606862646741874, -2.000071036334325036, 0.4962039222910428760 ) ) ;
#203632 = CARTESIAN_POINT ( 'NONE',  ( 2.783070106938976274, 1.373617692895822806, 1.372961415081490610 ) ) ;
#203633 = CARTESIAN_POINT ( 'NONE',  ( -4.894130264408866893, 6.732904613275549899, -1.443375672974051449 ) ) ;
#203634 = CARTESIAN_POINT ( 'NONE',  ( 0.1851935683049925341, 13.36182424988519912, -1.369245237587793040 ) ) ;
#203635 = ADVANCED_FACE ( 'NONE', ( #95202 ), #123515, .T. ) ;
#203636 = CARTESIAN_POINT ( 'NONE',  ( 3.268924434670684498, 6.827845917175511481, -1.734723475976807094E-15 ) ) ;
#203637 = CARTESIAN_POINT ( 'NONE',  ( 1.360316468749963592, 0.03645833367470611985, -0.7853790794159122290 ) ) ;
#203638 = CARTESIAN_POINT ( 'NONE',  ( 2.936172824561166905, -1.650081981912490336, -1.158688413653415239 ) ) ;
#203639 = CARTESIAN_POINT ( 'NONE',  ( -3.592547517496941900, 5.214391408544949869, -1.443375672974051449 ) ) ;
#203640 = CARTESIAN_POINT ( 'NONE',  ( -6.740338644649361832, 7.892758502626242567, -1.199719254218452047 ) ) ;
#203641 = CARTESIAN_POINT ( 'NONE',  ( 7.750457368506414646, 12.19395069656619945, 0.7998128361456462443 ) ) ;
#203643 = CARTESIAN_POINT ( 'NONE',  ( -1.177110729581226867, 3.120878374463987193, 0.7750000000000083489 ) ) ;
#203642 = CARTESIAN_POINT ( 'NONE',  ( 1.471042373949003501, 0.1361147407585860392, -1.820667060309004937 ) ) ;
#203644 = CARTESIAN_POINT ( 'NONE',  ( -4.098307573080856692, 8.003385611894792362, 0.7998128361456352531 ) ) ;
#203645 = CARTESIAN_POINT ( 'NONE',  ( -5.655686355556086120, 6.627330832017406692, 1.199719254218452935 ) ) ;
#203646 = CARTESIAN_POINT ( 'NONE',  ( -10.97061778408437505, 3.255139717175850933, 6.407648009301818881 ) ) ;
#203647 = ORIENTED_EDGE ( 'NONE', *, *, #205165, .T. ) ;
#203648 = CARTESIAN_POINT ( 'NONE',  ( 0.4620835240300471547, 2.137967531602209981, -0.3185850937674692407 ) ) ;
#203649 = CARTESIAN_POINT ( 'NONE',  ( -7.078765599666485997, 7.431183752465250869, 0.000000000000000000 ) ) ;
#203650 = CARTESIAN_POINT ( 'NONE',  ( 4.121315508874254796, 5.831287398485175189, -1.443375672974051449 ) ) ;
#203651 = CARTESIAN_POINT ( 'NONE',  ( -4.302014814237876017, 3.913438792899272212, 0.7998128361456341429 ) ) ;
#203653 = CARTESIAN_POINT ( 'NONE',  ( -9.134442807305063639, 11.67993591332117376, 1.599625672291281386 ) ) ;
#203652 = B_SPLINE_CURVE_WITH_KNOTS ( 'NONE', 3,
 ( #69788, #119701, #166252, #52500, #87133, #153204 ),
 .UNSPECIFIED., .F., .F.,
 ( 4, 2, 4 ),
 ( 0.000000000000000000, 0.5000000000000001110, 1.000000000000000000 ),
 .UNSPECIFIED. ) ;
#203654 = CARTESIAN_POINT ( 'NONE',  ( 5.285809349500922849, 1.945818207184028426, -0.5408622128197750900 ) ) ;
#203656 = EDGE_LOOP ( 'NONE', ( #163351, #56827, #2534 ) ) ;
#203655 = CARTESIAN_POINT ( 'NONE',  ( 5.444044349889116674, -1.407711435423303792, -1.718264895412445536 ) ) ;
#203657 = CARTESIAN_POINT ( 'NONE',  ( -3.709037541790315640, 6.484905011134099340, -1.199719254218450271 ) ) ;
#203658 = CARTESIAN_POINT ( 'NONE',  ( 6.817052309572890323, 6.847649204123507083, 0.7998128361456341429 ) ) ;
#203659 = CARTESIAN_POINT ( 'NONE',  ( 5.348532861604016198, 0.5962098156395375659, 1.972770010162463228 ) ) ;
#203660 = CARTESIAN_POINT ( 'NONE',  ( 4.219375079941334761, 1.978050461189932552, 0.3905991720301109082 ) ) ;
#203661 = ORIENTED_EDGE ( 'NONE', *, *, #90488, .T. ) ;
#203662 = CARTESIAN_POINT ( 'NONE',  ( 5.181758602633668609, 4.945385036406048762, -2.420000000000000373 ) ) ;
#203663 = CARTESIAN_POINT ( 'NONE',  ( 2.354312230267378236, 5.898448035287240820, -0.7998128361456281477 ) ) ;
#203664 =( GEOMETRIC_REPRESENTATION_CONTEXT ( 3 ) GLOBAL_UNCERTAINTY_ASSIGNED_CONTEXT ( ( #135217 ) ) GLOBAL_UNIT_ASSIGNED_CONTEXT ( ( #89600, #108033, #90666 ) ) REPRESENTATION_CONTEXT ( 'NONE', 'WORKASPACE' ) );
#203666 = ORIENTED_EDGE ( 'NONE', *, *, #197814, .T. ) ;
#203665 = CARTESIAN_POINT ( 'NONE',  ( -6.688968683495758683, 8.897159112202094988, -1.599625672291271394 ) ) ;
#203667 = CARTESIAN_POINT ( 'NONE',  ( 4.681345713234763117, 8.384430392927429310, -0.5894114041281351968 ) ) ;
#203668 = CARTESIAN_POINT ( 'NONE',  ( 4.059922587279920947, 1.704677108394496043, -1.076152822228809480 ) ) ;
#203669 = CARTESIAN_POINT ( 'NONE',  ( 3.099365256270599112, -1.839010575856118823, 0.09107247011905240941 ) ) ;
#203670 = DIRECTION ( 'NONE',  ( 0.000000000000000000, 0.000000000000000000, 1.000000000000000000 ) ) ;
#203671 = CARTESIAN_POINT ( 'NONE',  ( 2.315413608375629817, 2.062204878978285194, 1.035883635760030508 ) ) ;
#203672 = CARTESIAN_POINT ( 'NONE',  ( 4.492547798081839794, 6.334668079219206049, 1.599625672291262513 ) ) ;
#203673 = CARTESIAN_POINT ( 'NONE',  ( 4.130267194010744269, 1.160198474277823300, -1.823679694223250491 ) ) ;
#203674 = CARTESIAN_POINT ( 'NONE',  ( 7.248805684800777804, 11.60869039890961218, 1.040834085586084257E-14 ) ) ;
#203675 = CARTESIAN_POINT ( 'NONE',  ( -4.791917227426195858, 7.677988301050826969, -1.199719254218452047 ) ) ;
#203676 = CARTESIAN_POINT ( 'NONE',  ( 3.357065504480163387, -0.9345643552367989271, 2.099969358187879109 ) ) ;
#203677 = CARTESIAN_POINT ( 'NONE',  ( -9.523545778475458690, 14.62276350342200359, -7.300907474435643252 ) ) ;
#203678 = CARTESIAN_POINT ( 'NONE',  ( 1.252085211431710698, 2.800000000000024691, 0.7750000000000152323 ) ) ;
#203679 = CARTESIAN_POINT ( 'NONE',  ( 2.324885834233282544, -0.002380789299309681549, 1.870836310375329381 ) ) ;
#203680 = CIRCLE ( 'NONE', #158721, 0.08000000000000004330 ) ;
#203681 = CARTESIAN_POINT ( 'NONE',  ( 0.3156150085598420363, -1.934196717871897953, 0.3801348212975861895 ) ) ;
#203683 = CARTESIAN_POINT ( 'NONE',  ( -7.584860592202423035, 7.813701877183096833, -0.7998128361456362523 ) ) ;
#203682 = CARTESIAN_POINT ( 'NONE',  ( -0.6823417656249969321, 4.467708333674755394, -1.181850606188749264 ) ) ;
#203684 = CARTESIAN_POINT ( 'NONE',  ( 2.069229996397306426, -2.018448871333050842, -0.8927042923378907258 ) ) ;
#203685 = ORIENTED_EDGE ( 'NONE', *, *, #6236, .T. ) ;
#203686 = ADVANCED_FACE ( 'NONE', ( #25899 ), #32063, .T. ) ;
#203687 = CARTESIAN_POINT ( 'NONE',  ( 10.38614328979755719, 3.507114751586604129, -5.996442624206805405 ) ) ;
#203688 = CARTESIAN_POINT ( 'NONE',  ( 4.891794496432329886, 4.601515088792824670, -0.7998128361456211532 ) ) ;
#203689 = CARTESIAN_POINT ( 'NONE',  ( -5.596818484342970912, 5.424043074688562172, -0.7998128361456221525 ) ) ;
#203690 = CARTESIAN_POINT ( 'NONE',  ( 5.981319044003478247, 1.821754654810204599, -0.7540403668018207384 ) ) ;
#203691 = CARTESIAN_POINT ( 'NONE',  ( 5.531924057230363623, -1.459877215294088204, -1.787231782134098168 ) ) ;
#203692 = CARTESIAN_POINT ( 'NONE',  ( 0.1858947801188018389, -1.204007190563995078, -1.549573762531175625 ) ) ;
#203693 = EDGE_CURVE ( 'NONE', #100096, #44672, #178573, .T. ) ;
#203694 = CARTESIAN_POINT ( 'NONE',  ( 4.680570805348211572, 1.272886101012826288, -1.622837931747274975 ) ) ;
#203695 = CARTESIAN_POINT ( 'NONE',  ( 4.853455804012212660, 7.645820290447483458, 1.082531754730558626 ) ) ;
#203696 = CARTESIAN_POINT ( 'NONE',  ( 6.535912570239620578, 9.782925877658371405, 1.199719254218452047 ) ) ;
#203697 = CARTESIAN_POINT ( 'NONE',  ( 8.093854517234030155, 8.545177812968924869, -0.7216878364870267237 ) ) ;
#203698 = CARTESIAN_POINT ( 'NONE',  ( 0.6823417656249917140, 3.655208333674754506, 1.181850606188765695 ) ) ;
#203699 = CARTESIAN_POINT ( 'NONE',  ( -10.10413230197131540, 3.643845688154880857, -6.474695611014302798 ) ) ;
#203700 = CARTESIAN_POINT ( 'NONE',  ( 5.314433026432511475, 5.302519407033794430, 1.040834085586084257E-14 ) ) ;
#203701 = CARTESIAN_POINT ( 'NONE',  ( 5.969212972359552616, 1.911920703953375655, 1.028910892658722265 ) ) ;
#203703 = CARTESIAN_POINT ( 'NONE',  ( 5.688959394570705541, 1.398425918548395153, 1.197878823674280779 ) ) ;
#203702 = CARTESIAN_POINT ( 'NONE',  ( 0.3282377607281144472, 0.3861645503674552837, 1.224999999999980105 ) ) ;
#203704 = CARTESIAN_POINT ( 'NONE',  ( 6.620655732516659064, 6.039214117936751336, 2.421170424969817603 ) ) ;
#203705 = CARTESIAN_POINT ( 'NONE',  ( 1.859593142679900613, 3.245846270153683211, 0.3999999999999849787 ) ) ;
#203706 = CARTESIAN_POINT ( 'NONE',  ( -0.3769810270651957618, 3.049942316455299451, -0.4288785890453079008 ) ) ;
#203707 = CARTESIAN_POINT ( 'NONE',  ( -4.172014829671058855, 7.596244486910340044, 0.9145543751994407167 ) ) ;
#203708 = CARTESIAN_POINT ( 'NONE',  ( 0.3620597222943388038, 2.804586296877760621, 2.034343604466669397 ) ) ;
#203709 = CARTESIAN_POINT ( 'NONE',  ( 5.803742400754204667, 7.332416669035665358, 1.290654366993408297 ) ) ;
#203710 = CARTESIAN_POINT ( 'NONE',  ( 0.3813228709106940006, 0.1872568833237615027, -1.903067810102520241 ) ) ;
#203711 = CARTESIAN_POINT ( 'NONE',  ( 1.797346856567107798, -0.6001438452145327895, 1.665118380002019283 ) ) ;
#203712 = CARTESIAN_POINT ( 'NONE',  ( -0.09332341176954485340, -0.4182270256129701491, -1.872751671355552983 ) ) ;
#203714 = CARTESIAN_POINT ( 'NONE',  ( 4.394081885627950435, -0.8225995951327015332, -1.730150695830068308 ) ) ;
#203713 = CARTESIAN_POINT ( 'NONE',  ( -10.34217224912604571, 10.96028913360221502, 0.7998128361456462443 ) ) ;
#203715 = DIRECTION ( 'NONE',  ( -0.7592566023653004592, -0.6507913734559641616, 0.000000000000000000 ) ) ;
#203716 = CARTESIAN_POINT ( 'NONE',  ( 5.301205566836260985, -1.690247886301226909, 1.010757534590230433 ) ) ;
#203717 = CARTESIAN_POINT ( 'NONE',  ( 6.258070668236964451, 0.7691888804484037223, -1.867794269369964066 ) ) ;
#203718 = CARTESIAN_POINT ( 'NONE',  ( -1.712858683735141163, -1.037413707456537715, 1.381497717048121299 ) ) ;
#203719 = CARTESIAN_POINT ( 'NONE',  ( 3.309304339999539657, -0.3661640501408692794, 1.834289908569000538 ) ) ;
#203721 = ORIENTED_EDGE ( 'NONE', *, *, #161474, .F. ) ;
#203720 = CARTESIAN_POINT ( 'NONE',  ( 6.481054518252093111, -0.09278056567359710405, -1.722521162943893014 ) ) ;
#203723 = CARTESIAN_POINT ( 'NONE',  ( 3.172244755917638770, 5.684407401003788607, -1.082531754730543083 ) ) ;
#203722 = CARTESIAN_POINT ( 'NONE',  ( 2.368051099418837069, 2.164043333312406503, -0.4318774905316472013 ) ) ;
#203724 = CARTESIAN_POINT ( 'NONE',  ( -0.6823417656249969321, 4.030208333674754506, -1.181850606188749264 ) ) ;
#203725 = CARTESIAN_POINT ( 'NONE',  ( 0.3442780524403609155, -0.9739420414685855398, 1.818282578471181132 ) ) ;
#203727 = MECHANICAL_DESIGN_GEOMETRIC_PRESENTATION_REPRESENTATION (  '', ( #106870 ), #110431 ) ;
#203726 = CARTESIAN_POINT ( 'NONE',  ( 5.777746017718023097, 9.892454120646377191, 0.7998128361456462443 ) ) ;
#203728 = CARTESIAN_POINT ( 'NONE',  ( -9.022061154889962964, 12.61315621642528129, -1.199719254218446718 ) ) ;
#203729 = CARTESIAN_POINT ( 'NONE',  ( 9.811039896441892338, -7.242250812739402299, 1.725646424474048093E-15 ) ) ;
#203730 = CARTESIAN_POINT ( 'NONE',  ( 0.1747926744264920174, 4.095712681614646300, -2.410328719303979739 ) ) ;
#203731 = ADVANCED_FACE ( 'NONE', ( #49623 ), #54205, .F. ) ;
#203732 = CARTESIAN_POINT ( 'NONE',  ( -7.710100441483604072, -6.699703214240861904, -7.845789747616953136 ) ) ;
#203733 = ORIENTED_EDGE ( 'NONE', *, *, #191341, .T. ) ;
#203734 = CARTESIAN_POINT ( 'NONE',  ( 3.420434311836465291, 0.9283866757503267397, 1.850595421526677775 ) ) ;
#203735 = CARTESIAN_POINT ( 'NONE',  ( -1.500000000000011324, 4.879166666666690411, -0.8660254037844313801 ) ) ;
#203736 = CARTESIAN_POINT ( 'NONE',  ( 3.486418057008484617, 7.219238166485217434, 1.040834085586084257E-14 ) ) ;
#203737 = CARTESIAN_POINT ( 'NONE',  ( -5.889893629278568632, 7.264407438959931795, 1.268144897863663356 ) ) ;
#203738 = CARTESIAN_POINT ( 'NONE',  ( 0.4342474147537092044, -1.082315208530496786, -1.704999936850047249 ) ) ;
#203739 = CARTESIAN_POINT ( 'NONE',  ( -0.6823417656250212460, 2.863541667008084879, 1.181850606188767472 ) ) ;
#203740 = CARTESIAN_POINT ( 'NONE',  ( -0.6823417656249969321, 3.967708333674754950, -1.181850606188749264 ) ) ;
#203741 = ORIENTED_EDGE ( 'NONE', *, *, #13980, .T. ) ;
#203743 = CARTESIAN_POINT ( 'NONE',  ( 7.917598520700710019, 12.18102267421877727, -0.7216878364870328300 ) ) ;
#203742 = CARTESIAN_POINT ( 'NONE',  ( 0.07479286986305544449, 6.948552162806721277, -2.450557996216149892 ) ) ;
#203744 = DIRECTION ( 'NONE',  ( 8.638326563840814399E-31, 0.000000000000000000, 1.000000000000000000 ) ) ;
#203745 = CARTESIAN_POINT ( 'NONE',  ( 6.157445398352582977, 1.830988975552667153, -0.5633538272611648967 ) ) ;
#203746 = CARTESIAN_POINT ( 'NONE',  ( 6.539320575229247368, 1.272291865413360812, 2.120198356887960767 ) ) ;
#203747 = CARTESIAN_POINT ( 'NONE',  ( 4.335597073515660149, 0.9364531651635084053, -1.981528385891350386 ) ) ;
#203748 =( BOUNDED_CURVE ( )  B_SPLINE_CURVE ( 2, ( #183158, #52098, #1182, #115027, #17432, #149596, #148538, #67246, #16370 ),
 .UNSPECIFIED., .F., .T. ) 
 B_SPLINE_CURVE_WITH_KNOTS ( ( 3, 2, 2, 2, 3 ),
 ( 0.2343749999999998057, 0.2395833333333333426, 0.2500000000000000000, 0.2604166666666666852, 0.2656250000000001110 ),
 .UNSPECIFIED. ) 
 CURVE ( )  GEOMETRIC_REPRESENTATION_ITEM ( )  RATIONAL_B_SPLINE_CURVE ( ( 0.9330127018922194093, 0.9330127018922168558, 1.000000000000000000, 0.8660254037844387076, 1.000000000000000000, 0.8660254037844387076, 1.000000000000000000, 0.9330127018922178550, 0.9330127018922192983 ) ) 
 REPRESENTATION_ITEM ( '' )  );
#203749 = CARTESIAN_POINT ( 'NONE',  ( 1.499999999999989120, 2.306250000682817713, 1.214306433183764966E-14 ) ) ;
#203750 = CARTESIAN_POINT ( 'NONE',  ( 2.531394148431935776, -0.1834752923718512840, 1.903540536635806912 ) ) ;
#203751 = CARTESIAN_POINT ( 'NONE',  ( -4.218558352146454915, 8.073401844146177453, 1.040834085586084257E-14 ) ) ;
#203752 = CARTESIAN_POINT ( 'NONE',  ( 5.029711800545521250, 5.930713857800314237, -1.082531754730549078 ) ) ;
#203754 = CARTESIAN_POINT ( 'NONE',  ( 0.8785300617164049086, -0.4926655378557908138, -1.955167820405806056 ) ) ;
#203753 = CARTESIAN_POINT ( 'NONE',  ( -4.905110356762790502, 4.827649200395154772, -0.06592220986076716138 ) ) ;
#203755 = CARTESIAN_POINT ( 'NONE',  ( -1.364683531250014514, 11.15104166700806232, -0.7879004041258335089 ) ) ;
#203756 = AXIS2_PLACEMENT_3D ( 'NONE', #136279, #53951, #68024 ) ;
#203758 = CARTESIAN_POINT ( 'NONE',  ( -5.631432701629818460, 7.663367133358481631, 1.599625672291263179 ) ) ;
#203757 = CARTESIAN_POINT ( 'NONE',  ( 6.321842903100939104, 1.263506803105146847, -1.790488031206059372 ) ) ;
#203760 = ORIENTED_EDGE ( 'NONE', *, *, #113143, .T. ) ;
#203759 = CARTESIAN_POINT ( 'NONE',  ( 3.258550815082728036, -1.306766610546957530, 1.125807055032159054 ) ) ;
#203761 = CARTESIAN_POINT ( 'NONE',  ( -0.1399997263889819488, 4.088450529495776919, -2.555104583160577203 ) ) ;
#203762 = CARTESIAN_POINT ( 'NONE',  ( 7.283754839039659146, 9.520799950344851936, -1.599625672291262513 ) ) ;
#203763 = CARTESIAN_POINT ( 'NONE',  ( 3.811813743736467419, 7.598866467667865443, 1.040834085586084257E-14 ) ) ;
#203764 = CARTESIAN_POINT ( 'NONE',  ( -1.104620755056546555, 13.37576698399828246, -0.8213461108120255760 ) ) ;
#203765 = CARTESIAN_POINT ( 'NONE',  ( 0.3968290921660848070, 0.3316028935436679537, 1.933473477243151439 ) ) ;
#203766 = CARTESIAN_POINT ( 'NONE',  ( 5.301401758143367893, 6.143722458377430584, 1.199719254218462483 ) ) ;
#203767 = DIRECTION ( 'NONE',  ( 0.000000000000000000, 0.000000000000000000, -1.000000000000000000 ) ) ;
#203768 = ORIENTED_EDGE ( 'NONE', *, *, #118985, .F. ) ;
#203769 = CARTESIAN_POINT ( 'NONE',  ( -0.4000000000000166755, 3.949999999999995293, -0.8338124244296005738 ) ) ;
#203770 = ORIENTED_EDGE ( 'NONE', *, *, #43314, .F. ) ;
#203771 = CARTESIAN_POINT ( 'NONE',  ( 3.703588720873185469, 1.314418127562553940, 1.246746269480051073 ) ) ;
#203772 = EDGE_LOOP ( 'NONE', ( #126905, #52289, #8567, #138812, #162382, #40230 ) ) ;
#203773 = CARTESIAN_POINT ( 'NONE',  ( 9.297140650669039275, 11.86975006391249643, 1.599625672291281386 ) ) ;
#203774 = CARTESIAN_POINT ( 'NONE',  ( 3.223806664999388172, 6.983134552466421674, -0.7998128361456362523 ) ) ;
#203775 = CARTESIAN_POINT ( 'NONE',  ( 4.459482644723921752, -1.403152132390030449, -1.145693287117461656 ) ) ;
#203776 = CARTESIAN_POINT ( 'NONE',  ( 0.000000000000000000, 2.000000000000001776, -11.00000000000000000 ) ) ;
#203777 = CARTESIAN_POINT ( 'NONE',  ( 0.04151047742771083598, -7.963884727586698631, 9.500000000000147438 ) ) ;
#203778 = CARTESIAN_POINT ( 'NONE',  ( 5.824368567101982030, 6.018301469053008113, 0.4368841385695241275 ) ) ;
#203779 =( GEOMETRIC_REPRESENTATION_CONTEXT ( 3 ) GLOBAL_UNCERTAINTY_ASSIGNED_CONTEXT ( ( #120119 ) ) GLOBAL_UNIT_ASSIGNED_CONTEXT ( ( #30165, #79972, #114681 ) ) REPRESENTATION_CONTEXT ( 'NONE', 'WORKASPACE' ) );
#203781 = CARTESIAN_POINT ( 'NONE',  ( -1.364683531250014514, 14.83854166700806410, -0.7879004041258335089 ) ) ;
#203780 = CARTESIAN_POINT ( 'NONE',  ( 5.019887821480574885, 1.840843491799005527, -0.2725137592536843734 ) ) ;
#203782 = CARTESIAN_POINT ( 'NONE',  ( 2.407709352951839854, -1.104968261951447595, -1.564578956373291696 ) ) ;
#203783 = DIRECTION ( 'NONE',  ( 1.016547956922408957E-15, 1.000000000000000000, -4.622230424712075819E-32 ) ) ;
#203784 = CARTESIAN_POINT ( 'NONE',  ( -11.83256397649420677, 7.177290438377375459, -1.867481893931521419 ) ) ;
#203785 = CARTESIAN_POINT ( 'NONE',  ( 0.000000000000000000, 12.22000000000000064, 0.000000000000000000 ) ) ;
#203786 = CARTESIAN_POINT ( 'NONE',  ( 6.588899466561449536, 9.670504563421618016, -1.082531754730537088 ) ) ;
#203787 = CARTESIAN_POINT ( 'NONE',  ( -4.790108344329849110, 4.482881244673243337, 0.7998128361456341429 ) ) ;
#203788 = CARTESIAN_POINT ( 'NONE',  ( 11.89197415570408900, 12.30000000000000071, -0.8055989572471863314 ) ) ;
#203789 = CARTESIAN_POINT ( 'NONE',  ( 1.447338344653009701, 0.6056102050338266762, -2.000996673686726179 ) ) ;
#203790 = CARTESIAN_POINT ( 'NONE',  ( 6.215487077222150880, 6.216099443039444949, 0.000000000000000000 ) ) ;
#203791 = CARTESIAN_POINT ( 'NONE',  ( 6.598663746767657656, -0.5144617408539242653, -1.856373320315672037 ) ) ;
#203792 = CARTESIAN_POINT ( 'NONE',  ( -3.893162665418476109, 7.693773542963529444, 1.040834085586084257E-14 ) ) ;
#203793 = CARTESIAN_POINT ( 'NONE',  ( 2.942213871598579722, 1.811567870905493205, 0.2252638538085757203 ) ) ;
#203794 = CARTESIAN_POINT ( 'NONE',  ( -5.905025204054467736, 4.805319369744820435, 2.499999999999998668 ) ) ;
#203795 = CARTESIAN_POINT ( 'NONE',  ( 2.302860652515530848, -0.3306829512400177862, -1.883434002855538081 ) ) ;
#203796 = CARTESIAN_POINT ( 'NONE',  ( 2.031642458604762780, 1.885605923395494044, -0.5689241207685117319 ) ) ;
#203797 = CARTESIAN_POINT ( 'NONE',  ( 3.210425159823264707, 1.756831471361683494, 0.8279855452232912638 ) ) ;
#203798 = ORIENTED_EDGE ( 'NONE', *, *, #31271, .F. ) ;
#203799 = CARTESIAN_POINT ( 'NONE',  ( -1.084637062511559336, 3.213621193390831188, 1.105835307554800639 ) ) ;
#203801 = CARTESIAN_POINT ( 'NONE',  ( 6.491040186595096628, 0.1814514006053032646, 1.852032668777810587 ) ) ;
#203800 = CARTESIAN_POINT ( 'NONE',  ( -3.630551273409382329, 7.457669928944732796, 0.7998128361456352531 ) ) ;
#203803 = CARTESIAN_POINT ( 'NONE',  ( 4.166350089634453191, 2.120059694336435374, -0.05518752902338577848 ) ) ;
#203802 = CARTESIAN_POINT ( 'NONE',  ( 3.573456005653643519, 6.326726552307992080, -1.199719254218453823 ) ) ;
#203804 = DIRECTION ( 'NONE',  ( 0.000000000000000000, 1.000000000000000000, 0.000000000000000000 ) ) ;
#203805 = CARTESIAN_POINT ( 'NONE',  ( 8.048736748007069508, 12.54194330598362406, -0.7998128361456352531 ) ) ;
#203806 = B_SPLINE_CURVE_WITH_KNOTS ( 'NONE', 3,
 ( #103332, #20980, #72946, #186701, #40480, #74036, #206154, #123942 ),
 .UNSPECIFIED., .F., .F.,
 ( 4, 2, 2, 4 ),
 ( 0.0003130156513459781678, 0.0009018580307266956669, 0.001196279220417054579, 0.001490700410107413491 ),
 .UNSPECIFIED. ) ;
#203807 = CARTESIAN_POINT ( 'NONE',  ( -6.394605727500880299, 7.489403432619674561, -1.199719254218452047 ) ) ;
#203808 = CARTESIAN_POINT ( 'NONE',  ( 2.250290310188348464, 5.569163095287620990, 0.7216878364870438212 ) ) ;
#203809 = ORIENTED_EDGE ( 'NONE', *, *, #78727, .F. ) ;
#203810 = CARTESIAN_POINT ( 'NONE',  ( 5.189738938980948291, 9.276722205444929870, 0.000000000000000000 ) ) ;
#203811 = PLANE ( 'NONE',  #144680 ) ;
#203812 = CARTESIAN_POINT ( 'NONE',  ( 4.424309136736732206, 1.121156565774838354, -1.440799707636587712 ) ) ;
#203813 = FACE_OUTER_BOUND ( 'NONE', #77433, .T. ) ;
#203814 = CARTESIAN_POINT ( 'NONE',  ( -9.327646496521984076, 11.90534021740758064, -1.443375672974059665 ) ) ;
#203815 = CARTESIAN_POINT ( 'NONE',  ( -5.321855017605967575, 7.728530711523490027, 1.321107644836617467 ) ) ;
#203816 = DIRECTION ( 'NONE',  ( 5.551115123125764213E-17, 0.000000000000000000, -1.000000000000000000 ) ) ;
#203817 = CARTESIAN_POINT ( 'NONE',  ( 4.117926171558832671, -0.9613396577640184182, -1.604580606731422554 ) ) ;
#203818 = CARTESIAN_POINT ( 'NONE',  ( 7.377608144130607393, 11.75895993479440982, -0.7998128361456291469 ) ) ;
#203819 = CARTESIAN_POINT ( 'NONE',  ( 2.191906549581578822, -0.8239416835312768361, 1.741544141456285555 ) ) ;
#203820 = CARTESIAN_POINT ( 'NONE',  ( 6.807479307002794577, -1.573682814073861902, -1.171087784426767753 ) ) ;
#203821 = ADVANCED_FACE ( 'NONE', ( #38720 ), #159217, .T. ) ;
#203822 = CARTESIAN_POINT ( 'NONE',  ( 0.6823417656249934904, 8.505208333674733723, 1.181850606188764807 ) ) ;
#203823 = CARTESIAN_POINT ( 'NONE',  ( -5.526920175865215334, 9.599823971818089774, 0.7998128361456481317 ) ) ;
#203824 = CARTESIAN_POINT ( 'NONE',  ( 4.847203612085560387, 5.613824621309978724, -1.199719254218452047 ) ) ;
#203825 = CARTESIAN_POINT ( 'NONE',  ( -5.465345319640241506, 5.548860092434608760, 0.7216878364870257245 ) ) ;
#203826 = CARTESIAN_POINT ( 'NONE',  ( 0.6502104730865595483, 1.047635159188778031, 1.839821444870335165 ) ) ;
#203827 = CARTESIAN_POINT ( 'NONE',  ( 9.459838494033030898, 12.05956421450382088, 1.599625672291281386 ) ) ;
#203829 = ORIENTED_EDGE ( 'NONE', *, *, #92379, .T. ) ;
#203828 = CARTESIAN_POINT ( 'NONE',  ( 3.475000000000000533, -2.304166666666668473, 2.006292185433948827 ) ) ;
#203830 = CARTESIAN_POINT ( 'NONE',  ( 5.295788417638883416, -1.460108768623759712, -1.467927865959644862 ) ) ;
#203832 = CARTESIAN_POINT ( 'NONE',  ( -1.402160292154681736E-14, 2.009375000341422801, -1.575800808251660134 ) ) ;
#203831 = CARTESIAN_POINT ( 'NONE',  ( 0.1515692981730529243, 0.7036590017722235135, 1.701685288394996665 ) ) ;
#203833 = CARTESIAN_POINT ( 'NONE',  ( 5.379591378607442742, -0.5557209876673010474, -2.230391596181950042 ) ) ;
#203834 = CARTESIAN_POINT ( 'NONE',  ( 6.317736394288135493, 8.393778431468064127, 1.443375672974076540 ) ) ;
#203836 = DIRECTION ( 'NONE',  ( -0.000000000000000000, 1.000000000000000000, -0.000000000000000000 ) ) ;
#203835 = CARTESIAN_POINT ( 'NONE',  ( 4.584065335196260804, 6.441438539186039591, 1.443375672974065660 ) ) ;
#203837 = CARTESIAN_POINT ( 'NONE',  ( 1.887097267728707894, 1.992918150068530014, -1.132464722766779675 ) ) ;
#203838 = CARTESIAN_POINT ( 'NONE',  ( 7.550983558724411182, -6.148216694138056937, -7.550983558724436051 ) ) ;
#203839 = CARTESIAN_POINT ( 'NONE',  ( -5.738844160334429567, 9.917344963690652548, 0.000000000000000000 ) ) ;
#203840 = CARTESIAN_POINT ( 'NONE',  ( 5.419850138435895914, 1.155063568626579995, -1.560950513000541662 ) ) ;
#203841 = EDGE_LOOP ( 'NONE', ( #204035, #186901, #207422, #45858, #14339, #197827, #198217, #89840 ) ) ;
#203842 = CARTESIAN_POINT ( 'NONE',  ( 8.283668667825342169, 9.726996869626816533, -1.082531754730543083 ) ) ;
#203843 = EDGE_CURVE ( 'NONE', #141526, #185203, #35499, .T. ) ;
#203844 = ORIENTED_EDGE ( 'NONE', *, *, #186883, .F. ) ;
#203845 = CARTESIAN_POINT ( 'NONE',  ( -0.1403655429255863119, -1.558841978801903894, -1.273620833657141072 ) ) ;
#203846 = B_SPLINE_CURVE_WITH_KNOTS ( 'NONE', 3,
 ( #204490, #138468, #89731, #155779, #7364, #73441, #8441, #74529, #205571, #90792, #40975, #107086, #189336, #173108, #123369, #156856, #24688, #57209, #80327, #199383, #182070, #196221, #16368, #117152, #49961, #130227, #112903, #113974, #64084 ),
 .UNSPECIFIED., .F., .F.,
 ( 4, 2, 2, 2, 2, 2, 2, 2, 2, 2, 2, 1, 1, 1, 2, 4 ),
 ( 0.3664058785177394806, 0.3808373650965696244, 0.3952688516753998238, 0.4097003382542300232, 0.4241318248330601670, 0.4385633114118903109, 0.4457790547013054105, 0.4529947979907205102, 0.4674262845695507096, 0.4746420278589658093, 0.4782498995036733036, 0.4800538353260270785, 0.4809558032372039382, 0.4814067871927923403, 0.4816322791705865969, 0.4818577711483807979 ),
 .UNSPECIFIED. ) ;
#203847 = CARTESIAN_POINT ( 'NONE',  ( 5.911342272548039567, -1.897112096406332382, 0.6839327336411114011 ) ) ;
#203849 = CARTESIAN_POINT ( 'NONE',  ( 11.06297021485807264, 12.34330698512527569, 0.9089447062504968367 ) ) ;
#203848 = CARTESIAN_POINT ( 'NONE',  ( -8.829384350997580455, 11.32403438096243775, 1.599625672291269396 ) ) ;
#203850 = CARTESIAN_POINT ( 'NONE',  ( 1.642778471875001811, -1.130208332855375808, 2.845375778867859751 ) ) ;
#203852 = CARTESIAN_POINT ( 'NONE',  ( 0.8832604684265840111, 1.184483277375179666, 1.315230855816750921 ) ) ;
#203851 = CARTESIAN_POINT ( 'NONE',  ( 2.906283313408718705, 1.513773858955402618, -1.442204806208322809 ) ) ;
#203853 = FACE_OUTER_BOUND ( 'NONE', #160516, .T. ) ;
#203855 = CARTESIAN_POINT ( 'NONE',  ( 4.418134799529137346, 1.412088972526281072, -1.805610035947482039 ) ) ;
#203854 = CARTESIAN_POINT ( 'NONE',  ( 2.911969131885072670, 6.619324097166378706, 0.000000000000000000 ) ) ;
#203856 = CARTESIAN_POINT ( 'NONE',  ( 2.642201187982503363, -1.446964261146063802, 0.9666251106823405825 ) ) ;
#203857 = CARTESIAN_POINT ( 'NONE',  ( 4.864678189204997949, 4.569879397027603929, 0.7998128361456341429 ) ) ;
#203858 = AXIS2_PLACEMENT_3D ( 'NONE', #121754, #89189, #188799 ) ;
#203859 = CARTESIAN_POINT ( 'NONE',  ( -4.891620403477875634, 4.880467829835995808, -0.5985276763357317842 ) ) ;
#203860 = CARTESIAN_POINT ( 'NONE',  ( 2.038076752987047602, 1.660595340560795607, -0.4986328326925906773 ) ) ;
#203861 = CARTESIAN_POINT ( 'NONE',  ( 2.084662720398474001, 1.251192046665784208, -1.774223565721672724 ) ) ;
#203862 = CARTESIAN_POINT ( 'NONE',  ( 5.880485940025228508, 7.883652901494672349, 1.599625672291267398 ) ) ;
#203863 = CARTESIAN_POINT ( 'NONE',  ( 4.575407832915947104, 1.497500392235491029, 1.350737390116145242 ) ) ;
#203864 = CARTESIAN_POINT ( 'NONE',  ( 2.937500000000001776, 1.451031289060998430, -1.451031289061236018 ) ) ;
#203865 = B_SPLINE_CURVE_WITH_KNOTS ( 'NONE', 3,
 ( #176074, #114079, #66272, #213595, #180070, #212548, #125263, #47963, #32743, #16469, #159806, #31694, #42887 ),
 .UNSPECIFIED., .F., .F.,
 ( 4, 3, 3, 3, 4 ),
 ( 1.011944969444384544E-17, 3.127682647416726467E-05, 7.184504844521671105E-05, 0.0001122487170298541655, 0.0001140435926658500367 ),
 .UNSPECIFIED. ) ;
#203866 = CARTESIAN_POINT ( 'NONE',  ( 1.499999999999989120, 3.285416667349486897, 0.8660254037844524744 ) ) ;
#203867 = CARTESIAN_POINT ( 'NONE',  ( 0.6746739519505640104, -1.812841073067989361, -0.6519485973254712796 ) ) ;
#203868 = CARTESIAN_POINT ( 'NONE',  ( -1.364683531250000748, 13.85937500034140157, 0.000000000000000000 ) ) ;
#203869 = CARTESIAN_POINT ( 'NONE',  ( 5.080443840416010381, 1.095562506470529884, 1.932424796230156616 ) ) ;
#203870 = ORIENTED_EDGE ( 'NONE', *, *, #52880, .T. ) ;
#203871 = CARTESIAN_POINT ( 'NONE',  ( -0.1110810684433141682, 4.095429159110416606, -2.351882046268341409 ) ) ;
#203872 = CARTESIAN_POINT ( 'NONE',  ( -1.402160292154681736E-14, 0.5875000000000220046, -1.732050807568863648 ) ) ;
#203873 = CARTESIAN_POINT ( 'NONE',  ( 7.100719765255169236, 9.307259030929609267, -1.599625672291262513 ) ) ;
#203874 = CARTESIAN_POINT ( 'NONE',  ( 6.453317929980448397, 6.631218461173066459, 1.040834085586084257E-14 ) ) ;
#203875 = CARTESIAN_POINT ( 'NONE',  ( 1.642778471875000035, -1.976041666188709689, -2.845375778867859751 ) ) ;
#203876 = CARTESIAN_POINT ( 'NONE',  ( 0.5928132819080602633, -1.229099697874297181, 1.850090981381287358 ) ) ;
#203877 = CARTESIAN_POINT ( 'NONE',  ( 5.476992472119650124, 1.812042599547862176, 0.7524171098330990626 ) ) ;
#203878 = CARTESIAN_POINT ( 'NONE',  ( 9.951321562750607086, 11.67259191370631477, -1.082531754730537088 ) ) ;
#203879 = STYLED_ITEM ( 'NONE', ( #26228 ), #9068 ) ;
#203880 = CARTESIAN_POINT ( 'NONE',  ( -1.435158330144267635, 4.071532573434739177, -0.4529249069356953150 ) ) ;
#203881 = CARTESIAN_POINT ( 'NONE',  ( 6.485631321617453260, 1.553040037441177690, 1.645414220380213788 ) ) ;
#203882 = CARTESIAN_POINT ( 'NONE',  ( -5.492461627311929995, 5.580495784718250363, 0.000000000000000000 ) ) ;
#203883 = CARTESIAN_POINT ( 'NONE',  ( 3.262228214153365169, -2.060424958539575524, 0.09861793142403557644 ) ) ;
#203884 = CARTESIAN_POINT ( 'NONE',  ( -5.368138756007025947, 8.350246751061767725, 1.199719254218452047 ) ) ;
#203885 = CARTESIAN_POINT ( 'NONE',  ( 1.499999999999989120, 3.035416667349485564, 0.8660254037844524744 ) ) ;
#203886 = CARTESIAN_POINT ( 'NONE',  ( 0.6823417656249917140, 5.405208333674749177, 1.181850606188765695 ) ) ;
#203887 = CARTESIAN_POINT ( 'NONE',  ( 4.780451015977909002, -1.813929833846049666, -0.4561423458772846939 ) ) ;
#203888 = CARTESIAN_POINT ( 'NONE',  ( 3.375360373764887179, -0.3420621250952958214, -1.699858368971490563 ) ) ;
#203889 = CARTESIAN_POINT ( 'NONE',  ( 3.737644501653397455, 1.732476483319781657, 0.1661042753308156761 ) ) ;
#203890 = CARTESIAN_POINT ( 'NONE',  ( 0.4512259348973605699, -1.940755322566484642, -1.219765617878470376 ) ) ;
#203891 = CARTESIAN_POINT ( 'NONE',  ( -1.201851678989727383E-14, 3.884375000341423689, 1.575800808251672791 ) ) ;
#203892 = CARTESIAN_POINT ( 'NONE',  ( 4.687105897418362588, 1.550225779131916726, 1.403071992899749931 ) ) ;
#203893 = CARTESIAN_POINT ( 'NONE',  ( 0.3570341529223716726, 1.821527202347131169, -0.2672101559373847857 ) ) ;
#203895 = VERTEX_POINT ( 'NONE', #70116 ) ;
#203894 = CARTESIAN_POINT ( 'NONE',  ( 0.1007326007325774070, -9.920000000000095852, 10.99953876047307944 ) ) ;
#203896 = CARTESIAN_POINT ( 'NONE',  ( 0.3873425458618062200, -0.6819987885887256462, -1.897696807414723796 ) ) ;
#203897 = ADVANCED_FACE ( 'NONE', ( #1912 ), #137302, .F. ) ;
#203898 = CARTESIAN_POINT ( 'NONE',  ( 0.7738737444688469358, 0.4079195088417563730, -2.080830740624163955 ) ) ;
#203899 = CARTESIAN_POINT ( 'NONE',  ( 6.604150280000163242, -0.1430408514614608939, 1.983920101186954721 ) ) ;
#203900 = CARTESIAN_POINT ( 'NONE',  ( -7.557780564614042795, 10.90482886110335414, -1.199719254218446718 ) ) ;
#203901 = CARTESIAN_POINT ( 'NONE',  ( 6.518772930072240790, 6.499656594706071822, -0.7998128361456281477 ) ) ;
#203902 = CARTESIAN_POINT ( 'NONE',  ( 2.209781436637091367, 1.640924847721588975, 1.343087772177023353 ) ) ;
#203903 = CARTESIAN_POINT ( 'NONE',  ( 1.109591582173274693, -4.250299932362443300, -0.07813100402512697384 ) ) ;
#203904 = CARTESIAN_POINT ( 'NONE',  ( 4.336427269025699971, 1.790907886515300085, 0.3537760332646966432 ) ) ;
#203905 = ORIENTED_EDGE ( 'NONE', *, *, #80012, .F. ) ;
#203906 = CARTESIAN_POINT ( 'NONE',  ( -8.120407659942227241, 8.438506789546210030, 0.7998128361456341429 ) ) ;
#203907 = CARTESIAN_POINT ( 'NONE',  ( -0.1520312049661516063, -8.104757123234351823, -9.499050059654539524 ) ) ;
#203908 = CARTESIAN_POINT ( 'NONE',  ( -3.285556943750000070, -0.5468749995220407722, 0.000000000000000000 ) ) ;
#203909 = CARTESIAN_POINT ( 'NONE',  ( -6.181627972826976958, 9.299317504018391745, 1.199719254218452047 ) ) ;
#203910 = CARTESIAN_POINT ( 'NONE',  ( 1.828384590600404591, -0.9557513975326953348, -1.779375440769872752 ) ) ;
#203911 = CARTESIAN_POINT ( 'NONE',  ( 5.965903178300210108, 2.175115270774199416, -0.3715683035191638117 ) ) ;
#203912 = CARTESIAN_POINT ( 'NONE',  ( -3.311934663488232733, 7.085950550703385531, -0.7998128361456481317 ) ) ;
#203913 = CARTESIAN_POINT ( 'NONE',  ( 4.240933880512650411, -0.1787712432332102808, -1.852300418306342955 ) ) ;
#203914 = CARTESIAN_POINT ( 'NONE',  ( 9.541187415715040032, 12.15447128979948310, -1.599625672291262513 ) ) ;
#203915 = CARTESIAN_POINT ( 'NONE',  ( 10.56514123924917392, 12.34108045521194263, -3.404988257269842222 ) ) ;
#203916 = CARTESIAN_POINT ( 'NONE',  ( -5.590039407536138150, 5.416134151747256986, 0.000000000000000000 ) ) ;
#203917 = CARTESIAN_POINT ( 'NONE',  ( -9.969323024750229578, 10.52529837183042716, -0.7998128361456291469 ) ) ;
#203918 = CARTESIAN_POINT ( 'NONE',  ( 5.232948167349782409, 0.1380416123818763163, 1.820529236867339584 ) ) ;
#203920 = CARTESIAN_POINT ( 'NONE',  ( -4.662544117754887196, 7.086110115384146368, -1.393066284953614620 ) ) ;
#203919 = CARTESIAN_POINT ( 'NONE',  ( -4.787964524281469458, 5.614988695530339413, -1.199719254218453823 ) ) ;
#203921 = CARTESIAN_POINT ( 'NONE',  ( 0.6823417656249882723, -1.157291666325249713, 1.181850606188755259 ) ) ;
#203922 = CARTESIAN_POINT ( 'NONE',  ( 0.2625146791020065984, -1.733275965524210482, -0.05152637578398518159 ) ) ;
#203923 = CARTESIAN_POINT ( 'NONE',  ( 6.580030785786400216, -1.806642183828395920, -0.3538341520857649081 ) ) ;
#203924 = CARTESIAN_POINT ( 'NONE',  ( 5.496783081331708232, -0.5556612750647730303, -2.239684525637525514 ) ) ;
#203925 = CARTESIAN_POINT ( 'NONE',  ( 5.041653019435334393, 6.975290837464928728, -1.599625672291269396 ) ) ;
#203926 = CARTESIAN_POINT ( 'NONE',  ( 1.581398767000765426, 1.905217558097069386, -0.7859657096468860571 ) ) ;
#203927 = CARTESIAN_POINT ( 'NONE',  ( 6.114890974963323345, 7.092793211334054604, 1.199719254218462483 ) ) ;
#203928 = CARTESIAN_POINT ( 'NONE',  ( 6.345094440775825184, -1.237889906630392334, 1.936425090000978289 ) ) ;
#203929 = CARTESIAN_POINT ( 'NONE',  ( -2.176944501978025137, -3.232243495192087313, 2.478859588741756603 ) ) ;
#203930 = CARTESIAN_POINT ( 'NONE',  ( -6.017840079619296567, 8.114175741012878973, -1.599625672291271394 ) ) ;
#203931 = CARTESIAN_POINT ( 'NONE',  ( 5.928550619183988957, 1.803260976426118489, 0.4972845834502263584 ) ) ;
#203933 = CARTESIAN_POINT ( 'NONE',  ( -3.634467696915153034, 6.397906858779740524, 1.199719254218452935 ) ) ;
#203932 = CARTESIAN_POINT ( 'NONE',  ( 4.078302138561982204, 0.9061299177482335931, 1.684124486321957104 ) ) ;
#203934 = CARTESIAN_POINT ( 'NONE',  ( 5.110101661328442901, -2.196521081226535443, 0.2136625748923453583 ) ) ;
#203935 = CARTESIAN_POINT ( 'NONE',  ( -5.157946788997579689E-14, 1.250000000682857992, -1.414508159514609620 ) ) ;
#203936 = EDGE_CURVE ( 'NONE', #109340, #117810, #187086, .T. ) ;
#203937 = CARTESIAN_POINT ( 'NONE',  ( 3.716343503477301802, 7.349834830783237294, -1.734723475976807094E-15 ) ) ;
#203938 = CARTESIAN_POINT ( 'NONE',  ( -5.953438849732214599, 6.118302544208584770, 0.7216878364870257245 ) ) ;
#203939 = CARTESIAN_POINT ( 'NONE',  ( 5.672555391165950311, 0.8593836824349295744, 1.938725756316476589 ) ) ;
#203940 = CARTESIAN_POINT ( 'NONE',  ( 2.573609363736366618, 0.1136701668994527237, -2.304911326000145699 ) ) ;
#203941 = CARTESIAN_POINT ( 'NONE',  ( 3.490630252122446375, 1.913478943654752129, 0.4322817992908413176 ) ) ;
#203942 = CARTESIAN_POINT ( 'NONE',  ( -6.310394152517828203, 6.326824364217715768, 0.7998128361456282587 ) ) ;
#203943 = CARTESIAN_POINT ( 'NONE',  ( 0.2858946156298440844, -1.202361161835348025, -1.550730028719159215 ) ) ;
#203944 = CARTESIAN_POINT ( 'NONE',  ( 3.226477370372305753, 4.787309570232886280, 1.443375672974062551 ) ) ;
#203945 = CARTESIAN_POINT ( 'NONE',  ( 5.090160327287878594, 4.903218234782778850, -0.7998128361456481317 ) ) ;
#203946 = ORIENTED_EDGE ( 'NONE', *, *, #205068, .T. ) ;
#203947 = CARTESIAN_POINT ( 'NONE',  ( 6.069546051295945155, 1.394081536189460069, 1.457239770841619597 ) ) ;
#203948 = CARTESIAN_POINT ( 'NONE',  ( -10.29471871147821282, 10.90492667301307605, -0.7998128361456291469 ) ) ;
#203949 = CARTESIAN_POINT ( 'NONE',  ( 1.841222038795635206E-16, 0.000000000000000000, 2.750000000000000000 ) ) ;
#203950 = CARTESIAN_POINT ( 'NONE',  ( 3.045941508711128787, 1.532170317875800603, 1.538426465386952380 ) ) ;
#203951 = CARTESIAN_POINT ( 'NONE',  ( 0.000000000000000000, 6.999999999999992006, -4.500000000000000000 ) ) ;
#203953 = EDGE_CURVE ( 'NONE', #40273, #159908, #75539, .T. ) ;
#203952 = CARTESIAN_POINT ( 'NONE',  ( 1.178162429063234207, 2.088287186665960693, -0.3679680078583212333 ) ) ;
#203954 = CARTESIAN_POINT ( 'NONE',  ( -1.402160292154681736E-14, 1.618750000682814827, -1.732050807568863648 ) ) ;
#203955 = CARTESIAN_POINT ( 'NONE',  ( 9.083072846151447166, 12.68433652289702884, 1.199719254218450271 ) ) ;
#203956 = CARTESIAN_POINT ( 'NONE',  ( 0.000000000000000000, 9.799999999999998934, 0.000000000000000000 ) ) ;
#203957 = CARTESIAN_POINT ( 'NONE',  ( 5.355371708033295874, 7.701368364266228284, 1.317571137710125351 ) ) ;
#203958 = CARTESIAN_POINT ( 'NONE',  ( 0.6849272659917711170, -0.2494827685093256309, -2.045528899044207982 ) ) ;
#203960 = CARTESIAN_POINT ( 'NONE',  ( 1.499999999999996891, 8.427083334016131744, -0.8660254037844378194 ) ) ;
#203959 = DIRECTION ( 'NONE',  ( -1.207943261119674327E-30, -2.168404344971008079E-15, -1.000000000000000000 ) ) ;
#203961 = CARTESIAN_POINT ( 'NONE',  ( -0.6823417656250003738, 0.4677083336747517306, -1.181850606188749264 ) ) ;
#203962 = DIRECTION ( 'NONE',  ( 0.2553790820074260948, 0.9650728656995758437, 0.05844560174600864355 ) ) ;
#203963 = ORIENTED_EDGE ( 'NONE', *, *, #99218, .F. ) ;
#203964 = CARTESIAN_POINT ( 'NONE',  ( 3.316961667764028121, 1.505919282548912719, -1.178437403786938731 ) ) ;
#203965 =( GEOMETRIC_REPRESENTATION_CONTEXT ( 3 ) GLOBAL_UNCERTAINTY_ASSIGNED_CONTEXT ( ( #89665 ) ) GLOBAL_UNIT_ASSIGNED_CONTEXT ( ( #88563, #72270, #157831 ) ) REPRESENTATION_CONTEXT ( 'NONE', 'WORKASPACE' ) );
#203966 = CARTESIAN_POINT ( 'NONE',  ( 5.647242114940491220, -1.397150190615953358, -1.086277386216354168 ) ) ;
#203967 = CARTESIAN_POINT ( 'NONE',  ( 5.352436782344940802, 9.466536356036257871, 0.000000000000000000 ) ) ;
#203968 = CARTESIAN_POINT ( 'NONE',  ( -3.255929445576174697, 6.950334786480840243, -0.7998128361456281477 ) ) ;
#203969 = CARTESIAN_POINT ( 'NONE',  ( 0.3865838573892222962, -1.705918499434391444, -0.6100900862041622741 ) ) ;
#203970 = CARTESIAN_POINT ( 'NONE',  ( 0.9189787140968961321, -1.730522700298501304, 0.8221016984403562988 ) ) ;
#203971 = CARTESIAN_POINT ( 'NONE',  ( 1.873570696236816158, -0.2555354716398828274, 2.054483085851127377 ) ) ;
#203972 = CARTESIAN_POINT ( 'NONE',  ( 0.6823417656249882723, 0.2385416670080825474, -1.181850606188749264 ) ) ;
#203973 = CARTESIAN_POINT ( 'NONE',  ( 6.684453402082996654, -1.835023323784425564, -0.3624468955198830722 ) ) ;
#203974 = CARTESIAN_POINT ( 'NONE',  ( 3.176193443437186126, -1.086901434622984830, 1.466744820640853098 ) ) ;
#203976 = CARTESIAN_POINT ( 'NONE',  ( 6.484283628081795037, 6.752753718119230975, 0.1579380340677779548 ) ) ;
#203975 = CARTESIAN_POINT ( 'NONE',  ( 6.691986956589398794, -0.9478133180038283978, 1.990996264204819122 ) ) ;
#203977 = CARTESIAN_POINT ( 'NONE',  ( -0.6823417656250246877, 0.05104166700808931978, 1.181850606188755259 ) ) ;
#203978 = CARTESIAN_POINT ( 'NONE',  ( 4.053227687556320014, 1.744102858319864113, -1.100964799198749455 ) ) ;
#203979 = CARTESIAN_POINT ( 'NONE',  ( -7.172426956829277778, 8.326585190177668849, -1.199719254218452935 ) ) ;
#203980 = CARTESIAN_POINT ( 'NONE',  ( 9.402743226277308963, 10.92862083786708816, -1.199719254218446718 ) ) ;
#203981 = CARTESIAN_POINT ( 'NONE',  ( 5.138703914779377158, 5.953908307786102583, 1.199719254218462483 ) ) ;
#203982 = EDGE_CURVE ( 'NONE', #97098, #205382, #189784, .T. ) ;
#203983 = CARTESIAN_POINT ( 'NONE',  ( 0.3862812426984676972, -1.019270635400490121, 1.906220128828392646 ) ) ;
#203984 = CARTESIAN_POINT ( 'NONE',  ( 6.514133371570012265, 2.065101995627930620, -0.1482383472809906122 ) ) ;
#203985 = CARTESIAN_POINT ( 'NONE',  ( 1.364683531249988757, 1.446875000341421469, 0.000000000000000000 ) ) ;
#203986 = CARTESIAN_POINT ( 'NONE',  ( 4.253314833958360630, -1.794556715717060769, -1.204719293387515489 ) ) ;
#203987 = CARTESIAN_POINT ( 'NONE',  ( 3.809243936906735239, 1.705047127353828351, -1.082240749027115978 ) ) ;
#203990 = CARTESIAN_POINT ( 'NONE',  ( 7.144783764721768904, 7.437928601704619780, 1.040834085586084257E-14 ) ) ;
#203989 = CARTESIAN_POINT ( 'NONE',  ( 1.642778471875000035, -3.026041666188708401, -2.845375778867859751 ) ) ;
#203988 = DIRECTION ( 'NONE',  ( 0.000000000000000000, -1.000000000000000000, 0.000000000000000000 ) ) ;
#203991 = CARTESIAN_POINT ( 'NONE',  ( -6.143779885648060102, 7.196773283791382703, 1.199719254218452047 ) ) ;
#203992 = CARTESIAN_POINT ( 'NONE',  ( 3.010954138651841916, 0.05432569772663429358, 2.015980714967258614 ) ) ;
#203993 = CARTESIAN_POINT ( 'NONE',  ( -8.376239975144482486, 8.666701480623698828, 1.040834085586084257E-14 ) ) ;
#203994 = CARTESIAN_POINT ( 'NONE',  ( -5.590039407536138150, 5.416134151747256986, 0.000000000000000000 ) ) ;
#203995 = CARTESIAN_POINT ( 'NONE',  ( 5.192409643909512873, 6.120528008391641350, -1.082531754730549078 ) ) ;
#203996 = CARTESIAN_POINT ( 'NONE',  ( 5.291234991620993533, -0.05314252713351996088, -1.911838368980276703 ) ) ;
#203997 = CARTESIAN_POINT ( 'NONE',  ( -3.440018289565379028, 5.036440642624797626, 1.599625672291267398 ) ) ;
#203998 = CARTESIAN_POINT ( 'NONE',  ( 5.965224399888476192, 6.061776009399090448, 1.040834085586084257E-14 ) ) ;
#204000 = CARTESIAN_POINT ( 'NONE',  ( 4.323842328482737862, 0.8596156136044874607, -1.824127480631778653 ) ) ;
#203999 = CARTESIAN_POINT ( 'NONE',  ( -7.321039761255057066, 11.48503745486550365, 0.000000000000000000 ) ) ;
#204001 = CARTESIAN_POINT ( 'NONE',  ( -0.7500000000000215383, 4.191666666666690411, 1.299038105676671107 ) ) ;
#204002 = CARTESIAN_POINT ( 'NONE',  ( -1.402160292154681736E-14, 14.48437500034139980, 1.575800808251682339 ) ) ;
#204003 = CARTESIAN_POINT ( 'NONE',  ( 0.04690384546136848465, -1.329360633743952746, -1.098954345569080893 ) ) ;
#204004 = CARTESIAN_POINT ( 'NONE',  ( 5.712781623311797397, 7.758274208654143855, -1.599625672291283607 ) ) ;
#204005 = CARTESIAN_POINT ( 'NONE',  ( 7.293923454472069245, 11.45340176361870199, 0.7216878364870438212 ) ) ;
#204006 = CONICAL_SURFACE ( 'NONE', #169406, 7.034482758620711706, 0.8621700546672336207 ) ;
#204007 = CARTESIAN_POINT ( 'NONE',  ( 6.717278222822382183, 7.849261790823902629, -6.830415307812251591 ) ) ;
#204008 = CARTESIAN_POINT ( 'NONE',  ( 5.395714598229544023, -0.6742385858747660388, 1.744967798948720228 ) ) ;
#204009 = CARTESIAN_POINT ( 'NONE',  ( 5.924093355334532518, -1.997480882691978987, 0.2508417921044738819 ) ) ;
#204010 = CARTESIAN_POINT ( 'NONE',  ( 0.000000000000000000, 2.000000000000001776, 0.000000000000000000 ) ) ;
#204011 = CARTESIAN_POINT ( 'NONE',  ( 2.079047829753433163, 1.930162853665925216, 0.7490395704240898622 ) ) ;
#204012 = DIRECTION ( 'NONE',  ( 0.000000000000000000, 8.546850786086437571E-32, 1.000000000000000000 ) ) ;
#204013 = VERTEX_POINT ( 'NONE', #138364 ) ;
#204014 = CARTESIAN_POINT ( 'NONE',  ( 8.554831740098642001, 12.92446143018304916, 0.7216878364870438212 ) ) ;
#204015 = CARTESIAN_POINT ( 'NONE',  ( 0.6500178175347062215, 0.9963223104369985927, 1.753020061881369829 ) ) ;
#204016 = CARTESIAN_POINT ( 'NONE',  ( 1.019438801881300316, -0.4388897500222695425, 1.757493349343726585 ) ) ;
#204017 = CARTESIAN_POINT ( 'NONE',  ( 5.519577934094864524, 5.612131475965050242, 0.7216878364870328300 ) ) ;
#204018 = DIRECTION ( 'NONE',  ( -0.000000000000000000, -1.000000000000000000, -0.000000000000000000 ) ) ;
#204019 = CARTESIAN_POINT ( 'NONE',  ( 8.101160479365381306, 9.410107633136481908, -1.199719254218446718 ) ) ;
#204021 = CARTESIAN_POINT ( 'NONE',  ( 6.028903631427566800, -1.615475894945080926, 1.029159534634891626 ) ) ;
#204020 = CARTESIAN_POINT ( 'NONE',  ( -5.585069213825653023, 8.603332285183535433, -1.199719254218440723 ) ) ;
#204022 = CARTESIAN_POINT ( 'NONE',  ( 3.714570900464274850, 6.317121236308204324, 1.082531754730558626 ) ) ;
#204023 = CARTESIAN_POINT ( 'NONE',  ( 11.86145016429273191, 12.69999999999999929, -1.180000000000000604 ) ) ;
#204024 = CARTESIAN_POINT ( 'NONE',  ( -3.619663825168619731, 7.166765529431275539, 1.040834085586084257E-14 ) ) ;
#204026 = VERTEX_POINT ( 'NONE', #186010 ) ;
#204025 = CARTESIAN_POINT ( 'NONE',  ( 3.877268743828266029, 6.506935386899531437, 1.082531754730558626 ) ) ;
#204027 = CARTESIAN_POINT ( 'NONE',  ( -8.853111120043687166, 9.430977182913531820, 1.040834085586084257E-14 ) ) ;
#204028 = CARTESIAN_POINT ( 'NONE',  ( 3.274459119871219848, -1.289031633699177171, 1.735169069618908599 ) ) ;
#204029 = CARTESIAN_POINT ( 'NONE',  ( -5.465345320084574965, 9.390336950158399532, 0.000000000000000000 ) ) ;
#204030 = CARTESIAN_POINT ( 'NONE',  ( 7.349928672384120176, 7.747540670635879145, 0.7216878364870267237 ) ) ;
#204031 = CARTESIAN_POINT ( 'NONE',  ( 0.3695850531008069706, -1.794773754367712693, -1.129184308951653781 ) ) ;
#204032 = CARTESIAN_POINT ( 'NONE',  ( 6.264658373536383884, -1.288822541704701230, 1.293195164663100361 ) ) ;
#204033 = CARTESIAN_POINT ( 'NONE',  ( 2.178924785135676334, -0.09298872875643586500, -1.969266502737290425 ) ) ;
#204034 = CARTESIAN_POINT ( 'NONE',  ( 5.045129621168108258, 0.1466893748028277877, 1.906852434080000824 ) ) ;
#204035 = ORIENTED_EDGE ( 'NONE', *, *, #131165, .T. ) ;
#204036 = CARTESIAN_POINT ( 'NONE',  ( -8.784791485860443672, 14.48107303905707255, -8.187053764137555589 ) ) ;
#204037 = CARTESIAN_POINT ( 'NONE',  ( 4.527769023902194157, 1.910916496070225179, -0.4765158004534468805 ) ) ;
#204038 = CARTESIAN_POINT ( 'NONE',  ( 6.614805133705309537, -0.1285734799129842065, 1.912263277720785970 ) ) ;
#204039 = ORIENTED_EDGE ( 'NONE', *, *, #192235, .T. ) ;
#204040 = CARTESIAN_POINT ( 'NONE',  ( -5.635349125135588721, 6.603604063193491136, 1.199719254218452935 ) ) ;
#204041 = CARTESIAN_POINT ( 'NONE',  ( -7.485510208520816278, 8.866088343763324886, 1.082531754730549078 ) ) ;
#204043 = CARTESIAN_POINT ( 'NONE',  ( 6.549997608733495902, 7.774656977344789333, -1.082531754730548412 ) ) ;
#204042 = CARTESIAN_POINT ( 'NONE',  ( 8.067265095331215718, 9.370563018429956870, 1.199719254218462483 ) ) ;
#204045 = ORIENTED_EDGE ( 'NONE', *, *, #79889, .T. ) ;
#204044 = CARTESIAN_POINT ( 'NONE',  ( 5.479139036522528983, -1.730609802697373079, -0.8137914003483390779 ) ) ;
#204046 = CARTESIAN_POINT ( 'NONE',  ( 0.7982362974770088604, -0.7925503509537080715, 2.059710425106767939 ) ) ;
#204047 = CARTESIAN_POINT ( 'NONE',  ( 9.452508394161709404, 3.481540833006149249, -7.393820799723212822 ) ) ;
#204048 = CARTESIAN_POINT ( 'NONE',  ( 5.795569859559966730, 1.859138327062941132, -0.7725605513991992135 ) ) ;
#204049 = CARTESIAN_POINT ( 'NONE',  ( 0.07661050522435489119, 2.064768137775649048, -2.128874817076317871 ) ) ;
#204050 = CYLINDRICAL_SURFACE ( 'NONE', #176933, 0.08000000000000020983 ) ;
#204051 = CARTESIAN_POINT ( 'NONE',  ( -1.786765180256111307E-13, 7.629137130509076492, -2.599999999999921929 ) ) ;
#204052 = CARTESIAN_POINT ( 'NONE',  ( 2.576698201331685922, 1.354182300986291887, -1.566139152919379329 ) ) ;
#204053 = CARTESIAN_POINT ( 'NONE',  ( -5.391338639728555648, 9.441645512991978961, -0.7998128361456231517 ) ) ;
#204054 = CARTESIAN_POINT ( 'NONE',  ( -4.900660301121059881, 8.037431844279481652, -0.9627648694432132670 ) ) ;
#204056 = CARTESIAN_POINT ( 'NONE',  ( 0.8839147992780393981, 1.452536163361785260, 1.601146772000871188 ) ) ;
#204055 = CARTESIAN_POINT ( 'NONE',  ( -6.078132937628113908, 5.985576603521232109, 1.040834085586084257E-14 ) ) ;
#204057 = CARTESIAN_POINT ( 'NONE',  ( -11.15646993939951059, 7.316272439152442963, -4.426198049908277810 ) ) ;
#204058 = CARTESIAN_POINT ( 'NONE',  ( 4.584065335196260804, 6.441438539186039591, 1.443375672974065660 ) ) ;
#204059 = CARTESIAN_POINT ( 'NONE',  ( 8.043940816608021294, -6.893137084989709784, -7.503508839934921681 ) ) ;
#204060 = EDGE_CURVE ( 'NONE', #125323, #177320, #120606, .T. ) ;
#204061 = CARTESIAN_POINT ( 'NONE',  ( -1.364683531250000748, 13.42187500034139980, 0.000000000000000000 ) ) ;
#204063 = CARTESIAN_POINT ( 'NONE',  ( -6.818824913030298696, 6.919993584815607335, 0.7998128361456341429 ) ) ;
#204062 = CARTESIAN_POINT ( 'NONE',  ( 6.825078400183545391, 0.005516643811322509937, 1.755566376062764222 ) ) ;
#204064 = CARTESIAN_POINT ( 'NONE',  ( 4.394945383863869459, -0.7467295182301251222, -1.565304230221546300 ) ) ;
#204065 = CARTESIAN_POINT ( 'NONE',  ( -3.307299406729781399, 5.945934176904983381, -1.199719254218452935 ) ) ;
#204066 = CARTESIAN_POINT ( 'NONE',  ( 2.799741537105740363, -1.531010120401912200, -1.393694001666223814 ) ) ;
#204067 = CARTESIAN_POINT ( 'NONE',  ( 4.499685226448436381, -2.076086866053193258, 0.4145649545581850393 ) ) ;
#204068 = CARTESIAN_POINT ( 'NONE',  ( 6.693975156845185737, 8.832723654451292816, 1.599625672291281386 ) ) ;
#204069 = CARTESIAN_POINT ( 'NONE',  ( 0.08246874231330963978, -9.908734156519555469, 10.99969088041220999 ) ) ;
#204070 = CARTESIAN_POINT ( 'NONE',  ( 1.780066195911081284, -1.089727156841081346, -1.640273131265007844 ) ) ;
#204071 = CARTESIAN_POINT ( 'NONE',  ( 6.046415161660691595, 6.058605959254545148, 0.4744590674741564484 ) ) ;
#204072 = CARTESIAN_POINT ( 'NONE',  ( 1.125099709691119276, 1.687896996356451629, 0.8989547360247207575 ) ) ;
#204073 = CARTESIAN_POINT ( 'NONE',  ( 5.121132688944100231, -2.177879115872250360, 0.7152381750462534216 ) ) ;
#204074 = CARTESIAN_POINT ( 'NONE',  ( 1.699542765152612711, -0.6164703606487755838, 1.718597393154073671 ) ) ;
#204075 = CARTESIAN_POINT ( 'NONE',  ( 5.740951700743842423, 5.662474837148078421, -0.7998128361456481317 ) ) ;
#204076 = CARTESIAN_POINT ( 'NONE',  ( 5.219525951136835928, 7.112532914458205013, -1.443375672974051449 ) ) ;
#204077 = CARTESIAN_POINT ( 'NONE',  ( -8.667740277838301921, 9.006785167099828016, -0.7998128361456291469 ) ) ;
#204078 = CARTESIAN_POINT ( 'NONE',  ( 3.181892525975566155, 1.963218260121324166, -0.4451317699624996460 ) ) ;
#204079 = CARTESIAN_POINT ( 'NONE',  ( 3.573055779259231457, 1.771592698278463107, 0.8429337356923997104 ) ) ;
#204080 = CARTESIAN_POINT ( 'NONE',  ( -7.160677686311960777, 11.50587440067263678, -0.7998128361456291469 ) ) ;
#204081 = CARTESIAN_POINT ( 'NONE',  ( -5.005985031943793295, 6.863401842066301661, -1.599625672291256295 ) ) ;
#204082 = CARTESIAN_POINT ( 'NONE',  ( 0.07516593201273635838, 1.359561921253334749, -2.300590921312398951 ) ) ;
#204084 = CARTESIAN_POINT ( 'NONE',  ( 4.486996778590452983, 1.580468086399078542, -0.7966448122273452892 ) ) ;
#204083 = CARTESIAN_POINT ( 'NONE',  ( 5.683562130502735954, -0.9407222913834032418, 1.867095764824426851 ) ) ;
#204085 = CARTESIAN_POINT ( 'NONE',  ( 4.904534058535990226, 4.831883945567478911, 0.6074287960816383558 ) ) ;
#204086 = CARTESIAN_POINT ( 'NONE',  ( 1.060776890969020059, -1.982532595227912475, -0.9341070725938580566 ) ) ;
#204087 = CARTESIAN_POINT ( 'NONE',  ( -0.1239745564502250652, -0.1323307239476738673, -1.711383809018538038 ) ) ;
#204088 = CARTESIAN_POINT ( 'NONE',  ( 6.856673000209174695, 9.022537805042615489, 1.599625672291281386 ) ) ;
#204089 = CARTESIAN_POINT ( 'NONE',  ( 0.2331713839410602396, 7.629137130509072939, -2.553349835631549603 ) ) ;
#204090 = CARTESIAN_POINT ( 'NONE',  ( 5.836663081169705336, 0.6703748249779170054, -2.198801845021758350 ) ) ;
#204091 = DIRECTION ( 'NONE',  ( 0.000000000000000000, -1.000000000000000000, 0.000000000000000000 ) ) ;
#204092 = CARTESIAN_POINT ( 'NONE',  ( 5.641838915941918664, -0.04494510194943436565, -1.733422878500885167 ) ) ;
#204093 = CARTESIAN_POINT ( 'NONE',  ( 1.805583701156989518, 1.836052299496168771, 1.224139149458243425 ) ) ;
#204094 = COLOUR_RGB ( '', 0.66274510, 0.83137255, 0.94901961) ;
#204095 = CARTESIAN_POINT ( 'NONE',  ( 0.4796376738960402841, -0.1079922143863345368, 2.168524981076371372 ) ) ;
#204096 = CARTESIAN_POINT ( 'NONE',  ( -3.929058411375426108, 6.499999999999999112, 0.7499999999999988898 ) ) ;
#204097 = CARTESIAN_POINT ( 'NONE',  ( 0.9544967768389999163, -1.338301201188813572, 1.640804622059524043 ) ) ;
#204098 = CARTESIAN_POINT ( 'NONE',  ( 3.812500000000003109, 1.451031289061270213, 1.451031289060960905 ) ) ;
#204099 = CARTESIAN_POINT ( 'NONE',  ( 6.727182134110199385, 7.052145554274142469, 2.687205589382557491 ) ) ;
#204100 = CARTESIAN_POINT ( 'NONE',  ( 4.260710244665906643, -1.428042822336324846, 1.293124370783913735 ) ) ;
#204101 = CARTESIAN_POINT ( 'NONE',  ( 0.9443249964648057215, -1.413213925058560028, -1.713760899525147874 ) ) ;
#204102 = ORIENTED_EDGE ( 'NONE', *, *, #109210, .T. ) ;
#204104 = CARTESIAN_POINT ( 'NONE',  ( -0.7500000000000215383, 4.691666666666684193, 1.299038105676671107 ) ) ;
#204103 = CARTESIAN_POINT ( 'NONE',  ( 1.857357856600039048, 0.3871700131025680447, -2.259295229882941403 ) ) ;
#204105 = CARTESIAN_POINT ( 'NONE',  ( 4.147904930777053245, 6.926640621626830807, -1.199719254218452047 ) ) ;
#204106 = CARTESIAN_POINT ( 'NONE',  ( 4.333802657862601215, 8.207853534148366492, 0.7998128361456462443 ) ) ;
#204107 = CARTESIAN_POINT ( 'NONE',  ( 4.248835331960220785, 2.178490119157860061, 0.4332075398792554766 ) ) ;
#204108 = CARTESIAN_POINT ( 'NONE',  ( -7.537970219518075332, 10.77775377520434574, -1.082531754730543971 ) ) ;
#204109 = CARTESIAN_POINT ( 'NONE',  ( -1.109591582173425461, -4.250299932362596067, 0.07813100402492727248 ) ) ;
#204110 = CARTESIAN_POINT ( 'NONE',  ( 7.795575138177731844, 8.197185204069915798, 1.040834085586084257E-14 ) ) ;
#204111 = CARTESIAN_POINT ( 'NONE',  ( -8.473482818416664841, 11.86918514058604757, -1.082531754730543083 ) ) ;
#204112 = CARTESIAN_POINT ( 'NONE',  ( 7.024532985656141371, 7.367912369453226695, 0.7216878364870328300 ) ) ;
#204113 = CARTESIAN_POINT ( 'NONE',  ( 1.336564801266389990, 0.5826540126645517459, -1.930418273149013153 ) ) ;
#204115 = CARTESIAN_POINT ( 'NONE',  ( 6.355934510867760956, -0.6984221382469282258, 1.940952099462374569 ) ) ;
#204114 = CARTESIAN_POINT ( 'NONE',  ( 6.968000882419564945, 10.21675256520979858, 1.199719254218460707 ) ) ;
#204116 = SPHERICAL_SURFACE ( 'NONE', #133770, 0.08000000000000000167 ) ;
#204117 = CARTESIAN_POINT ( 'NONE',  ( 6.495764994278797388, 8.671754808115688107, 1.443375672974063439 ) ) ;
#204118 = CARTESIAN_POINT ( 'NONE',  ( 0.1339853816830008371, 0.3136495386693045062, 1.814181566856580607 ) ) ;
#204119 = CARTESIAN_POINT ( 'NONE',  ( -10.97031310326519282, 13.80000000000000071, -1.695146482106561381 ) ) ;
#204120 = CARTESIAN_POINT ( 'NONE',  ( 1.364683531249988757, 2.384375000341422357, 1.214306433183764966E-14 ) ) ;
#204121 = CARTESIAN_POINT ( 'NONE',  ( 1.668863397688532091, 0.1364744985549205814, -1.764554890378322805 ) ) ;
#204122 = CARTESIAN_POINT ( 'NONE',  ( 0.3170300144729014669, 1.034162889623980286, -1.730867746391979933 ) ) ;
#204123 = CARTESIAN_POINT ( 'NONE',  ( 6.233937787808796038, 1.722893207988238862, 0.2456954999437432341 ) ) ;
#204124 = CARTESIAN_POINT ( 'NONE',  ( 4.669621734427405357, 1.318897967798425608, 1.874777261101326920 ) ) ;
#204125 = CARTESIAN_POINT ( 'NONE',  ( 3.626748959588219634, -1.700609458330613055, 0.7059681596332522124 ) ) ;
#204126 = CARTESIAN_POINT ( 'NONE',  ( 9.206149998879153529, 10.69926207256923689, 1.199719254218453823 ) ) ;
#204127 = CARTESIAN_POINT ( 'NONE',  ( 3.311362000969253039, -0.3573404788377897989, 1.790086433339547201 ) ) ;
#204128 = CARTESIAN_POINT ( 'NONE',  ( 3.340470361411255418, 0.4872029778183216697, -1.956561305313428978 ) ) ;
#204129 = CARTESIAN_POINT ( 'NONE',  ( -10.15235809853472126, 10.73883929124566983, -0.7998128361456291469 ) ) ;
#204131 = CARTESIAN_POINT ( 'NONE',  ( -7.119966945832006289, 8.335658187339330283, 1.199719254218452047 ) ) ;
#204130 = CARTESIAN_POINT ( 'NONE',  ( 3.889755562772099662, 1.636703778197702075, 1.562332884182315196 ) ) ;
#204132 = CARTESIAN_POINT ( 'NONE',  ( 5.790091041381728587, -0.9498100376258570288, 1.879691625423451029 ) ) ;
#204133 = CARTESIAN_POINT ( 'NONE',  ( -11.88168509644349058, 13.87999999999999901, -1.685788023084331400 ) ) ;
#204134 = CARTESIAN_POINT ( 'NONE',  ( 3.525891238081061640, 2.020528833579691597, -0.4508363271973143682 ) ) ;
#204135 = CARTESIAN_POINT ( 'NONE',  ( 2.758194185376297902, 5.305311418659259814, 1.199719254218452047 ) ) ;
#204136 = CARTESIAN_POINT ( 'NONE',  ( 1.360316468750007779, 1.296875000341410455, -2.602085213965210642E-14 ) ) ;
#204137 = CARTESIAN_POINT ( 'NONE',  ( 5.285831659486547984, 2.043504495962459977, -0.5658664308652374686 ) ) ;
#204139 = CARTESIAN_POINT ( 'NONE',  ( 0.8031968939124977114, 1.574386321349549700, 1.110025428916910917 ) ) ;
#204138 = CARTESIAN_POINT ( 'NONE',  ( -9.691380875670077444, 10.20103253123691189, 0.7998128361456462443 ) ) ;
#204140 = CARTESIAN_POINT ( 'NONE',  ( -3.006876207180748217, 6.730049018344652190, -0.7998128361456481317 ) ) ;
#204141 = CARTESIAN_POINT ( 'NONE',  ( 6.842638217859555283, -1.930751226189564962, -0.3875045943893626887 ) ) ;
#204142 = CARTESIAN_POINT ( 'NONE',  ( 3.241808126998965811, 6.796210224891872542, 0.7216878364870257245 ) ) ;
#204143 = CARTESIAN_POINT ( 'NONE',  ( 5.856753424380153561, 5.998585917076054486, 0.3190708477142957245 ) ) ;
#204144 = CARTESIAN_POINT ( 'NONE',  ( -0.4393598995549214958, 2.800000000000018030, -1.361929136425236386 ) ) ;
#204145 = CARTESIAN_POINT ( 'NONE',  ( -5.251085567194491155, 5.020688004682002159, -0.7998128361456221525 ) ) ;
#204146 = CARTESIAN_POINT ( 'NONE',  ( 0.9322285317887604172, -2.165714743787349406, 0.4936765188615526712 ) ) ;
#204147 = CARTESIAN_POINT ( 'NONE',  ( 2.380028573532027458, 1.294904889207445509, 1.660730631172540495 ) ) ;
#204148 = CARTESIAN_POINT ( 'NONE',  ( -3.006876207180748217, 6.730049018344652190, -0.7998128361456481317 ) ) ;
#204149 = CARTESIAN_POINT ( 'NONE',  ( 7.401861798056875053, 10.72292363345333399, -1.199719254218441611 ) ) ;
#204150 = CARTESIAN_POINT ( 'NONE',  ( 0.1680794356360598985, -0.7909032441709142880, -1.683366987590989350 ) ) ;
#204151 = CARTESIAN_POINT ( 'NONE',  ( 7.233438648090761980, 8.397765496649418182, 1.199719254218462483 ) ) ;
#204152 =( BOUNDED_CURVE ( )  B_SPLINE_CURVE ( 2, ( #86024, #37272, #124749, #109555, #22051, #42370, #71879, #19938, #140952 ),
 .UNSPECIFIED., .F., .T. ) 
 B_SPLINE_CURVE_WITH_KNOTS ( ( 3, 2, 2, 2, 3 ),
 ( 0.6696428571428570953, 0.6726190476190476719, 0.6785714285714286031, 0.6845238095238095344, 0.6875000000000000000 ),
 .UNSPECIFIED. ) 
 CURVE ( )  GEOMETRIC_REPRESENTATION_ITEM ( )  RATIONAL_B_SPLINE_CURVE ( ( 0.9330127018922194093, 0.9330127018922180770, 1.000000000000000000, 0.8660254037844387076, 1.000000000000000000, 0.8660254037844387076, 1.000000000000000000, 0.9330127018922194093, 0.9330127018922194093 ) ) 
 REPRESENTATION_ITEM ( '' )  );
#204153 = CARTESIAN_POINT ( 'NONE',  ( 11.97302537858640115, 9.801240101919827197, 0.8111997896468206015 ) ) ;
#204154 = CARTESIAN_POINT ( 'NONE',  ( -5.478903473698241378, 9.406154796041011679, -0.7216878364870338292 ) ) ;
#204155 = CARTESIAN_POINT ( 'NONE',  ( -8.676855123066022912, 10.18571440074093282, -1.082531754730543971 ) ) ;
#204156 = CARTESIAN_POINT ( 'NONE',  ( 0.6684183810189650021, 2.117893379942568988, -0.1100008709709817956 ) ) ;
#204157 = CARTESIAN_POINT ( 'NONE',  ( -8.072954122294394352, 8.383144328957069291, -0.7998128361456362523 ) ) ;
#204159 = CARTESIAN_POINT ( 'NONE',  ( 3.719154087244529894, -1.729071306366702698, -0.9269775827704658244 ) ) ;
#204158 = CARTESIAN_POINT ( 'NONE',  ( 0.6125000000000037081, -0.1666666666666691277, 1.060881119635939562 ) ) ;
#204160 = CARTESIAN_POINT ( 'NONE',  ( 1.956163130892615731, 2.155914767609674598, -0.1587918856347721730 ) ) ;
#204161 = CARTESIAN_POINT ( 'NONE',  ( 2.278628554356322500, 1.682734121078124812, -0.7478279864501293783 ) ) ;
#204163 = CARTESIAN_POINT ( 'NONE',  ( -5.029675114306419559, 6.591709307070120261, -1.234896939913838754 ) ) ;
#204162 = CARTESIAN_POINT ( 'NONE',  ( -6.120580001926503755, 6.105374521861167914, -0.7998128361456362523 ) ) ;
#204164 = CARTESIAN_POINT ( 'NONE',  ( 3.943067085940495264, 0.5840054040482050013, -1.639550319303827219 ) ) ;
#204165 = CARTESIAN_POINT ( 'NONE',  ( 6.805829924380114804, 8.002851668940699881, 1.082531754730558626 ) ) ;
#204166 = CARTESIAN_POINT ( 'NONE',  ( -11.43653507270588499, 5.655220009861049668, 5.468867579827167980 ) ) ;
#204167 = CARTESIAN_POINT ( 'NONE',  ( 0.4972265960483426284, 1.796464302094663346, -1.202062886709959422 ) ) ;
#204168 = CARTESIAN_POINT ( 'NONE',  ( 3.216172551982798833, -1.646586737935524125, -1.163091166099708529 ) ) ;
#204169 = CARTESIAN_POINT ( 'NONE',  ( -3.046854503059236663, 2.800000000000024691, 2.500000000000011102 ) ) ;
#204170 = CARTESIAN_POINT ( 'NONE',  ( 0.2159880523044250267, -2.119658899406823505, 0.4233941889316418239 ) ) ;
#204171 = CARTESIAN_POINT ( 'NONE',  ( 2.782053229633123959, -1.014971971657689709, 1.689997848710776740 ) ) ;
#204172 = CARTESIAN_POINT ( 'NONE',  ( 6.508999999999982577, 2.977730662443831111, 2.353651457310241835 ) ) ;
#204173 = CARTESIAN_POINT ( 'NONE',  ( 2.472129730261590552, -1.859182766463037151, -0.5613441811427360983 ) ) ;
#204176 = VERTEX_POINT ( 'NONE', #56037 ) ;
#204175 = CARTESIAN_POINT ( 'NONE',  ( -3.689227196694341515, 7.318199139536432973, -0.7216878364870458196 ) ) ;
#204174 = CARTESIAN_POINT ( 'NONE',  ( 10.98546401119367566, 11.25740562920347365, 1.592223900679732518 ) ) ;
#204177 = B_SPLINE_CURVE_WITH_KNOTS ( 'NONE', 3,
 ( #151681, #82393, #83458, #149538, #168979, #1124 ),
 .UNSPECIFIED., .F., .F.,
 ( 4, 2, 4 ),
 ( 0.000000000000000000, 0.0003844267940947826011, 0.0007688535881895652022 ),
 .UNSPECIFIED. ) ;
#204178 = CARTESIAN_POINT ( 'NONE',  ( -4.299344108864953995, 7.069632989434141201, -1.082531754730551743 ) ) ;
#204179 = CARTESIAN_POINT ( 'NONE',  ( -0.1108833634136767998, 2.883350581177961391, -2.385667623150728556 ) ) ;
#204180 = CARTESIAN_POINT ( 'NONE',  ( 5.682802662783380754, 6.658966523782627434, 1.199719254218452935 ) ) ;
#204181 = CARTESIAN_POINT ( 'NONE',  ( -4.956387674247580755, 7.940146832334256111, 1.199719254218452935 ) ) ;
#204182 = CARTESIAN_POINT ( 'NONE',  ( -6.526270840131767059, 8.707344961610770540, -1.599625672291271394 ) ) ;
#204183 = DIRECTION ( 'NONE',  ( -0.000000000000000000, -1.000000000000000000, -0.000000000000000000 ) ) ;
#204184 = CARTESIAN_POINT ( 'NONE',  ( 0.3412290553763823175, 0.3797058362894655814, 2.173699509851903855 ) ) ;
#204185 = CARTESIAN_POINT ( 'NONE',  ( -8.283668668269720925, 8.766627655843896250, 1.056142170575426150E-14 ) ) ;
#204186 = CARTESIAN_POINT ( 'NONE',  ( 3.696105151714265347, 0.8860871710942277435, -1.750347149911928968 ) ) ;
#204187 = CARTESIAN_POINT ( 'NONE',  ( 6.435316467980822353, 10.65961964595298817, 1.040834085586084257E-14 ) ) ;
#204188 = CARTESIAN_POINT ( 'NONE',  ( 1.477185633673218312, -2.006960102380969779, -0.1948397147320118372 ) ) ;
#204189 = ORIENTED_EDGE ( 'NONE', *, *, #193885, .T. ) ;
#204190 = CARTESIAN_POINT ( 'NONE',  ( 1.833370464255643206, -1.703966518588348578, -1.256690760101538240 ) ) ;
#204191 = CARTESIAN_POINT ( 'NONE',  ( 1.499999999999989120, 1.056250000682816603, 0.000000000000000000 ) ) ;
#204193 = CARTESIAN_POINT ( 'NONE',  ( -6.235860587281615075, 9.362588887548838557, -1.199719254218440723 ) ) ;
#204192 = CARTESIAN_POINT ( 'NONE',  ( -10.53927507717405909, 2.018041202054385419, 6.084853302870027569 ) ) ;
#204194 = CARTESIAN_POINT ( 'NONE',  ( 3.204851553285171573, -0.3583046703147829692, 1.805758307424263354 ) ) ;
#204195 = ORIENTED_EDGE ( 'NONE', *, *, #16602, .T. ) ;
#204196 = CARTESIAN_POINT ( 'NONE',  ( -7.797910906154257304, 12.24931315715533486, 0.000000000000000000 ) ) ;
#204197 = DIRECTION ( 'NONE',  ( 0.000000000000000000, 0.000000000000000000, -1.000000000000000000 ) ) ;
#204199 = EDGE_CURVE ( 'NONE', #164712, #91680, #115000, .T. ) ;
#204198 = CARTESIAN_POINT ( 'NONE',  ( 4.254221937059123881, 0.9039275175388861161, -1.918405034562712830 ) ) ;
#204200 = CARTESIAN_POINT ( 'NONE',  ( 0.005434845660363255178, -0.7843016415976924449, -1.664241202765592176 ) ) ;
#204201 = CARTESIAN_POINT ( 'NONE',  ( -0.7499999999999972244, 5.389583334016151639, -1.299038105676652899 ) ) ;
#204202 = CARTESIAN_POINT ( 'NONE',  ( 6.368579470117202490, 8.453095353268645695, 1.599625672291281386 ) ) ;
#204203 = CARTESIAN_POINT ( 'NONE',  ( 5.254667053748194760, 8.288139441751686931, 1.199719254218452047 ) ) ;
#204204 = CARTESIAN_POINT ( 'NONE',  ( 4.007146649590315413, 1.765602988722612565, 1.062546815679512369 ) ) ;
#204205 = AXIS2_PLACEMENT_3D ( 'NONE', #202724, #74891, #120514 ) ;
#204207 = CARTESIAN_POINT ( 'NONE',  ( 1.382094229771430705, -0.2707140722739818650, -1.821126350552772610 ) ) ;
#204206 = CARTESIAN_POINT ( 'NONE',  ( -5.689618019229208734, 9.789638122409414223, 0.7998128361456481317 ) ) ;
#204208 = CARTESIAN_POINT ( 'NONE',  ( 5.929387212421286080, 6.133046765490340668, -0.7644126115040312808 ) ) ;
#204209 = DIRECTION ( 'NONE',  ( 0.000000000000000000, -0.000000000000000000, 1.000000000000000000 ) ) ;
#204210 = CARTESIAN_POINT ( 'NONE',  ( -9.499643733017421710, -9.912496545390952818, 0.08228199421455106854 ) ) ;
#204211 = CARTESIAN_POINT ( 'NONE',  ( 10.96381302404140179, -7.750949308402022453, -0.4891431138946180646 ) ) ;
#204212 =( BOUNDED_CURVE ( )  B_SPLINE_CURVE ( 2, ( #12577, #78649, #144776, #63479, #195620, #211841, #129633, #79720, #145837 ),
 .UNSPECIFIED., .F., .T. ) 
 B_SPLINE_CURVE_WITH_KNOTS ( ( 3, 2, 2, 2, 3 ),
 ( 0.2656250000000001110, 0.2708333333333333148, 0.2812500000000000000, 0.2916666666666666852, 0.2968749999999997780 ),
 .UNSPECIFIED. ) 
 CURVE ( )  GEOMETRIC_REPRESENTATION_ITEM ( )  RATIONAL_B_SPLINE_CURVE ( ( 0.9330127018922192983, 0.9330127018922207416, 1.000000000000000000, 0.8660254037844387076, 1.000000000000000000, 0.8660254037844387076, 1.000000000000000000, 0.9330127018922221849, 0.9330127018922194093 ) ) 
 REPRESENTATION_ITEM ( '' )  );
#204213 = CARTESIAN_POINT ( 'NONE',  ( 0.9091299924109221831, 1.668792687453458878, -1.444214864661397035 ) ) ;
#204214 = CARTESIAN_POINT ( 'NONE',  ( 4.183118113821016948, -0.2165105290278953043, -2.252005913828499573 ) ) ;
#204215 = CARTESIAN_POINT ( 'NONE',  ( -7.510853912290736289, 11.70648729774046792, 0.7216878364870458196 ) ) ;
#204216 = CARTESIAN_POINT ( 'NONE',  ( 3.550846374533889183, 0.2710319999918932021, 1.791078082347187683 ) ) ;
#204217 = CARTESIAN_POINT ( 'NONE',  ( 4.592943030449060160, 1.669885041223855060, 0.9386680909919845606 ) ) ;
#204218 = CARTESIAN_POINT ( 'NONE',  ( 5.020015195830264787, 2.048331326439792210, -0.3003445753073652469 ) ) ;
#204219 = CARTESIAN_POINT ( 'NONE',  ( -1.364683531250012516, 3.801041667008087099, -0.7879004041258300672 ) ) ;
#204220 = TOROIDAL_SURFACE ( 'NONE', #27986, 6.909076424898650259, 0.08000000000000000167 ) ;
#204221 = CARTESIAN_POINT ( 'NONE',  ( 3.098462860235187133, -0.5706901479570201108, -1.887068881103808327 ) ) ;
#204222 = CARTESIAN_POINT ( 'NONE',  ( 1.061403713111798153, 0.3786953092320010650, -1.888642112844605592 ) ) ;
#204223 = CARTESIAN_POINT ( 'NONE',  ( 3.449935675575486638, 1.870836310073907827, 0.001118452434160921221 ) ) ;
#204224 = CARTESIAN_POINT ( 'NONE',  ( 3.598509747979701690, -2.304983022191483766, -0.1141929325871558626 ) ) ;
#204225 = CARTESIAN_POINT ( 'NONE',  ( 3.209261600960995775, -1.519886386175553605, -1.073685847751577604 ) ) ;
#204226 = CARTESIAN_POINT ( 'NONE',  ( -1.364683531249997417, 4.759375000341424133, 1.214306433183764966E-14 ) ) ;
#204227 = CARTESIAN_POINT ( 'NONE',  ( 3.469446951953614189E-15, 5.290451655907108197, 1.214306433183764966E-14 ) ) ;
#204228 = EDGE_CURVE ( 'NONE', #183752, #115982, #110324, .T. ) ;
#204229 = CARTESIAN_POINT ( 'NONE',  ( 1.418734189139436275, 1.413363300903627717, -1.561561204404242842 ) ) ;
#204230 = CARTESIAN_POINT ( 'NONE',  ( 4.161989969270902812, 4.918371721313249623, 1.082531754730560403 ) ) ;
#204232 = DIRECTION ( 'NONE',  ( 0.000000000000000000, -1.000000000000000000, 0.000000000000000000 ) ) ;
#204231 = CARTESIAN_POINT ( 'NONE',  ( -1.364683531249997417, 5.321875000341417916, 1.214306433183764966E-14 ) ) ;
#204233 = LINE ( 'NONE', #24428, #179298 ) ;
#204234 = CARTESIAN_POINT ( 'NONE',  ( 2.672263739372262137, 2.109986773948614225, -0.2121620573234672125 ) ) ;
#204235 = CARTESIAN_POINT ( 'NONE',  ( 5.765600714192544274, 7.067438534623806667, -2.440103264412656348 ) ) ;
#204236 = CARTESIAN_POINT ( 'NONE',  ( 0.9143263792395848188, -2.019972748253701322, 0.004280675582559247648 ) ) ;
#204237 = CARTESIAN_POINT ( 'NONE',  ( 1.364683531249988757, 0.3843750003414206362, 0.000000000000000000 ) ) ;
#204238 = CARTESIAN_POINT ( 'NONE',  ( -4.446711195602264688, 4.290177271065136466, -0.7216878364870207285 ) ) ;
#204239 = CARTESIAN_POINT ( 'NONE',  ( 4.527533231959700366, 7.369540306339926516, 1.199719254218462483 ) ) ;
#204240 = ORIENTED_EDGE ( 'NONE', *, *, #42999, .F. ) ;
#204241 = CARTESIAN_POINT ( 'NONE',  ( 0.7378453340087381962, -1.528073262844112268, -1.529135702860604074 ) ) ;
#204242 = DIRECTION ( 'NONE',  ( -5.578564026256490882E-16, -1.000000000000000000, -9.066213480720158442E-32 ) ) ;
#204245 = CARTESIAN_POINT ( 'NONE',  ( 3.212919216758630014, 6.692230152952963529, 0.000000000000000000 ) ) ;
#204244 = CARTESIAN_POINT ( 'NONE',  ( 6.825078400183548055, 2.447738240532343124, 2.338733633852312366 ) ) ;
#204243 = CARTESIAN_POINT ( 'NONE',  ( 6.547661840756936691, 6.603636667163397256, 0.7998128361456352531 ) ) ;
#204246 = CARTESIAN_POINT ( 'NONE',  ( 11.94105721237523277, 10.19999999999999929, 1.187919463087244720 ) ) ;
#204247 = CARTESIAN_POINT ( 'NONE',  ( 5.542203953035277131, 0.8216685229280199509, 1.841735684200429990 ) ) ;
#204248 = CARTESIAN_POINT ( 'NONE',  ( -7.321039761699444703, 10.52466824108257804, 1.082531754730549967 ) ) ;
#204249 = CARTESIAN_POINT ( 'NONE',  ( 0.2928600448571066495, 1.818678932476354149, -1.222557900829209121 ) ) ;
#204250 = CARTESIAN_POINT ( 'NONE',  ( -1.665334536937729880E-16, -0.5000000000000004441, 3.000000000000000444 ) ) ;
#204252 = CARTESIAN_POINT ( 'NONE',  ( 1.364683531249997417, 10.48437500034139802, 2.602085213965210642E-15 ) ) ;
#204251 = CARTESIAN_POINT ( 'NONE',  ( 0.3568017664055183613, 0.8693207686717405736, 2.089032543936353736 ) ) ;
#204253 = CARTESIAN_POINT ( 'NONE',  ( -8.188234707649510113, 11.64035869464474082, -1.199719254218446718 ) ) ;
#204254 = CARTESIAN_POINT ( 'NONE',  ( 4.294157853547872605, -0.8666056138363428252, -1.820986994602634024 ) ) ;
#204256 = CARTESIAN_POINT ( 'NONE',  ( 1.335391617855705926, 0.5546556490612590817, -1.833562831147776739 ) ) ;
#204255 = CARTESIAN_POINT ( 'NONE',  ( -4.677199806590235376, 7.440188293455128665, 1.082531754730560403 ) ) ;
#204257 = CARTESIAN_POINT ( 'NONE',  ( -0.6823417656250003738, 2.530208333674753618, -1.181850606188749264 ) ) ;
#204258 = DIRECTION ( 'NONE',  ( -1.000000000000000000, 0.000000000000000000, 0.000000000000000000 ) ) ;
#204259 = CARTESIAN_POINT ( 'NONE',  ( 0.7500000000000006661, 9.666666666666671404, -1.299038105676657340 ) ) ;
#204260 = CARTESIAN_POINT ( 'NONE',  ( 3.000334558935643603, -0.5012536917932303160, -1.650428355875031228 ) ) ;
#204261 = CARTESIAN_POINT ( 'NONE',  ( 3.393283585170187688, 7.180857625999046867, 0.7998128361456271485 ) ) ;
#204262 = CARTESIAN_POINT ( 'NONE',  ( 2.284116761108864413, -1.734514481284253007, -0.3503773294724100706 ) ) ;
#204263 = CARTESIAN_POINT ( 'NONE',  ( 2.526041439118778431, -1.990860190764773829, 0.2976642988744558904 ) ) ;
#204264 = CARTESIAN_POINT ( 'NONE',  ( 5.596761079150560647, -0.5311557606857522096, -2.141783596114990917 ) ) ;
#204265 = ORIENTED_EDGE ( 'NONE', *, *, #155084, .F. ) ;
#204266 = CARTESIAN_POINT ( 'NONE',  ( -7.449279056065764237, 7.655523418356991350, 0.7998128361456341429 ) ) ;
#204268 = CARTESIAN_POINT ( 'NONE',  ( 3.796500049179197589, 1.423950305759081214, -1.427950143821264506 ) ) ;
#204267 = CARTESIAN_POINT ( 'NONE',  ( 3.985108911058360182, -1.979049277059058864, -0.7619450576143712572 ) ) ;
#204270 = VERTEX_POINT ( 'NONE', #105894 ) ;
#204269 = CARTESIAN_POINT ( 'NONE',  ( 4.359482725938978120, -1.404519563743265920, -1.144221460762798737 ) ) ;
#204271 = CARTESIAN_POINT ( 'NONE',  ( 4.050854035433010480, 7.948023151305657841, 0.000000000000000000 ) ) ;
#204272 = EDGE_LOOP ( 'NONE', ( #5840, #152607, #165328, #88110 ) ) ;
#204273 = CARTESIAN_POINT ( 'NONE',  ( 1.340467186903429253, 0.3614942610149494695, 1.835218787103513050 ) ) ;
#204274 = CARTESIAN_POINT ( 'NONE',  ( 1.451998047843343409, 7.315968950353815892, -4.301760722578415574 ) ) ;
#204275 = CARTESIAN_POINT ( 'NONE',  ( 6.428355384240774129, -0.8606449381524762243, -1.593976378398887173 ) ) ;
#204276 = FACE_OUTER_BOUND ( 'NONE', #198726, .T. ) ;
#204277 = CARTESIAN_POINT ( 'NONE',  ( -11.30309668167796922, 5.150585336095395483, -5.742054036728553967 ) ) ;
#204278 = CARTESIAN_POINT ( 'NONE',  ( -1.500000000000008216, 8.531250000682797818, 3.469446951953614189E-15 ) ) ;
#204279 = CARTESIAN_POINT ( 'NONE',  ( -1.402160292154681736E-14, 2.509375000341417028, -1.575800808251660134 ) ) ;
#204280 = SURFACE_SIDE_STYLE ('',( #171819 ) ) ;
#204281 = ORIENTED_EDGE ( 'NONE', *, *, #63015, .F. ) ;
#204282 = CARTESIAN_POINT ( 'NONE',  ( 5.831415467653547680, 8.857049574687536619, -1.082531754730548412 ) ) ;
#204283 = CARTESIAN_POINT ( 'NONE',  ( -3.499413046103020175, 7.096749297179887783, 0.7216878364870338292 ) ) ;
#204284 = CARTESIAN_POINT ( 'NONE',  ( -6.798487682609798632, 6.896266815991691779, 0.7998128361456341429 ) ) ;
#204285 = CARTESIAN_POINT ( 'NONE',  ( 4.306960158517386894, -0.4675538901007176285, -2.068242682749166672 ) ) ;
#204287 = CARTESIAN_POINT ( 'NONE',  ( -10.01593736600300311, 5.734280347462529015, 5.906528988732270058 ) ) ;
#204286 = CARTESIAN_POINT ( 'NONE',  ( -0.1296875068448125334, 2.048176110289974261, -2.243787855586779401 ) ) ;
#204288 = CARTESIAN_POINT ( 'NONE',  ( 5.448493488195655488, 0.5694873833897282633, 1.887333253073280703 ) ) ;
#204289 = CARTESIAN_POINT ( 'NONE',  ( 1.364683531249986537, 0.9052083336747533959, -0.7879004041258239610 ) ) ;
#204290 = CARTESIAN_POINT ( 'NONE',  ( 0.4924401237900773443, -1.114920267122095021, 1.676101429157205613 ) ) ;
#204291 = ORIENTED_EDGE ( 'NONE', *, *, #210514, .F. ) ;
#204292 = CARTESIAN_POINT ( 'NONE',  ( 6.491443032814855130, -0.4656331456187530748, 2.073361762655197893 ) ) ;
#204293 = B_SPLINE_CURVE_WITH_KNOTS ( 'NONE', 3,
 ( #120169, #102783, #170974, #38849 ),
 .UNSPECIFIED., .F., .F.,
 ( 4, 4 ),
 ( 0.000000000000000000, 1.930757672285080358E-06 ),
 .UNSPECIFIED. ) ;
#204294 = CARTESIAN_POINT ( 'NONE',  ( 8.776224899084628106, 13.27471476138783224, 8.184001253707569035 ) ) ;
#204295 = CARTESIAN_POINT ( 'NONE',  ( 1.416557266959647787, 0.8372786474034592530, 1.893679232998768391 ) ) ;
#204296 = ORIENTED_EDGE ( 'NONE', *, *, #61620, .T. ) ;
#204297 = CARTESIAN_POINT ( 'NONE',  ( 4.030516805012513082, 7.924296382481737844, 0.000000000000000000 ) ) ;
#204298 = CARTESIAN_POINT ( 'NONE',  ( 4.525389411911321602, 8.501647757197021704, -0.7998128361456381397 ) ) ;
#204300 = CARTESIAN_POINT ( 'NONE',  ( 6.003563092752934871, 5.898578451166879510, 0.7998128361456341429 ) ) ;
#204299 = CARTESIAN_POINT ( 'NONE',  ( 4.962875334715753262, 0.2052988877573138915, -2.080521221900538009 ) ) ;
#204301 = CARTESIAN_POINT ( 'NONE',  ( 5.501576472095266901, 9.640532660744973725, -0.7998128361456481317 ) ) ;
#204304 = EDGE_LOOP ( 'NONE', ( #171986, #160548, #208885, #167990, #73679, #181462 ) ) ;
#204303 = CARTESIAN_POINT ( 'NONE',  ( 1.260107830910334181, 1.809384220011617028, 0.08917393313457448734 ) ) ;
#204302 = CARTESIAN_POINT ( 'NONE',  ( 2.836711209001481659, 0.2215568149019596367, 1.812007907362273018 ) ) ;
#204305 = CARTESIAN_POINT ( 'NONE',  ( 6.428370569364434850, 1.274405893209800356, -1.801548588985131039 ) ) ;
#204306 = DIRECTION ( 'NONE',  ( 0.000000000000000000, 1.000000000000000000, 0.000000000000000000 ) ) ;
#204307 = CARTESIAN_POINT ( 'NONE',  ( 4.085166796624926100, -0.2132991444873769959, -2.196430506890618695 ) ) ;
#204308 = CARTESIAN_POINT ( 'NONE',  ( 6.446011968293428041, 9.607765498729298415, -1.199719254218440723 ) ) ;
#204309 = CARTESIAN_POINT ( 'NONE',  ( 0.6823417656249969321, 8.838541667008065872, -1.181850606188757036 ) ) ;
#204310 = CARTESIAN_POINT ( 'NONE',  ( 2.912652942483742180, -0.5572119909246497915, -1.829279355302193544 ) ) ;
#204311 = CARTESIAN_POINT ( 'NONE',  ( 9.420217803396747414, 9.884675613584706255, 0.7998128361456462443 ) ) ;
#204312 = CARTESIAN_POINT ( 'NONE',  ( 6.127406499145813257, 0.1562011534181114436, -2.064545280851529885 ) ) ;
#204313 = CARTESIAN_POINT ( 'NONE',  ( -2.353626204688216217E-14, 0.7343750003414535321, 1.570758158831780271 ) ) ;
#204314 = CARTESIAN_POINT ( 'NONE',  ( 5.425378541715013547, -1.389685604419872655, -1.694579525865948844 ) ) ;
#204315 = CARTESIAN_POINT ( 'NONE',  ( 5.911136963822321455, 7.250628055112136039, -1.245581879728396846 ) ) ;
#204316 = CARTESIAN_POINT ( 'NONE',  ( -9.469892045836674654, -6.532648833121162291, 0.4294077647110516871 ) ) ;
#204317 = CARTESIAN_POINT ( 'NONE',  ( 9.578928831967440161, -9.999999999999978684, -0.1215685829351341452 ) ) ;
#204318 = EDGE_CURVE ( 'NONE', #180616, #185672, #81857, .T. ) ;
#204319 = CARTESIAN_POINT ( 'NONE',  ( 4.869313445963426190, 5.709895770826003414, 1.199719254218452935 ) ) ;
#204320 = CARTESIAN_POINT ( 'NONE',  ( 0.000000000000000000, -1.684374999522041394, -3.793834371823813445 ) ) ;
#204321 = CARTESIAN_POINT ( 'NONE',  ( 0.000000000000000000, -2.000000000000001776, 10.24999999999998934 ) ) ;
#204322 = AXIS2_PLACEMENT_3D ( 'NONE', #57684, #25167, #107561 ) ;
#204323 = CARTESIAN_POINT ( 'NONE',  ( -8.351459436338041442, 9.806086099558291025, -1.082531754730543971 ) ) ;
#204324 = CARTESIAN_POINT ( 'NONE',  ( 3.627688620108284745, 6.389997935838436227, 1.199719254218452047 ) ) ;
#204325 = CARTESIAN_POINT ( 'NONE',  ( 6.983263157960365675, -0.006178392973848687020, 2.053544886540019210 ) ) ;
#204326 = CARTESIAN_POINT ( 'NONE',  ( 1.194935658704935566, 1.779638138761422628, 0.9480210990304924756 ) ) ;
#204327 = CARTESIAN_POINT ( 'NONE',  ( -9.806625181386236179, 10.33548422123910449, -0.7998128361456291469 ) ) ;
#204328 = CARTESIAN_POINT ( 'NONE',  ( 6.668631453075247073, 8.873432343378178544, -1.599625672291281386 ) ) ;
#204329 = CARTESIAN_POINT ( 'NONE',  ( 1.869323357045350686, 2.096458975851514861, -0.6381942758529115522 ) ) ;
#204330 = CARTESIAN_POINT ( 'NONE',  ( 5.461492464141177727, 0.3521552718798379722, -1.791230276788812414 ) ) ;
#204331 = CARTESIAN_POINT ( 'NONE',  ( -5.274285450916075035, 6.112086766612214284, 1.199719254218450271 ) ) ;
#204332 = EDGE_CURVE ( 'NONE', #129544, #93441, #7255, .T. ) ;
#204333 = CARTESIAN_POINT ( 'NONE',  ( 5.939880696562888751, 7.062853913145737295, -1.082531754730548412 ) ) ;
#204334 = CARTESIAN_POINT ( 'NONE',  ( 9.694243528971124846, 11.26870452434320491, 1.199719254218450271 ) ) ;
#204335 = CARTESIAN_POINT ( 'NONE',  ( -6.479871072688648148, 6.524547437750345402, 0.000000000000000000 ) ) ;
#204336 = CARTESIAN_POINT ( 'NONE',  ( 3.818592820543298405, 7.606775390609172405, -0.7998128361456221525 ) ) ;
#204337 = CARTESIAN_POINT ( 'NONE',  ( 4.686278372178935392, 5.496354851410763409, 1.199719254218452047 ) ) ;
#204338 = VERTEX_POINT ( 'NONE', #43010 ) ;
#204340 = CARTESIAN_POINT ( 'NONE',  ( 0.02993902094421736770, -1.973830418800892161, 0.3948085296872869687 ) ) ;
#204339 = CARTESIAN_POINT ( 'NONE',  ( 2.841158510722852970, 0.6603703904487292498, -1.718939526767604420 ) ) ;
#204341 = CARTESIAN_POINT ( 'NONE',  ( 2.460726772196987433, 1.776095029035225537, 1.458756201258274210 ) ) ;
#204343 = CARTESIAN_POINT ( 'NONE',  ( 0.3384086464433467278, -1.803039684303367141, -0.4601552930486965121 ) ) ;
#204342 = CARTESIAN_POINT ( 'NONE',  ( 2.562127843302666186, 5.932973550587659517, 0.000000000000000000 ) ) ;
#204344 = CARTESIAN_POINT ( 'NONE',  ( -4.660252114795309097, 6.460046772059735432, -1.599625672291256295 ) ) ;
#204345 = CARTESIAN_POINT ( 'NONE',  ( -5.487584206907313522, 6.516568040952106067, -1.094815266226579098 ) ) ;
#204346 = CARTESIAN_POINT ( 'NONE',  ( 2.935702856749936362, -1.841876368404654629, 0.5141854427313449216 ) ) ;
#204347 = CARTESIAN_POINT ( 'NONE',  ( -10.15913717534155047, 10.74674821418697057, 0.7998128361456462443 ) ) ;
#204348 = CARTESIAN_POINT ( 'NONE',  ( 6.348661983278831578, 6.841051910588018536, 0.6299351563821649069 ) ) ;
#204349 = CARTESIAN_POINT ( 'NONE',  ( -5.008811405605897882, 4.808311159487113073, 0.7998128361456281477 ) ) ;
#204351 = CARTESIAN_POINT ( 'NONE',  ( 0.7252172114964609007, -1.777616610744123804, 0.5828384007960025759 ) ) ;
#204350 = CARTESIAN_POINT ( 'NONE',  ( 2.823863332701610940, 1.159264052448713889, -1.739707760033171180 ) ) ;
#204352 = CARTESIAN_POINT ( 'NONE',  ( 2.442732317853496760, 1.238130588059358717, 1.591075322344523535 ) ) ;
#204353 = CARTESIAN_POINT ( 'NONE',  ( 8.107412671292035355, 10.48173408797264194, 1.443375672974076540 ) ) ;
#204354 = VERTEX_POINT ( 'NONE', #109123 ) ;
#204355 = CARTESIAN_POINT ( 'NONE',  ( -0.6823417656249969321, 4.030208333674754506, -1.181850606188749264 ) ) ;
#204356 = CARTESIAN_POINT ( 'NONE',  ( 2.700428686635591546, 1.471443353139300081, 0.9291617766199999906 ) ) ;
#204357 = AXIS2_PLACEMENT_3D ( 'NONE', #99355, #148110, #210946 ) ;
#204358 = CARTESIAN_POINT ( 'NONE',  ( 4.847203612085560387, 5.613824621309978724, -1.199719254218452047 ) ) ;
#204360 =( NAMED_UNIT ( * ) SI_UNIT ( $, .STERADIAN. ) SOLID_ANGLE_UNIT ( ) );
#204359 = CARTESIAN_POINT ( 'NONE',  ( -6.824425546749161242, -8.104785249476792686, 6.609253696060804373 ) ) ;
#204361 = CARTESIAN_POINT ( 'NONE',  ( 3.193694537771115449, -0.6981934656059236577, 1.577442374586303320 ) ) ;
#204362 = CARTESIAN_POINT ( 'NONE',  ( 3.052458795248469414, -1.657928338269051505, 1.433322580492613296 ) ) ;
#204363 = CARTESIAN_POINT ( 'NONE',  ( 5.250674450588199704, 0.6379336648693231249, 2.112661011922472021 ) ) ;
#204364 = CARTESIAN_POINT ( 'NONE',  ( -9.968662085647130411, 5.546348307810219147, -6.001034872913991514 ) ) ;
#204365 = CARTESIAN_POINT ( 'NONE',  ( 3.256845431185355633, -0.6256494993409821292, -2.079000826131827129 ) ) ;
#204366 = CARTESIAN_POINT ( 'NONE',  ( 2.420285107995377327, 1.192830232448302441, -1.382225081888274643 ) ) ;
#204367 = CARTESIAN_POINT ( 'NONE',  ( -0.4019237886466871523, 9.229914550367427140, -1.499999999999998668 ) ) ;
#204368 = CARTESIAN_POINT ( 'NONE',  ( 4.311780797230674089, -1.305379566919599332, -1.666953740739559819 ) ) ;
#204369 = CARTESIAN_POINT ( 'NONE',  ( 6.639320575229291421, 7.052752469465089824, 2.594893258668645952 ) ) ;
#204370 = ADVANCED_FACE ( 'NONE', ( #175137 ), #4200, .T. ) ;
#204371 = ORIENTED_EDGE ( 'NONE', *, *, #97999, .T. ) ;
#204373 = CARTESIAN_POINT ( 'NONE',  ( -1.364683531250000748, 2.071875000341422357, 1.214306433183764966E-14 ) ) ;
#204372 = CARTESIAN_POINT ( 'NONE',  ( 4.476316811684385222, -2.223409025971525121, -0.5576598666321966880 ) ) ;
#204374 = DIRECTION ( 'NONE',  ( -0.000000000000000000, 1.000000000000000000, -0.000000000000000000 ) ) ;
#204375 = CARTESIAN_POINT ( 'NONE',  ( 10.38962578677386084, 11.01565159419135043, 0.000000000000000000 ) ) ;
#204376 = AXIS2_PLACEMENT_3D ( 'NONE', #3679, #23140, #202961 ) ;
#204377 = CARTESIAN_POINT ( 'NONE',  ( 0.1531979293848736434, 0.3668625560977051281, 2.088361607889513305 ) ) ;
#204378 = CARTESIAN_POINT ( 'NONE',  ( -4.934804725694220906, 7.740727365743146571, -1.082531754730549967 ) ) ;
#204379 = CARTESIAN_POINT ( 'NONE',  ( 2.711267533052988732, 6.106969855296372707, -0.7216878364870267237 ) ) ;
#204380 = CARTESIAN_POINT ( 'NONE',  ( -6.195713011320804320, 7.291048603704809672, -1.082531754730543083 ) ) ;
#204381 = DIRECTION ( 'NONE',  ( 0.000000000000000000, 0.000000000000000000, 1.000000000000000000 ) ) ;
#204382 = ORIENTED_EDGE ( 'NONE', *, *, #211675, .F. ) ;
#204383 = CARTESIAN_POINT ( 'NONE',  ( 5.572888750952301073, -0.9041123360693378297, 1.802415994888312722 ) ) ;
#204385 = CARTESIAN_POINT ( 'NONE',  ( 3.836832695767174783, -1.986499165045521265, -0.5546697284559941599 ) ) ;
#204384 = CARTESIAN_POINT ( 'NONE',  ( 3.798255590122797898, 7.583048621785260401, -0.7998128361456221525 ) ) ;
#204387 = CARTESIAN_POINT ( 'NONE',  ( -0.1411974294642098227, 4.091293698307607585, -2.455098582995118406 ) ) ;
#204386 = CARTESIAN_POINT ( 'NONE',  ( 8.154303043976348420, 8.478051404252736845, 0.7998128361456281477 ) ) ;
#204388 = ADVANCED_FACE ( 'NONE', ( #166936 ), #82465, .F. ) ;
#204389 = CARTESIAN_POINT ( 'NONE',  ( 5.338878628731272613, 9.450718510153643948, -0.7998128361456481317 ) ) ;
#204390 = CARTESIAN_POINT ( 'NONE',  ( 3.285556943750000514, -1.013541666188710888, 1.896917185911906500 ) ) ;
#204391 = DIRECTION ( 'NONE',  ( 1.000000000000000000, -0.000000000000000000, -0.000000000000000000 ) ) ;
#204392 = CARTESIAN_POINT ( 'NONE',  ( 6.333935822332933618, 2.167035306593240840, 0.3253760364356065860 ) ) ;
#204393 = CARTESIAN_POINT ( 'NONE',  ( 3.463517678199812266, -1.944071305346905643, -0.5350885120067662148 ) ) ;
#204394 = CARTESIAN_POINT ( 'NONE',  ( 2.929072846782492245, -1.238530643895646488, -1.362589426554157157 ) ) ;
#204395 = ADVANCED_FACE ( 'NONE', ( #112920 ), #147493, .F. ) ;
#204396 = CARTESIAN_POINT ( 'NONE',  ( 6.993308306550549247, 7.053281200597435685, 1.040834085586084257E-14 ) ) ;
#204397 = PRESENTATION_STYLE_ASSIGNMENT (( #138379 ) ) ;
#204398 = CARTESIAN_POINT ( 'NONE',  ( 0.4809449578498920519, 1.612012756419522352, -0.6139154093185476002 ) ) ;
#204399 = CARTESIAN_POINT ( 'NONE',  ( -2.927671105547157371, 5.503034492191895666, 1.199719254218462483 ) ) ;
#204400 = CARTESIAN_POINT ( 'NONE',  ( 1.231506118810040018, 2.296321937838792238, 0.1066795702680169711 ) ) ;
#204401 = CARTESIAN_POINT ( 'NONE',  ( -6.256197817702116026, 9.386315656372753224, -1.199719254218440723 ) ) ;
#204402 = CARTESIAN_POINT ( 'NONE',  ( 0.3337811221923889793, -2.067640401758659596, 0.9186946961548744239 ) ) ;
#204403 = CARTESIAN_POINT ( 'NONE',  ( 3.264387862500417903, 0.9470664325190655264, 1.881190857022313478 ) ) ;
#204404 = CARTESIAN_POINT ( 'NONE',  ( -5.101610940492132151, 9.173906207207963348, -0.7998128361456362523 ) ) ;
#204405 = CARTESIAN_POINT ( 'NONE',  ( 8.450809820019639318, 8.753699632978056755, -0.7998128361456291469 ) ) ;
#204406 = CARTESIAN_POINT ( 'NONE',  ( 7.146556367734776316, 7.510272981878305387, 0.7216878364870267237 ) ) ;
#204407 = CARTESIAN_POINT ( 'NONE',  ( 8.378074386687000441, 10.50815134976859078, 15.76159487570644124 ) ) ;
#204408 = CARTESIAN_POINT ( 'NONE',  ( -6.575868197828002693, 7.630599971342813426, 1.199719254218450271 ) ) ;
#204409 = CARTESIAN_POINT ( 'NONE',  ( 6.941411460072420603, 7.200660912947041581, 1.040834085586084257E-14 ) ) ;
#204410 = CARTESIAN_POINT ( 'NONE',  ( 5.026094266273638311, 6.779731885415203330, 1.422988838494985364 ) ) ;
#204411 = CARTESIAN_POINT ( 'NONE',  ( -3.764360206088648297, 7.543504007078730922, -0.7998128361456281477 ) ) ;
#204412 = CARTESIAN_POINT ( 'NONE',  ( 3.656649667753679278, 2.210956852819144114, 0.2149545701610345305 ) ) ;
#204413 = CARTESIAN_POINT ( 'NONE',  ( 2.466951935624495107, 0.1062163371072753354, -2.188993582743845590 ) ) ;
#204414 = CARTESIAN_POINT ( 'NONE',  ( -7.386494761346872551, 7.511998731193139989, -0.7998128361456291469 ) ) ;
#204415 = CARTESIAN_POINT ( 'NONE',  ( -4.111865726694519552, 8.019203457777400956, 0.000000000000000000 ) ) ;
#204416 = CARTESIAN_POINT ( 'NONE',  ( 5.758247127753066685, -1.962046631956643195, -0.001586170976335121285 ) ) ;
#204417 = PRODUCT_DEFINITION_FORMATION_WITH_SPECIFIED_SOURCE ( 'ANY', '', #80054, .NOT_KNOWN. ) ;
#204418 = DIRECTION ( 'NONE',  ( -1.000000000000000000, 0.000000000000000000, 0.000000000000000000 ) ) ;
#204419 = CARTESIAN_POINT ( 'NONE',  ( -0.6823417656250212460, 1.301041667008083547, 1.181850606188755259 ) ) ;
#204420 = CARTESIAN_POINT ( 'NONE',  ( -3.634994582239682526, 6.294558541704648569, 1.082531754730549967 ) ) ;
#204421 = CARTESIAN_POINT ( 'NONE',  ( -4.934804725694212912, 8.701096580044490381, -0.7216878364870207285 ) ) ;
#204422 = CARTESIAN_POINT ( 'NONE',  ( 4.324552338190708056, -0.9094542848507057853, -1.915842285305848769 ) ) ;
#204423 = CARTESIAN_POINT ( 'NONE',  ( -3.298376509874564988, 7.070132704820777825, 0.000000000000000000 ) ) ;
#204424 = VERTEX_POINT ( 'NONE', #47878 ) ;
#204425 = CARTESIAN_POINT ( 'NONE',  ( 5.049776242366147194, 0.6816224847111511664, -2.051488706027407183 ) ) ;
#204426 = CARTESIAN_POINT ( 'NONE',  ( 7.142447996300871793, 7.227277505306155092, 0.7998128361456341429 ) ) ;
#204427 = CARTESIAN_POINT ( 'NONE',  ( 4.651808992177354440, 0.7092673950449077669, 1.699362209096597187 ) ) ;
#204428 = UNCERTAINTY_MEASURE_WITH_UNIT (LENGTH_MEASURE( 1.000000000000000082E-05 ), #33353, 'distance_accuracy_value', 'NONE');
#204429 = AXIS2_PLACEMENT_3D ( 'NONE', #89749, #121242, #154730 ) ;
#204430 = CARTESIAN_POINT ( 'NONE',  ( -10.99943592164172834, -8.407420853759269619, 0.1113975120798846308 ) ) ;
#204431 = CARTESIAN_POINT ( 'NONE',  ( 1.364683531249986537, 1.967708333674750731, -0.7879004041258239610 ) ) ;
#204432 = CARTESIAN_POINT ( 'NONE',  ( 0.1689663589281220069, 0.9994598401263864451, 1.424626921871420926 ) ) ;
#204433 = CARTESIAN_POINT ( 'NONE',  ( 6.827182134110233669, 2.063332311267600971, 2.217821918593851027 ) ) ;
#204434 = LINE ( 'NONE', #188203, #190007 ) ;
#204435 = CARTESIAN_POINT ( 'NONE',  ( -7.058808231563621582, -6.527411821100059797, 6.446420058208181203 ) ) ;
#204436 = CARTESIAN_POINT ( 'NONE',  ( 4.627887939457571598, -1.327398817707679868, -1.706084338546076662 ) ) ;
#204437 = CARTESIAN_POINT ( 'NONE',  ( -5.461236948206312114, 5.265864615862458464, 0.7998128361456341429 ) ) ;
#204438 = CARTESIAN_POINT ( 'NONE',  ( -8.066738210006693777, 10.43428054980638997, 1.443375672974090751 ) ) ;
#204439 = CARTESIAN_POINT ( 'NONE',  ( 2.993221558690632556, 1.854768100113469265, -1.110066390340218367 ) ) ;
#204440 = CARTESIAN_POINT ( 'NONE',  ( 4.411372364376418886, -0.3401156029278085136, 1.941656249039567905 ) ) ;
#204441 = CARTESIAN_POINT ( 'NONE',  ( 3.409274926616968404, 0.4192967605245543905, 1.682228440661166502 ) ) ;
#204442 = CARTESIAN_POINT ( 'NONE',  ( 0.7850416839378616674, 1.930235501049954339, -1.037882601892345713 ) ) ;
#204443 = CARTESIAN_POINT ( 'NONE',  ( 1.606910496583548786, -0.8321943236449917958, -2.152478949753482862 ) ) ;
#204444 = CARTESIAN_POINT ( 'NONE',  ( 3.796211532432732572, -2.058264701994051649, -0.1047273801592675524 ) ) ;
#204445 = CARTESIAN_POINT ( 'NONE',  ( 5.899939537456503125, -0.7029524595547633758, -1.810543181819963321 ) ) ;
#204446 = CARTESIAN_POINT ( 'NONE',  ( -7.578644679914719795, 9.864838098032418401, 1.443375672974090751 ) ) ;
#204447 = CARTESIAN_POINT ( 'NONE',  ( -5.224688093219839402, 7.188831756880171397, -1.599625672291271394 ) ) ;
#204448 = DIRECTION ( 'NONE',  ( 1.224646799147353454E-16, 0.000000000000000000, -1.000000000000000000 ) ) ;
#204450 = ORIENTED_EDGE ( 'NONE', *, *, #117680, .T. ) ;
#204449 =( NAMED_UNIT ( * ) PLANE_ANGLE_UNIT ( ) SI_UNIT ( $, .RADIAN. ) );
#204451 = CARTESIAN_POINT ( 'NONE',  ( -6.344852701071109102, 10.34615255131755163, 0.000000000000000000 ) ) ;
#204452 = CARTESIAN_POINT ( 'NONE',  ( 3.188704395469597497, -2.173853526369253331, -0.3788738375181537332 ) ) ;
#204453 = CARTESIAN_POINT ( 'NONE',  ( -3.285556943750000514, -0.1385416661887106660, -1.896917185911906500 ) ) ;
#204454 = ORIENTED_EDGE ( 'NONE', *, *, #59437, .T. ) ;
#204455 = CARTESIAN_POINT ( 'NONE',  ( 0.7778919621034340315, -0.9889961724188134351, -1.576189065804904477 ) ) ;
#204456 = CARTESIAN_POINT ( 'NONE',  ( -0.02919842301644676522, 2.866066704180502800, -2.562138095921069780 ) ) ;
#204457 = CARTESIAN_POINT ( 'NONE',  ( -1.500000000000011324, 5.452083334016153415, 0.8660254037844403729 ) ) ;
#204458 = CARTESIAN_POINT ( 'NONE',  ( 4.357662274398333757, 7.395159486995275699, -1.145423081618229144 ) ) ;
#204460 = CARTESIAN_POINT ( 'NONE',  ( 0.7500000000000006661, 12.69791666734946389, -1.299038105676657340 ) ) ;
#204459 = FACE_OUTER_BOUND ( 'NONE', #154134, .T. ) ;
#204461 = CARTESIAN_POINT ( 'NONE',  ( 6.246043375366982175, 0.5822610321466625827, 1.746719530172704760 ) ) ;
#204462 = ORIENTED_EDGE ( 'NONE', *, *, #40921, .T. ) ;
#204463 = CARTESIAN_POINT ( 'NONE',  ( 2.043891306636512528, 0.7897949731258145922, -1.903750762553678921 ) ) ;
#204464 = CARTESIAN_POINT ( 'NONE',  ( -1.360316468750026653, -0.1302083329919105914, -0.7853790794159422051 ) ) ;
#204465 = CARTESIAN_POINT ( 'NONE',  ( -7.542413527904030524, 7.693903958843159252, 1.040834085586084257E-14 ) ) ;
#204466 = DIRECTION ( 'NONE',  ( -0.6483454320283799088, 0.000000000000000000, 0.7613463080411786432 ) ) ;
#204467 = EDGE_CURVE ( 'NONE', #122076, #68973, #210497, .T. ) ;
#204468 = CARTESIAN_POINT ( 'NONE',  ( 3.171717870593107058, 5.787755718078879674, -1.199719254218446718 ) ) ;
#204469 = CARTESIAN_POINT ( 'NONE',  ( 1.270465292308793126, -1.308197635955485216, 1.592426268366262665 ) ) ;
#204471 = CARTESIAN_POINT ( 'NONE',  ( 4.440845869443198701, -1.426288408191313639, -1.164454570719307469 ) ) ;
#204470 = FACE_OUTER_BOUND ( 'NONE', #10610, .T. ) ;
#204472 = CARTESIAN_POINT ( 'NONE',  ( 5.469824908109481854, 8.468880595181346393, -1.199719254218446718 ) ) ;
#204473 = CARTESIAN_POINT ( 'NONE',  ( -4.145761110728687804, 8.058748072483927771, -0.7998128361456481317 ) ) ;
#204474 = CARTESIAN_POINT ( 'NONE',  ( 7.013428937081384262, 5.939655416065873439, 2.436399677959149024 ) ) ;
#204475 = CARTESIAN_POINT ( 'NONE',  ( 4.055453297694236348, -1.834216022232620702, -1.226887332174103173 ) ) ;
#204476 = CARTESIAN_POINT ( 'NONE',  ( 6.731690493876715919, -1.469984723218084488, -1.719904613669322790 ) ) ;
#204477 = CARTESIAN_POINT ( 'NONE',  ( -3.456965981804629884, 6.976951378839947537, 1.040834085586084257E-14 ) ) ;
#204478 = CARTESIAN_POINT ( 'NONE',  ( 0.5274218815167727170, -0.2782315536139517431, 1.891897276498944347 ) ) ;
#204479 = CARTESIAN_POINT ( 'NONE',  ( 1.112517963266421939, 1.944731545904467396, 0.5331650539944567946 ) ) ;
#204480 = CARTESIAN_POINT ( 'NONE',  ( -6.673079560224743467, -7.008190897455698121, 6.761669295867172025 ) ) ;
#204481 = CARTESIAN_POINT ( 'NONE',  ( 1.740083653633100580, -2.182622149841602521, -0.7203450084119922270 ) ) ;
#204482 = CARTESIAN_POINT ( 'NONE',  ( 6.789956943122251509, -0.7972922127613899512, 1.690610701080223821 ) ) ;
#204483 = EDGE_CURVE ( 'NONE', #42660, #175731, #26366, .T. ) ;
#204484 = CARTESIAN_POINT ( 'NONE',  ( 1.499999999999996891, 12.17708333401613352, -0.8660254037844378194 ) ) ;
#204485 = DIRECTION ( 'NONE',  ( 0.000000000000000000, 0.000000000000000000, 1.000000000000000000 ) ) ;
#204486 = AXIS2_PLACEMENT_3D ( 'NONE', #6568, #105184, #190654 ) ;
#204487 = CARTESIAN_POINT ( 'NONE',  ( 2.201827603038747139, -1.870314503716500099, 0.04339327950253490246 ) ) ;
#204488 = CARTESIAN_POINT ( 'NONE',  ( 2.132046339962359038, 2.016188815772378629, 0.04465230659478347519 ) ) ;
#204490 = CARTESIAN_POINT ( 'NONE',  ( -5.980802423990385641, 6.150226714305422782, 9.481663569016276247E-06 ) ) ;
#204489 = CARTESIAN_POINT ( 'NONE',  ( -1.402160292154681736E-14, 0.4468750003414233563, -1.575800808251665908 ) ) ;
#204492 = CARTESIAN_POINT ( 'NONE',  ( 4.811209553025526553, 1.832079168721172380, 1.038602630702612384 ) ) ;
#204491 = CARTESIAN_POINT ( 'NONE',  ( -9.124801077197171040, 10.60435499727357289, -1.199719254218441611 ) ) ;
#204493 = CARTESIAN_POINT ( 'NONE',  ( 8.606728586576791074, 8.935604860628076906, 0.7998128361456462443 ) ) ;
#204495 = CARTESIAN_POINT ( 'NONE',  ( -6.530223543276495235, 10.77034456713125188, -0.7998128361456291469 ) ) ;
#204494 = CARTESIAN_POINT ( 'NONE',  ( 4.980641328173811999, 6.904110530993182948, 1.599625672291269396 ) ) ;
#204496 = FILL_AREA_STYLE ('',( #138474 ) ) ;
#204497 = CARTESIAN_POINT ( 'NONE',  ( 4.377216478116826792, -1.806098078589046807, -0.9042721688041258643 ) ) ;
#204498 = CARTESIAN_POINT ( 'NONE',  ( -1.364683531250012516, 4.988541667008084879, -0.7879004041258300672 ) ) ;
#204499 = CARTESIAN_POINT ( 'NONE',  ( 6.092244811693771744, 1.020019244021443727, -1.792768071708307431 ) ) ;
#204500 = CARTESIAN_POINT ( 'NONE',  ( 9.002250809793993724, 11.52571191622492464, -1.443375672974057666 ) ) ;
#204501 = CARTESIAN_POINT ( 'NONE',  ( 4.200566210393744448, -0.6737006675727378324, -2.054019326127386691 ) ) ;
#204502 = CARTESIAN_POINT ( 'NONE',  ( 7.198453214212898743, 7.362893269528701268, 0.7998128361456291469 ) ) ;
#204503 = CARTESIAN_POINT ( 'NONE',  ( -0.7499999999999972244, 5.858333333333353821, -1.299038105676652011 ) ) ;
#204505 = CARTESIAN_POINT ( 'NONE',  ( 8.762124912781171560, 3.934209603697781166, 7.549522310265921021 ) ) ;
#204504 = CARTESIAN_POINT ( 'NONE',  ( 4.844006021832467646, 8.873367135438366304, 0.000000000000000000 ) ) ;
#204506 = CARTESIAN_POINT ( 'NONE',  ( 7.171900071504736296, 9.390302721554109056, -1.443375672974058777 ) ) ;
#204508 = LINE ( 'NONE', #138486, #83379 ) ;
#204507 = CARTESIAN_POINT ( 'NONE',  ( 1.557326333469456481, 1.775469013113859074, -1.249449068179921518 ) ) ;
#204510 = CARTESIAN_POINT ( 'NONE',  ( 1.452429406588066740, -1.579491434881035827, -0.9459884711465746943 ) ) ;
#204509 = CARTESIAN_POINT ( 'NONE',  ( -4.609409038966234995, 7.361099064560491456, -1.082531754730549967 ) ) ;
#204511 = CARTESIAN_POINT ( 'NONE',  ( -1.364683531250012516, 3.030208333674755394, 0.7879004041258379498 ) ) ;
#204512 = CARTESIAN_POINT ( 'NONE',  ( 2.736070936638954176, 2.175344985778558726, 0.2654339622269741295 ) ) ;
#204513 = CARTESIAN_POINT ( 'NONE',  ( 6.883263157960367806, 6.035304072343574688, 2.648703854151325032 ) ) ;
#204514 = CARTESIAN_POINT ( 'NONE',  ( 3.784249319668216760, -1.117672106238891461, 1.967118024168002410 ) ) ;
#204515 = CARTESIAN_POINT ( 'NONE',  ( -7.203459687562382641, 7.298457811777897319, -0.7998128361456291469 ) ) ;
#204516 = DIRECTION ( 'NONE',  ( -1.000000000000000000, 7.771561172376097755E-16, 4.440892098500627148E-16 ) ) ;
#204517 = CARTESIAN_POINT ( 'NONE',  ( 5.954584599377941601, 7.113081392617206511, -1.094866876611422235 ) ) ;
#204518 = AXIS2_PLACEMENT_3D ( 'NONE', #123971, #170484, #5823 ) ;
#204519 = CARTESIAN_POINT ( 'NONE',  ( 0.7500000000000006661, 13.41666666666666785, -1.299038105676657340 ) ) ;
#204520 = CARTESIAN_POINT ( 'NONE',  ( 5.939880696562888751, 7.062853913145737295, -1.082531754730548412 ) ) ;
#204521 = CARTESIAN_POINT ( 'NONE',  ( 5.923074920120706466, -0.04171666621876138348, 1.769427632397130079 ) ) ;
#204522 = CARTESIAN_POINT ( 'NONE',  ( 3.563142721848435279, -1.644496397275853505, 1.160845683069864798 ) ) ;
#204523 = CARTESIAN_POINT ( 'NONE',  ( 7.476431642932036326, 10.80992178580769014, 1.199719254218460707 ) ) ;
#204524 = CARTESIAN_POINT ( 'NONE',  ( 2.010898292529788467, 1.560970962663108752, -1.413861550561988922 ) ) ;
#204526 = CARTESIAN_POINT ( 'NONE',  ( -1.500000000000013101, 0.6708333333333583726, 0.8660254037844403729 ) ) ;
#204525 = CARTESIAN_POINT ( 'NONE',  ( 1.364683531249997417, 10.98437500034139802, 2.602085213965210642E-15 ) ) ;
#204527 = CARTESIAN_POINT ( 'NONE',  ( 1.451539297965124264, 1.489159454907125646, 1.289083465231783299 ) ) ;
#204528 = LINE ( 'NONE', #108198, #936 ) ;
#204529 = DIRECTION ( 'NONE',  ( 0.7592566023653005702, 0.6507913734559639396, 0.000000000000000000 ) ) ;
#204531 = EDGE_LOOP ( 'NONE', ( #43091, #136857, #2364, #115177, #119995, #152541, #127593, #113938 ) ) ;
#204530 = CARTESIAN_POINT ( 'NONE',  ( 5.431847905162764611, -1.765542832439458198, 0.4050695418617160648 ) ) ;
#204532 = CARTESIAN_POINT ( 'NONE',  ( 5.450014563013511726, 8.341805509282339770, -1.082531754730543083 ) ) ;
#204533 = AXIS2_PLACEMENT_3D ( 'NONE', #120232, #53017, #104991 ) ;
#204534 = CARTESIAN_POINT ( 'NONE',  ( 0.6823417656249882723, -0.09479166632524876901, 1.181850606188755259 ) ) ;
#204535 = EDGE_CURVE ( 'NONE', #166283, #105851, #183173, .T. ) ;
#204536 = CARTESIAN_POINT ( 'NONE',  ( 4.908994958506140094, 1.627828031611065152, 0.9215782234750914403 ) ) ;
#204537 = B_SPLINE_CURVE_WITH_KNOTS ( 'NONE', 3,
 ( #16187, #15132, #98539, #130057 ),
 .UNSPECIFIED., .F., .F.,
 ( 4, 4 ),
 ( 0.003367049630611286277, 0.004112888465975162409 ),
 .UNSPECIFIED. ) ;
#204538 = CARTESIAN_POINT ( 'NONE',  ( 5.243061650278370678, -0.2479348644398685908, -2.055265572831247667 ) ) ;
#204539 = CARTESIAN_POINT ( 'NONE',  ( 1.225000000000000311, 1.874999999999994671, -1.734723475976807094E-15 ) ) ;
#204540 = CARTESIAN_POINT ( 'NONE',  ( -5.112833325684908559, 8.018703742390766109, -1.082531754730549967 ) ) ;
#204541 = CARTESIAN_POINT ( 'NONE',  ( 1.496383747040779033, -0.9083167890128959199, -2.962306210641313164 ) ) ;
#204542 = CARTESIAN_POINT ( 'NONE',  ( 6.577677080924314801, 10.82570702772039262, 1.040834085586084257E-14 ) ) ;
#204543 = CARTESIAN_POINT ( 'NONE',  ( -9.667127221743832877, 11.23706883257798772, 1.199719254218462483 ) ) ;
#204544 = CARTESIAN_POINT ( 'NONE',  ( 5.982890925380405456, 10.20206618957764100, 0.000000000000000000 ) ) ;
#204545 = CARTESIAN_POINT ( 'NONE',  ( -1.402160292154681736E-14, -0.05312499965857903073, -1.575800808251665908 ) ) ;
#204546 = CARTESIAN_POINT ( 'NONE',  ( -0.7500000000000006661, 1.358333333333357151, -1.299038105676652011 ) ) ;
#204548 = CARTESIAN_POINT ( 'NONE',  ( 5.823390672269506574, 6.752709524857930745, -1.199719254218446718 ) ) ;
#204547 = CARTESIAN_POINT ( 'NONE',  ( 5.266048140081638351, -1.952571265509401854, 0.1905133553196102503 ) ) ;
#204549 = CARTESIAN_POINT ( 'NONE',  ( 2.003279617838377824, 1.993765885540278004, 0.2985825316763612847 ) ) ;
#204550 = CARTESIAN_POINT ( 'NONE',  ( 1.284279953904119864, 2.827889714876734129, -0.7749999999999910294 ) ) ;
#204551 = CARTESIAN_POINT ( 'NONE',  ( 0.1874131419884322858, 1.628132678060219884, 1.467219630700428157 ) ) ;
#204552 = CARTESIAN_POINT ( 'NONE',  ( 4.019144481351099252, -2.000086177330139492, 0.6089195546459759134 ) ) ;
#204553 = CARTESIAN_POINT ( 'NONE',  ( 1.809613641711980359, -1.857008771552502768, 0.2239427725650791623 ) ) ;
#204554 = CARTESIAN_POINT ( 'NONE',  ( 1.364683531249988535, 4.655208333674755394, -0.7879004041258300672 ) ) ;
#204555 = CARTESIAN_POINT ( 'NONE',  ( 4.008068315354725186, -0.7665524943986418149, 1.861746286504823988 ) ) ;
#204556 = CARTESIAN_POINT ( 'NONE',  ( -7.483210719738908168, 10.81783070874899799, 1.199719254218453823 ) ) ;
#204558 = CARTESIAN_POINT ( 'NONE',  ( 3.093478398350542946, -0.4104027421963015732, 2.076914780291692519 ) ) ;
#204557 = CARTESIAN_POINT ( 'NONE',  ( -3.945059511896602089, 7.546393830613923548, 1.040834085586084257E-14 ) ) ;
#204559 = CARTESIAN_POINT ( 'NONE',  ( -0.08832626591289140239, -9.919998018383708427, -9.499595568239943333 ) ) ;
#204560 = CARTESIAN_POINT ( 'NONE',  ( 4.809070886388271404, -1.664838503569150419, 1.230558894880565246 ) ) ;
#204561 = CARTESIAN_POINT ( 'NONE',  ( 5.155843554946782703, 9.237177590738404831, -0.7998128361456481317 ) ) ;
#204563 = CARTESIAN_POINT ( 'NONE',  ( 6.620655732516625314, 7.629137130509059617, 2.773739711112707340 ) ) ;
#204562 = CARTESIAN_POINT ( 'NONE',  ( 0.9606207175340542026, -1.891748053602306578, -0.8905051939756128965 ) ) ;
#204565 = ORIENTED_EDGE ( 'NONE', *, *, #50840, .T. ) ;
#204564 = CARTESIAN_POINT ( 'NONE',  ( 6.176747059734421619, -1.734417727105644680, -0.5698399933231483860 ) ) ;
#204566 = EDGE_CURVE ( 'NONE', #88062, #164595, #101010, .T. ) ;
#204567 = CARTESIAN_POINT ( 'NONE',  ( 6.577677080924314801, 10.82570702772039262, 1.040834085586084257E-14 ) ) ;
#204568 = CARTESIAN_POINT ( 'NONE',  ( 1.734723475976807094E-15, 14.56776713488954655, 11.92913357381758388 ) ) ;
#204569 = DIRECTION ( 'NONE',  ( 0.000000000000000000, -0.000000000000000000, 1.000000000000000000 ) ) ;
#204570 = CARTESIAN_POINT ( 'NONE',  ( -10.78913822082115281, 5.463154562124156399, 6.589184675844935057 ) ) ;
#204571 = CARTESIAN_POINT ( 'NONE',  ( -1.908029163539572748, 3.237038651130945244, 0.4603255239806047228 ) ) ;
#204572 = CARTESIAN_POINT ( 'NONE',  ( 6.498695769366850783, -1.876353784076413067, -0.3680397143606057853 ) ) ;
#204573 = CARTESIAN_POINT ( 'NONE',  ( -8.518600588087975822, 8.832788862391110385, 1.040834085586084257E-14 ) ) ;
#204574 = CARTESIAN_POINT ( 'NONE',  ( 4.659198344590585350, 8.587481835331020719, 0.7998128361456462443 ) ) ;
#204575 = AXIS2_PLACEMENT_3D ( 'NONE', #148671, #86862, #136693 ) ;
#204576 = CARTESIAN_POINT ( 'NONE',  ( -9.474246188248169886, -6.532648833121168508, 0.3333842132581058548 ) ) ;
#204577 = EDGE_CURVE ( 'NONE', #89251, #38200, #72104, .T. ) ;
#204578 = CARTESIAN_POINT ( 'NONE',  ( 4.844340958784499662, 4.546152628203684820, 0.7998128361456341429 ) ) ;
#204579 = ORIENTED_EDGE ( 'NONE', *, *, #143132, .T. ) ;
#204580 = CARTESIAN_POINT ( 'NONE',  ( 5.589470316598125876, -0.4871849528341637425, 1.956566939648955339 ) ) ;
#204581 = CYLINDRICAL_SURFACE ( 'NONE', #76582, 2.750000000000000444 ) ;
#204582 = CARTESIAN_POINT ( 'NONE',  ( 0.5227789990447535562, -7.252376619629073204E-15, -1.145890942912077826 ) ) ;
#204583 = CARTESIAN_POINT ( 'NONE',  ( 0.1394461523056798324, 0.009327122704651937685, -1.719853553173174232 ) ) ;
#204584 = CARTESIAN_POINT ( 'NONE',  ( -5.802526556968872207, 6.832331073627524454, 1.082531754730548412 ) ) ;
#204585 = CARTESIAN_POINT ( 'NONE',  ( 4.383363735919856730, 4.008345868194933104, -0.7998128361456211532 ) ) ;
#204586 = CARTESIAN_POINT ( 'NONE',  ( 3.203910658309446990, 0.7132968404394635087, -1.835904812064126590 ) ) ;
#204587 = CARTESIAN_POINT ( 'NONE',  ( 4.710564641745673242, 1.930423983604495630, 0.5826390268678026674 ) ) ;
#204588 = CARTESIAN_POINT ( 'NONE',  ( -7.369020184227459858, 8.555943955475521889, 1.199719254218450271 ) ) ;
#204589 = CARTESIAN_POINT ( 'NONE',  ( -9.490416961614045022, -9.037429132956699362, 0.4317745627846718559 ) ) ;
#204590 = CARTESIAN_POINT ( 'NONE',  ( 4.611385148785618782, -2.149487334021232599, 0.4259423572047504880 ) ) ;
#204591 = FACE_OUTER_BOUND ( 'NONE', #210625, .T. ) ;
#204592 = CARTESIAN_POINT ( 'NONE',  ( 2.924735480247532937, 1.813364411391896969, 0.6504805730627157834 ) ) ;
#204593 = CARTESIAN_POINT ( 'NONE',  ( -8.483651433849100698, 10.92067931095586886, 1.599625672291269396 ) ) ;
#204594 = CARTESIAN_POINT ( 'NONE',  ( -0.1298852118743893114, 2.060165343084968459, -2.144168685196511159 ) ) ;
#204595 = LINE ( 'NONE', #56248, #129762 ) ;
#204596 = EDGE_CURVE ( 'NONE', #89693, #200465, #27783, .T. ) ;
#204597 = CARTESIAN_POINT ( 'NONE',  ( -4.933501523973760072E-10, 15.51845925587262798, -12.00000000000000178 ) ) ;
#204598 = CARTESIAN_POINT ( 'NONE',  ( -6.755468634461358590, 14.48046873815656177, 9.927994241953896903 ) ) ;
#204599 = CARTESIAN_POINT ( 'NONE',  ( 4.635998460869027227, 7.496083073400806818, -1.199719254218452047 ) ) ;
#204600 = ORIENTED_EDGE ( 'NONE', *, *, #39272, .F. ) ;
#204601 = CARTESIAN_POINT ( 'NONE',  ( 4.828112100242277549, 6.726159765073026264, -1.443375672974068769 ) ) ;
#204602 = EDGE_LOOP ( 'NONE', ( #47341, #107053, #69395, #133928 ) ) ;
#204603 = VERTEX_POINT ( 'NONE', #199400 ) ;
#204605 = CARTESIAN_POINT ( 'NONE',  ( 2.508449741805112154, -2.007837557984166299, -0.1460343770829114485 ) ) ;
#204604 = CARTESIAN_POINT ( 'NONE',  ( 0.1517630622446651534, 0.7442075171455504456, 1.793999140845178530 ) ) ;
#204606 = CARTESIAN_POINT ( 'NONE',  ( 4.991759546967353245, 2.197549137908102246, 0.6733019004761026105 ) ) ;
#204608 = CARTESIAN_POINT ( 'NONE',  ( 3.256551146222384396, -0.5358571751262303229, -1.782154170384263603 ) ) ;
#204607 = CARTESIAN_POINT ( 'NONE',  ( -7.608060475923978494, 8.905100639113307182, 1.199719254218452047 ) ) ;
#204609 = DIRECTION ( 'NONE',  ( 5.578564026256490882E-16, 1.000000000000000000, 9.066213480720158442E-32 ) ) ;
#204610 = DIRECTION ( 'NONE',  ( -0.000000000000000000, 1.000000000000000000, -0.000000000000000000 ) ) ;
#204611 = CARTESIAN_POINT ( 'NONE',  ( 6.205323455156911194, 1.660478276859885582, -0.9486371710855368011 ) ) ;
#204612 = CARTESIAN_POINT ( 'NONE',  ( -8.016948904382338981, 8.247528564734524892, -0.7998128361456291469 ) ) ;
#204613 = CARTESIAN_POINT ( 'NONE',  ( -3.675669043080673770, 7.302381293653823491, 0.000000000000000000 ) ) ;
#204614 = CARTESIAN_POINT ( 'NONE',  ( 6.181206942494069878, 1.442326931096184151, 1.513799708994074900 ) ) ;
#204615 = CARTESIAN_POINT ( 'NONE',  ( 5.504247177468179153, 7.444707678511436555, 1.443375672974062551 ) ) ;
#204616 = ORIENTED_EDGE ( 'NONE', *, *, #106413, .T. ) ;
#204617 = FACE_OUTER_BOUND ( 'NONE', #172262, .T. ) ;
#204618 = CARTESIAN_POINT ( 'NONE',  ( 3.094265954482833703, 2.800000000000017586, -2.490342512183683965 ) ) ;
#204619 = CARTESIAN_POINT ( 'NONE',  ( 0.9788029507734037349, -0.04229004422508231970, -1.825371421953936757 ) ) ;
#204620 = CARTESIAN_POINT ( 'NONE',  ( -4.303823697334223652, 7.108545849276850959, -1.199719254218452047 ) ) ;
#204621 = CARTESIAN_POINT ( 'NONE',  ( 2.654579492894239223, 0.9294799389642364185, 1.463784073337747849 ) ) ;
#204622 = LINE ( 'NONE', #60522, #57768 ) ;
#204623 = FACE_OUTER_BOUND ( 'NONE', #14717, .T. ) ;
#204624 = CARTESIAN_POINT ( 'NONE',  ( -5.181187258716735577, 9.196468901811520880, 0.7998128361456481317 ) ) ;
#204625 = CARTESIAN_POINT ( 'NONE',  ( 0.08058608058606961388, -5.907420853759267843, -10.99970480893079738 ) ) ;
#204626 = CARTESIAN_POINT ( 'NONE',  ( 0.2333690889706682703, 0.003390530909083006028, -2.053566628440507635 ) ) ;
#204627 = CARTESIAN_POINT ( 'NONE',  ( 6.006453938882227561, -0.6616566355047011072, -1.701761020394356283 ) ) ;
#204628 = CARTESIAN_POINT ( 'NONE',  ( 3.274216958324972726, -0.9628348462043828659, -1.709115330885315309 ) ) ;
#204629 = CARTESIAN_POINT ( 'NONE',  ( -0.6125000000000192513, -0.9791666659838688114, -1.060881119635955327 ) ) ;
#204630 = CARTESIAN_POINT ( 'NONE',  ( -7.316596452869116973, 11.68777962832266049, 0.7998128361456481317 ) ) ;
#204631 = CARTESIAN_POINT ( 'NONE',  ( 5.615048174354031474, 9.702639970055050966, 0.7998128361456462443 ) ) ;
#204632 = CARTESIAN_POINT ( 'NONE',  ( 4.108145954595856075, -0.8103754143699601897, 1.959725966023172727 ) ) ;
#204633 = CARTESIAN_POINT ( 'NONE',  ( -2.467220768007014176, 5.822248629409386922, 0.7216878364870317197 ) ) ;
#204634 = CARTESIAN_POINT ( 'NONE',  ( -9.996439331977562404, 10.55693406359564790, 0.7998128361456462443 ) ) ;
#204635 = PRESENTATION_LAYER_ASSIGNMENT (  '', '', ( #31820 ) ) ;
#204636 = CARTESIAN_POINT ( 'NONE',  ( 2.114207291064807759, 2.064986537539798661, -0.1480984254652456533 ) ) ;
#204637 = CARTESIAN_POINT ( 'NONE',  ( 1.579999999999991189, 8.674529973577531194, -2.499999999999989342 ) ) ;
#204639 = ORIENTED_EDGE ( 'NONE', *, *, #9755, .T. ) ;
#204638 = CARTESIAN_POINT ( 'NONE',  ( 5.092532722643547061, -1.235012376581679172, 1.846140261684477091 ) ) ;
#204640 = CARTESIAN_POINT ( 'NONE',  ( 2.268584743917153368, 2.099868620093465754, -0.9355518099330699666 ) ) ;
#204642 = CARTESIAN_POINT ( 'NONE',  ( 6.473490848629269045, -0.2583879851764906976, 2.046290913384725130 ) ) ;
#204641 = CARTESIAN_POINT ( 'NONE',  ( 9.734391104931951588, 11.41950637958454706, 1.082531754730548412 ) ) ;
#204644 = CARTESIAN_POINT ( 'NONE',  ( 1.001543065824772753E-15, -3.521874999522041083, 3.793834371823811669 ) ) ;
#204643 = CARTESIAN_POINT ( 'NONE',  ( 3.067887898442204442, 6.801229324816399746, 0.7998128361456271485 ) ) ;
#204645 = EDGE_CURVE ( 'NONE', #23400, #139590, #120693, .T. ) ;
#204646 = CYLINDRICAL_SURFACE ( 'NONE', #206549, 1.500000000000000222 ) ;
#204647 = CARTESIAN_POINT ( 'NONE',  ( 6.614805131849967879, -0.1256686391097518729, 1.812046779126045726 ) ) ;
#204648 = DIRECTION ( 'NONE',  ( -0.000000000000000000, 1.000000000000000000, -0.000000000000000000 ) ) ;
#204649 = EDGE_CURVE ( 'NONE', #18660, #188370, #85671, .T. ) ;
#204650 = CARTESIAN_POINT ( 'NONE',  ( 3.146637304467227558, 1.866760668956708447, 0.4145885930168375921 ) ) ;
#204651 = CARTESIAN_POINT ( 'NONE',  ( -0.2106725631050176961, 4.086973797293973476, -2.558389695104481554 ) ) ;
#204652 = CARTESIAN_POINT ( 'NONE',  ( 4.313312247719586878, -0.2936513069345859650, 1.699412160066446909 ) ) ;
#204653 = CARTESIAN_POINT ( 'NONE',  ( 2.466030083290056130, -1.032479112849067793, 1.731996155473938481 ) ) ;
#204654 = CARTESIAN_POINT ( 'NONE',  ( 4.096513536321761073, -0.3929280286100769182, 2.264727396410810556 ) ) ;
#204655 = CARTESIAN_POINT ( 'NONE',  ( 3.462467831702148668, 1.013738371934786331, 2.022624228200241348 ) ) ;
#204656 = CARTESIAN_POINT ( 'NONE',  ( 6.199853529602823876, -0.7113111419616345854, 1.982453129600779462 ) ) ;
#204657 = CARTESIAN_POINT ( 'NONE',  ( -5.695833931516914639, 6.778132687258748845, 1.082531754730549078 ) ) ;
#204658 = CARTESIAN_POINT ( 'NONE',  ( 4.833122733705673468, -1.618250600028045216, 0.7167863974541763827 ) ) ;
#204660 = CARTESIAN_POINT ( 'NONE',  ( 1.131297326486919497, -2.070297854115164871, 0.9843215409001818683 ) ) ;
#204659 = CARTESIAN_POINT ( 'NONE',  ( 6.176621499477501054, 9.363752961769195693, -1.199719254218452047 ) ) ;
#204661 = CARTESIAN_POINT ( 'NONE',  ( 6.070224334863941529, -1.749758606415029449, -0.5730458292283467925 ) ) ;
#204662 = CARTESIAN_POINT ( 'NONE',  ( -4.135400547368138113, 4.783387712472935149, 1.199719254218462483 ) ) ;
#204663 = CIRCLE ( 'NONE', #52541, 6.329999999999995630 ) ;
#204664 = CARTESIAN_POINT ( 'NONE',  ( 5.701184558104195332, -0.5354452791076976803, 2.124913622581547479 ) ) ;
#204665 = CARTESIAN_POINT ( 'NONE',  ( -3.755772246185468788, 4.340488027759846545, -1.199719254218452047 ) ) ;
#204666 = CARTESIAN_POINT ( 'NONE',  ( -10.36809559534898284, -7.321523296574929063, 0.4642244361878736236 ) ) ;
#204667 = CARTESIAN_POINT ( 'NONE',  ( 6.391088794356012848, 0.1989163192229244648, 2.060770550043041993 ) ) ;
#204668 = ADVANCED_FACE ( 'NONE', ( #102996 ), #9915, .T. ) ;
#204669 = CARTESIAN_POINT ( 'NONE',  ( 10.12374542407608935, 0.7598076211376182387, -4.551898349974264235 ) ) ;
#204670 = CARTESIAN_POINT ( 'NONE',  ( -1.500000000000015099, -1.047916665983845919, 0.8660254037844403729 ) ) ;
#204671 = CARTESIAN_POINT ( 'NONE',  ( 3.844294682379956640, 1.917307101836130512, 0.1879692045662837430 ) ) ;
#204672 = CARTESIAN_POINT ( 'NONE',  ( 0.6823417656249934904, 10.94270833367473550, 1.181850606188764807 ) ) ;
#204673 = CARTESIAN_POINT ( 'NONE',  ( 0.000000000000000000, 9.719999999999982876, 0.000000000000000000 ) ) ;
#204674 = CARTESIAN_POINT ( 'NONE',  ( 1.406790049154776234, -2.211310019597735987, -0.2114152780076440363 ) ) ;
#204676 = EDGE_LOOP ( 'NONE', ( #129937, #142109, #39607, #61007 ) ) ;
#204675 = DIRECTION ( 'NONE',  ( 0.000000000000000000, 0.000000000000000000, -1.000000000000000000 ) ) ;
#204677 = DIRECTION ( 'NONE',  ( 1.000000000000000000, 0.000000000000000000, 0.000000000000000000 ) ) ;
#204678 = CARTESIAN_POINT ( 'NONE',  ( 8.516493047678546091, 13.08765898893368629, -0.7998128361456352531 ) ) ;
#204679 = CARTESIAN_POINT ( 'NONE',  ( -4.406036734316898240, 6.163462161501578329, -1.443375672974051449 ) ) ;
#204680 = CARTESIAN_POINT ( 'NONE',  ( -1.874158809982213958, 3.299964346911606228, -0.4000000000000374922 ) ) ;
#204681 = CARTESIAN_POINT ( 'NONE',  ( 10.65531535955785536, 9.862547934939467353, 5.420879958757526929 ) ) ;
#204682 = CARTESIAN_POINT ( 'NONE',  ( 8.365017589507326434, 12.70301158782650397, -0.7216878364870338292 ) ) ;
#204684 = CARTESIAN_POINT ( 'NONE',  ( 1.680054527999317759, -1.087118939145682583, -1.632918184844594611 ) ) ;
#204683 = AXIS2_PLACEMENT_3D ( 'NONE', #184079, #69243, #70308 ) ;
#204685 = CARTESIAN_POINT ( 'NONE',  ( -1.402160292154681736E-14, 2.259375000341416140, -1.575800808251660134 ) ) ;
#204686 = CARTESIAN_POINT ( 'NONE',  ( 9.569423160901791903, -7.256398209936433474, 9.269928574751062911E-15 ) ) ;
#204687 = CARTESIAN_POINT ( 'NONE',  ( 6.373494408814909917, -0.2414686440028299685, 1.946897059556201848 ) ) ;
#204688 = CARTESIAN_POINT ( 'NONE',  ( -9.508345801885592863, 9.987491611821676329, 0.7998128361456462443 ) ) ;
#204689 = CARTESIAN_POINT ( 'NONE',  ( -5.382223794500845315, 6.341977850748185652, -1.082531754730543971 ) ) ;
#204690 = CARTESIAN_POINT ( 'NONE',  ( 0.4622851218389683603, 2.237382594954186565, -0.3354954470186234383 ) ) ;
#204692 = ORIENTED_EDGE ( 'NONE', *, *, #120407, .T. ) ;
#204691 = CARTESIAN_POINT ( 'NONE',  ( -6.230135280679522936, 7.227244901336242755, 1.199719254218450271 ) ) ;
#204693 = CARTESIAN_POINT ( 'NONE',  ( 0.7499999999999867883, -0.9020833326505162120, -1.299038105676652011 ) ) ;
#204694 = CARTESIAN_POINT ( 'NONE',  ( 1.088877184111051832, 1.652420591378000791, -0.8765777015899289815 ) ) ;
#204695 = CARTESIAN_POINT ( 'NONE',  ( 6.884150274805287850, -0.1404709382532287054, 1.702994612897957394 ) ) ;
#204697 = CARTESIAN_POINT ( 'NONE',  ( 4.265290774032561849, 2.125562838249666964, -0.5332280334861272397 ) ) ;
#204696 = CARTESIAN_POINT ( 'NONE',  ( -4.757329562667670667E-14, 1.953125000341451312, 1.570758158831762286 ) ) ;
#204698 = CARTESIAN_POINT ( 'NONE',  ( 4.436755630409714435, 2.262211819008316027, 0.4546042144240244887 ) ) ;
#204699 = CARTESIAN_POINT ( 'NONE',  ( 0.1630570004950296636, -1.840724325608022127, -0.9269800520197747362 ) ) ;
#204700 = CARTESIAN_POINT ( 'NONE',  ( 2.818227900350485982, 1.828750386608999356, 0.6536940613037258707 ) ) ;
#204701 = CARTESIAN_POINT ( 'NONE',  ( -6.046573321570485327, 6.156683084694754449, 0.000000000000000000 ) ) ;
#204702 = CARTESIAN_POINT ( 'NONE',  ( 5.099275172515607579, 5.121778254122544283, -0.7216878364870458196 ) ) ;
#204703 = CARTESIAN_POINT ( 'NONE',  ( 0.6801582343749970061, 0.5572916670080683144, -1.178068619123862515 ) ) ;
#204704 = CARTESIAN_POINT ( 'NONE',  ( 3.938125092175647879, -1.678004675797317713, -1.117833462672225497 ) ) ;
#204705 = CARTESIAN_POINT ( 'NONE',  ( -3.755245360860919757, 7.324943987738961049, -0.7216878364870257245 ) ) ;
#204706 = CARTESIAN_POINT ( 'NONE',  ( -5.908321080505254841, 10.11506803722328129, 0.7998128361456291469 ) ) ;
#204707 = CARTESIAN_POINT ( 'NONE',  ( 10.58621901417202515, 11.24501035948919991, -0.7998128361456281477 ) ) ;
#204708 = CARTESIAN_POINT ( 'NONE',  ( 0.5920835508136900183, -1.811502216344462735, -0.2265648652611390590 ) ) ;
#204709 = CARTESIAN_POINT ( 'NONE',  ( -5.424143973919053785, 8.485862515284315677, 1.199719254218454489 ) ) ;
#204710 = CARTESIAN_POINT ( 'NONE',  ( -3.983063267364693960, 7.868933921892603323, -0.7998128361456481317 ) ) ;
#204711 = CARTESIAN_POINT ( 'NONE',  ( -11.38450596090590849, 3.710255710271473273, 5.708599601896569453 ) ) ;
#204712 = ORIENTED_EDGE ( 'NONE', *, *, #138377, .F. ) ;
#204713 = CARTESIAN_POINT ( 'NONE',  ( 5.981337812661591258, 1.905142945929317211, -0.7864339424841911841 ) ) ;
#204714 = B_SPLINE_CURVE_WITH_KNOTS ( 'NONE', 3,
 ( #159870, #59162, #42946, #27735, #174019, #172937, #23446, #10403, #25588, #109055 ),
 .UNSPECIFIED., .F., .F.,
 ( 4, 3, 3, 4 ),
 ( 0.000000000000000000, 3.125151129215626700E-05, 5.612054754981304444E-05, 8.099579648775786166E-05 ),
 .UNSPECIFIED. ) ;
#204715 = CARTESIAN_POINT ( 'NONE',  ( -7.417719440008134768, 7.826629899530511025, 0.7216878364870317197 ) ) ;
#204716 = CARTESIAN_POINT ( 'NONE',  ( 5.043269954603521121, 4.986162489900023864, -0.7216878364870420448 ) ) ;
#204717 = CARTESIAN_POINT ( 'NONE',  ( -3.741160322367112379, 6.452105245148518797, 1.199719254218464037 ) ) ;
#204718 = CARTESIAN_POINT ( 'NONE',  ( -8.435144125996554720, 12.99275191363802229, 0.7998128361456341429 ) ) ;
#204719 = CARTESIAN_POINT ( 'NONE',  ( 5.813150814160550794, 1.649844410012293539, -1.164645984317608463 ) ) ;
#204720 = CARTESIAN_POINT ( 'NONE',  ( 5.197972062552532080, 1.490711083722006780, 1.646940351458234808 ) ) ;
#204721 = CARTESIAN_POINT ( 'NONE',  ( -4.248501033035892327, 6.049946853332221153, -1.599625672291271394 ) ) ;
#204722 = CARTESIAN_POINT ( 'NONE',  ( 6.331821432781979730, 7.345878745455822312, -1.199719254218445830 ) ) ;
#204723 = CARTESIAN_POINT ( 'NONE',  ( 4.276283029400809177, -1.188189442049456535, 1.683678490072185285 ) ) ;
#204724 = CARTESIAN_POINT ( 'NONE',  ( 3.604138833494671346, -0.1455340571130462057, 2.011204217620660373 ) ) ;
#204725 = VERTEX_POINT ( 'NONE', #133987 ) ;
#204726 = LINE ( 'NONE', #7602, #62650 ) ;
#204727 = DIRECTION ( 'NONE',  ( 0.01641209967245726292, -0.005323139086630727067, -0.9998511425080263137 ) ) ;
#204728 = VECTOR ( 'NONE', #49929, 1000.000000000000114 ) ;
#204730 = ORIENTED_EDGE ( 'NONE', *, *, #152121, .T. ) ;
#204729 = CARTESIAN_POINT ( 'NONE',  ( -7.618755976236585958, 7.853246491889623648, 0.000000000000000000 ) ) ;
#204731 = CARTESIAN_POINT ( 'NONE',  ( 4.890561790263044273, 8.149264200713410844, -1.004099907704804950 ) ) ;
#204732 = CARTESIAN_POINT ( 'NONE',  ( 4.499374939222855474, 1.976653413780619761, 0.3960398538903551757 ) ) ;
#204733 = CARTESIAN_POINT ( 'NONE',  ( 3.732213890823964597, 0.2717154217161937280, 1.820854149191558635 ) ) ;
#204734 = VECTOR ( 'NONE', #209116, 1000.000000000000000 ) ;
#204735 = CARTESIAN_POINT ( 'NONE',  ( 1.734723475976807094E-15, 15.43265149481033305, 11.92913362508773822 ) ) ;
#204736 = CARTESIAN_POINT ( 'NONE',  ( 1.893647147081824356, 2.006347305559322169, -1.140069799644787940 ) ) ;
#204737 = CARTESIAN_POINT ( 'NONE',  ( 5.259637247458703868, 5.100941308315409373, 0.000000000000000000 ) ) ;
#204738 = CARTESIAN_POINT ( 'NONE',  ( 3.181113218772323226, -0.1555236193923059951, -2.156033859764289407 ) ) ;
#204739 = CARTESIAN_POINT ( 'NONE',  ( 9.121938423896107651, 9.536683004167278099, -0.7998128361456221525 ) ) ;
#204740 = CARTESIAN_POINT ( 'NONE',  ( -4.238895582566952314, 8.097128612970093897, 1.040834085586084257E-14 ) ) ;
#204741 = CARTESIAN_POINT ( 'NONE',  ( 3.304404366906594337, -2.028264134497267168, 1.081039266028597234 ) ) ;
#204742 = DIRECTION ( 'NONE',  ( 1.000000000000000000, 0.000000000000000000, 0.000000000000000000 ) ) ;
#204743 = CARTESIAN_POINT ( 'NONE',  ( 2.061206331123175861, 0.3224310286589862629, -1.842498087946140561 ) ) ;
#204744 =( BOUNDED_CURVE ( )  B_SPLINE_CURVE ( 3, ( #104723, #70037, #21289, #67897 ),
 .UNSPECIFIED., .F., .T. ) 
 B_SPLINE_CURVE_WITH_KNOTS ( ( 4, 4 ),
 ( 0.6625062783165582836, 1.570796326794877462 ),
 .UNSPECIFIED. ) 
 CURVE ( )  GEOMETRIC_REPRESENTATION_ITEM ( )  RATIONAL_B_SPLINE_CURVE ( ( 1.000000000000000000, 0.9324242863012628391, 0.9324242863012628391, 1.000000000000000000 ) ) 
 REPRESENTATION_ITEM ( '' )  );
#204745 = CARTESIAN_POINT ( 'NONE',  ( 6.491095702449441340, 1.715375089605765124, -0.9715357305846801239 ) ) ;
#204747 = CARTESIAN_POINT ( 'NONE',  ( -5.912237504011027767, 9.055304967058290799, 1.199719254218454489 ) ) ;
#204746 = CARTESIAN_POINT ( 'NONE',  ( -1.364683531250012516, 4.488541667008090208, -0.7879004041258300672 ) ) ;
#204749 = CARTESIAN_POINT ( 'NONE',  ( 1.418904949497600487, 1.480075412272121582, -1.637148382315711359 ) ) ;
#204748 = CARTESIAN_POINT ( 'NONE',  ( -4.791917227426195858, 7.677988301050826969, -1.199719254218452047 ) ) ;
#204750 = CARTESIAN_POINT ( 'NONE',  ( 3.894033820048811823, 8.999999999999998224, -0.7749999999999996891 ) ) ;
#204751 = CARTESIAN_POINT ( 'NONE',  ( 5.331380718671758778, 7.243030143248949670, -1.599625672291256295 ) ) ;
#204752 = CARTESIAN_POINT ( 'NONE',  ( -3.737243898861318137, 7.511868315313511069, 0.7998128361456341429 ) ) ;
#204753 = FACE_OUTER_BOUND ( 'NONE', #174875, .T. ) ;
#204754 = CARTESIAN_POINT ( 'NONE',  ( 5.893431036533754330, 1.492594341498763466, 1.288039297220463730 ) ) ;
#204755 = CARTESIAN_POINT ( 'NONE',  ( 5.215558013723960329, -0.3431011331927047991, 2.281934296042067878 ) ) ;
#204756 = CARTESIAN_POINT ( 'NONE',  ( 0.6956633456795427994, -1.384754418207832405, -1.389998539416361423 ) ) ;
#204757 = CARTESIAN_POINT ( 'NONE',  ( 2.764570516439817549, -0.7852151221510113022, -1.907448154738192514 ) ) ;
#204758 = CARTESIAN_POINT ( 'NONE',  ( 6.724481002698112775, 8.868313807946373473, -1.443375672974057666 ) ) ;
#204759 = CARTESIAN_POINT ( 'NONE',  ( 5.494797395288433250, 9.632623737803665875, 0.000000000000000000 ) ) ;
#204760 = CARTESIAN_POINT ( 'NONE',  ( 5.788968402910795064, 9.697620870130524651, 0.7216878364870438212 ) ) ;
#204761 = CARTESIAN_POINT ( 'NONE',  ( -1.201851678989727383E-14, 3.259375000341420581, -1.575800808251660134 ) ) ;
#204762 = CARTESIAN_POINT ( 'NONE',  ( -9.367496997750912158, 14.48154074412965997, 7.499999999808506068 ) ) ;
#204763 = CARTESIAN_POINT ( 'NONE',  ( 3.497640442201256139, 7.024404915969360452, 1.040834085586084257E-14 ) ) ;
#204764 = CARTESIAN_POINT ( 'NONE',  ( 5.406739488685087025, 0.6250254011054052761, 2.079287783280135304 ) ) ;
#204766 = CARTESIAN_POINT ( 'NONE',  ( 5.513187957602974976, -1.795010045117376496, 0.4093405989887277663 ) ) ;
#204765 = CYLINDRICAL_SURFACE ( 'NONE', #80509, 1.224999999999996980 ) ;
#204767 = DIRECTION ( 'NONE',  ( 0.000000000000000000, -1.000000000000000000, 0.000000000000000000 ) ) ;
#204768 = CARTESIAN_POINT ( 'NONE',  ( 1.919777701841143713, 3.227564709615617033, 0.3999999999999849787 ) ) ;
#204769 = CARTESIAN_POINT ( 'NONE',  ( 0.4384654110765589530, 0.3132546388123040870, 1.843968665737522050 ) ) ;
#204770 = CARTESIAN_POINT ( 'NONE',  ( 0.3864610594027502732, -1.064975819449946126, 1.996106434226818216 ) ) ;
#204771 = CARTESIAN_POINT ( 'NONE',  ( -5.011569529345123897, 6.785514760743092566, 1.449221747052743092 ) ) ;
#204772 = CARTESIAN_POINT ( 'NONE',  ( -1.999999999999996669, 8.900000000000019895, 1.214306433183764966E-14 ) ) ;
#204773 = CARTESIAN_POINT ( 'NONE',  ( 5.753927575595171540, 7.371122731025397279, 1.306365966420112601 ) ) ;
#204774 = AXIS2_PLACEMENT_3D ( 'NONE', #114870, #178764, #115933 ) ;
#204775 = CARTESIAN_POINT ( 'NONE',  ( -0.05814382529654647802, -1.176414490726215734, -1.508152472379259867 ) ) ;
#204776 = CARTESIAN_POINT ( 'NONE',  ( 2.025891818203702233, 1.021928659931588435, -1.444778566663025954 ) ) ;
#204777 = CARTESIAN_POINT ( 'NONE',  ( -0.1108833634136767443, 0.0002062650063822807356, -1.896853557917008271 ) ) ;
#204779 = CARTESIAN_POINT ( 'NONE',  ( 2.899894056866093361, -0.9465274319002868753, -1.665356295385928442 ) ) ;
#204778 = CARTESIAN_POINT ( 'NONE',  ( -10.10098813738111545, 11.74323990082152491, -1.199719254218441611 ) ) ;
#204780 = FACE_OUTER_BOUND ( 'NONE', #200608, .T. ) ;
#204781 = CARTESIAN_POINT ( 'NONE',  ( 4.193778028305522376, -1.356587754280412339, -1.428115657216560974 ) ) ;
#204783 = EDGE_CURVE ( 'NONE', #5098, #149263, #188019, .T. ) ;
#204782 = CARTESIAN_POINT ( 'NONE',  ( 0.1410940620840978044, 2.031152781523197337, 0.6094965309384676733 ) ) ;
#204784 = CARTESIAN_POINT ( 'NONE',  ( -3.297657676621885692, 4.870353260857385180, 1.599625672291267398 ) ) ;
#204785 = CARTESIAN_POINT ( 'NONE',  ( 2.623731232481395725, -1.075365945362505293, -1.530472918023266571 ) ) ;
#204787 = EDGE_LOOP ( 'NONE', ( #188115, #189674, #66306, #183203 ) ) ;
#204786 = CARTESIAN_POINT ( 'NONE',  ( 6.270102258788001315, 0.8933021238881621029, 1.475393591635131507 ) ) ;
#204789 = CARTESIAN_POINT ( 'NONE',  ( -10.90207482560803420, -7.666862915010147717, 0.6254314485565921622 ) ) ;
#204788 = CARTESIAN_POINT ( 'NONE',  ( 2.772332522587173997, 1.181257105606844160, 1.863944272329665086 ) ) ;
#204790 = CARTESIAN_POINT ( 'NONE',  ( -1.364683531250012516, 3.592708333674750509, 0.7879004041258379498 ) ) ;
#204791 = CARTESIAN_POINT ( 'NONE',  ( 6.514115657861259123, 1.956686900881845714, -0.1430618042221123987 ) ) ;
#204793 = EDGE_CURVE ( 'NONE', #210292, #196229, #61781, .T. ) ;
#204792 = CARTESIAN_POINT ( 'NONE',  ( 8.423693512792301163, 8.722063941212843119, 0.7998128361456481317 ) ) ;
#204794 = CARTESIAN_POINT ( 'NONE',  ( 8.283668668269706714, 8.766627655843896250, 1.040834085586084257E-14 ) ) ;
#204795 = DIRECTION ( 'NONE',  ( -1.000000000000000000, -2.210062264950106756E-32, 1.224646799147353207E-16 ) ) ;
#204796 = CARTESIAN_POINT ( 'NONE',  ( -3.420250508247430155, -0.02876672507465954931, -0.2938434605158617985 ) ) ;
#204797 = AXIS2_PLACEMENT_3D ( 'NONE', #99016, #137658, #86757 ) ;
#204798 = FACE_OUTER_BOUND ( 'NONE', #165922, .T. ) ;
#204799 = VERTEX_POINT ( 'NONE', #186954 ) ;
#204800 = CARTESIAN_POINT ( 'NONE',  ( 3.543477799061961253, 1.872898848466747479, -0.8826743078152868849 ) ) ;
#204801 = CARTESIAN_POINT ( 'NONE',  ( -0.7500000000000215383, 3.441666666666689967, 1.299038105676671107 ) ) ;
#204802 = CARTESIAN_POINT ( 'NONE',  ( 6.159481859310094620, 6.080483678816896109, 1.040834085586084257E-14 ) ) ;
#204803 = CARTESIAN_POINT ( 'NONE',  ( -6.584207447892295839, 6.778236197985048506, 0.3223495580488393575 ) ) ;
#204804 = CARTESIAN_POINT ( 'NONE',  ( 0.3815177477655702920, 0.1955376695662625619, -2.010167716959633033 ) ) ;
#204805 = CARTESIAN_POINT ( 'NONE',  ( -1.201851678989727383E-14, 3.571875000341422357, 1.575800808251672791 ) ) ;
#204806 = VERTEX_POINT ( 'NONE', #202109 ) ;
#204808 = CARTESIAN_POINT ( 'NONE',  ( 7.754900677336718395, 11.99120852362745460, -0.7216878364870267237 ) ) ;
#204807 = CARTESIAN_POINT ( 'NONE',  ( 0.1745949693968510408, 0.7659234433113177865, -1.841618699378000601 ) ) ;
#204809 = CARTESIAN_POINT ( 'NONE',  ( 4.903672622533054692, 0.3418847601762939337, 1.986741992616162245 ) ) ;
#204810 = CARTESIAN_POINT ( 'NONE',  ( 5.366386423658583205, -1.870495304593930097, -0.4130858509987145877 ) ) ;
#204811 = CARTESIAN_POINT ( 'NONE',  ( 6.539320575229276677, 6.035451701470580410, 2.698157228745074576 ) ) ;
#204812 = CARTESIAN_POINT ( 'NONE',  ( 4.265290774032561849, 2.125562838249666964, -0.5332280334861272397 ) ) ;
#204813 = CARTESIAN_POINT ( 'NONE',  ( 0.7499999999999902300, 2.514583334016148974, 1.299038105676669330 ) ) ;
#204814 = CARTESIAN_POINT ( 'NONE',  ( 2.812653035604309348, -0.5591599321941118639, -1.828790038765286452 ) ) ;
#204815 = CARTESIAN_POINT ( 'NONE',  ( -4.880045225915050189, 7.780804299287790826, 1.199719254218464037 ) ) ;
#204816 = CARTESIAN_POINT ( 'NONE',  ( 3.511198595814921219, 7.040222761851976152, 0.7216878364870317197 ) ) ;
#204818 = CARTESIAN_POINT ( 'NONE',  ( 6.603150282362637569, -0.1459358296138096867, 2.084196934165093662 ) ) ;
#204817 = CARTESIAN_POINT ( 'NONE',  ( 3.568415406894422492, 7.340509688221367846, -0.2824851646710802022 ) ) ;
#204819 = CARTESIAN_POINT ( 'NONE',  ( 1.364683531249997417, 10.54687500034139802, 2.602085213965210642E-15 ) ) ;
#204821 = CARTESIAN_POINT ( 'NONE',  ( -5.875479466675803231, 7.948088359245467416, -1.599625672291271394 ) ) ;
#204820 = CARTESIAN_POINT ( 'NONE',  ( 5.724229345562060089, 2.111793275502030554, 0.5857118945327836057 ) ) ;
#204823 = EDGE_LOOP ( 'NONE', ( #57654, #43404, #8861, #188954 ) ) ;
#204822 = CARTESIAN_POINT ( 'NONE',  ( 2.608071471510875039, -0.6576475463303601554, -1.594674760072743114 ) ) ;
#204824 = CARTESIAN_POINT ( 'NONE',  ( 5.798083248138522272, 9.916180889470295412, 0.7998128361456462443 ) ) ;
#204825 = CARTESIAN_POINT ( 'NONE',  ( 6.145923705696426431, 6.064665832934283962, 0.7998128361456341429 ) ) ;
#204826 = AXIS2_PLACEMENT_3D ( 'NONE', #80297, #164741, #99742 ) ;
#204827 = CARTESIAN_POINT ( 'NONE',  ( 3.469446951953614189E-15, 8.900000000000019895, 1.214306433183764966E-14 ) ) ;
#204828 = CARTESIAN_POINT ( 'NONE',  ( 0.5726126529861442771, 1.355618539282506640, -1.418395753018865113 ) ) ;
#204829 = CARTESIAN_POINT ( 'NONE',  ( 6.880414557363751626, -8.057948861126641660, -6.598949805828051574 ) ) ;
#204830 = CARTESIAN_POINT ( 'NONE',  ( 6.505214776458575265, 6.483838748823460563, 1.040834085586084257E-14 ) ) ;
#204831 = CARTESIAN_POINT ( 'NONE',  ( -1.500000000000001110, 10.77083333333333037, 0.8660254037844418162 ) ) ;
#204832 = ORIENTED_EDGE ( 'NONE', *, *, #84212, .T. ) ;
#204834 =( BOUNDED_SURFACE ( )  B_SPLINE_SURFACE ( 3, 2, ( 
 ( #89192, #140084, #41508 ),
 ( #208237, #56677, #7901 ),
 ( #188802, #24148, #27364 ),
 ( #8982, #123898, #75057 ),
 ( #155243, #6825, #93465 ),
 ( #141170, #72905, #139009 ),
 ( #205031, #122841, #172565 ),
 ( #173653, #175771, #90251 ),
 ( #109763, #207179, #77178 ),
 ( #40439, #121757, #105449 ),
 ( #209291, #159505, #11102 ),
 ( #73990, #42584, #106540 ),
 ( #156318, #143300, #187725 ),
 ( #206108, #58804, #39353 ) ),
 .UNSPECIFIED., .F., .F., .F. ) 
 B_SPLINE_SURFACE_WITH_KNOTS ( ( 4, 2, 2, 2, 2, 2, 4 ),
 ( 3, 3 ),
 ( -6.505213034913026604E-19, 0.002680181519792705202, 0.004020272279689058453, 0.005360363039585411271, 0.006700453799481764089, 0.008040544559378116907, 0.01072072607917082254 ),
 ( 0.000000000000000000, 1.000000000000000000 ),
 .UNSPECIFIED. ) 
 GEOMETRIC_REPRESENTATION_ITEM ( )  RATIONAL_B_SPLINE_SURFACE ( (
 ( 1.000000000000000000, 0.8509629433892340611, 1.000000000000000000),
 ( 1.000000000000000000, 0.8507311530181393966, 1.000000000000000000),
 ( 1.000000000000000000, 0.8494583134163782301, 1.000000000000000000),
 ( 1.000000000000000000, 0.8495296534838289171, 1.000000000000000000),
 ( 1.000000000000000000, 0.8498242239227816741, 1.000000000000000000),
 ( 1.000000000000000000, 0.8505549521784944167, 1.000000000000000000),
 ( 1.000000000000000000, 0.8509834526754082029, 1.000000000000000000),
 ( 1.000000000000000000, 0.8509410435525731620, 1.000000000000000000),
 ( 1.000000000000000000, 0.8504680959802140006, 1.000000000000000000),
 ( 1.000000000000000000, 0.8496964069595507318, 1.000000000000000000),
 ( 1.000000000000000000, 0.8493987049676730017, 1.000000000000000000),
 ( 1.000000000000000000, 0.8493809005009217428, 1.000000000000000000),
 ( 1.000000000000000000, 0.8507510709369977553, 1.000000000000000000),
 ( 1.000000000000000000, 0.8509629433967522694, 1.000000000000000000) ) ) 
 REPRESENTATION_ITEM ( '' )  SURFACE ( )  );
#204833 = CARTESIAN_POINT ( 'NONE',  ( -5.346851039111035320, 6.199209027673978412, 2.420000000000001261 ) ) ;
#204835 = ORIENTED_EDGE ( 'NONE', *, *, #180876, .T. ) ;
#204836 = CARTESIAN_POINT ( 'NONE',  ( 2.490610001455384470, -1.733883600701890737, -0.5244944224890700779 ) ) ;
#204837 = ORIENTED_EDGE ( 'NONE', *, *, #182421, .T. ) ;
#204838 = CARTESIAN_POINT ( 'NONE',  ( 10.05353459973327368, 11.68787744023238417, -1.199719254218440723 ) ) ;
#204839 = CARTESIAN_POINT ( 'NONE',  ( 4.549643065837591038, 7.465611455855944101, -1.199719254218452047 ) ) ;
#204840 = CARTESIAN_POINT ( 'NONE',  ( 4.055163089163640322, -1.574157218682000758, 0.8962264629079966793 ) ) ;
#204841 = CARTESIAN_POINT ( 'NONE',  ( 0.5150272702496164756, 3.543562648825416161, 0.3999758201171684791 ) ) ;
#204842 = LINE ( 'NONE', #155061, #93891 ) ;
#204843 = CARTESIAN_POINT ( 'NONE',  ( 5.150161082644886257, 6.468739049537000518, 1.195298158575591074 ) ) ;
#204845 = CARTESIAN_POINT ( 'NONE',  ( -8.012344526598182026E-15, 14.79687500034140157, -1.575800808251669460 ) ) ;
#204844 = CARTESIAN_POINT ( 'NONE',  ( 5.265987090187672415, -1.852092866064008803, 0.1821183643400964280 ) ) ;
#204846 = CARTESIAN_POINT ( 'NONE',  ( 2.179167455442470480, 1.482148263166820801, 1.213602503745815353 ) ) ;
#204847 = CARTESIAN_POINT ( 'NONE',  ( -11.14501278000869355, 7.223412960316487386, -3.546411330735405265 ) ) ;
#204848 = CARTESIAN_POINT ( 'NONE',  ( 5.054560120293923653, 7.862967615930308796, 1.113740650586869219 ) ) ;
#204849 = CARTESIAN_POINT ( 'NONE',  ( -6.329444829450759258, 6.903589915222720919, 0.7840647185534960206 ) ) ;
#204850 = CARTESIAN_POINT ( 'NONE',  ( 3.475000000000000533, -2.610416665710752593, 2.006292185433948827 ) ) ;
#204851 = CARTESIAN_POINT ( 'NONE',  ( 8.107412671292047790, 8.560995659369956101, 0.7216878364870458196 ) ) ;
#204852 = CARTESIAN_POINT ( 'NONE',  ( -3.066115294984855133, 6.728884944124295053, 0.7998128361456341429 ) ) ;
#204853 = CARTESIAN_POINT ( 'NONE',  ( 6.661184041420940005, -7.246166700180828535, -6.773376349083132908 ) ) ;
#204854 = CARTESIAN_POINT ( 'NONE',  ( 0.9727375897880451427, -0.05299885879509737968, -2.090136731789421276 ) ) ;
#204855 = CARTESIAN_POINT ( 'NONE',  ( 0.1647065507319189492, -1.628042339203483957, -0.8261295386280396169 ) ) ;
#204856 = CARTESIAN_POINT ( 'NONE',  ( -4.554649539187067830, 7.401175998105142817, 1.199719254218464037 ) ) ;
#204857 = CARTESIAN_POINT ( 'NONE',  ( 2.625780896952558674, -1.049238153381076177, -1.493741879923994542 ) ) ;
#204858 = CARTESIAN_POINT ( 'NONE',  ( 3.633602750639616019, -2.039237483250630589, 0.8441791899983088765 ) ) ;
#204859 = EDGE_CURVE ( 'NONE', #125687, #83422, #168908, .T. ) ;
#204860 = CARTESIAN_POINT ( 'NONE',  ( 1.500000000000001332, 9.906250000682799595, 0.000000000000000000 ) ) ;
#204861 = CARTESIAN_POINT ( 'NONE',  ( 1.318461241437279607, -0.6911404020932455650, -1.783297644634279200 ) ) ;
#204862 = CARTESIAN_POINT ( 'NONE',  ( 1.258185455790395979, -1.969739565659900160, -0.003359478883382254876 ) ) ;
#204863 = CARTESIAN_POINT ( 'NONE',  ( 4.124509801231989847, 0.09871269697571230517, 1.939684287242355420 ) ) ;
#204864 = ORIENTED_EDGE ( 'NONE', *, *, #59542, .T. ) ;
#204865 = DIRECTION ( 'NONE',  ( 0.9999455182791218144, -5.694964898128450927E-17, -0.01043841336116897549 ) ) ;
#204867 = CARTESIAN_POINT ( 'NONE',  ( 6.526204204079649962, 0.9558936715202811518, 1.596491800297286545 ) ) ;
#204866 = CARTESIAN_POINT ( 'NONE',  ( -3.481411583659053566, 7.283673624236017830, 0.000000000000000000 ) ) ;
#204868 = CARTESIAN_POINT ( 'NONE',  ( 3.711900195091365262, 7.552577004240394132, -0.7998128361456362523 ) ) ;
#204869 = CARTESIAN_POINT ( 'NONE',  ( -3.147653791585729444, 8.920000000000001705, 2.419999999999999485 ) ) ;
#204870 = CARTESIAN_POINT ( 'NONE',  ( 10.23370702021670020, 10.83374636654133383, 0.7998128361456462443 ) ) ;
#204871 = CARTESIAN_POINT ( 'NONE',  ( -7.273023059088104425, 7.449891421883056530, 0.000000000000000000 ) ) ;
#204872 = CARTESIAN_POINT ( 'NONE',  ( 2.753686713869853531, 2.180749500395392282, -0.2175628297749406803 ) ) ;
#204873 = ORIENTED_EDGE ( 'NONE', *, *, #68379, .F. ) ;
#204874 = CARTESIAN_POINT ( 'NONE',  ( 7.537407054554579489, 7.758339416593960536, 0.000000000000000000 ) ) ;
#204875 = FACE_OUTER_BOUND ( 'NONE', #210976, .T. ) ;
#204878 = EDGE_CURVE ( 'NONE', #34907, #156, #110243, .T. ) ;
#204877 = CARTESIAN_POINT ( 'NONE',  ( 5.841029835422532734, -1.731992920607817288, -1.032484497598872064 ) ) ;
#204876 = CARTESIAN_POINT ( 'NONE',  ( 3.457459740917231628, 0.4424662778084071935, -1.771134634090239190 ) ) ;
#204879 = DIRECTION ( 'NONE',  ( -0.9512177852344306794, 0.3085202182251672864, 0.000000000000000000 ) ) ;
#204880 = CARTESIAN_POINT ( 'NONE',  ( -3.735435015764967837, 4.316761258935923884, -1.199719254218452047 ) ) ;
#204881 = AXIS2_PLACEMENT_3D ( 'NONE', #136779, #117381, #86951 ) ;
#204882 = CARTESIAN_POINT ( 'NONE',  ( -4.607972389651186162, 8.469779238289159906, 0.3137405545926199579 ) ) ;
#204883 = DIRECTION ( 'NONE',  ( 0.000000000000000000, -1.000000000000000000, 0.000000000000000000 ) ) ;
#204884 = CARTESIAN_POINT ( 'NONE',  ( 4.065207594588423845, 0.2294239933214488880, -1.856472568989680161 ) ) ;
#204885 = CARTESIAN_POINT ( 'NONE',  ( 7.889955328148847258, 11.29236608522730911, -1.199719254218446718 ) ) ;
#204886 = CIRCLE ( 'NONE', #111598, 0.07999999999999993228 ) ;
#204887 = CARTESIAN_POINT ( 'NONE',  ( 1.928227594698066039, 1.109388971949121228, -1.574834034052971399 ) ) ;
#204888 = CARTESIAN_POINT ( 'NONE',  ( 6.754749089495472703, -0.5201146403621333958, -1.891512521893109700 ) ) ;
#204889 = CARTESIAN_POINT ( 'NONE',  ( -1.364683531250000748, 8.421875000341403350, 0.000000000000000000 ) ) ;
#204890 = CARTESIAN_POINT ( 'NONE',  ( -4.903245109636583443, 8.872203061218007392, -0.7998128361456281477 ) ) ;
#204891 = CARTESIAN_POINT ( 'NONE',  ( 5.359550796103802028, 5.147230771742885125, -0.7998128361456231517 ) ) ;
#204892 = CARTESIAN_POINT ( 'NONE',  ( -4.462041952228954500, 6.299077925724123617, -1.443375672974066548 ) ) ;
#204893 = CARTESIAN_POINT ( 'NONE',  ( 0.5095558700928676243, -2.008984845895735116, 0.6684745883070477568 ) ) ;
#204894 = CARTESIAN_POINT ( 'NONE',  ( 4.996790860652426159E-15, 0.6250000006827882704, 1.224999999999976330 ) ) ;
#204895 = CARTESIAN_POINT ( 'NONE',  ( -2.168941388506379742, 5.474256019991960542, -0.7216878364870267237 ) ) ;
#204896 = CARTESIAN_POINT ( 'NONE',  ( 4.645415698524104187, 1.851598927129451955, -0.9261206523473937136 ) ) ;
#204898 = CARTESIAN_POINT ( 'NONE',  ( 1.364683531249990311, 3.196875000341416140, 1.214306433183764966E-14 ) ) ;
#204897 = CARTESIAN_POINT ( 'NONE',  ( 0.01093749962182561514, -1.805946196879631094, 0.3578947576599255664 ) ) ;
#204899 = EDGE_LOOP ( 'NONE', ( #193159, #45573 ) ) ;
#204900 = CARTESIAN_POINT ( 'NONE',  ( 5.203857780826313117, 2.123009612837105209, 0.8817886472500915396 ) ) ;
#204901 = CARTESIAN_POINT ( 'NONE',  ( 7.483737605063422116, 7.833374748769873719, -0.7216878364870257245 ) ) ;
#204903 = CARTESIAN_POINT ( 'NONE',  ( 0.6124999999999914957, 1.416666666666690944, -1.060881119635986414 ) ) ;
#204902 = CARTESIAN_POINT ( 'NONE',  ( 5.261973015879598314, 5.311592404713873172, -0.7216878364870458196 ) ) ;
#204904 = CARTESIAN_POINT ( 'NONE',  ( 0.4633194693007875453, 0.2188196410306940398, -2.281803551658576179 ) ) ;
#204906 = EDGE_CURVE ( 'NONE', #34978, #106531, #2848, .T. ) ;
#204905 = CARTESIAN_POINT ( 'NONE',  ( 1.579999999999985860, -1.099999999999982991, 2.499999999999998668 ) ) ;
#204907 = CARTESIAN_POINT ( 'NONE',  ( -6.749980374757255319, 8.968339418673846097, 1.599625672291269396 ) ) ;
#204908 = CARTESIAN_POINT ( 'NONE',  ( 4.962805208576138938, 0.1888075513713943498, -1.932747541012701964 ) ) ;
#204909 = ORIENTED_EDGE ( 'NONE', *, *, #50401, .F. ) ;
#204910 = CARTESIAN_POINT ( 'NONE',  ( 8.798878505144646311, 11.28844422746735532, -1.443375672974052559 ) ) ;
#204911 = EDGE_CURVE ( 'NONE', #142172, #144460, #53769, .T. ) ;
#204912 = ORIENTED_EDGE ( 'NONE', *, *, #156299, .T. ) ;
#204913 = CARTESIAN_POINT ( 'NONE',  ( 6.099862406061942188, 1.323743610676546334, 1.380425988546908567 ) ) ;
#204914 = CARTESIAN_POINT ( 'NONE',  ( 5.682827415814322158, 1.645762192317705486, -1.164983060713747909 ) ) ;
#204916 = PRESENTATION_STYLE_ASSIGNMENT (( #40327 ) ) ;
#204915 = CARTESIAN_POINT ( 'NONE',  ( -7.492852449846775897, 11.89341162479659531, 0.000000000000000000 ) ) ;
#204917 = CARTESIAN_POINT ( 'NONE',  ( 3.285556943750000514, -1.101041666188710355, 1.896917185911906500 ) ) ;
#204919 = CARTESIAN_POINT ( 'NONE',  ( 0.7601953647339227960, -1.285989511019115517, 1.216233164963770763 ) ) ;
#204918 = CARTESIAN_POINT ( 'NONE',  ( 2.396528757545500099, 1.678484640409601436, -1.246154833996036437 ) ) ;
#204920 = CARTESIAN_POINT ( 'NONE',  ( 0.000000000000000000, 2.000000000000001776, 0.000000000000000000 ) ) ;
#204922 = CARTESIAN_POINT ( 'NONE',  ( 4.101757505036166762, -2.286240945789700607, 0.1669829803510776423 ) ) ;
#204921 = SURFACE_SIDE_STYLE ('',( #41408 ) ) ;
#204923 = CARTESIAN_POINT ( 'NONE',  ( 2.765247366594007605, 0.9310170973755277357, 1.470147560556547273 ) ) ;
#204924 = CARTESIAN_POINT ( 'NONE',  ( 4.029797971759831121, 5.724516938518342535, -1.599625672291255185 ) ) ;
#204925 = AXIS2_PLACEMENT_3D ( 'NONE', #100721, #97555, #2121 ) ;
#204926 = CARTESIAN_POINT ( 'NONE',  ( 2.707414796094851361, 1.816601298730673220, -1.093838055662835096 ) ) ;
#204927 = CARTESIAN_POINT ( 'NONE',  ( 6.547661840756935803, 6.603636667163397256, 0.7998128361456350310 ) ) ;
#204928 = CARTESIAN_POINT ( 'NONE',  ( 1.774300323613137165, -1.721452415463576635, 0.2060816229845687519 ) ) ;
#204929 = CARTESIAN_POINT ( 'NONE',  ( 0.6801582343749952297, 2.088541667008066316, -1.178068619123855409 ) ) ;
#204930 = CARTESIAN_POINT ( 'NONE',  ( 1.961162895873772127, 1.544969826164013238, 1.037258533166736996 ) ) ;
#204931 = CARTESIAN_POINT ( 'NONE',  ( 2.594372030776093574, 1.025359171358769306, -1.913825152921688311 ) ) ;
#204932 = CARTESIAN_POINT ( 'NONE',  ( 4.527533231959700366, 7.369540306339926516, 1.199719254218462483 ) ) ;
#204933 = CARTESIAN_POINT ( 'NONE',  ( 3.872279980006509970, -1.995268062538615883, -0.2910826752766728642 ) ) ;
#204934 = CARTESIAN_POINT ( 'NONE',  ( 2.187500000000001332, -1.451031289061030849, 1.451031289061208041 ) ) ;
#204935 = CARTESIAN_POINT ( 'NONE',  ( 1.499999999999987121, 2.577083334016147198, -0.8660254037844262731 ) ) ;
#204936 = CARTESIAN_POINT ( 'NONE',  ( 0.5164664324388609229, 1.330803901959699997, -1.393038531337851493 ) ) ;
#204937 = CARTESIAN_POINT ( 'NONE',  ( -0.6823417656250003738, 14.15104166700806232, 1.181850606188754593 ) ) ;
#204938 = CARTESIAN_POINT ( 'NONE',  ( 4.834350099735578610, -1.189287197132185669, -1.876079791293260079 ) ) ;
#204939 = ORIENTED_EDGE ( 'NONE', *, *, #202630, .T. ) ;
#204940 = CARTESIAN_POINT ( 'NONE',  ( -1.500000000000013101, 0.9208333333333594828, 0.8660254037844403729 ) ) ;
#204941 = CARTESIAN_POINT ( 'NONE',  ( 8.111855979677986994, 8.358253485912799263, 1.040834085586084257E-14 ) ) ;
#204942 = CARTESIAN_POINT ( 'NONE',  ( -1.364683531250000748, 0.2593750003414205252, 0.000000000000000000 ) ) ;
#204943 = CARTESIAN_POINT ( 'NONE',  ( 0.7509959265504009274, 2.189410886431830239, 0.3742058002541984729 ) ) ;
#204944 = CARTESIAN_POINT ( 'NONE',  ( 5.934033239752054989, 1.167398200610193282, 1.576599764842034457 ) ) ;
#204945 = CARTESIAN_POINT ( 'NONE',  ( 7.944714827928033962, 12.21265836598400689, 0.7216878364870438212 ) ) ;
#204946 = CARTESIAN_POINT ( 'NONE',  ( -1.423138914311270709, 3.789383647063556904, -0.4995195405159393309 ) ) ;
#204947 = CARTESIAN_POINT ( 'NONE',  ( 5.448581927027607463, 0.6492139302081233465, 2.167288725150788409 ) ) ;
#204948 = AXIS2_PLACEMENT_3D ( 'NONE', #945, #36664, #102751 ) ;
#204949 = B_SPLINE_CURVE_WITH_KNOTS ( 'NONE', 3,
 ( #131173, #81293, #176664, #197163, #147370, #213396 ),
 .UNSPECIFIED., .F., .F.,
 ( 4, 2, 4 ),
 ( 0.0004044236633722958431, 0.0006920484658239115742, 0.0009796732682755271426 ),
 .UNSPECIFIED. ) ;
#204951 = AXIS2_PLACEMENT_3D ( 'NONE', #182654, #195730, #149095 ) ;
#204950 = CARTESIAN_POINT ( 'NONE',  ( -5.153507786970276783, 6.145418851954329575, -1.082531754730549967 ) ) ;
#204952 = CARTESIAN_POINT ( 'NONE',  ( 3.402832357982612077, 0.4983898525147857361, 2.001458950477213339 ) ) ;
#204953 = CARTESIAN_POINT ( 'NONE',  ( -4.394814349124112951, 8.279033840620114049, -0.7998128361456281477 ) ) ;
#204954 = CARTESIAN_POINT ( 'NONE',  ( 1.499999999999989120, 2.285416667349482012, 0.8660254037844524744 ) ) ;
#204955 = CARTESIAN_POINT ( 'NONE',  ( 1.364683531249990311, 5.676041667008088432, 0.7879004041258500513 ) ) ;
#204956 = CARTESIAN_POINT ( 'NONE',  ( 4.305816765424046011, -1.865681898550693107, 0.1353468896250972775 ) ) ;
#204957 = CARTESIAN_POINT ( 'NONE',  ( 3.639074924717408788, 0.6284830325712500443, 1.616442243290783232 ) ) ;
#204958 = CARTESIAN_POINT ( 'NONE',  ( 3.491524089112467699, -1.738650433694358233, -0.08144215361822156052 ) ) ;
#204959 = CARTESIAN_POINT ( 'NONE',  ( 0.5742758271649881507, -1.267216683205124150, 1.910101658145799020 ) ) ;
#204960 = CARTESIAN_POINT ( 'NONE',  ( -0.6823417656250212460, 3.863541667008085767, 1.181850606188767472 ) ) ;
#204961 = CARTESIAN_POINT ( 'NONE',  ( 4.774988821994140764, 1.950233014344885385, -0.7539837885136254636 ) ) ;
#204962 = CARTESIAN_POINT ( 'NONE',  ( 8.235688245297327015, 11.69572115523387268, -1.199719254218446718 ) ) ;
#204963 = CARTESIAN_POINT ( 'NONE',  ( 5.560475942038150876, -1.756435177671934911, -0.8285927890409640062 ) ) ;
#204964 = CARTESIAN_POINT ( 'NONE',  ( 9.397486876216094132, 13.53113053364065443, 7.462549781540788629 ) ) ;
#204965 = CARTESIAN_POINT ( 'NONE',  ( 2.468750000000001776, 0.7852924748298570901, -1.895863743164139859 ) ) ;
#204966 = CARTESIAN_POINT ( 'NONE',  ( 0.5455463417442986129, -1.458554840210561476, 1.392547631435703037 ) ) ;
#204967 = CARTESIAN_POINT ( 'NONE',  ( 0.8090202166558431163, -0.5209130535433897924, -2.055487714681260236 ) ) ;
#204968 = SURFACE_STYLE_FILL_AREA ( #105386 ) ;
#204969 = CARTESIAN_POINT ( 'NONE',  ( -11.86687934130374167, 12.49048050383441577, -1.056332641424308827 ) ) ;
#204970 = CARTESIAN_POINT ( 'NONE',  ( -7.818248136574758256, 12.27303992597924420, 0.000000000000000000 ) ) ;
#204971 = CARTESIAN_POINT ( 'NONE',  ( 7.955937213120826357, 8.176348258262782664, 0.7998128361456481317 ) ) ;
#204972 = DIRECTION ( 'NONE',  ( 0.000000000000000000, 0.000000000000000000, 1.000000000000000000 ) ) ;
#204973 = CARTESIAN_POINT ( 'NONE',  ( 4.688025921862073453, -0.8580590012943272171, 1.611482198803436905 ) ) ;
#204974 = ORIENTED_EDGE ( 'NONE', *, *, #65647, .T. ) ;
#204975 = CARTESIAN_POINT ( 'NONE',  ( -6.851666526859749418, 9.086973262793417661, -1.599625672291271394 ) ) ;
#204976 = UNCERTAINTY_MEASURE_WITH_UNIT (LENGTH_MEASURE( 1.000000000000000082E-05 ), #111538, 'distance_accuracy_value', 'NONE');
#204977 = FACE_OUTER_BOUND ( 'NONE', #107943, .T. ) ;
#204978 = CARTESIAN_POINT ( 'NONE',  ( 1.001543065824772753E-15, -2.909374999522043925, 3.793834371823811669 ) ) ;
#204979 = CARTESIAN_POINT ( 'NONE',  ( -6.073162743917628781, 9.172774736957510555, -1.199719254218440723 ) ) ;
#204980 = CARTESIAN_POINT ( 'NONE',  ( 2.549087187268097576, 0.2513027392179004171, 2.004046050866041817 ) ) ;
#204981 = CARTESIAN_POINT ( 'NONE',  ( 5.579209114504255496, -0.04897750150410771358, -2.206396493298476980 ) ) ;
#204982 = AXIS2_PLACEMENT_3D ( 'NONE', #164935, #52254, #67400 ) ;
#204983 = CARTESIAN_POINT ( 'NONE',  ( -4.634908411025374875, 6.500755460986618495, 1.599625672291263179 ) ) ;
#204984 = CARTESIAN_POINT ( 'NONE',  ( 3.326847623520872155, -1.717698991579403422, -0.7164791247627964044 ) ) ;
#204985 = CARTESIAN_POINT ( 'NONE',  ( 9.999301985278609806, 11.62460605670194447, 1.199719254218452047 ) ) ;
#204986 = CARTESIAN_POINT ( 'NONE',  ( -0.3000000000000103140, 0.6284510210557009424, -1.086836331270430334 ) ) ;
#204987 = EDGE_LOOP ( 'NONE', ( #46819, #197812, #70076, #129140 ) ) ;
#204988 = VERTEX_POINT ( 'NONE', #119902 ) ;
#204989 = CARTESIAN_POINT ( 'NONE',  ( -5.928993247877788697, 5.811580298812519807, 0.7998128361456341429 ) ) ;
#204990 = CARTESIAN_POINT ( 'NONE',  ( -9.820183334999905256, 10.35130206712171130, 1.040834085586084257E-14 ) ) ;
#204992 = ADVANCED_FACE ( 'NONE', ( #167516, #185876 ), #19113, .F. ) ;
#204991 = CARTESIAN_POINT ( 'NONE',  ( 4.898959864523320107, 1.516061528642864253, -1.016892643307308441 ) ) ;
#204994 = CARTESIAN_POINT ( 'NONE',  ( -3.999491622362644883, 7.816382810427971783, -0.3443157113667428271 ) ) ;
#204993 = CARTESIAN_POINT ( 'NONE',  ( -5.517242166118370150, 5.401480380085008193, 0.7998128361456281477 ) ) ;
#204995 = CARTESIAN_POINT ( 'NONE',  ( 6.246047416222394233, 7.008439898793222156, -0.9866338212708870570 ) ) ;
#204996 = CARTESIAN_POINT ( 'NONE',  ( 0.2976278659034147789, -1.588993460933589841, 0.6942472086189295233 ) ) ;
#204997 = CARTESIAN_POINT ( 'NONE',  ( 0.1634481287224815171, -1.141006008805772298, 1.314205411033820381 ) ) ;
#204998 = CARTESIAN_POINT ( 'NONE',  ( 5.373738807407080209, 2.225351779437909183, -0.6107155785605354881 ) ) ;
#204999 = CARTESIAN_POINT ( 'NONE',  ( 3.854260808034858155, 7.718664386007802136, -0.7998128361456362523 ) ) ;
#205000 = CARTESIAN_POINT ( 'NONE',  ( 0.2454759580562664856, -1.591291808662575580, -1.309149871672641297 ) ) ;
#205001 = CARTESIAN_POINT ( 'NONE',  ( 5.494078562035752178, 7.432844293840273231, -1.599625672291262513 ) ) ;
#205002 = CARTESIAN_POINT ( 'NONE',  ( 5.765083458594993715, -2.298542321979883507, -0.008455817729055568541 ) ) ;
#205003 = CARTESIAN_POINT ( 'NONE',  ( 5.378281411895265762, 4.339595938922572671, 2.499999999999998668 ) ) ;
#205004 = CARTESIAN_POINT ( 'NONE',  ( -6.961185525973791144, 7.086080966583015339, 0.7998128361456341429 ) ) ;
#205005 = CARTESIAN_POINT ( 'NONE',  ( 5.735183426005796115, -1.690533149647139410, 0.8011652756413772947 ) ) ;
#205007 = CARTESIAN_POINT ( 'NONE',  ( -3.149236820124241110, 6.896136400112061970, -0.7998128361456481317 ) ) ;
#205006 = CARTESIAN_POINT ( 'NONE',  ( 3.920094060441734030, -1.906919942518231936, 0.1457910263855527466 ) ) ;
#205008 = CARTESIAN_POINT ( 'NONE',  ( 5.619807753665406302, -2.153844256707802440, 0.4802137346974973409 ) ) ;
#205009 = CARTESIAN_POINT ( 'NONE',  ( 4.716069161646245789, 1.085680477651463915, -1.817652797078447735 ) ) ;
#205010 = CARTESIAN_POINT ( 'NONE',  ( 1.224999999999965006, 0.4166666673494939799, 0.7072540797572456350 ) ) ;
#205011 = CARTESIAN_POINT ( 'NONE',  ( -10.56199358538776778, 4.161122272433269487, 5.602120407118017731 ) ) ;
#205012 = CARTESIAN_POINT ( 'NONE',  ( -0.2108831679770960255, 0.2438762813419328990, -1.931650693707862132 ) ) ;
#205013 = CARTESIAN_POINT ( 'NONE',  ( 4.678972410047582464, 8.472901888448573615, -0.7216878364870357165 ) ) ;
#205014 = CARTESIAN_POINT ( 'NONE',  ( -3.960390268523300339, 7.634556056670224855, 1.214306433183764966E-14 ) ) ;
#205015 = CARTESIAN_POINT ( 'NONE',  ( 5.408877457991549953, -0.5154355754800542533, -2.056752310636373426 ) ) ;
#205016 = CARTESIAN_POINT ( 'NONE',  ( 2.134188411380482098, -1.507708438093162018, -1.747028958505469909 ) ) ;
#205017 = CARTESIAN_POINT ( 'NONE',  ( 3.420314466093795414, 0.8798059112791326575, 1.753580237611163994 ) ) ;
#205018 =( NAMED_UNIT ( * ) PLANE_ANGLE_UNIT ( ) SI_UNIT ( $, .RADIAN. ) );
#205019 = CARTESIAN_POINT ( 'NONE',  ( 5.875849835592577897, -2.013560656311346619, 0.4463529024570592751 ) ) ;
#205020 = CARTESIAN_POINT ( 'NONE',  ( 4.365362273920252889, 4.195270195769483124, 0.7216878364870317197 ) ) ;
#205021 = CARTESIAN_POINT ( 'NONE',  ( 5.564695703766185275, 5.456842840674144490, 0.000000000000000000 ) ) ;
#205022 = ORIENTED_EDGE ( 'NONE', *, *, #20455, .T. ) ;
#205023 = CARTESIAN_POINT ( 'NONE',  ( 5.559779856078610472, 1.205038519190555268, 1.616695979245158066 ) ) ;
#205024 =( BOUNDED_SURFACE ( )  B_SPLINE_SURFACE ( 3, 3, ( 
 ( #68318, #127312, #198323, #116081, #48907, #19583, #210595, #98720, #18514, #150680, #182072, #99781, #177042, #82448, #35834, #165846 ),
 ( #134449, #3312, #164779, #200452, #193282, #83515, #101912, #85655, #44927, #151742, #111035, #94744, #120370, #91014, #201512, #71517 ),
 ( #189552, #36898, #72593, #154932, #4373, #102980, #157076, #137629, #88879, #5438, #187416, #41199, #169038, #40117, #20635, #107306 ),
 ( #86724, #186345, #185275, #152793, #188487, #39047, #105132, #22762, #6517, #70443, #24908, #89949, #37980, #56361, #119289, #23841 ),
 ( #171172, #136559, #121447, #69382, #173330, #57426, #203646, #138694, #204711, #104053, #139770, #170099, #21685, #122524, #135490, #202580 ),
 ( #106228, #172254, #87795, #123588, #155999, #205796, #53160, #7586, #54232, #153869, #55297, #73671, #78999, #108377, #28124, #12919 ),
 ( #44391, #144058, #46523, #60618, #158141, #95287, #206861, #125708, #11859, #9732, #145115, #75807, #94218, #211121, #178654, #176512 ) ),
 .UNSPECIFIED., .T., .F., .T. ) 
 B_SPLINE_SURFACE_WITH_KNOTS ( ( 4, 3, 4 ),
 ( 4, 2, 2, 2, 2, 2, 2, 4 ),
 ( 0.000000000000000000, 0.5000000000000000000, 1.000000000000000000 ),
 ( 0.3501333200791456046, 0.3551713324458994903, 0.3602093448126533759, 0.3702853695461611472, 0.3803518226137216351, 0.3853850491475018791, 0.3879016624143920011, 0.3904182756812821231 ),
 .UNSPECIFIED. ) 
 GEOMETRIC_REPRESENTATION_ITEM ( )  RATIONAL_B_SPLINE_SURFACE ( (
 ( 1.000000000000000000, 1.000000000000000000, 1.000000000000000000, 1.000000000000000000, 1.000000000000000000, 1.000000000000000000, 1.000000000000000000, 1.000000000000000000, 1.000000000000000000, 1.000000000000000000, 1.000000000000000000, 1.000000000000000000, 1.000000000000000000, 1.000000000000000000, 1.000000000000000000, 1.000000000000000000),
 ( 0.3333333333333333703, 0.3333333333333333703, 0.3333333333333333703, 0.3333333333333333703, 0.3333333333333333703, 0.3333333333333333703, 0.3333333333333333703, 0.3333333333333333703, 0.3333333333333333703, 0.3333333333333333703, 0.3333333333333333703, 0.3333333333333333703, 0.3333333333333333703, 0.3333333333333333703, 0.3333333333333333703, 0.3333333333333333703),
 ( 0.3333333333333333703, 0.3333333333333333703, 0.3333333333333333703, 0.3333333333333333703, 0.3333333333333333703, 0.3333333333333333703, 0.3333333333333333703, 0.3333333333333333703, 0.3333333333333333703, 0.3333333333333333703, 0.3333333333333333703, 0.3333333333333333703, 0.3333333333333333703, 0.3333333333333333703, 0.3333333333333333703, 0.3333333333333333703),
 ( 1.000000000000000000, 1.000000000000000000, 1.000000000000000000, 1.000000000000000000, 1.000000000000000000, 1.000000000000000000, 1.000000000000000000, 1.000000000000000000, 1.000000000000000000, 1.000000000000000000, 1.000000000000000000, 1.000000000000000000, 1.000000000000000000, 1.000000000000000000, 1.000000000000000000, 1.000000000000000000),
 ( 0.3333333333333333703, 0.3333333333333333703, 0.3333333333333333703, 0.3333333333333333703, 0.3333333333333333703, 0.3333333333333333703, 0.3333333333333333703, 0.3333333333333333703, 0.3333333333333333703, 0.3333333333333333703, 0.3333333333333333703, 0.3333333333333333703, 0.3333333333333333703, 0.3333333333333333703, 0.3333333333333333703, 0.3333333333333333703),
 ( 0.3333333333333333703, 0.3333333333333333703, 0.3333333333333333703, 0.3333333333333333703, 0.3333333333333333703, 0.3333333333333333703, 0.3333333333333333703, 0.3333333333333333703, 0.3333333333333333703, 0.3333333333333333703, 0.3333333333333333703, 0.3333333333333333703, 0.3333333333333333703, 0.3333333333333333703, 0.3333333333333333703, 0.3333333333333333703),
 ( 1.000000000000000000, 1.000000000000000000, 1.000000000000000000, 1.000000000000000000, 1.000000000000000000, 1.000000000000000000, 1.000000000000000000, 1.000000000000000000, 1.000000000000000000, 1.000000000000000000, 1.000000000000000000, 1.000000000000000000, 1.000000000000000000, 1.000000000000000000, 1.000000000000000000, 1.000000000000000000) ) ) 
 REPRESENTATION_ITEM ( '' )  SURFACE ( )  );
#205025 = CARTESIAN_POINT ( 'NONE',  ( 1.499999999999997113, 4.254166666666687746, 0.8660254037844477004 ) ) ;
#205026 = CARTESIAN_POINT ( 'NONE',  ( -10.57232898948313604, 5.599354254162436817, 4.968808419985093039 ) ) ;
#205027 = CARTESIAN_POINT ( 'NONE',  ( 3.467796559821629820, -0.4283512159202977343, 2.128237193570106101 ) ) ;
#205028 = CARTESIAN_POINT ( 'NONE',  ( 4.044074958626150185, 7.940114228364351767, 0.7998128361456271485 ) ) ;
#205029 = CARTESIAN_POINT ( 'NONE',  ( 1.213308285724056690, 1.730450836393576886, -1.225479750871574458 ) ) ;
#205030 = CARTESIAN_POINT ( 'NONE',  ( 1.499999999999989120, 1.056250000682816603, 0.000000000000000000 ) ) ;
#205031 = CARTESIAN_POINT ( 'NONE',  ( -5.580962959613590790, 14.55306900392666947, -10.58267955529689175 ) ) ;
#205032 = CARTESIAN_POINT ( 'NONE',  ( 5.695510712908186335, 6.192163513152999066, 0.9270467717220601811 ) ) ;
#205033 = CARTESIAN_POINT ( 'NONE',  ( 4.873468316212648865, 8.167532512703042258, 0.9812947938723035612 ) ) ;
#205034 = CARTESIAN_POINT ( 'NONE',  ( 1.141951006405941715, 0.8376953415718463303, -1.883039458060199900 ) ) ;
#205036 = CARTESIAN_POINT ( 'NONE',  ( -9.305047017617296135, 14.48154074412967596, 7.449999999995404742 ) ) ;
#205035 = DIRECTION ( 'NONE',  ( 3.330669073875478989E-16, -3.540251991789410786E-16, -1.000000000000000000 ) ) ;
#205037 = CARTESIAN_POINT ( 'NONE',  ( 1.364683531249986537, 1.155208333674754728, -0.7879004041258239610 ) ) ;
#205038 = FACE_OUTER_BOUND ( 'NONE', #207240, .T. ) ;
#205039 = EDGE_LOOP ( 'NONE', ( #142883, #199857, #96714, #177995 ) ) ;
#205040 = CARTESIAN_POINT ( 'NONE',  ( 3.844317892072905973, 1.020479721125296280, -1.617037373464407457 ) ) ;
#205041 = COLOUR_RGB ( '', 0.66274510, 0.83137255, 0.94901961) ;
#205042 = CARTESIAN_POINT ( 'NONE',  ( 5.102326758870145973, -0.5985492928855026262, -1.665706573615277852 ) ) ;
#205043 = CARTESIAN_POINT ( 'NONE',  ( 4.552505719138623341, 8.533283448962240669, 0.7998128361456341429 ) ) ;
#205044 = TOROIDAL_SURFACE ( 'NONE', #111752, 1.811274280335456677, 0.2000000000000000111 ) ;
#205045 = CARTESIAN_POINT ( 'NONE',  ( -3.578462479003122976, 6.262291094557191684, 1.199719254218464037 ) ) ;
#205046 = CARTESIAN_POINT ( 'NONE',  ( -0.01774202353897573470, -1.183624524064251116, 1.371566177806067932 ) ) ;
#205048 = CARTESIAN_POINT ( 'NONE',  ( 6.204688727450275110, 1.789332568231709608, 0.6845011832880606439 ) ) ;
#205047 = CARTESIAN_POINT ( 'NONE',  ( -6.719405205104948209, -7.217450603038109591, 6.716119544743302860 ) ) ;
#205049 = CARTESIAN_POINT ( 'NONE',  ( 0.8540665308606997241, -0.7467690478978536994, 1.931163149162813619 ) ) ;
#205050 = CARTESIAN_POINT ( 'NONE',  ( 0.6823417656249882723, -0.09479166632524876901, 1.181850606188755259 ) ) ;
#205051 = EDGE_CURVE ( 'NONE', #80820, #39859, #6054, .T. ) ;
#205052 = CARTESIAN_POINT ( 'NONE',  ( 6.051601594667258333, 0.5412791183288803154, -1.790613848972313571 ) ) ;
#205053 = CARTESIAN_POINT ( 'NONE',  ( 2.824607995650964209, 1.719152210223941823, 0.6149139946348627372 ) ) ;
#205055 = CARTESIAN_POINT ( 'NONE',  ( 5.309622429108474151, 7.625948988765205883, 1.230663689527239812 ) ) ;
#205054 = CARTESIAN_POINT ( 'NONE',  ( 5.285833163787800437, 1.479997892162682849, 1.637210856327932618 ) ) ;
#205056 = CARTESIAN_POINT ( 'NONE',  ( -1.364683531250000748, 0.009375000341420303140, 0.000000000000000000 ) ) ;
#205057 = CARTESIAN_POINT ( 'NONE',  ( 4.035635273026453085, 1.943268055400270811, -0.6920256600186375229 ) ) ;
#205058 = CARTESIAN_POINT ( 'NONE',  ( -7.446452682403657874, 9.710614100936176385, -1.599625672291263179 ) ) ;
#205059 = CARTESIAN_POINT ( 'NONE',  ( 8.860417081730671995, 10.29590700256267155, 1.199719254218453823 ) ) ;
#205060 = CARTESIAN_POINT ( 'NONE',  ( 1.286813488861813459, 4.047007041464545374, -0.4595522011843575783 ) ) ;
#205061 = CARTESIAN_POINT ( 'NONE',  ( -0.04699017840227408260, -9.984793624843945281, -10.91963405940077791 ) ) ;
#205062 = CARTESIAN_POINT ( 'NONE',  ( 6.478973898625433492, 1.930320082341809629, 0.7489585856828018251 ) ) ;
#205063 = CARTESIAN_POINT ( 'NONE',  ( -0.6823417656250003738, 1.280208333674752508, -1.181850606188749264 ) ) ;
#205064 = CARTESIAN_POINT ( 'NONE',  ( 3.884175197147401892, -1.069116497136082700, 1.878640351225938421 ) ) ;
#205066 = CARTESIAN_POINT ( 'NONE',  ( 1.592165322863370980, 0.9698756732311950568, -1.705302290208744687 ) ) ;
#205065 = CARTESIAN_POINT ( 'NONE',  ( 4.354169037430507316, 0.8614980693376246279, -1.826848373156648497 ) ) ;
#205067 = CARTESIAN_POINT ( 'NONE',  ( 6.620655732516610215, 1.221631503675042030, 2.386181433960798071 ) ) ;
#205068 = EDGE_CURVE ( 'NONE', #193462, #45616, #161664, .T. ) ;
#205071 = CARTESIAN_POINT ( 'NONE',  ( 6.561783159334121152, 8.678499657355050800, -1.443375672974057666 ) ) ;
#205070 = CARTESIAN_POINT ( 'NONE',  ( 3.475000000000000533, -0.1750000000000015432, 0.000000000000000000 ) ) ;
#205069 = DIRECTION ( 'NONE',  ( 0.000000000000000000, 0.000000000000000000, -1.000000000000000000 ) ) ;
#205072 = CARTESIAN_POINT ( 'NONE',  ( -6.444921918449773024, 8.612437886315108315, 1.599625672291269396 ) ) ;
#205073 = CARTESIAN_POINT ( 'NONE',  ( 2.870327622459168726, -1.987497926849005836, -0.3399570244180456502 ) ) ;
#205075 = CARTESIAN_POINT ( 'NONE',  ( 0.9486429539237137831, 3.163339070649072937, 1.028101543438981080 ) ) ;
#205074 = CARTESIAN_POINT ( 'NONE',  ( -3.418627288940168096, 7.140148937072163804, -0.7998128361456281477 ) ) ;
#205076 = DIRECTION ( 'NONE',  ( 1.000000000000000000, -7.771561172376097755E-16, -4.440892098500627148E-16 ) ) ;
#205077 = CARTESIAN_POINT ( 'NONE',  ( 6.345967646908174054, -1.254484226688237669, -1.443505786478386899 ) ) ;
#205078 = CARTESIAN_POINT ( 'NONE',  ( -11.96209379583854293, 12.27207059405763445, 0.9572398070798600056 ) ) ;
#205079 = CARTESIAN_POINT ( 'NONE',  ( 5.138177029454841893, 7.017625839162543677, 1.443375672974062551 ) ) ;
#205081 = CARTESIAN_POINT ( 'NONE',  ( 4.956657736208940790, -1.899625167328807374, -0.6766988040120130998 ) ) ;
#205080 = CARTESIAN_POINT ( 'NONE',  ( -9.314088342463968218, 9.968783942403868892, 0.7216878364870438212 ) ) ;
#205082 = CARTESIAN_POINT ( 'NONE',  ( 1.499999999999987121, 4.045833333333359150, -0.8660254037844323793 ) ) ;
#205083 = CARTESIAN_POINT ( 'NONE',  ( -1.364683531250000748, 15.17187500034139447, 0.000000000000000000 ) ) ;
#205084 = CARTESIAN_POINT ( 'NONE',  ( 6.000961845343044665, 1.407127125985812466, -0.9971243314716814465 ) ) ;
#205085 = CARTESIAN_POINT ( 'NONE',  ( 5.306037014901791693, 7.283738832175834510, 1.599625672291269396 ) ) ;
#205086 = AXIS2_PLACEMENT_3D ( 'NONE', #197450, #62137, #115211 ) ;
#205087 = CARTESIAN_POINT ( 'NONE',  ( 9.002250809793993724, 11.52571191622492464, -1.443375672974057666 ) ) ;
#205088 = CARTESIAN_POINT ( 'NONE',  ( -6.775479680898469859, -7.217880409000358100, -6.775479680898433443 ) ) ;
#205089 = CARTESIAN_POINT ( 'NONE',  ( 4.569519670753737550, 1.814867081516871261, -0.4525428206468632975 ) ) ;
#205090 = DIRECTION ( 'NONE',  ( -0.1959617823641899015, 0.8823239620903393643, -0.4279058375085054156 ) ) ;
#205091 = CARTESIAN_POINT ( 'NONE',  ( 2.307561340129569150, -1.660171796135110567, -1.236610361758017751 ) ) ;
#205092 = CARTESIAN_POINT ( 'NONE',  ( -7.607533590599451223, 9.008448956188397361, 1.082531754730549078 ) ) ;
#205093 = VERTEX_POINT ( 'NONE', #122055 ) ;
#205094 = CARTESIAN_POINT ( 'NONE',  ( 4.553559489343365740, 6.405848385690952718, -1.599625672291269396 ) ) ;
#205095 = CARTESIAN_POINT ( 'NONE',  ( 0.2457205463545810431, 1.994068899247893434, -0.2986513045247774500 ) ) ;
#205096 = CARTESIAN_POINT ( 'NONE',  ( 0.6327121402699478203, 1.674153623460835627, 0.6926115325788273491 ) ) ;
#205097 = CARTESIAN_POINT ( 'NONE',  ( 5.248414861821569133, 6.256143772614186638, -1.082531754730548412 ) ) ;
#205098 = DIRECTION ( 'NONE',  ( -0.7592566023653005702, -0.6507913734559640506, 0.000000000000000000 ) ) ;
#205099 = CARTESIAN_POINT ( 'NONE',  ( 6.577677080924314801, 10.82570702772039262, 1.040834085586084257E-14 ) ) ;
#205100 = MECHANICAL_DESIGN_GEOMETRIC_PRESENTATION_REPRESENTATION (  '', ( #28720 ), #56393 ) ;
#205102 = CARTESIAN_POINT ( 'NONE',  ( 6.415652790497161639, -1.255571041358375384, -1.446825450776100919 ) ) ;
#205101 = CARTESIAN_POINT ( 'NONE',  ( -6.230135280679522936, 7.227244901336242755, 1.199719254218450271 ) ) ;
#205103 = CIRCLE ( 'NONE', #111816, 0.04999999999999934358 ) ;
#205104 = DIRECTION ( 'NONE',  ( 0.000000000000000000, 0.000000000000000000, -1.000000000000000000 ) ) ;
#205105 = CARTESIAN_POINT ( 'NONE',  ( 1.850000000000000089, 6.384842951632563950E-31, -1.540743955509788682E-30 ) ) ;
#205106 = CARTESIAN_POINT ( 'NONE',  ( 7.785697387528199762E-15, 0.5624999999999894529, 1.224999999999973443 ) ) ;
#205108 = ORIENTED_EDGE ( 'NONE', *, *, #2927, .F. ) ;
#205107 = CARTESIAN_POINT ( 'NONE',  ( 5.029711800989886683, 4.970344644017389513, 1.040834085586084257E-14 ) ) ;
#205109 = CARTESIAN_POINT ( 'NONE',  ( -8.514157279702033065, 9.995900250149611921, -1.082531754730543971 ) ) ;
#205110 = CARTESIAN_POINT ( 'NONE',  ( 3.327187652246216931, 0.05129554954072869377, 2.161254785723889515 ) ) ;
#205111 = CARTESIAN_POINT ( 'NONE',  ( -6.780486220610184134, 9.003929572168926754, -1.443375672974066548 ) ) ;
#205112 = CARTESIAN_POINT ( 'NONE',  ( 6.753369913382843315, 8.011924666102361314, -1.082531754730548412 ) ) ;
#205113 = CARTESIAN_POINT ( 'NONE',  ( 1.318772358905948794, -0.7683209907942339933, -1.976687055281033611 ) ) ;
#205114 = CARTESIAN_POINT ( 'NONE',  ( 6.211906940382025510, -1.811394037990306627, 0.2264786762415857968 ) ) ;
#205115 = EDGE_CURVE ( 'NONE', #19980, #95167, #9818, .T. ) ;
#205116 = CARTESIAN_POINT ( 'NONE',  ( 1.616417101162690440, 1.326873100732330890, -1.458104111731808983 ) ) ;
#205117 = CARTESIAN_POINT ( 'NONE',  ( 3.093911922779784440, 1.216618333484908998, 1.475457842794763996 ) ) ;
#205118 = CARTESIAN_POINT ( 'NONE',  ( -11.44800751629991353, 9.799999999999998934, -3.302956944461114652 ) ) ;
#205119 = CARTESIAN_POINT ( 'NONE',  ( 5.266046268760843141, -1.960244874886694744, 0.1909964021715639393 ) ) ;
#205120 = CARTESIAN_POINT ( 'NONE',  ( 0.3572357504952353158, 1.920940290975415854, -0.2841381762913769427 ) ) ;
#205121 = ORIENTED_EDGE ( 'NONE', *, *, #27140, .F. ) ;
#205122 = CARTESIAN_POINT ( 'NONE',  ( -4.502189528189771472, 7.410248995266807803, -1.199719254218453823 ) ) ;
#205123 = CARTESIAN_POINT ( 'NONE',  ( -6.455090533882193782, 9.584670485287619002, -1.082531754730549967 ) ) ;
#205124 = CARTESIAN_POINT ( 'NONE',  ( 7.160114521348466710, 7.526090827760914870, 0.000000000000000000 ) ) ;
#205126 = VERTEX_POINT ( 'NONE', #150213 ) ;
#205125 = CARTESIAN_POINT ( 'NONE',  ( 5.531871257421491883, -1.864710570029969317, 0.4231498525801706823 ) ) ;
#205127 = AXIS2_PLACEMENT_3D ( 'NONE', #42526, #104306, #136808 ) ;
#205128 = CARTESIAN_POINT ( 'NONE',  ( 0.5521677985501523001, 0.6901698128830742185, -2.096122547012829962 ) ) ;
#205129 = CARTESIAN_POINT ( 'NONE',  ( 7.524604700374169397, -5.166862990899455887, 8.024185963717899384 ) ) ;
#205130 = CARTESIAN_POINT ( 'NONE',  ( 5.971345465650553130, -1.727703365644253086, -1.033000238237492763 ) ) ;
#205131 = CARTESIAN_POINT ( 'NONE',  ( 0.2871295479481039137, 7.105992221059469927, 1.980474574527469667 ) ) ;
#205132 = CARTESIAN_POINT ( 'NONE',  ( 5.507046092540283766, -0.04465857163906890998, 2.016188657829049991 ) ) ;
#205133 = CARTESIAN_POINT ( 'NONE',  ( -0.4500000000000232703, 4.000000000000003553, -0.8627243683430544374 ) ) ;
#205134 = CARTESIAN_POINT ( 'NONE',  ( 1.838419004579601834, -1.109345826794335688, 1.747895861591180156 ) ) ;
#205135 = CARTESIAN_POINT ( 'NONE',  ( -7.223796917982883592, 7.322184580601816428, -0.7998128361456291469 ) ) ;
#205136 = CARTESIAN_POINT ( 'NONE',  ( -4.896236220255085314, 8.042264628280536343, 0.9566786516278618091 ) ) ;
#205137 = CARTESIAN_POINT ( 'NONE',  ( 0.3566080023540801336, 0.8287714912002723811, 1.996717379258300840 ) ) ;
#205138 = CARTESIAN_POINT ( 'NONE',  ( -11.90498647923048914, 8.894293214940326209, 1.536019656081360152 ) ) ;
#205139 = CARTESIAN_POINT ( 'NONE',  ( 4.095971805104285934, 6.832365301713403838, 1.082531754730549078 ) ) ;
#205140 = CARTESIAN_POINT ( 'NONE',  ( 0.2834499523633389750, -6.554910290221304336, 9.477100695693453147 ) ) ;
#205141 = DIRECTION ( 'NONE',  ( 0.000000000000000000, 0.000000000000000000, 1.000000000000000000 ) ) ;
#205142 = CARTESIAN_POINT ( 'NONE',  ( -1.364683531250000748, 12.42187500034139980, 0.000000000000000000 ) ) ;
#205144 = CARTESIAN_POINT ( 'NONE',  ( -5.094831863685302942, 9.165997284266655498, 0.7998128361456291469 ) ) ;
#205143 = CARTESIAN_POINT ( 'NONE',  ( 6.925078400183545035, 3.707308446744279617, 2.270182774727365516 ) ) ;
#205145 = CARTESIAN_POINT ( 'NONE',  ( 4.482897354602959794, -1.733954122632981099, -0.03610910148283198728 ) ) ;
#205146 = CARTESIAN_POINT ( 'NONE',  ( -3.093231602212184850, 6.760520635889515795, -0.7998128361456281477 ) ) ;
#205147 = CARTESIAN_POINT ( 'NONE',  ( 2.184514099445804547, 1.195434181571125132, -1.690031224328606196 ) ) ;
#205148 = CARTESIAN_POINT ( 'NONE',  ( 3.357133807288110727, 0.04956003552011908203, -2.116800119666595315 ) ) ;
#205149 = CARTESIAN_POINT ( 'NONE',  ( 7.344766530301147789, 9.591980256816594164, 1.599625672291281386 ) ) ;
#205150 = CARTESIAN_POINT ( 'NONE',  ( 0.6823417656249917140, 3.592708333674754506, 1.181850606188765695 ) ) ;
#205151 = CARTESIAN_POINT ( 'NONE',  ( 2.096482953606861432, 1.947282536051987201, 0.2939031187191037398 ) ) ;
#205152 = CARTESIAN_POINT ( 'NONE',  ( 6.114015800945279189, 6.016301931502064271, 0.06476946160361742033 ) ) ;
#205153 = CARTESIAN_POINT ( 'NONE',  ( -0.1581436608063293003, -1.178060542814472367, -1.506996232563104776 ) ) ;
#205154 = CARTESIAN_POINT ( 'NONE',  ( 3.715000766203532034, -0.1696613574440029304, 2.286031353463747529 ) ) ;
#205156 = EDGE_CURVE ( 'NONE', #149901, #208182, #171782, .T. ) ;
#205155 = CARTESIAN_POINT ( 'NONE',  ( 1.506192966688112644, -0.6554880476431452774, -1.704135612709246184 ) ) ;
#205157 = CARTESIAN_POINT ( 'NONE',  ( 4.854701522145073334, 7.821512988214679218, -1.199719254218450271 ) ) ;
#205158 = CARTESIAN_POINT ( 'NONE',  ( 5.300874872818821082, 9.128178418356554857, 0.7216878364870438212 ) ) ;
#205159 = CARTESIAN_POINT ( 'NONE',  ( -7.965578943228732278, 9.251929174310385307, -1.199719254218446718 ) ) ;
#205160 = CARTESIAN_POINT ( 'NONE',  ( 3.058842833410029272, 0.4931317667464900634, 1.951740033431844434 ) ) ;
#205161 = CARTESIAN_POINT ( 'NONE',  ( 3.309375504473045293, -1.601080850277468715, -1.133301831143386007 ) ) ;
#205162 = CARTESIAN_POINT ( 'NONE',  ( -8.290974629956718189, 9.631557475493025322, -1.199719254218446718 ) ) ;
#205163 = CARTESIAN_POINT ( 'NONE',  ( -6.901263884555985051, 8.010228272525461435, 1.199719254218450271 ) ) ;
#205165 = EDGE_CURVE ( 'NONE', #117856, #45686, #137166, .T. ) ;
#205164 = CARTESIAN_POINT ( 'NONE',  ( -11.33772463945036968, 12.69999999999999929, -3.680000000000002824 ) ) ;
#205167 = CARTESIAN_POINT ( 'NONE',  ( 4.627684317651063139, -1.090007866362858291, -1.394274008033623113 ) ) ;
#205166 = CARTESIAN_POINT ( 'NONE',  ( 6.158164957586691912, -1.479299979846586455, 1.477571280793017694 ) ) ;
#205168 = CARTESIAN_POINT ( 'NONE',  ( 0.000000000000000000, 3.079999999999999183, 0.000000000000000000 ) ) ;
#205169 = CARTESIAN_POINT ( 'NONE',  ( 0.8147124124333324779, 2.026155960571228043, 0.8354305900151803854 ) ) ;
#205170 = CARTESIAN_POINT ( 'NONE',  ( 5.507646315527288117, -0.7876679103963373230, -1.551952608056671457 ) ) ;
#205171 = CARTESIAN_POINT ( 'NONE',  ( 7.832860060393120882, 10.16142270859057462, 1.599625672291281386 ) ) ;
#205172 = CARTESIAN_POINT ( 'NONE',  ( 2.449293598294706414E-16, 5.499999999999998224, 2.000000000000000000 ) ) ;
#205173 = CARTESIAN_POINT ( 'NONE',  ( 6.258407524398033495, 2.201109419358293628, -0.6625764064998507230 ) ) ;
#205174 = CARTESIAN_POINT ( 'NONE',  ( 3.811250579217332568, 5.539821323877241355, 1.214306433183764966E-14 ) ) ;
#205175 = CARTESIAN_POINT ( 'NONE',  ( 5.589090328658773643, 1.030979737101325400, -1.393799353210682046 ) ) ;
#205176 = CARTESIAN_POINT ( 'NONE',  ( 2.121956728516772639, -2.140194184088719531, 0.5379336890513550795 ) ) ;
#205177 = AXIS2_PLACEMENT_3D ( 'NONE', #142391, #158611, #74158 ) ;
#205178 = CARTESIAN_POINT ( 'NONE',  ( 5.266168369200141086, -2.161202989243858674, 0.2077703183603739345 ) ) ;
#205179 = CARTESIAN_POINT ( 'NONE',  ( -1.115562610750309283E-14, 11.31249999999999822, 1.500000000000001554 ) ) ;
#205180 = CARTESIAN_POINT ( 'NONE',  ( 0.7611333729100393519, -0.05844121263920940695, -2.116714853662078344 ) ) ;
#205181 = CARTESIAN_POINT ( 'NONE',  ( 2.750000000000001332, 1.574424887750340441E-13, 2.052068128417947612 ) ) ;
#205182 = AXIS2_PLACEMENT_3D ( 'NONE', #44489, #174496, #139860 ) ;
#205183 = CARTESIAN_POINT ( 'NONE',  ( 6.827182134110199030, 1.254919323356920025, 2.204230526214937758 ) ) ;
#205184 = CARTESIAN_POINT ( 'NONE',  ( 4.348602224742101008, 0.5129591300635885087, 1.856786894687269207 ) ) ;
#205185 = CARTESIAN_POINT ( 'NONE',  ( 1.647463811467297701, 0.2220449547728920447, 2.210189655316461277 ) ) ;
#205186 = ORIENTED_EDGE ( 'NONE', *, *, #17565, .T. ) ;
#205187 = CARTESIAN_POINT ( 'NONE',  ( -1.201851678989727383E-14, 4.837500000000018119, -1.732050807568863648 ) ) ;
#205188 = CARTESIAN_POINT ( 'NONE',  ( 6.010342169559767633, 5.906487374108181143, -0.7998128361456281477 ) ) ;
#205189 = CARTESIAN_POINT ( 'NONE',  ( 5.147291874682557555, 9.156924287104992288, 0.7998128361456462443 ) ) ;
#205190 = CARTESIAN_POINT ( 'NONE',  ( 3.493049024619375054, -2.141166226970441233, -0.5910787634417090652 ) ) ;
#205191 = CARTESIAN_POINT ( 'NONE',  ( -7.863365906246054138, 11.15738207638699464, -1.082531754730543971 ) ) ;
#205192 = CARTESIAN_POINT ( 'NONE',  ( -1.387778780781445676E-14, -5.907420853759282053, -10.91970695577495398 ) ) ;
#205193 = CARTESIAN_POINT ( 'NONE',  ( 7.185458225562760148, 8.445751353653788485, -1.082531754730543083 ) ) ;
#205194 = CARTESIAN_POINT ( 'NONE',  ( -7.497295758232712437, 11.69066945133944380, -0.7216878364870267237 ) ) ;
#205195 = EDGE_CURVE ( 'NONE', #109538, #12920, #51644, .T. ) ;
#205196 = CARTESIAN_POINT ( 'NONE',  ( 5.397554552016204710, 9.311247720745345902, 0.7216878364870317197 ) ) ;
#205197 = CARTESIAN_POINT ( 'NONE',  ( 1.881482635453747720, -0.5404922439061732309, -1.942541187959702764 ) ) ;
#205199 = CARTESIAN_POINT ( 'NONE',  ( 6.109847269609326226, 0.6021898890512421554, -1.972802226155190297 ) ) ;
#205198 = CARTESIAN_POINT ( 'NONE',  ( 7.239163954692881653, 10.53310948286200599, -1.199719254218441611 ) ) ;
#205200 = CARTESIAN_POINT ( 'NONE',  ( -15.75000000000000000, 11.29999999999998117, 3.199999999999997957 ) ) ;
#205201 = CARTESIAN_POINT ( 'NONE',  ( 6.143253000323500856, 10.18122924377050609, -0.7216878364870458196 ) ) ;
#205202 = CARTESIAN_POINT ( 'NONE',  ( -0.09456490281532430042, -0.7861721075429689565, -1.663503389917226460 ) ) ;
#205203 = FILL_AREA_STYLE_COLOUR ( '', #106205 ) ;
#205204 = CARTESIAN_POINT ( 'NONE',  ( 0.6823417656249899377, 1.842708333674752952, 1.181850606188755259 ) ) ;
#205205 = CARTESIAN_POINT ( 'NONE',  ( 1.282078435845935616, -1.724974465617232999, -0.3947418589646100040 ) ) ;
#205206 = CARTESIAN_POINT ( 'NONE',  ( 0.4928148368598186946, -2.006445878461552645, 0.2004378712678403507 ) ) ;
#205207 = CARTESIAN_POINT ( 'NONE',  ( 6.181193141064822427, 1.207202257718576144, 1.253980304253142997 ) ) ;
#205208 = CARTESIAN_POINT ( 'NONE',  ( 4.159948666787936844, 1.080635193647750292, 2.021704573604603095 ) ) ;
#205209 = CARTESIAN_POINT ( 'NONE',  ( 2.607153984523866264, -1.821078476238715327, 0.2702138248509636242 ) ) ;
#205210 = CARTESIAN_POINT ( 'NONE',  ( 10.08456733046637765, 10.65975006183261087, 0.000000000000000000 ) ) ;
#205211 = CARTESIAN_POINT ( 'NONE',  ( 3.346530664597209714, 0.4423686283943834563, 1.771051422834311051 ) ) ;
#205212 = CARTESIAN_POINT ( 'NONE',  ( 3.727185537919291747, 2.006959858346604619, 0.1948421285040344286 ) ) ;
#205213 = CARTESIAN_POINT ( 'NONE',  ( -8.910733272679575379, 11.41894145625809820, -1.599625672291263179 ) ) ;
#205215 = CARTESIAN_POINT ( 'NONE',  ( -0.006768871532359390167, 8.210909518262125673, -2.038649385027042626 ) ) ;
#205214 = CARTESIAN_POINT ( 'NONE',  ( 3.766728628225763043, -1.521468805364207144, 1.674700015324230407 ) ) ;
#205216 = CARTESIAN_POINT ( 'NONE',  ( 5.157299734135989411, -1.777537633589726163, -1.129047594716176217 ) ) ;
#205217 = CARTESIAN_POINT ( 'NONE',  ( -11.92619526913700057, 13.52781666661243243, -1.328859060402685976 ) ) ;
#205218 = CARTESIAN_POINT ( 'NONE',  ( 2.242711981562468093, -2.029969483702593003, -0.4061203719310027549 ) ) ;
#205219 = CARTESIAN_POINT ( 'NONE',  ( 4.517891501851804215, 6.293959390292322986, -1.599625672291255185 ) ) ;
#205220 = CARTESIAN_POINT ( 'NONE',  ( 1.360316468749978469, 1.046875000341403128, -2.602085213965210642E-14 ) ) ;
#205221 = CARTESIAN_POINT ( 'NONE',  ( 5.250683377293950294, 2.089169806880130320, 0.3621421040747307973 ) ) ;
#205222 = ITEM_DEFINED_TRANSFORMATION ( 'NONE', 'NONE', #27890,  #200407 ) ;
#205224 = CARTESIAN_POINT ( 'NONE',  ( 1.225083325515680555, -0.04812572341393595021, 1.926057772195179485 ) ) ;
#205223 = CARTESIAN_POINT ( 'NONE',  ( -9.287498920561160887, 10.79416914786490089, -1.199719254218441611 ) ) ;
#205225 = CARTESIAN_POINT ( 'NONE',  ( -4.034433228518296666, 6.864533312316751790, -1.199719254218450271 ) ) ;
#205226 = CARTESIAN_POINT ( 'NONE',  ( 7.262363838414439776, 11.62450824479221900, 0.7998128361456462443 ) ) ;
#205227 = CARTESIAN_POINT ( 'NONE',  ( 6.183927461164522299, 6.387205924212962849, 0.000000000000000000 ) ) ;
#205228 = CARTESIAN_POINT ( 'NONE',  ( 4.274728378101444903, 7.249864702071729283, 0.9550516446962635797 ) ) ;
#205229 = CARTESIAN_POINT ( 'NONE',  ( -1.115562610750309283E-14, 9.593750000682799595, 1.500000000000001554 ) ) ;
#205230 = CARTESIAN_POINT ( 'NONE',  ( -4.120788623549732854, 6.895004929861607401, -1.199719254218452047 ) ) ;
#205231 = CARTESIAN_POINT ( 'NONE',  ( 0.4049022847291971483, -2.205595429402911201, -0.2640273158710532142 ) ) ;
#205232 = CARTESIAN_POINT ( 'NONE',  ( 2.186679620839627969, -2.065140684961807249, -0.4117111178513747638 ) ) ;
#205233 = CARTESIAN_POINT ( 'NONE',  ( -4.411198876399886615, 6.239761003923544713, -1.599625672291271394 ) ) ;
#205234 = CARTESIAN_POINT ( 'NONE',  ( 9.264299036839600987, 9.702770385934682551, -0.7998128361456281477 ) ) ;
#205235 = CARTESIAN_POINT ( 'NONE',  ( 6.737149535461696814, -0.09068363363158969681, -1.858830251952103385 ) ) ;
#205236 = CARTESIAN_POINT ( 'NONE',  ( 5.750629710490689384, 9.860818428881154674, -0.7998128361456291469 ) ) ;
#205237 = CARTESIAN_POINT ( 'NONE',  ( 11.89942855770814312, 9.799999999999998934, 0.6999999999999992895 ) ) ;
#205238 = CARTESIAN_POINT ( 'NONE',  ( -5.953438850176548947, 9.959779401932374654, 0.000000000000000000 ) ) ;
#205239 = CARTESIAN_POINT ( 'NONE',  ( -7.849807752632384172, 12.10193344480572897, 0.000000000000000000 ) ) ;
#205240 = CARTESIAN_POINT ( 'NONE',  ( 0.0004480315400831600455, -0.9938866557669153723, 1.873244595478529728 ) ) ;
#205241 = FACE_OUTER_BOUND ( 'NONE', #146336, .T. ) ;
#205243 = CARTESIAN_POINT ( 'NONE',  ( 3.613678190204441254, 0.4790664972640528152, -1.902336835828049244 ) ) ;
#205242 = CARTESIAN_POINT ( 'NONE',  ( 1.360316468749975582, 2.776041667008103175, 0.7853790794158820310 ) ) ;
#205244 = CARTESIAN_POINT ( 'NONE',  ( 2.465889518630470789, 2.120156730345585938, -0.4209195040108040797 ) ) ;
#205245 = CARTESIAN_POINT ( 'NONE',  ( 1.153568636672014369, 0.7464410156945017194, 1.683350060182234209 ) ) ;
#205247 = CARTESIAN_POINT ( 'NONE',  ( -5.204229338117261072, 6.461601495962581154, -1.180324454998063377 ) ) ;
#205246 = CARTESIAN_POINT ( 'NONE',  ( -3.623772196602547346, 7.449761006003425834, 0.000000000000000000 ) ) ;
#205248 = CARTESIAN_POINT ( 'NONE',  ( 2.993823619545363801, -0.5058645990140339110, -1.665172204756032448 ) ) ;
#205249 = CARTESIAN_POINT ( 'NONE',  ( 6.155038550924144758, 8.203964280876741455, 1.443375672974076540 ) ) ;
#205250 = CARTESIAN_POINT ( 'NONE',  ( -10.99298880388840338, 6.209297407268072888, -6.173882299569079635 ) ) ;
#205251 = CARTESIAN_POINT ( 'NONE',  ( 1.200320640528436789, -2.161883444890321915, 0.0006282887012112879947 ) ) ;
#205252 = AXIS2_PLACEMENT_3D ( 'NONE', #116145, #150738, #2299 ) ;
#205253 = CARTESIAN_POINT ( 'NONE',  ( 2.671249783466634220, -0.7690017779844946499, -1.863883771055181660 ) ) ;
#205254 = CARTESIAN_POINT ( 'NONE',  ( -2.428612866367529932E-14, 2.999999999999999112, 2.420000000000000373 ) ) ;
#205256 = CIRCLE ( 'NONE', #111974, 10.99999999999718980 ) ;
#205255 = CARTESIAN_POINT ( 'NONE',  ( 0.3917762336288696523, 1.602822130585265015, 1.450656209987542855 ) ) ;
#205257 = CARTESIAN_POINT ( 'NONE',  ( 2.289859582131337223, -0.8446868967569521880, 1.781483357239101117 ) ) ;
#205258 = CARTESIAN_POINT ( 'NONE',  ( -0.02319159430947542386, 0.2540490248266329965, -1.846305437520213477 ) ) ;
#205261 = ORIENTED_EDGE ( 'NONE', *, *, #171086, .T. ) ;
#205260 = CARTESIAN_POINT ( 'NONE',  ( -4.448483799059637533, 7.243629294661272588, 1.082531754730549967 ) ) ;
#205259 = DIRECTION ( 'NONE',  ( -5.578564026256490882E-16, -1.000000000000000000, -9.066213480720158442E-32 ) ) ;
#205262 = CARTESIAN_POINT ( 'NONE',  ( -5.383996397958228819, 8.335060660042973524, 1.082531754730550855 ) ) ;
#205263 = CARTESIAN_POINT ( 'NONE',  ( -0.1106856583841060310, -0.002128758811529348188, -1.996853503091333470 ) ) ;
#205264 = CARTESIAN_POINT ( 'NONE',  ( 4.929271367020211514, 7.908511140569038922, 1.199719254218452047 ) ) ;
#205265 = CARTESIAN_POINT ( 'NONE',  ( -4.308458954092677651, 8.248562223075252220, -0.7998128361456362523 ) ) ;
#205266 = CARTESIAN_POINT ( 'NONE',  ( 2.402995385916364857, -0.3474029756719719808, -1.989407454614970261 ) ) ;
#205267 = CARTESIAN_POINT ( 'NONE',  ( -7.795011973214244883, 8.058878488363559356, 0.7998128361456341429 ) ) ;
#205268 = CARTESIAN_POINT ( 'NONE',  ( -6.567365632596091629, 6.787193466117722451, -0.4468828428391571350 ) ) ;
#205269 = CARTESIAN_POINT ( 'NONE',  ( 5.438606028847273066, 2.272309368472532398, 0.4011960609803484901 ) ) ;
#205270 = CARTESIAN_POINT ( 'NONE',  ( 3.147653791585717453, 8.920000000000001705, -2.420000000000002149 ) ) ;
#205271 = AXIS2_PLACEMENT_3D ( 'NONE', #44343, #80018, #177535 ) ;
#205272 = CARTESIAN_POINT ( 'NONE',  ( 4.241029431094700541, -0.1880360549168894613, -1.952691919460777026 ) ) ;
#205273 = CARTESIAN_POINT ( 'NONE',  ( 7.262363838414439776, 11.62450824479221900, 0.7998128361456462443 ) ) ;
#205274 = CARTESIAN_POINT ( 'NONE',  ( 0.08851783505585239520, -0.5350849913869708541, 1.944072358963434333 ) ) ;
#205275 = ORIENTED_EDGE ( 'NONE', *, *, #105631, .F. ) ;
#205276 = CARTESIAN_POINT ( 'NONE',  ( 2.659486872612493613, 2.008994876937011398, -0.6687478447182227947 ) ) ;
#205277 = CARTESIAN_POINT ( 'NONE',  ( -0.7500000000000215383, 1.472916667349486008, 1.299038105676659116 ) ) ;
#205279 = CARTESIAN_POINT ( 'NONE',  ( -5.520141099058386125, 9.591915048876776595, 0.000000000000000000 ) ) ;
#205278 = CARTESIAN_POINT ( 'NONE',  ( -2.272963308585411735, 5.803540959991587478, 0.7998128361456341429 ) ) ;
#205280 = CARTESIAN_POINT ( 'NONE',  ( 2.009460956091331685, -0.8672641894471898594, -1.624084198382821587 ) ) ;
#205281 = ORIENTED_EDGE ( 'NONE', *, *, #59332, .T. ) ;
#205282 = B_SPLINE_CURVE_WITH_KNOTS ( 'NONE', 3,
 ( #145763, #16753, #30920, #45042, #47177, #63402, #194464 ),
 .UNSPECIFIED., .F., .F.,
 ( 4, 3, 4 ),
 ( 4.336808689942000884E-19, 0.0008000000000004425012, 0.002977368225425618478 ),
 .UNSPECIFIED. ) ;
#205283 = CARTESIAN_POINT ( 'NONE',  ( -8.890396042259075315, 11.39521468743417998, -1.599625672291263179 ) ) ;
#205284 = DIRECTION ( 'NONE',  ( -0.000000000000000000, -1.000000000000000000, -0.000000000000000000 ) ) ;
#205285 = CARTESIAN_POINT ( 'NONE',  ( 3.568700945156903614, 0.7666329941097769218, 1.977337035738421900 ) ) ;
#205286 = CARTESIAN_POINT ( 'NONE',  ( 0.4449246239494052402, 0.5802587426733482046, -1.747387232072565189 ) ) ;
#205287 = CARTESIAN_POINT ( 'NONE',  ( 1.499999999999991118, 5.285416667349480235, 0.8660254037844524744 ) ) ;
#205288 = CARTESIAN_POINT ( 'NONE',  ( 7.293396569147545527, 10.59638086639245280, 1.199719254218460707 ) ) ;
#205289 = CARTESIAN_POINT ( 'NONE',  ( 5.691390622686558487, 9.861982503101517139, 0.7998128361456341429 ) ) ;
#205290 = CARTESIAN_POINT ( 'NONE',  ( 3.936836037902153418, 0.2985264485904081111, 2.038899620686930536 ) ) ;
#205292 = CARTESIAN_POINT ( 'NONE',  ( 1.909461114401575843, -0.8690924446688346183, -1.623246667998109682 ) ) ;
#205291 = CARTESIAN_POINT ( 'NONE',  ( -6.527360889975461156, 9.702672574024962415, 1.199719254218452047 ) ) ;
#205293 = CARTESIAN_POINT ( 'NONE',  ( 0.6823417656249899377, 4.926041667008086655, -1.181850606188754593 ) ) ;
#205294 = PRESENTATION_STYLE_ASSIGNMENT (( #20143 ) ) ;
#205295 = CARTESIAN_POINT ( 'NONE',  ( -9.499717950937029087, -9.918872507113817960, 0.07320418461264667498 ) ) ;
#205296 = DIRECTION ( 'NONE',  ( -0.6483454320283800199, 0.000000000000000000, 0.7613463080411787542 ) ) ;
#205297 = CARTESIAN_POINT ( 'NONE',  ( 0.6103625832605160673, -2.195865045534075133, 0.2202409711149767024 ) ) ;
#205298 = CARTESIAN_POINT ( 'NONE',  ( 3.919400689748584465, -0.1713981403653370705, 2.255992170122776308 ) ) ;
#205299 = CARTESIAN_POINT ( 'NONE',  ( -9.029367117021344313, 9.636609179387466639, 0.7216878364870438212 ) ) ;
#205300 = CARTESIAN_POINT ( 'NONE',  ( 3.269578866965703767, 0.4354455071775619190, -1.758352452871074334 ) ) ;
#205301 = CARTESIAN_POINT ( 'NONE',  ( 3.714002460163209562, 1.020071527678518164, -1.621341143276352703 ) ) ;
#205302 = CARTESIAN_POINT ( 'NONE',  ( 5.371561628297467195, -0.3073141173523045167, 2.047320497149993646 ) ) ;
#205303 = CARTESIAN_POINT ( 'NONE',  ( -1.201851678989727383E-14, 3.759375000341422801, -1.575800808251660134 ) ) ;
#205304 = EDGE_CURVE ( 'NONE', #150638, #126115, #128385, .T. ) ;
#205305 = CARTESIAN_POINT ( 'NONE',  ( 2.869950281991093810, 1.053363813896515788, 1.666286737264175866 ) ) ;
#205306 = PRODUCT_RELATED_PRODUCT_CATEGORY ( 'part', '', ( #74733 ) ) ;
#205307 = CARTESIAN_POINT ( 'NONE',  ( 0.9031967280443575774, 1.573137106080691572, 1.111599351221918663 ) ) ;
#205308 = CARTESIAN_POINT ( 'NONE',  ( 3.537841792810627606, 0.8420186812403904764, -1.670516725672297031 ) ) ;
#205309 = CARTESIAN_POINT ( 'NONE',  ( 2.139721691919532098, -2.060220725375282225, 1.039829281875967570 ) ) ;
#205310 = CARTESIAN_POINT ( 'NONE',  ( 3.683913666659529795, -1.106983821303194171, -1.495880402381715824 ) ) ;
#205311 = CARTESIAN_POINT ( 'NONE',  ( -1.364683531250012516, 4.488541667008090208, -0.7879004041258300672 ) ) ;
#205312 = CARTESIAN_POINT ( 'NONE',  ( -5.434120640978981065, 5.234228924097238611, -0.7998128361456221525 ) ) ;
#205313 = CARTESIAN_POINT ( 'NONE',  ( 7.284808609244363353, 7.393364887073558656, 0.7998128361456341429 ) ) ;
#205314 = CARTESIAN_POINT ( 'NONE',  ( 11.07123604129543359, 9.799999999999998934, 0.8055550039003240848 ) ) ;
#205315 = CARTESIAN_POINT ( 'NONE',  ( 0.9441299549096024979, 0.8517545906277513845, -1.926334332536754346 ) ) ;
#205316 = CARTESIAN_POINT ( 'NONE',  ( 3.456965981360264895, 6.016582164020185530, -1.082531754730543971 ) ) ;
#205318 = LINE ( 'NONE', #75338, #7758 ) ;
#205317 = CARTESIAN_POINT ( 'NONE',  ( -1.364683531250010295, 5.551041667008087543, -0.7879004041258300672 ) ) ;
#205319 = CARTESIAN_POINT ( 'NONE',  ( 2.144932638433934002, 2.058100890041581810, 0.5106320605416380110 ) ) ;
#205320 = CARTESIAN_POINT ( 'NONE',  ( 3.853900823549051502, 8.531065964594045425, -2.447540105570114477 ) ) ;
#205321 = CARTESIAN_POINT ( 'NONE',  ( 0.5979230068290807276, 1.359733756741304811, 1.493685216911154967 ) ) ;
#205322 = CARTESIAN_POINT ( 'NONE',  ( -1.402160292154681736E-14, 0.9468750003414176941, -1.575800808251659024 ) ) ;
#205323 = CARTESIAN_POINT ( 'NONE',  ( -4.148431816101615155, 3.942184661647709198, 0.7216878364870317197 ) ) ;
#205324 = CARTESIAN_POINT ( 'NONE',  ( 5.606460214450851964, 6.499623990736163037, 1.199719254218462483 ) ) ;
#205325 = CARTESIAN_POINT ( 'NONE',  ( 0.9312127099814873077, 0.1580370610147242560, 2.155845405312675211 ) ) ;
#205326 = CARTESIAN_POINT ( 'NONE',  ( -0.6125000000000105915, 0.04166666666666901664, 1.060881119635925796 ) ) ;
#205329 = CARTESIAN_POINT ( 'NONE',  ( 4.541618270897912701, 4.400902192243413502, 1.214306433183764966E-14 ) ) ;
#205328 = DIRECTION ( 'NONE',  ( 1.779758311459934189E-16, 0.000000000000000000, -1.000000000000000000 ) ) ;
#205327 = CARTESIAN_POINT ( 'NONE',  ( 4.227110032410640095, 8.153655147779589996, 0.7998128361456271485 ) ) ;
#205330 = CARTESIAN_POINT ( 'NONE',  ( -3.546339698426324460, 6.295090860542775779, -1.199719254218450271 ) ) ;
#205331 = CARTESIAN_POINT ( 'NONE',  ( 6.315638730379727228, -1.320822524126588515, -1.523799118890494020 ) ) ;
#205332 = CARTESIAN_POINT ( 'NONE',  ( -7.809133291791416909, 11.09411069285655493, 1.082531754730549967 ) ) ;
#205333 = CARTESIAN_POINT ( 'NONE',  ( 0.3631484714031462668, 0.2087870660046411420, -2.181583536649676525 ) ) ;
#205334 = DIRECTION ( 'NONE',  ( -0.6483454320283799088, 0.000000000000000000, 0.7613463080411786432 ) ) ;
#205336 = CARTESIAN_POINT ( 'NONE',  ( -0.6823417656250003738, 10.90104166700806765, 1.181850606188754593 ) ) ;
#205335 = CARTESIAN_POINT ( 'NONE',  ( 0.1810634928296238622, -2.195609808662852824, -0.5457317257893978812 ) ) ;
#205337 = CARTESIAN_POINT ( 'NONE',  ( -8.784793466650835825, 12.33634391347959713, 1.199719254218462483 ) ) ;
#205339 = CARTESIAN_POINT ( 'NONE',  ( 0.8607750341611281053, -0.04820650858186093651, -1.915179348411770954 ) ) ;
#205338 = CARTESIAN_POINT ( 'NONE',  ( -4.229780737339226881, 7.878568593630327577, 1.040834085586084257E-14 ) ) ;
#205340 = CARTESIAN_POINT ( 'NONE',  ( -1.364683531250000748, 1.321875000341421469, 0.000000000000000000 ) ) ;
#205341 = B_SPLINE_CURVE_WITH_KNOTS ( 'NONE', 3,
 ( #82304, #29312, #147333, #213362, #161458, #160377, #64983 ),
 .UNSPECIFIED., .F., .F.,
 ( 4, 3, 4 ),
 ( 0.0001126021370636923631, 0.0006031550062628982618, 0.002006790698585272145 ),
 .UNSPECIFIED. ) ;
#205342 = LINE ( 'NONE', #120997, #57901 ) ;
#205343 = CARTESIAN_POINT ( 'NONE',  ( 3.609978820808554811, 4.211641957610042120, -7.499999999999997335 ) ) ;
#205344 = CARTESIAN_POINT ( 'NONE',  ( 2.666273504311657661, -1.189765394598929937, 1.249106299861786118 ) ) ;
#205345 = CARTESIAN_POINT ( 'NONE',  ( 5.123001941117305336, 7.070197912760590064, 1.599625672291268286 ) ) ;
#205346 = CARTESIAN_POINT ( 'NONE',  ( 0.9832602892492541269, 1.182927327958797070, 1.316506037215345426 ) ) ;
#205347 = AXIS2_PLACEMENT_3D ( 'NONE', #203785, #71653, #107451 ) ;
#205348 = CARTESIAN_POINT ( 'NONE',  ( 1.822903811843211264, 1.490285103888006280, -1.353523025221949450 ) ) ;
#205349 =( NAMED_UNIT ( * ) SI_UNIT ( $, .STERADIAN. ) SOLID_ANGLE_UNIT ( ) );
#205350 = CARTESIAN_POINT ( 'NONE',  ( 4.717920652503574175, -2.164970738276258189, 0.4266498443898231185 ) ) ;
#205351 = AXIS2_PLACEMENT_3D ( 'NONE', #28447, #73997, #92412 ) ;
#205352 = VERTEX_POINT ( 'NONE', #110050 ) ;
#205353 = CARTESIAN_POINT ( 'NONE',  ( 7.524412065460039933, 10.76193592880331984, -1.082531754730537976 ) ) ;
#205354 = CARTESIAN_POINT ( 'NONE',  ( -7.045397100956844127, 8.248660034984974132, -1.199719254218452047 ) ) ;
#205356 = CARTESIAN_POINT ( 'NONE',  ( 3.919546125582054508, -1.392558991000433011, -1.458545569310132350 ) ) ;
#205355 = CARTESIAN_POINT ( 'NONE',  ( 4.143311163141574660, 0.1052805922370502884, 2.118007119816091688 ) ) ;
#205357 = ORIENTED_EDGE ( 'NONE', *, *, #101740, .T. ) ;
#205358 = CARTESIAN_POINT ( 'NONE',  ( 5.387385936583818591, 7.378645907471495846, -1.599625672291283607 ) ) ;
#205359 = EDGE_LOOP ( 'NONE', ( #100465, #18325, #134570, #183629 ) ) ;
#205360 = CARTESIAN_POINT ( 'NONE',  ( 1.076777757339364205, -0.04213119042271313425, -1.870346338061685154 ) ) ;
#205361 = CARTESIAN_POINT ( 'NONE',  ( -10.39649820107528733, 2.629643693813587646, 5.992760101887464330 ) ) ;
#205362 = B_SPLINE_CURVE_WITH_KNOTS ( 'NONE', 3,
 ( #173658, #194135, #75061, #27369, #109768, #127099 ),
 .UNSPECIFIED., .F., .F.,
 ( 4, 2, 4 ),
 ( 0.000000000000000000, 0.0003239988925529259747, 0.0006479977851058519494 ),
 .UNSPECIFIED. ) ;
#205363 = DIRECTION ( 'NONE',  ( 0.000000000000000000, 0.000000000000000000, 1.000000000000000000 ) ) ;
#205364 = CARTESIAN_POINT ( 'NONE',  ( 0.000000000000000000, 3.079999999999999183, 0.000000000000000000 ) ) ;
#205365 = CARTESIAN_POINT ( 'NONE',  ( -3.904855289079262270, 2.800000000000024691, 0.7750000000000135669 ) ) ;
#205366 = B_SPLINE_CURVE_WITH_KNOTS ( 'NONE', 3,
 ( #141931, #123604, #172269, #173345, #140864, #71532, #58509, #205812, #124664, #42280, #120385, #186360, #60633, #210068, #77952, #10804, #194900, #159203, #46538, #111591, #160273, #112659 ),
 .UNSPECIFIED., .F., .F.,
 ( 4, 3, 3, 3, 3, 3, 3, 4 ),
 ( -1.454680003632761151E-06, 0.000000000000000000, 2.747234201905744114E-05, 5.316625080982969768E-05, 7.164957654723469569E-05, 8.369272870878160088E-05, 9.574357740280491178E-05, 0.0001078040709964582646 ),
 .UNSPECIFIED. ) ;
#205367 = CARTESIAN_POINT ( 'NONE',  ( 0.6823417656249899377, 3.238541667008085323, -1.181850606188754593 ) ) ;
#205368 = PRESENTATION_STYLE_ASSIGNMENT (( #157721 ) ) ;
#205369 = CARTESIAN_POINT ( 'NONE',  ( 5.695833931516881776, 9.659240330162777610, -0.7216878364870458196 ) ) ;
#205370 = CARTESIAN_POINT ( 'NONE',  ( -3.851925040058345573, 5.587274861525073355, -1.443375672974078761 ) ) ;
#205371 = CARTESIAN_POINT ( 'NONE',  ( -5.611095471209320174, 7.639640364534566075, 1.599625672291263179 ) ) ;
#205372 = CARTESIAN_POINT ( 'NONE',  ( 4.219064148821600746, 1.637239594409030330, -1.347683705884415106 ) ) ;
#205374 = CARTESIAN_POINT ( 'NONE',  ( -10.28816806463375144, 6.680837282875757843, -5.326249955113787848 ) ) ;
#205373 = CARTESIAN_POINT ( 'NONE',  ( -0.1296875068447882473, 5.724785194352729256, -2.420566058096422779 ) ) ;
#205375 = CARTESIAN_POINT ( 'NONE',  ( 5.782488548463037503, -1.922744423562244620, -0.4343835447332323740 ) ) ;
#205376 = CARTESIAN_POINT ( 'NONE',  ( -1.364683531250012516, 1.780208333674757615, 0.7879004041258379498 ) ) ;
#205377 = CARTESIAN_POINT ( 'NONE',  ( 0.3869771421881840201, -1.897093440144840937, -0.6742409396158774992 ) ) ;
#205378 = ORIENTED_EDGE ( 'NONE', *, *, #204318, .F. ) ;
#205379 = CARTESIAN_POINT ( 'NONE',  ( 6.175037754964278314, 1.841102675566621771, -1.045632355512320144 ) ) ;
#205380 = CARTESIAN_POINT ( 'NONE',  ( 8.776224899084631659, 13.27471476138782336, 8.184001253707570811 ) ) ;
#205381 = CARTESIAN_POINT ( 'NONE',  ( 1.029834584532058672, 1.995790600324919506, -0.5504719462680053299 ) ) ;
#205382 = VERTEX_POINT ( 'NONE', #143593 ) ;
#205383 = CARTESIAN_POINT ( 'NONE',  ( 5.071631979963703962, 8.074598522336444262, 1.199719254218451159 ) ) ;
#205384 = CARTESIAN_POINT ( 'NONE',  ( 4.701645408888975197, 8.707279753670952971, 0.000000000000000000 ) ) ;
#205386 = CARTESIAN_POINT ( 'NONE',  ( 4.873266149108180123, 7.772895376346490970, 1.199719254218462483 ) ) ;
#205385 = CARTESIAN_POINT ( 'NONE',  ( 3.539087885488776397, -1.583190213782994515, -1.365486535101219534 ) ) ;
#205388 = AXIS2_PLACEMENT_3D ( 'NONE', #125781, #108452, #28196 ) ;
#205387 = CARTESIAN_POINT ( 'NONE',  ( 6.444921918449731280, 8.612437886315108315, 1.599625672291268286 ) ) ;
#205391 = VERTEX_POINT ( 'NONE', #157682 ) ;
#205390 = CARTESIAN_POINT ( 'NONE',  ( 1.558926746901686089, -1.530267751544078347, 0.9690644009569903128 ) ) ;
#205389 = CARTESIAN_POINT ( 'NONE',  ( 2.291784574284541964, -0.7830779901500490858, 1.649245556672715995 ) ) ;
#205392 = CARTESIAN_POINT ( 'NONE',  ( 5.953802724510454780, 0.6443607167232848765, -2.110727517106169682 ) ) ;
#205393 = DIRECTION ( 'NONE',  ( -0.000000000000000000, -0.000000000000000000, 1.000000000000000000 ) ) ;
#205394 = CARTESIAN_POINT ( 'NONE',  ( 4.173040645679537697, -2.057929556117383374, -0.7971749352265260491 ) ) ;
#205395 = CARTESIAN_POINT ( 'NONE',  ( 0.6823417656249934904, 8.505208333674733723, 1.181850606188764807 ) ) ;
#205396 = CARTESIAN_POINT ( 'NONE',  ( 2.578645926699867363, -1.317302948579327504, 1.386430337501590282 ) ) ;
#205397 = CARTESIAN_POINT ( 'NONE',  ( 7.690499447449630210, 9.995335326823163058, 1.599625672291281386 ) ) ;
#205398 = CARTESIAN_POINT ( 'NONE',  ( 5.652806998763869828, -0.4994405740583847675, -2.009109930559597856 ) ) ;
#205399 = DIRECTION ( 'NONE',  ( -0.9999160831030532437, -0.01240418662286108496, 0.003736697214589113167 ) ) ;
#205400 = CARTESIAN_POINT ( 'NONE',  ( 6.409741707328596938, -1.031184584194230647, -1.933826218581576439 ) ) ;
#205401 = CARTESIAN_POINT ( 'NONE',  ( 5.612152705277200226, 7.484198595525810127, -1.333638438132278559 ) ) ;
#205402 = ORIENTED_EDGE ( 'NONE', *, *, #32385, .T. ) ;
#205403 = ORIENTED_EDGE ( 'NONE', *, *, #116869, .F. ) ;
#205404 = CARTESIAN_POINT ( 'NONE',  ( 11.40816717570227468, 3.487142912321097299, -3.706738213303538920 ) ) ;
#205405 = CARTESIAN_POINT ( 'NONE',  ( 4.224247379109608680, 7.085983154673295203, -1.199719254218452047 ) ) ;
#205406 = CARTESIAN_POINT ( 'NONE',  ( 3.285556943750000070, -2.121874999522044281, 0.000000000000000000 ) ) ;
#205407 = CARTESIAN_POINT ( 'NONE',  ( 1.214306433183764966E-14, 2.428612866367529932E-14, 1.500000000000001332 ) ) ;
#205408 = AXIS2_PLACEMENT_3D ( 'NONE', #62972, #45687, #145346 ) ;
#205409 = CARTESIAN_POINT ( 'NONE',  ( -8.188761592974051595, 9.616271948966963024, -1.082531754730543971 ) ) ;
#205410 = CARTESIAN_POINT ( 'NONE',  ( 4.278479993564246797, 7.149254538203735798, 1.199719254218452047 ) ) ;
#205411 = CARTESIAN_POINT ( 'NONE',  ( 6.209843387784004243, 0.6066176463192971546, -1.979359621541395331 ) ) ;
#205412 = CARTESIAN_POINT ( 'NONE',  ( 4.617753627809100259, -1.889021752119159459, 0.3773520080231194673 ) ) ;
#205413 = ADVANCED_FACE ( 'NONE', ( #27659 ), #158566, .T. ) ;
#205414 = CARTESIAN_POINT ( 'NONE',  ( 1.634388897023292486, 0.6352195160324504153, 1.913798142305182415 ) ) ;
#205415 = CIRCLE ( 'NONE', #94761, 1.250000000000000222 ) ;
#205416 = CARTESIAN_POINT ( 'NONE',  ( -7.960608749518247151, 12.43912730774665576, 0.000000000000000000 ) ) ;
#205417 = CARTESIAN_POINT ( 'NONE',  ( 8.154303043976348420, 8.478051404252736845, 0.7998128361456281477 ) ) ;
#205418 = CARTESIAN_POINT ( 'NONE',  ( -4.196906876117826535, 3.977091173117547562, -0.5668149747346932221 ) ) ;
#205419 = CARTESIAN_POINT ( 'NONE',  ( 1.851786237446376049, 2.185420115623282200, -0.1633297828415938846 ) ) ;
#205420 = CARTESIAN_POINT ( 'NONE',  ( 5.022008369909983116, -0.9795521577263366364, -1.540466923627185292 ) ) ;
#205421 = CARTESIAN_POINT ( 'NONE',  ( 6.373741612200174878, 6.608655767087927124, 0.7216878364870328300 ) ) ;
#205422 = CARTESIAN_POINT ( 'NONE',  ( 9.073431116043567002, 11.60875560684942265, -1.599625672291262513 ) ) ;
#205423 = CARTESIAN_POINT ( 'NONE',  ( -6.414942957921379474, 7.513130201443591005, -1.199719254218452047 ) ) ;
#205424 = CARTESIAN_POINT ( 'NONE',  ( 5.678167406024951624, 5.518950149984223508, 0.7998128361456341429 ) ) ;
#205425 = CARTESIAN_POINT ( 'NONE',  ( 4.903208829997618423, 5.749440385532527564, -1.199719254218450271 ) ) ;
#205426 = ORIENTED_EDGE ( 'NONE', *, *, #151476, .F. ) ;
#205428 = CARTESIAN_POINT ( 'NONE',  ( 6.029547050951932441, -0.2422988993314358630, 1.998484822443524322 ) ) ;
#205427 = CARTESIAN_POINT ( 'NONE',  ( 2.366542893654680402, 0.08848056876738576160, -1.839231530397527736 ) ) ;
#205429 = CARTESIAN_POINT ( 'NONE',  ( 1.775234297868668376, -2.280957755244545027, 0.2818987734495673192 ) ) ;
#205430 = CARTESIAN_POINT ( 'NONE',  ( 0.2388273096324589895, -0.1346187373043924163, -1.830540737478093982 ) ) ;
#205431 = CARTESIAN_POINT ( 'NONE',  ( -4.381256195510448315, 8.263215994737505454, 1.040834085586084257E-14 ) ) ;
#205432 = CARTESIAN_POINT ( 'NONE',  ( -15.75000000000000000, 11.29999999999999893, -3.200000000000001510 ) ) ;
#205433 = CARTESIAN_POINT ( 'NONE',  ( 2.865378420500460876, -1.565876230000915692, -1.097592462808501645 ) ) ;
#205434 = CARTESIAN_POINT ( 'NONE',  ( -2.948008335967658322, 5.526761261015804116, 1.199719254218462483 ) ) ;
#205436 = ADVANCED_FACE ( 'NONE', ( #59092 ), #33312, .T. ) ;
#205435 = CYLINDRICAL_SURFACE ( 'NONE', #171553, 0.5000000000000003331 ) ;
#205437 = CARTESIAN_POINT ( 'NONE',  ( -3.688700311369816909, 6.461178242310183784, -1.199719254218450271 ) ) ;
#205439 = CARTESIAN_POINT ( 'NONE',  ( 0.7427767429722329506, -1.606530860214189893, 0.9580933318182258684 ) ) ;
#205438 = CARTESIAN_POINT ( 'NONE',  ( 2.665665183201745947, 1.120710701610077908, 1.764813211807507942 ) ) ;
#205440 = CARTESIAN_POINT ( 'NONE',  ( 2.319685276966905629, -1.560262528187049025, 1.276846253076675541 ) ) ;
#205441 = CARTESIAN_POINT ( 'NONE',  ( 8.324343129110697959, 9.774450407793066731, -1.082531754730543083 ) ) ;
#205442 = ORIENTED_EDGE ( 'NONE', *, *, #116111, .T. ) ;
#205443 = CARTESIAN_POINT ( 'NONE',  ( -0.6823417656249969321, 4.530208333674755394, -1.181850606188749264 ) ) ;
#205444 = CARTESIAN_POINT ( 'NONE',  ( 2.577381053492054264, -0.8929794387350452611, 1.493718712549793715 ) ) ;
#205445 = CARTESIAN_POINT ( 'NONE',  ( 4.476163270806094552, 8.373940915915776273, 0.7998128361456462443 ) ) ;
#205447 =( LENGTH_UNIT ( ) NAMED_UNIT ( * ) SI_UNIT ( .MILLI., .METRE. ) );
#205446 = DIRECTION ( 'NONE',  ( -5.421010862427537947E-16, 0.000000000000000000, 1.000000000000000000 ) ) ;
#205448 = CARTESIAN_POINT ( 'NONE',  ( 3.088212622510533301, -1.699425283745788162, -0.2941843989033367524 ) ) ;
#205449 =( BOUNDED_CURVE ( )  B_SPLINE_CURVE ( 3, ( #81924, #13718, #144848, #115553 ),
 .UNSPECIFIED., .F., .T. ) 
 B_SPLINE_CURVE_WITH_KNOTS ( ( 4, 4 ),
 ( 0.5000000000000027756, 1.000000000000000000 ),
 .UNSPECIFIED. ) 
 CURVE ( )  GEOMETRIC_REPRESENTATION_ITEM ( )  RATIONAL_B_SPLINE_CURVE ( ( 0.9999999999999963363, 0.3333333333333333703, 0.3333333333333370896, 1.000000000000000000 ) ) 
 REPRESENTATION_ITEM ( '' )  );
#205450 = CARTESIAN_POINT ( 'NONE',  ( 2.894263506066748093, -0.6386881658498286818, -2.096408367471907841 ) ) ;
#205451 = CARTESIAN_POINT ( 'NONE',  ( 7.214646527853999024E-05, -1.701284277595259464, 0.3348680416483724720 ) ) ;
#205452 = CARTESIAN_POINT ( 'NONE',  ( 4.969440760808212509, 0.2186952961555181096, -2.196011921426939129 ) ) ;
#205453 = CARTESIAN_POINT ( 'NONE',  ( -9.812680342707254866, 4.108039100808300148, -6.337802944732694677 ) ) ;
#205454 = CARTESIAN_POINT ( 'NONE',  ( 2.044024736616629312, 1.494777392302085062, 1.574780046323517313 ) ) ;
#205455 = CARTESIAN_POINT ( 'NONE',  ( 1.435882461153328515, 0.9014729512111450127, -1.587519582607027635 ) ) ;
#205456 = CARTESIAN_POINT ( 'NONE',  ( 1.445368642220961508, 8.714907460504134562, -2.589984629573225838 ) ) ;
#205457 = CARTESIAN_POINT ( 'NONE',  ( 3.977823109611013930, -0.8067237889231733128, 1.957824063906116407 ) ) ;
#205458 = LINE ( 'NONE', #141586, #49466 ) ;
#205459 = ORIENTED_EDGE ( 'NONE', *, *, #5382, .F. ) ;
#205461 = CARTESIAN_POINT ( 'NONE',  ( 1.364683531249986537, 0.6760416670080884316, 0.7879004041258500513 ) ) ;
#205460 = CARTESIAN_POINT ( 'NONE',  ( 4.652058317211603011, 0.8762739730861779375, 2.118468771859642441 ) ) ;
#205462 = CARTESIAN_POINT ( 'NONE',  ( 11.44791656467458374, 11.29999999999997939, 3.303228920649577294 ) ) ;
#205463 = CARTESIAN_POINT ( 'NONE',  ( 9.297140650669039275, 11.86975006391249643, 1.599625672291281386 ) ) ;
#205464 = CARTESIAN_POINT ( 'NONE',  ( -0.07530339154229391541, -0.9103892951793614019, -1.913193754492636067 ) ) ;
#205465 = CARTESIAN_POINT ( 'NONE',  ( -5.368665641331555882, 8.246898433986675769, 1.082531754730548412 ) ) ;
#205466 = CARTESIAN_POINT ( 'NONE',  ( 4.284013352238246419, 6.021101549076499637, -1.443375672974051449 ) ) ;
#205467 = CARTESIAN_POINT ( 'NONE',  ( -4.880572110795192486, 8.637825195995631589, 1.214306433183764966E-14 ) ) ;
#205468 = EDGE_CURVE ( 'NONE', #204354, #40528, #117792, .T. ) ;
#205469 = CARTESIAN_POINT ( 'NONE',  ( 3.553645660557675612, 6.199651466408984568, -1.082531754730549967 ) ) ;
#205470 = ORIENTED_EDGE ( 'NONE', *, *, #181903, .T. ) ;
#205471 = CARTESIAN_POINT ( 'NONE',  ( 4.799454022740247794, 1.388487131293577592, -1.462444391756134943 ) ) ;
#205473 = CARTESIAN_POINT ( 'NONE',  ( 3.555586659033848740, 1.623084692090390080, 1.272569074839409398 ) ) ;
#205472 = CARTESIAN_POINT ( 'NONE',  ( 6.634017235788401301, 6.634108284708264414, 0.7998128361456341429 ) ) ;
#205475 = CARTESIAN_POINT ( 'NONE',  ( 6.883263157960364254, 6.036844454314826081, 2.541088405340941492 ) ) ;
#205474 = CARTESIAN_POINT ( 'NONE',  ( 6.902720145097993587, 14.55347103577521217, 9.761920446463554057 ) ) ;
#205476 = CARTESIAN_POINT ( 'NONE',  ( 8.039058738260216330, 8.343599714250547805, -0.7998128361456341429 ) ) ;
#205477 = CARTESIAN_POINT ( 'NONE',  ( 3.285556943749998737, -3.055208332855376518, -1.896917185911906500 ) ) ;
#205478 = SURFACE_STYLE_USAGE ( .BOTH. , #186020 ) ;
#205479 = CARTESIAN_POINT ( 'NONE',  ( 6.703104427915338448, -0.4847493572297522091, 2.145077170986497528 ) ) ;
#205480 = CARTESIAN_POINT ( 'NONE',  ( 3.604138833494671346, -0.1455340571130462057, 2.011204217620660817 ) ) ;
#205481 = CARTESIAN_POINT ( 'NONE',  ( 2.999365392321148516, -1.839032331094083927, 0.09308366406014097205 ) ) ;
#205482 = CARTESIAN_POINT ( 'NONE',  ( 4.306686350635271054, 8.176217842383143974, -0.7998128361456221525 ) ) ;
#205483 = CARTESIAN_POINT ( 'NONE',  ( 6.018537349360657984, 1.224031959697377658, -1.354583942311540667 ) ) ;
#205484 = CARTESIAN_POINT ( 'NONE',  ( -7.725448601688521322, 7.907444878258402809, 1.040834085586084257E-14 ) ) ;
#205485 = CARTESIAN_POINT ( 'NONE',  ( 6.719576162335838099, -2.196678875378419882, 0.5415391501680610897 ) ) ;
#205486 = CARTESIAN_POINT ( 'NONE',  ( 2.121831256377606501, -2.042539606455844758, 0.5128510974094899755 ) ) ;
#205487 = CARTESIAN_POINT ( 'NONE',  ( -6.445975688654487001, 6.485002823043819475, -0.7998128361456362523 ) ) ;
#205488 = CARTESIAN_POINT ( 'NONE',  ( 7.507464373665139412, 9.781794407407920389, 1.599625672291281386 ) ) ;
#205489 = CARTESIAN_POINT ( 'NONE',  ( 5.844973620822823790, 9.833236634353070826, 0.7216878364870317197 ) ) ;
#205490 = DIRECTION ( 'NONE',  ( 0.7613463080411788653, 0.000000000000000000, 0.6483454320283801309 ) ) ;
#205491 = CARTESIAN_POINT ( 'NONE',  ( -5.930802130974132780, 9.006687355190106103, -1.199719254218440723 ) ) ;
#205492 = CARTESIAN_POINT ( 'NONE',  ( 6.249945625775433555, 10.23542763013927726, -0.7216878364870267237 ) ) ;
#205493 = CARTESIAN_POINT ( 'NONE',  ( 5.239055555121258756, 6.613325079961110298, 1.380154382352281495 ) ) ;
#205494 = CARTESIAN_POINT ( 'NONE',  ( -5.708146366553361162, 6.618257834855742594, -1.199719254218446718 ) ) ;
#205496 = CARTESIAN_POINT ( 'NONE',  ( 4.219114570843409240, 1.715941675311336123, -1.410698622648777434 ) ) ;
#205495 = CARTESIAN_POINT ( 'NONE',  ( 2.127334043950947606, 1.896359100603739911, 0.9491756072362851349 ) ) ;
#205497 = CARTESIAN_POINT ( 'NONE',  ( 2.906388222866810978, 1.586772471669075424, -1.511725739355776366 ) ) ;
#205498 = CARTESIAN_POINT ( 'NONE',  ( 0.8036966383840878914, 1.806304194667744500, 1.267646993260997723 ) ) ;
#205499 = CARTESIAN_POINT ( 'NONE',  ( -4.960304097753355457, 6.880383762169266504, 1.599625672291263179 ) ) ;
#205500 = CARTESIAN_POINT ( 'NONE',  ( 4.650807877244386823, -0.4278111053654386486, -1.914496481071884970 ) ) ;
#205501 = CARTESIAN_POINT ( 'NONE',  ( 10.37606763316019531, 10.99983374830873650, 0.7998128361456462443 ) ) ;
#205502 =( NAMED_UNIT ( * ) SI_UNIT ( $, .STERADIAN. ) SOLID_ANGLE_UNIT ( ) );
#205503 = CARTESIAN_POINT ( 'NONE',  ( -1.402160292154681736E-14, 1.696875000341421469, -1.575800808251659024 ) ) ;
#205504 = CARTESIAN_POINT ( 'NONE',  ( -4.258669648468323743, 6.061810238003387141, 1.443375672974065660 ) ) ;
#205506 = VERTEX_POINT ( 'NONE', #213071 ) ;
#205505 = CARTESIAN_POINT ( 'NONE',  ( -5.260200412422200600, 8.120355666925794580, -1.082531754730544860 ) ) ;
#205507 =( BOUNDED_SURFACE ( )  B_SPLINE_SURFACE ( 3, 2, ( 
 ( #4370, #101909, #120367 ),
 ( #5435, #71514, #19580 ),
 ( #22759, #88876, #85652 ),
 ( #70440, #151739, #186342 ),
 ( #157882, #137626, #171169 ),
 ( #55294, #95017, #11598 ),
 ( #12658, #128653, #13729 ),
 ( #27859, #144856, #113450 ) ),
 .UNSPECIFIED., .F., .F., .T. ) 
 B_SPLINE_SURFACE_WITH_KNOTS ( ( 4, 2, 2, 4 ),
 ( 3, 3 ),
 ( 0.000000000000000000, 0.0004924884914732721459, 0.0007387327372099082188, 0.0009849769829465442918 ),
 ( 0.000000000000000000, 1.000000000000000000 ),
 .UNSPECIFIED. ) 
 GEOMETRIC_REPRESENTATION_ITEM ( )  RATIONAL_B_SPLINE_SURFACE ( (
 ( 1.000000000000000000, 0.7045118851637635071, 1.000000000000000000),
 ( 1.000000000000000000, 0.7593505504062313394, 1.000000000000000000),
 ( 1.000000000000000000, 0.8104906253035955022, 1.000000000000000000),
 ( 1.000000000000000000, 0.8722646935499712706, 1.000000000000000000),
 ( 1.000000000000000000, 0.8905178607894789211, 1.000000000000000000),
 ( 1.000000000000000000, 0.9170530604353609450, 1.000000000000000000),
 ( 1.000000000000000000, 0.9248184710077420601, 1.000000000000000000),
 ( 1.000000000000000000, 0.9238795325112880708, 1.000000000000000000) ) ) 
 REPRESENTATION_ITEM ( '' )  SURFACE ( )  );
#205508 = CARTESIAN_POINT ( 'NONE',  ( 3.902672080109194752, -2.098000727953463151, -0.3078000538283761078 ) ) ;
#205509 = CARTESIAN_POINT ( 'NONE',  ( -4.014095998097799267, 6.840806543492835345, -1.199719254218450271 ) ) ;
#205510 = CARTESIAN_POINT ( 'NONE',  ( 5.383715653711652394, 1.448795075966866852, 1.604530791579752202 ) ) ;
#205511 = CARTESIAN_POINT ( 'NONE',  ( 3.737712173649463399, 1.832726675769575486, 0.1767833568970395008 ) ) ;
#205512 = CARTESIAN_POINT ( 'NONE',  ( -5.803933766307007858, 6.065161521460068705, 0.5445525043519475750 ) ) ;
#205513 = CARTESIAN_POINT ( 'NONE',  ( 1.364683531249988535, 1.426041667008083991, 0.7879004041258500513 ) ) ;
#205514 = CARTESIAN_POINT ( 'NONE',  ( 6.439394946090388316, 0.6587646163928980725, -1.611052209844960670 ) ) ;
#205515 = CARTESIAN_POINT ( 'NONE',  ( 6.827182134110201694, 1.288579688585177685, 1.926502426867699569 ) ) ;
#205516 = CARTESIAN_POINT ( 'NONE',  ( 3.036663219780971978, 6.486598156479028709, -0.7216878364870267237 ) ) ;
#205517 = CARTESIAN_POINT ( 'NONE',  ( 11.96864102214210135, 6.616705618073630113, -0.9970986697839275825 ) ) ;
#205518 = CARTESIAN_POINT ( 'NONE',  ( 4.522454563201145028, 1.332364063043836033, -1.702191164408660251 ) ) ;
#205519 = CARTESIAN_POINT ( 'NONE',  ( -5.284980951228653190, 5.060232619388524533, 0.000000000000000000 ) ) ;
#205520 = CARTESIAN_POINT ( 'NONE',  ( 6.081407632663145435, 1.356090666932512789, -1.492028312255622824 ) ) ;
#205521 = CARTESIAN_POINT ( 'NONE',  ( -8.148087131688692253, 9.568818410800712826, -1.082531754730543083 ) ) ;
#205522 = CARTESIAN_POINT ( 'NONE',  ( 3.907220446582274853, 1.852832235905249370, 1.113321777468062823 ) ) ;
#205523 = CARTESIAN_POINT ( 'NONE',  ( 4.973880039175529788, 1.132619354422999436, 1.613344424267410204 ) ) ;
#205524 = CARTESIAN_POINT ( 'NONE',  ( 4.024493581903946016, 1.720846971656955438, -0.2109413284564972679 ) ) ;
#205525 = CARTESIAN_POINT ( 'NONE',  ( 0.5565083568685527116, -1.583368386835169783, 1.515454571103365344 ) ) ;
#205526 = CARTESIAN_POINT ( 'NONE',  ( 0.6577796130948220243, -1.951556776833747620, -1.231164357708439017 ) ) ;
#205527 = CARTESIAN_POINT ( 'NONE',  ( 3.866525002278593526, -1.386861471309716265, 1.524430686435477522 ) ) ;
#205528 = CARTESIAN_POINT ( 'NONE',  ( 5.530791563722144311, -1.753914071513791528, 0.8342105869050663314 ) ) ;
#205529 = CARTESIAN_POINT ( 'NONE',  ( -8.825994812371996900, 9.399341490629888440, 0.7216878364870438212 ) ) ;
#205530 = CARTESIAN_POINT ( 'NONE',  ( -4.294900800479008574, 8.232744377192641849, 0.000000000000000000 ) ) ;
#205532 = VERTEX_POINT ( 'NONE', #149151 ) ;
#205531 = CARTESIAN_POINT ( 'NONE',  ( -1.907519672996902838, 3.236073672982390903, -0.4612874649730039911 ) ) ;
#205533 = CARTESIAN_POINT ( 'NONE',  ( -7.659993601596720936, 8.999375959026737704, -1.082531754730543083 ) ) ;
#205534 = CARTESIAN_POINT ( 'NONE',  ( 2.116530880626496192, -1.040147864624408003, -1.946245422063937802 ) ) ;
#205535 = CARTESIAN_POINT ( 'NONE',  ( 1.642778471875000035, -4.163541666188708135, -2.845375778867859751 ) ) ;
#205536 = EDGE_LOOP ( 'NONE', ( #141769, #211278, #208475, #79293 ) ) ;
#205537 = CARTESIAN_POINT ( 'NONE',  ( 0.4439182389155779673, -0.8842316343482552465, 1.637490449460777153 ) ) ;
#205538 = CARTESIAN_POINT ( 'NONE',  ( -0.1291982275798443380, 0.7147424134107607241, -2.157361641090648874 ) ) ;
#205539 = CARTESIAN_POINT ( 'NONE',  ( 1.499999999999990896, 5.056250000682820378, 1.214306433183764966E-14 ) ) ;
#205540 = CARTESIAN_POINT ( 'NONE',  ( 4.707942587747941943, 7.051207734045064512, -1.383178547476830111 ) ) ;
#205542 = CARTESIAN_POINT ( 'NONE',  ( -10.99943592164172657, -8.240513804456425007, 0.1113975120798868373 ) ) ;
#205541 = DIRECTION ( 'NONE',  ( 0.000000000000000000, 1.000000000000000000, -8.546850786086437571E-32 ) ) ;
#205543 = VERTEX_POINT ( 'NONE', #730 ) ;
#205544 = CARTESIAN_POINT ( 'NONE',  ( 2.553650737195617637, 0.5510486643308718513, -1.985768735985605549 ) ) ;
#205545 = CARTESIAN_POINT ( 'NONE',  ( 0.6801582343749831283, 1.057291667008075642, -1.178068619123862515 ) ) ;
#205546 = CARTESIAN_POINT ( 'NONE',  ( -7.854251061018346469, 8.057714414143200443, -0.7998128361456291469 ) ) ;
#205547 = CARTESIAN_POINT ( 'NONE',  ( 3.486133158594716510E-16, 2.312499999999992006, 1.224999999999971889 ) ) ;
#205548 =( LENGTH_UNIT ( ) NAMED_UNIT ( * ) SI_UNIT ( .MILLI., .METRE. ) );
#205549 = CARTESIAN_POINT ( 'NONE',  ( 3.928111819657337911, 5.605883094398769195, 1.599625672291267398 ) ) ;
#205550 = CARTESIAN_POINT ( 'NONE',  ( 0.7431281084272289839, -1.767980789219452342, 1.058748425497215262 ) ) ;
#205552 = CARTESIAN_POINT ( 'NONE',  ( 4.669393045487420402, 1.064170941109745305, 1.502380130741477693 ) ) ;
#205551 = CARTESIAN_POINT ( 'NONE',  ( -2.788906526875773208E-15, 12.43750000000000000, -1.499999999999998446 ) ) ;
#205553 = CARTESIAN_POINT ( 'NONE',  ( 7.644099680006512187, 7.812537802962739697, 1.040834085586084257E-14 ) ) ;
#205554 = CARTESIAN_POINT ( 'NONE',  ( -6.306477729012051725, 7.386587434382707151, 1.199719254218452047 ) ) ;
#205556 = ORIENTED_EDGE ( 'NONE', *, *, #7000, .T. ) ;
#205555 = CARTESIAN_POINT ( 'NONE',  ( -5.546112223000226216, 5.929839062422638918, -0.8878705470019981894 ) ) ;
#205557 = CARTESIAN_POINT ( 'NONE',  ( 4.899154391205060577, 1.836108854712194649, -1.224054507610386366 ) ) ;
#205558 = CARTESIAN_POINT ( 'NONE',  ( 0.2808502495336914206, -2.096634173354972486, -0.5254431554712820640 ) ) ;
#205559 = CARTESIAN_POINT ( 'NONE',  ( -5.585596099150191840, 7.539614753807099667, -1.443375672974052559 ) ) ;
#205560 = CARTESIAN_POINT ( 'NONE',  ( 0.4043728756845180183, -1.898191424145349471, -0.2318213773434482650 ) ) ;
#205561 = CARTESIAN_POINT ( 'NONE',  ( 0.5851731681005939434, 1.651346252830317551, 1.157095189655330314 ) ) ;
#205562 = CARTESIAN_POINT ( 'NONE',  ( 7.960045584554727327, 8.459343734834927631, 0.7216878364870267237 ) ) ;
#205563 = ADVANCED_FACE ( 'NONE', ( #200019 ), #51671, .T. ) ;
#205564 = CARTESIAN_POINT ( 'NONE',  ( 7.901650181845425891, 15.38517925215461979, -9.032942408684748514 ) ) ;
#205565 = CARTESIAN_POINT ( 'NONE',  ( 0.4019237886466816012, 12.20758545099816672, -1.499999999999998668 ) ) ;
#205566 = CARTESIAN_POINT ( 'NONE',  ( 3.673896439623286714, 4.156855427197417185, -7.499999999999997335 ) ) ;
#205567 = AXIS2_PLACEMENT_3D ( 'NONE', #91185, #142084, #110685 ) ;
#205568 = CARTESIAN_POINT ( 'NONE',  ( 0.4615142869485132637, 1.850934062480696252, -0.2700578556205368574 ) ) ;
#205569 = CARTESIAN_POINT ( 'NONE',  ( 1.921111612355221654, -1.799121770747251547, 0.9110121207814986244 ) ) ;
#205571 = CARTESIAN_POINT ( 'NONE',  ( -5.175390966358026645, 6.917902677759380836, 1.252160023617815643 ) ) ;
#205570 = CARTESIAN_POINT ( 'NONE',  ( -0.6823417656250212460, 0.8010416670080899859, 1.181850606188755259 ) ) ;
#205573 = CARTESIAN_POINT ( 'NONE',  ( 4.529967234949650035, -1.295318019757265349, -1.660530462842347177 ) ) ;
#205572 = CARTESIAN_POINT ( 'NONE',  ( -7.503547950159405566, 10.84155747757291266, 1.199719254218453823 ) ) ;
#205574 = AXIS2_PLACEMENT_3D ( 'NONE', #201120, #182752, #98319 ) ;
#205575 = CARTESIAN_POINT ( 'NONE',  ( 9.094822116668764167, 9.505047312402055582, 0.7998128361456462443 ) ) ;
#205577 = CARTESIAN_POINT ( 'NONE',  ( -9.189729191964438826, 9.615772233580322848, 1.040834085586084257E-14 ) ) ;
#205576 = CARTESIAN_POINT ( 'NONE',  ( 4.817943484809818600, 6.714296380401858499, 1.599625672291269396 ) ) ;
#205578 = CARTESIAN_POINT ( 'NONE',  ( -0.3106162252735292229, -6.604184692106364274, -9.611175950047666561 ) ) ;
#205579 = CARTESIAN_POINT ( 'NONE',  ( 3.832289616293593770, -1.041828873002103917, -1.730228960026259255 ) ) ;
#205580 = CARTESIAN_POINT ( 'NONE',  ( 0.6823417656249899377, 4.426041667008086655, -1.181850606188754593 ) ) ;
#205581 = CARTESIAN_POINT ( 'NONE',  ( 6.039522989413334209, 1.907243403200251208, -0.7859975451465596175 ) ) ;
#205582 = CARTESIAN_POINT ( 'NONE',  ( 8.676855123066012254, 11.14608361504227574, -1.443375672974052559 ) ) ;
#205583 = CARTESIAN_POINT ( 'NONE',  ( 4.147864318636265146, 0.7325676050485960822, -2.033789780341701547 ) ) ;
#205584 = CARTESIAN_POINT ( 'NONE',  ( 6.875920180786008196, 8.050936961452347163, -1.199719254218452047 ) ) ;
#205585 = CARTESIAN_POINT ( 'NONE',  ( 1.364683531249986537, -0.3239583329919163424, 0.7879004041258500513 ) ) ;
#205587 = CYLINDRICAL_SURFACE ( 'NONE', #41411, 0.3999999999999997446 ) ;
#205586 = CARTESIAN_POINT ( 'NONE',  ( 5.668190738965027897, 8.770583741171307679, -1.199719254218452047 ) ) ;
#205588 = CARTESIAN_POINT ( 'NONE',  ( 6.588899466117086767, 10.63087377720454363, 1.040834085586084257E-14 ) ) ;
#205590 = CARTESIAN_POINT ( 'NONE',  ( -15.75000000000000000, 13.40000000000000036, -1.100000000000002087 ) ) ;
#205589 = CARTESIAN_POINT ( 'NONE',  ( 1.979201191301533047, 2.025398335218126622, 0.7825711269493199618 ) ) ;
#205592 = CARTESIAN_POINT ( 'NONE',  ( 1.259045258496578557, 1.813921241667546758, -0.3151448728593714277 ) ) ;
#205591 = CARTESIAN_POINT ( 'NONE',  ( -4.595850885352567694, 8.305650432979225783, 1.040834085586084257E-14 ) ) ;
#205593 = CARTESIAN_POINT ( 'NONE',  ( 1.364683531249988535, 2.363541667008088432, 0.7879004041258500513 ) ) ;
#205594 = CARTESIAN_POINT ( 'NONE',  ( 3.527062600443749307, -2.024233912922444478, 0.8403589366152917073 ) ) ;
#205595 = CARTESIAN_POINT ( 'NONE',  ( 6.983263157960362122, 6.035089925019382129, 2.648702789725385198 ) ) ;
#205596 = CARTESIAN_POINT ( 'NONE',  ( 3.872163259867720253, 1.254437384476282835, 1.882731698358128369 ) ) ;
#205597 = CARTESIAN_POINT ( 'NONE',  ( -6.170932472514347289, 10.35117165124207972, 0.000000000000000000 ) ) ;
#205598 = CARTESIAN_POINT ( 'NONE',  ( 1.364683531249988535, 4.467708333674754506, -0.7879004041258300672 ) ) ;
#205599 = CARTESIAN_POINT ( 'NONE',  ( 6.492781079782697695, 6.747302000852300807, 0.03582484399037785816 ) ) ;
#205600 = CARTESIAN_POINT ( 'NONE',  ( -1.500000000000001110, 14.27083333333333215, 0.8660254037844419273 ) ) ;
#205601 = CARTESIAN_POINT ( 'NONE',  ( 4.394251184604957672, 8.140727125432173139, -0.7216878364870357165 ) ) ;
#205602 = CARTESIAN_POINT ( 'NONE',  ( 5.413276439055476175, -0.2588944790761596448, 1.750576072867173316 ) ) ;
#205603 = CARTESIAN_POINT ( 'NONE',  ( 8.606728586576791074, 8.935604860628076906, 0.7998128361456462443 ) ) ;
#205604 = CARTESIAN_POINT ( 'NONE',  ( 1.676933785844336944, -1.999498008410249383, -0.6612845060171600453 ) ) ;
#205607 = ADVANCED_FACE ( 'NONE', ( #129801 ), #89517, .F. ) ;
#205606 = CARTESIAN_POINT ( 'NONE',  ( 0.7499999999999885647, 1.066666666666687968, -1.299038105676652899 ) ) ;
#205605 = CARTESIAN_POINT ( 'NONE',  ( -0.6823417656250039265, 10.31770833367473550, -1.181850606188755259 ) ) ;
#205608 = CARTESIAN_POINT ( 'NONE',  ( 1.310928286630644646, -1.554615626247756177, 1.209165358520351674 ) ) ;
#205609 = CARTESIAN_POINT ( 'NONE',  ( -4.659162064951642535, 5.464719159645540003, 1.199719254218452935 ) ) ;
#205610 = CARTESIAN_POINT ( 'NONE',  ( 3.615147460157889903, 7.348606074266929689, 0.4009180521483968196 ) ) ;
#205612 = ORIENTED_EDGE ( 'NONE', *, *, #84925, .T. ) ;
#205611 = CARTESIAN_POINT ( 'NONE',  ( 6.082253981448354274, 0.9392408507493594794, 1.548964021007705139 ) ) ;
#205613 = CARTESIAN_POINT ( 'NONE',  ( 8.270110514656037637, 8.750809809961280550, 0.7216878364870458196 ) ) ;
#205614 = CARTESIAN_POINT ( 'NONE',  ( 5.242975984329111050, -1.603930480038592510, 0.9624218375651681923 ) ) ;
#205615 = CARTESIAN_POINT ( 'NONE',  ( 4.944224162298806569, -0.9806570695735459253, 1.823293813017504039 ) ) ;
#205616 = CARTESIAN_POINT ( 'NONE',  ( 0.6125000000000001554, 2.166666666666670960, -1.060881119635941339 ) ) ;
#205617 = CARTESIAN_POINT ( 'NONE',  ( -6.278834536460198734, 6.497930845391236332, 0.7216878364870257245 ) ) ;
#205618 =( NAMED_UNIT ( * ) PLANE_ANGLE_UNIT ( ) SI_UNIT ( $, .RADIAN. ) );
#205619 = CARTESIAN_POINT ( 'NONE',  ( 9.074484886248265880, 9.481320543578137361, 0.7998128361456462443 ) ) ;
#205620 = CARTESIAN_POINT ( 'NONE',  ( -4.080641063585716211, 5.783833847506671511, -1.249999999999999334 ) ) ;
#205621 = CARTESIAN_POINT ( 'NONE',  ( 7.506374323821472849, 8.786466794993730289, -1.199719254218452047 ) ) ;
#205622 = EDGE_CURVE ( 'NONE', #119038, #31723, #182344, .T. ) ;
#205623 = CARTESIAN_POINT ( 'NONE',  ( -5.081322649207705489, 6.519081843335746029, -1.217513467538652305 ) ) ;
#205624 = CARTESIAN_POINT ( 'NONE',  ( -0.6823417656250003738, 0.2177083336747515085, -1.181850606188749264 ) ) ;
#205626 = VECTOR ( 'NONE', #27702, 1000.000000000000000 ) ;
#205625 = CARTESIAN_POINT ( 'NONE',  ( -0.7500000000000215383, 1.441666666666688190, 1.299038105676659116 ) ) ;
#205628 = CARTESIAN_POINT ( 'NONE',  ( 4.449046963578762615, 8.342305224150557308, -0.7998128361456231517 ) ) ;
#205627 = CARTESIAN_POINT ( 'NONE',  ( 4.492601031306558745, 1.923586649950057792, 0.3847822903023030428 ) ) ;
#205629 = CARTESIAN_POINT ( 'NONE',  ( 2.020861031540205133, 2.010896488828680440, -0.1455087364366919322 ) ) ;
#205630 =( BOUNDED_CURVE ( )  B_SPLINE_CURVE ( 2, ( #42451, #159371, #45642, #95475, #108557, #44578, #13108, #79185, #59737, #25094, #177764, #175642, #211306, #27228, #93335, #26162, #28304, #158323, #62931, #125895, #129099, #195071, #8847, #46710, #61873, #94399, #10969, #77043, #78114, #126964, #192922, #128038, #193993, #112824, #111759, #31518, #148464, #15233, #33, #99702, #162584, #84511, #165773, #66097, #133302, #114945, #16289, #14159, #150599, #113900, #67167, #80253, #197192, #137291, #178840, #147399, #1106, #71173, #48831, #180945, #17356, #100758, #2160, #132239, #82374, #163651, #199307, #149520, #198247 ),
 .UNSPECIFIED., .F., .T. ) 
 B_SPLINE_CURVE_WITH_KNOTS ( ( 3, 2, 2, 2, 2, 2, 2, 2, 2, 2, 2, 2, 2, 2, 2, 2, 2, 2, 2, 2, 2, 2, 2, 2, 2, 2, 2, 2, 2, 2, 2, 2, 2, 2, 3 ),
 ( 0.1422369605164288953, 0.1458333333333333426, 0.1499999999999999944, 0.1541666666666666741, 0.1583333333333333259, 0.1625000000000000056, 0.1666666666666666574, 0.1708333333333333370, 0.1749999999999999889, 0.1791666666666666685, 0.1833333333333333204, 0.1875000000000000000, 0.1916666666666666796, 0.1958333333333333315, 0.2000000000000000111, 0.2041666666666666630, 0.2083333333333333426, 0.2124999999999999944, 0.2166666666666666741, 0.2208333333333333259, 0.2250000000000000056, 0.2291666666666666574, 0.2333333333333333370, 0.2374999999999999889, 0.2416666666666666685, 0.2458333333333333204, 0.2500000000000000000, 0.2541666666666666519, 0.2583333333333333592, 0.2625000000000000111, 0.2666666666666666630, 0.2708333333333333148, 0.2750000000000000222, 0.2791666666666666741, 0.2794680684751273403 ),
 .UNSPECIFIED. ) 
 CURVE ( )  GEOMETRIC_REPRESENTATION_ITEM ( )  RATIONAL_B_SPLINE_CURVE ( ( 0.9683452906431684326, 0.8843625769635057310, 1.000000000000000000, 0.8660254037844387076, 1.000000000000000000, 0.8660254037844387076, 1.000000000000000000, 0.8660254037844387076, 1.000000000000000000, 0.8660254037844387076, 1.000000000000000000, 0.8660254037844387076, 1.000000000000000000, 0.8660254037844387076, 1.000000000000000000, 0.8660254037844387076, 1.000000000000000000, 0.8660254037844387076, 1.000000000000000000, 0.8660254037844387076, 1.000000000000000000, 0.8660254037844387076, 1.000000000000000000, 0.8660254037844387076, 1.000000000000000000, 0.8660254037844387076, 1.000000000000000000, 0.8660254037844387076, 1.000000000000000000, 0.8660254037844387076, 1.000000000000000000, 0.8660254037844387076, 1.000000000000000000, 0.8660254037844387076, 1.000000000000000000, 0.8660254037844387076, 1.000000000000000000, 0.8660254037844387076, 1.000000000000000000, 0.8660254037844387076, 1.000000000000000000, 0.8660254037844387076, 1.000000000000000000, 0.8660254037844387076, 1.000000000000000000, 0.8660254037844387076, 1.000000000000000000, 0.8660254037844387076, 1.000000000000000000, 0.8660254037844387076, 1.000000000000000000, 0.8660254037844387076, 1.000000000000000000, 0.8660254037844387076, 1.000000000000000000, 0.8660254037844387076, 1.000000000000000000, 0.8660254037844387076, 1.000000000000000000, 0.8660254037844387076, 1.000000000000000000, 0.8660254037844387076, 1.000000000000000000, 0.8660254037844387076, 1.000000000000000000, 0.8660254037844387076, 1.000000000000000000, 0.9903087554590821462, 0.9820195710609804784 ) ) 
 REPRESENTATION_ITEM ( '' )  );
#205631 = CARTESIAN_POINT ( 'NONE',  ( -11.88156762547254175, 9.720000084540298957, 1.686557021358693564 ) ) ;
#205632 = CARTESIAN_POINT ( 'NONE',  ( 1.915107840602244593, -0.2339084544023955492, 1.855816807740391150 ) ) ;
#205633 = CARTESIAN_POINT ( 'NONE',  ( -1.001543065824772872E-14, 5.571875000341416140, 1.575800808251672791 ) ) ;
#205634 = CARTESIAN_POINT ( 'NONE',  ( 4.025643311844375738, -0.3400233446379635760, 1.984125136466656558 ) ) ;
#205635 = CARTESIAN_POINT ( 'NONE',  ( -8.995998617867369873, 10.45408546138876993, 1.199719254218462483 ) ) ;
#205637 = CARTESIAN_POINT ( 'NONE',  ( 2.970428505833659472, -2.086373159142587586, -0.3592635996705355050 ) ) ;
#205636 = CARTESIAN_POINT ( 'NONE',  ( -6.249945626219832739, 6.393950773452325542, 1.040834085586084257E-14 ) ) ;
#205638 = CARTESIAN_POINT ( 'NONE',  ( -1.499999999999997780, 4.931250000682820378, 1.214306433183764966E-14 ) ) ;
#205639 = CARTESIAN_POINT ( 'NONE',  ( 4.738769824615551407, -2.007376682328159134, -0.5062664373569197851 ) ) ;
#205640 = CARTESIAN_POINT ( 'NONE',  ( 4.844006021832467646, 8.873367135438366304, 0.000000000000000000 ) ) ;
#205642 = CARTESIAN_POINT ( 'NONE',  ( 6.620655732516649294, 0.5674144795907026806, 2.226195167976598110 ) ) ;
#205641 = CARTESIAN_POINT ( 'NONE',  ( 0.9957797365991372107, -2.090933974770115444, 0.003689723154384760839 ) ) ;
#205644 = VERTEX_POINT ( 'NONE', #73225 ) ;
#205643 = CARTESIAN_POINT ( 'NONE',  ( 6.651389018303578204, -1.468406013062272253, -1.084454090978362428 ) ) ;
#205645 = CARTESIAN_POINT ( 'NONE',  ( 7.263417608619159083, 9.497073181520933716, -1.599625672291262513 ) ) ;
#205646 = CARTESIAN_POINT ( 'NONE',  ( 8.043985462411169962, -6.893136966056886195, -7.503460210123559015 ) ) ;
#205647 = DIRECTION ( 'NONE',  ( 0.000000000000000000, 1.000000000000000000, 0.000000000000000000 ) ) ;
#205648 = CARTESIAN_POINT ( 'NONE',  ( -11.25356361929547688, 4.972433335311166935, 5.839389443199928920 ) ) ;
#205649 = CARTESIAN_POINT ( 'NONE',  ( 7.904040366642695048, 9.284097184913720824, 1.082531754730558626 ) ) ;
#205650 = CARTESIAN_POINT ( 'NONE',  ( -1.402160292154681736E-14, 12.48437500034139802, 1.575800808251682339 ) ) ;
#205651 = CARTESIAN_POINT ( 'NONE',  ( 6.235011639695052565, 1.786057601157979180, 0.6837302122261402770 ) ) ;
#205652 = CARTESIAN_POINT ( 'NONE',  ( -8.296699936558862731, 11.76690146170562201, 1.199719254218453823 ) ) ;
#205653 = CARTESIAN_POINT ( 'NONE',  ( 6.277588818327314080, 7.282607361925381717, 1.199719254218462483 ) ) ;
#205654 = CARTESIAN_POINT ( 'NONE',  ( -11.91826849282518452, 10.89999999999999858, -1.400000000000001465 ) ) ;
#205655 = CARTESIAN_POINT ( 'NONE',  ( 3.267151830768944443, 4.834763107362302748, -1.443375672974058777 ) ) ;
#205656 = DIRECTION ( 'NONE',  ( 0.000000000000000000, -1.000000000000000000, 0.000000000000000000 ) ) ;
#205657 = CARTESIAN_POINT ( 'NONE',  ( 3.521367211247359741, 5.131347717920458962, -1.599625672291262513 ) ) ;
#205658 = ORIENTED_EDGE ( 'NONE', *, *, #30312, .T. ) ;
#205659 = CARTESIAN_POINT ( 'NONE',  ( -7.259464905474441565, 7.434073576000447048, -0.7998128361456362523 ) ) ;
#205660 = CARTESIAN_POINT ( 'NONE',  ( 5.132435489663482286, 0.5880379476735001498, 1.928747580961232444 ) ) ;
#205661 = PLANE ( 'NONE',  #38553 ) ;
#205662 = CARTESIAN_POINT ( 'NONE',  ( 10.96027417533446524, -7.850147675656145907, -0.3662874062585380619 ) ) ;
#205663 = CARTESIAN_POINT ( 'NONE',  ( 0.1399997263886038068, 6.947785072119228467, -2.594798351071639253 ) ) ;
#205664 = CARTESIAN_POINT ( 'NONE',  ( -4.446711195602245148, 7.171284913969171448, -1.082531754730549967 ) ) ;
#205665 = CARTESIAN_POINT ( 'NONE',  ( 9.625925876022625616, 11.29296361252366765, -1.082531754730537088 ) ) ;
#205666 = CARTESIAN_POINT ( 'NONE',  ( 2.114047118560181016, 1.964524245714272643, -0.1396653253868378186 ) ) ;
#205667 = CARTESIAN_POINT ( 'NONE',  ( 4.587517648402447357, -0.5350702435001615243, 1.944077497823355483 ) ) ;
#205668 = CARTESIAN_POINT ( 'NONE',  ( -6.124532705071231931, 8.168374127381657246, -1.599625672291263179 ) ) ;
#205669 = CARTESIAN_POINT ( 'NONE',  ( 6.727182134110196721, 7.051813866762763006, 2.787205683092201181 ) ) ;
#205670 = CARTESIAN_POINT ( 'NONE',  ( 4.382901342696458258, 1.958101449220098988, -0.9841704303943515919 ) ) ;
#205671 = CARTESIAN_POINT ( 'NONE',  ( 4.549612403093820312, 8.500000000000243361, -0.2314049244472246580 ) ) ;
#205672 = CARTESIAN_POINT ( 'NONE',  ( 3.469672154888691296, 1.879743449303279634, -0.4207095485242727806 ) ) ;
#205673 = CARTESIAN_POINT ( 'NONE',  ( -9.481229494658258261, 9.955855920056455588, -0.7998128361456291469 ) ) ;
#205674 = CARTESIAN_POINT ( 'NONE',  ( 1.203941962966154744, 3.072768152887747739, 0.7750000000000065725 ) ) ;
#205675 = CARTESIAN_POINT ( 'NONE',  ( 0.04788047853313340263, -1.708876078042343316, -1.396090968258607790 ) ) ;
#205676 = CARTESIAN_POINT ( 'NONE',  ( -2.273105066167325550, 5.702484939155337607, -7.499999999999997335 ) ) ;
#205677 = CARTESIAN_POINT ( 'NONE',  ( -1.364683531250000748, 13.35937500034139980, 0.000000000000000000 ) ) ;
#205678 = CARTESIAN_POINT ( 'NONE',  ( 4.798696304233017074, 7.685897223992134819, -1.199719254218452047 ) ) ;
#205679 = CARTESIAN_POINT ( 'NONE',  ( -6.689804758640344851, -7.818797203689483943, 6.745710774230989415 ) ) ;
#205680 = CARTESIAN_POINT ( 'NONE',  ( 3.757017964762656703, 7.397288368949487491, -1.734723475976807094E-15 ) ) ;
#205681 = ORIENTED_EDGE ( 'NONE', *, *, #122569, .T. ) ;
#205683 = CARTESIAN_POINT ( 'NONE',  ( 2.473293533796361299, -1.752518403998115426, -0.9904139345979168230 ) ) ;
#205682 = CARTESIAN_POINT ( 'NONE',  ( 6.058133912487986272, -1.297239342979487509, 1.306937132449899508 ) ) ;
#205684 = CARTESIAN_POINT ( 'NONE',  ( 5.325646502758397460, -1.669998024346308618, 1.579374382026963675 ) ) ;
#205686 = CARTESIAN_POINT ( 'NONE',  ( 2.869781510094356669, -1.841417136736220650, 0.2678509365347056526 ) ) ;
#205685 = CARTESIAN_POINT ( 'NONE',  ( -6.420668264523499147, 9.648474187656182366, 1.199719254218452935 ) ) ;
#205687 = FACE_OUTER_BOUND ( 'NONE', #7116, .T. ) ;
#205688 = CARTESIAN_POINT ( 'NONE',  ( 0.09999999999999592548, -9.999999999999994671, 6.938893903907228378E-15 ) ) ;
#205689 = CARTESIAN_POINT ( 'NONE',  ( 10.32992389895506413, 1.000000000000000888, 6.106772653521394645 ) ) ;
#205690 = CARTESIAN_POINT ( 'NONE',  ( -5.533699252672048985, 9.607732894759390518, -0.7998128361456231517 ) ) ;
#205691 = EDGE_CURVE ( 'NONE', #163734, #160319, #174432, .T. ) ;
#205692 = CARTESIAN_POINT ( 'NONE',  ( -4.665414256878301025, 6.536345614481700927, -1.443375672974066548 ) ) ;
#205693 = CARTESIAN_POINT ( 'NONE',  ( 6.356985058417449430, 0.3567463788109735967, -2.059909276252298582 ) ) ;
#205694 = CARTESIAN_POINT ( 'NONE',  ( 4.826339496784873617, 8.574553812983598533, -0.7216878364870257245 ) ) ;
#205695 = ORIENTED_EDGE ( 'NONE', *, *, #172187, .F. ) ;
#205696 = CARTESIAN_POINT ( 'NONE',  ( -0.1099460098627005888, 6.494484681433106310, 3.110387376256865011 ) ) ;
#205698 = CARTESIAN_POINT ( 'NONE',  ( 3.948449050077836642, 5.629609863222681199, 1.599625672291267398 ) ) ;
#205697 = DIRECTION ( 'NONE',  ( 5.551115123125764213E-17, 0.000000000000000000, -1.000000000000000000 ) ) ;
#205699 = CARTESIAN_POINT ( 'NONE',  ( 5.953657690368134858, 0.4940546211441557700, -1.652608054245385372 ) ) ;
#205700 = CARTESIAN_POINT ( 'NONE',  ( -5.708146366553361162, 6.618257834855742594, -1.199719254218446718 ) ) ;
#205701 = CARTESIAN_POINT ( 'NONE',  ( 1.986549370914699963, -1.733795460411426959, 0.04323319158786724514 ) ) ;
#205702 = CARTESIAN_POINT ( 'NONE',  ( -1.785986935459600966, 14.55200959964326124, 11.82982753855158542 ) ) ;
#205703 = CARTESIAN_POINT ( 'NONE',  ( 0.000000000000000000, 1.000000000000000888, 0.000000000000000000 ) ) ;
#205704 = CARTESIAN_POINT ( 'NONE',  ( -5.194745412330402878, 9.212286747694129474, 0.000000000000000000 ) ) ;
#205705 = FACE_OUTER_BOUND ( 'NONE', #96617, .T. ) ;
#205706 = CARTESIAN_POINT ( 'NONE',  ( 0.5849358142855852760, 1.980036476162419845, 0.6043757699017647811 ) ) ;
#205707 = CARTESIAN_POINT ( 'NONE',  ( 5.320859459983126705, 1.688362619374352613, 0.6951667914897319278 ) ) ;
#205708 = CARTESIAN_POINT ( 'NONE',  ( 2.131626046773547500, 1.878804184644796926, -0.5645400877590660560 ) ) ;
#205709 = DIRECTION ( 'NONE',  ( 0.000000000000000000, 0.000000000000000000, -1.000000000000000000 ) ) ;
#205710 = CARTESIAN_POINT ( 'NONE',  ( 5.858531774436539052, 6.007577623030311287, 0.000000000000000000 ) ) ;
#205711 = CARTESIAN_POINT ( 'NONE',  ( 7.800018446563675489, 7.994443030612759848, -0.7998128361456281477 ) ) ;
#205712 = CARTESIAN_POINT ( 'NONE',  ( 3.457788318579996467, -1.606868461378293755, -1.383752881913953292 ) ) ;
#205713 = CARTESIAN_POINT ( 'NONE',  ( -1.854049621773913525, 4.999999999999997335, 0.7500000000000006661 ) ) ;
#205714 = CARTESIAN_POINT ( 'NONE',  ( -5.704936041347759001, 6.126156357109620032, -0.7369488182252960096 ) ) ;
#205715 = CARTESIAN_POINT ( 'NONE',  ( 1.903268718874175480, -1.751121435885591548, 1.104011288380807532 ) ) ;
#205717 = CARTESIAN_POINT ( 'NONE',  ( 0.7500000000000006661, 15.19791666734946567, -1.299038105676657340 ) ) ;
#205716 = CARTESIAN_POINT ( 'NONE',  ( -11.46094690312891551, 3.019799309332925841, 3.723887386306169667 ) ) ;
#205720 = ORIENTED_EDGE ( 'NONE', *, *, #92993, .F. ) ;
#205719 = CARTESIAN_POINT ( 'NONE',  ( 2.912952216767932256, -0.6468334258018549887, -2.125021405654815787 ) ) ;
#205718 = VECTOR ( 'NONE', #49579, 1000.000000000000114 ) ;
#205721 = CARTESIAN_POINT ( 'NONE',  ( 1.424907242902058613, -1.669187457468356950, -1.580674740522235888 ) ) ;
#205723 = CARTESIAN_POINT ( 'NONE',  ( 6.420768979138045118, -1.462686491410120970, 1.454469991251945649 ) ) ;
#205722 = CARTESIAN_POINT ( 'NONE',  ( 8.107412671292022921, 12.40247251657532956, 0.7216878364870438212 ) ) ;
#205725 = CARTESIAN_POINT ( 'NONE',  ( 3.285556943750000514, -3.813541666188710710, 1.896917185911906500 ) ) ;
#205724 = CARTESIAN_POINT ( 'NONE',  ( 3.366167277942881064, 7.149221934233827014, -0.7998128361456362523 ) ) ;
#205726 = DIRECTION ( 'NONE',  ( 1.000000000000000000, 0.000000000000000000, 0.000000000000000000 ) ) ;
#205727 = FACE_OUTER_BOUND ( 'NONE', #116089, .T. ) ;
#205728 = EDGE_CURVE ( 'NONE', #67222, #16465, #107631, .T. ) ;
#205729 = CARTESIAN_POINT ( 'NONE',  ( -0.1106727585415940990, -0.002281114264979232885, -2.003378291782103027 ) ) ;
#205730 = CARTESIAN_POINT ( 'NONE',  ( 2.994803049195310596, 1.480226043003279424, -0.8850232739186939535 ) ) ;
#205731 = CARTESIAN_POINT ( 'NONE',  ( 2.026577684455236561, 0.4465047249504557891, 1.966304233017155845 ) ) ;
#205732 = CARTESIAN_POINT ( 'NONE',  ( 2.567332952821321790, -1.178922594190381146, 1.973231532614614148 ) ) ;
#205733 = CIRCLE ( 'NONE', #146876, 0.08000000000000015432 ) ;
#205734 = CARTESIAN_POINT ( 'NONE',  ( 3.110884140487602867, 1.641001393266024788, -1.557680395459557499 ) ) ;
#205735 = CARTESIAN_POINT ( 'NONE',  ( 5.444006973519509351, 0.8546016068469390881, -1.925070404590538242 ) ) ;
#205736 = CARTESIAN_POINT ( 'NONE',  ( -6.075462232699549325, 9.141770800574526845, 1.082531754730549967 ) ) ;
#205737 = ORIENTED_EDGE ( 'NONE', *, *, #45640, .T. ) ;
#205738 = CARTESIAN_POINT ( 'NONE',  ( 3.567426164108201903, 1.727176351593662007, -0.3850055527321315507 ) ) ;
#205740 = CARTESIAN_POINT ( 'NONE',  ( 0.5688445697737016804, -2.160344153581617022, -0.7667740616737575010 ) ) ;
#205739 = CARTESIAN_POINT ( 'NONE',  ( 7.364013710877980401, 8.620379413226322285, -1.199719254218452047 ) ) ;
#205741 = CARTESIAN_POINT ( 'NONE',  ( 5.859284738525260217, 1.813109059707292747, -0.3191327317438249489 ) ) ;
#205742 = CARTESIAN_POINT ( 'NONE',  ( -5.135841261478327979, 4.886236314679810455, 0.7998128361456341429 ) ) ;
#205743 = UNCERTAINTY_MEASURE_WITH_UNIT (LENGTH_MEASURE( 1.000000000000000082E-05 ), #183504, 'distance_accuracy_value', 'NONE');
#205744 = CARTESIAN_POINT ( 'NONE',  ( 5.683573789218531402, -0.9880169931659465998, 1.956149625775935430 ) ) ;
#205745 = CARTESIAN_POINT ( 'NONE',  ( -2.676845263694313637, 5.210404343363602919, -1.199719254218446718 ) ) ;
#205746 = CARTESIAN_POINT ( 'NONE',  ( -0.8416405318397626178, 15.44692714072533590, 11.95990509367077514 ) ) ;
#205747 = CARTESIAN_POINT ( 'NONE',  ( 6.426242046702522082, 1.060841730010402495, 1.777776562702712226 ) ) ;
#205748 = CARTESIAN_POINT ( 'NONE',  ( 0.05782782957228919940, 1.164991625563294386, 1.645756161228327130 ) ) ;
#205749 = B_SPLINE_CURVE_WITH_KNOTS ( 'NONE', 3,
 ( #209915, #14908, #109315, #161193, #142843, #113576, #76727, #43202 ),
 .UNSPECIFIED., .F., .F.,
 ( 4, 2, 2, 4 ),
 ( 0.000000000000000000, 0.0004970278158210351136, 0.0007455417237315527246, 0.0009940556316420702272 ),
 .UNSPECIFIED. ) ;
#205750 = CARTESIAN_POINT ( 'NONE',  ( -1.402160292154681736E-14, -0.6312499993171797330, -1.732050807568870754 ) ) ;
#205751 = CARTESIAN_POINT ( 'NONE',  ( 4.565017902933249161, -1.721472425840556930, -0.8649740032428044900 ) ) ;
#205752 = CARTESIAN_POINT ( 'NONE',  ( 0.6823417656249934904, 10.19270833367473550, 1.181850606188764807 ) ) ;
#205754 = DIRECTION ( 'NONE',  ( 0.000000000000000000, 0.000000000000000000, -1.000000000000000000 ) ) ;
#205753 = CIRCLE ( 'NONE', #43291, 1.829047314007942848 ) ;
#205755 = CARTESIAN_POINT ( 'NONE',  ( 1.283751863706618535, 0.1568931172264090290, -2.215910488618375584 ) ) ;
#205757 = ORIENTED_EDGE ( 'NONE', *, *, #162598, .T. ) ;
#205756 = CARTESIAN_POINT ( 'NONE',  ( 2.891631901464575272, 6.595597328342462262, 0.000000000000000000 ) ) ;
#205759 = FILL_AREA_STYLE ('',( #55261 ) ) ;
#205758 = CARTESIAN_POINT ( 'NONE',  ( -4.855228407469635243, 4.837057028235559386, 0.7216878364870257245 ) ) ;
#205760 = CARTESIAN_POINT ( 'NONE',  ( 4.376584659113025744, 4.000436945253625254, 0.7998128361456341429 ) ) ;
#205761 = CARTESIAN_POINT ( 'NONE',  ( 0.000000000000000000, 7.250000000000006217, 7.750000000000000888 ) ) ;
#205762 = CARTESIAN_POINT ( 'NONE',  ( -11.97929049433705373, 11.37999999999999901, 0.7046979865771783036 ) ) ;
#205763 = CARTESIAN_POINT ( 'NONE',  ( 11.08832952072288869, 9.065454946559635019, 4.456401202325765531 ) ) ;
#205764 = CARTESIAN_POINT ( 'NONE',  ( -1.474414414893379099, 7.826756755319753900, 10.64843978026286386 ) ) ;
#205765 = CARTESIAN_POINT ( 'NONE',  ( 1.275752070009423367, -1.914805681740685106, 0.4264308320794732432 ) ) ;
#205766 = CARTESIAN_POINT ( 'NONE',  ( 1.364683531249986537, 1.967708333674750731, -0.7879004041258239610 ) ) ;
#205767 = EDGE_CURVE ( 'NONE', #104455, #214357, #174727, .T. ) ;
#205768 = DIRECTION ( 'NONE',  ( -1.000000000000000000, 0.000000000000000000, 0.000000000000000000 ) ) ;
#205769 = CARTESIAN_POINT ( 'NONE',  ( 0.4321753131953905980, 1.186194839137414414, 1.687308244272892166 ) ) ;
#205770 = CARTESIAN_POINT ( 'NONE',  ( -9.833741488613570780, 10.36711991300432345, 0.7998128361456462443 ) ) ;
#205771 = CARTESIAN_POINT ( 'NONE',  ( -4.975479186090865369, 6.827811688571220117, 1.443375672974064550 ) ) ;
#205772 = B_SPLINE_CURVE_WITH_KNOTS ( 'NONE', 3,
 ( #58120, #127483, #42966, #109074, #124279, #190237 ),
 .UNSPECIFIED., .F., .F.,
 ( 4, 2, 4 ),
 ( 0.000000000000000000, 0.0006181257251340652832, 0.001236251450268130566 ),
 .UNSPECIFIED. ) ;
#205773 = CARTESIAN_POINT ( 'NONE',  ( 0.6204658552826959328, -1.213099742399858627, -1.909634413763374283 ) ) ;
#205775 = ORIENTED_EDGE ( 'NONE', *, *, #87967, .T. ) ;
#205774 = CARTESIAN_POINT ( 'NONE',  ( -5.018489415352746619, 9.006654751220198207, 0.7998128361456481317 ) ) ;
#205776 = CARTESIAN_POINT ( 'NONE',  ( -1.001543065824772872E-14, 5.571875000341416140, 1.575800808251672791 ) ) ;
#205777 = CARTESIAN_POINT ( 'NONE',  ( 1.124039026005444475, 1.118881483734196935, -1.498852260102357947 ) ) ;
#205778 = CARTESIAN_POINT ( 'NONE',  ( 0.3868564640647629282, -0.5820622975930835885, -1.633661194748408541 ) ) ;
#205780 = CARTESIAN_POINT ( 'NONE',  ( 4.458633810090739225, -1.957822973221786444, -0.9849130632908836835 ) ) ;
#205779 = CARTESIAN_POINT ( 'NONE',  ( -1.360316468750072838, 1.661458333674769694, 0.7853790794158601596 ) ) ;
#205781 = CARTESIAN_POINT ( 'NONE',  ( 4.542184868284099508, 0.9910628492805847456, -2.084066998532303483 ) ) ;
#205782 = CARTESIAN_POINT ( 'NONE',  ( 0.3564142383026321914, 0.7882222137287850927, 1.904402214580179331 ) ) ;
#205783 = CARTESIAN_POINT ( 'NONE',  ( 2.835803868134049388, 1.927321602952759338, 0.2373744266383533696 ) ) ;
#205784 = CARTESIAN_POINT ( 'NONE',  ( -4.243338890952892406, 7.894386439512932618, -0.7216878364870257245 ) ) ;
#205785 = CIRCLE ( 'NONE', #91721, 0.04999999999999929501 ) ;
#205786 = CARTESIAN_POINT ( 'NONE',  ( 0.4572639771135831865, 13.35664422513058547, -1.309345794938320928 ) ) ;
#205787 = CARTESIAN_POINT ( 'NONE',  ( 5.203433420164765622, 1.869144303625443371, -1.001675624404389620 ) ) ;
#205788 = CARTESIAN_POINT ( 'NONE',  ( 1.360316468749953600, 0.4947916670081084489, 0.7853790794158861388 ) ) ;
#205789 = CARTESIAN_POINT ( 'NONE',  ( 3.955704058034177351, -1.882473782773282700, -0.7231407674024927790 ) ) ;
#205790 = CARTESIAN_POINT ( 'NONE',  ( -4.229780737339226881, 7.878568593630327577, 1.040834085586084257E-14 ) ) ;
#205791 = CARTESIAN_POINT ( 'NONE',  ( -7.767895665986912057, 8.027242796598338614, -0.7998128361456362523 ) ) ;
#205792 = CARTESIAN_POINT ( 'NONE',  ( 8.374132434735052755, 12.92157160716627295, -0.7998128361456352531 ) ) ;
#205793 = CARTESIAN_POINT ( 'NONE',  ( 0.6272434487209905818, -1.734552980249819631, 0.5698080454362154379 ) ) ;
#205794 = CARTESIAN_POINT ( 'NONE',  ( -6.069210040772897052, 7.109775131437022999, -1.199719254218453823 ) ) ;
#205795 = CARTESIAN_POINT ( 'NONE',  ( -1.499999999999997780, 3.650000000000021227, 1.214306433183764966E-14 ) ) ;
#205796 = CARTESIAN_POINT ( 'NONE',  ( -9.978677811866239367, 3.146997876264563843, 6.103086072356673775 ) ) ;
#205797 = ORIENTED_EDGE ( 'NONE', *, *, #204645, .T. ) ;
#205798 = CARTESIAN_POINT ( 'NONE',  ( 5.928604924596339032, 1.985460353506541376, 0.5521678710885301600 ) ) ;
#205799 = CARTESIAN_POINT ( 'NONE',  ( -6.902509602688818191, 9.146290184594002781, -1.443375672974066548 ) ) ;
#205800 = CARTESIAN_POINT ( 'NONE',  ( 5.994113310573177422, 10.00723293906178846, 0.000000000000000000 ) ) ;
#205801 = CARTESIAN_POINT ( 'NONE',  ( -2.930533758848195447, 6.570706485298192234, -0.7998128361456281477 ) ) ;
#205802 = CARTESIAN_POINT ( 'NONE',  ( -10.08065090696061716, 11.71951313199760136, -1.199719254218441611 ) ) ;
#205803 = CARTESIAN_POINT ( 'NONE',  ( 4.705726078268232193, 1.497967940706146805, 1.354894159888963001 ) ) ;
#205805 = VERTEX_POINT ( 'NONE', #201077 ) ;
#205804 = CARTESIAN_POINT ( 'NONE',  ( 6.024141157665446222, -2.204869988984262896, 0.2693334978098835264 ) ) ;
#205807 = CARTESIAN_POINT ( 'NONE',  ( 8.324343129110697959, 9.774450407793066731, -1.082531754730543083 ) ) ;
#205806 = CARTESIAN_POINT ( 'NONE',  ( -6.912678218121246942, 9.158153569265168770, 1.599625672291269396 ) ) ;
#205808 = CARTESIAN_POINT ( 'NONE',  ( 6.993308306550549247, 7.053281200597435685, 1.040834085586084257E-14 ) ) ;
#205809 = CARTESIAN_POINT ( 'NONE',  ( 3.871991401782824749, 1.143396993664235417, 1.714400680826788426 ) ) ;
#205810 = CARTESIAN_POINT ( 'NONE',  ( 4.535779832184696936, -1.617819081767550182, 1.203352566194588746 ) ) ;
#205811 = EDGE_LOOP ( 'NONE', ( #32001, #213585, #110748, #117206 ) ) ;
#205812 = CARTESIAN_POINT ( 'NONE',  ( 1.914442667406926812, 3.262253226108007720, -0.4355078757044270610 ) ) ;
#205813 = CARTESIAN_POINT ( 'NONE',  ( 5.203632029546647608, 4.965325544092860532, 1.040834085586084257E-14 ) ) ;
#205815 = ORIENTED_EDGE ( 'NONE', *, *, #42056, .F. ) ;
#205814 = CARTESIAN_POINT ( 'NONE',  ( -7.781453819600577582, 8.043060642480948985, 0.000000000000000000 ) ) ;
#205816 = CARTESIAN_POINT ( 'NONE',  ( 5.348725299209624140, 7.591689785053232775, -1.238827213252717163 ) ) ;
#205817 = CARTESIAN_POINT ( 'NONE',  ( 4.235703761680151835, -1.880146911114020325, -0.7282675588539261335 ) ) ;
#205818 = CARTESIAN_POINT ( 'NONE',  ( 2.730204174461122069, 0.2256132759956077649, 1.827196471909063202 ) ) ;
#205819 = CARTESIAN_POINT ( 'NONE',  ( -0.007339009020582241277, 15.44567596354698402, 11.95332398895799386 ) ) ;
#205820 = CARTESIAN_POINT ( 'NONE',  ( 1.594773108836315956, -2.296930430523877575, -0.2226743027769726713 ) ) ;
#205821 = CARTESIAN_POINT ( 'NONE',  ( 4.869313445963426190, 5.709895770826003414, 1.199719254218452935 ) ) ;
#205822 = EDGE_CURVE ( 'NONE', #175582, #54346, #6640, .T. ) ;
#205823 = CARTESIAN_POINT ( 'NONE',  ( 4.077527805175058973, 2.036875575534887961, -0.7240464584713502960 ) ) ;
#205824 = CARTESIAN_POINT ( 'NONE',  ( 9.206149998879153529, 10.69926207256923689, 1.199719254218453823 ) ) ;
#205825 = CARTESIAN_POINT ( 'NONE',  ( -4.564291269294938225, 8.476756914152748124, 1.040834085586084257E-14 ) ) ;
#205826 = CARTESIAN_POINT ( 'NONE',  ( 3.532835791020246141, 2.243242391287715964, -0.4999081842005962395 ) ) ;
#205827 = EDGE_CURVE ( 'NONE', #23166, #137780, #6081, .T. ) ;
#205828 = DIRECTION ( 'NONE',  ( 1.000000000000000000, 0.000000000000000000, 0.000000000000000000 ) ) ;
#205829 = CARTESIAN_POINT ( 'NONE',  ( 2.658895327995167701, -1.626580691111865207, -0.9237732865615968514 ) ) ;
#205830 = CARTESIAN_POINT ( 'NONE',  ( 6.772342980177176841, -1.213407086615119423, 1.554582774731553707 ) ) ;
#205832 = CARTESIAN_POINT ( 'NONE',  ( -7.937372586157736443, 8.224965870130965584, 0.7998128361456341429 ) ) ;
#205831 = CARTESIAN_POINT ( 'NONE',  ( 0.6823417656249917140, 4.592708333674755394, 1.181850606188765695 ) ) ;
#205834 = CARTESIAN_POINT ( 'NONE',  ( 1.102499568101540817, -2.207063161980229005, 0.003256074490760872773 ) ) ;
#205833 = CARTESIAN_POINT ( 'NONE',  ( -4.726989112658928072, 8.666571064744069020, 1.040834085586084257E-14 ) ) ;
#205835 = DIRECTION ( 'NONE',  ( -0.000000000000000000, -0.000000000000000000, 1.000000000000000000 ) ) ;
#205836 = CARTESIAN_POINT ( 'NONE',  ( 6.356075086708249167, 6.309842444114747373, -0.7998128361456281477 ) ) ;
#205837 = CARTESIAN_POINT ( 'NONE',  ( -5.331380718671772101, 7.243030143248949670, -1.599625672291256295 ) ) ;
#205838 = CARTESIAN_POINT ( 'NONE',  ( -0.003376046620573100454, -7.161464053357560644, -9.586610838029425707 ) ) ;
#205839 = CARTESIAN_POINT ( 'NONE',  ( 6.350460794227542394, 0.6179267841925452087, 1.872200446973372179 ) ) ;
#205840 = CARTESIAN_POINT ( 'NONE',  ( 5.356226580172758212, 2.305273348739949935, -0.1085102657557151934 ) ) ;
#205842 = ADVANCED_FACE ( 'NONE', ( #54863 ), #91561, .T. ) ;
#205841 = CARTESIAN_POINT ( 'NONE',  ( 6.689920442068890694, -1.216917952458838270, -1.408172490277598721 ) ) ;
#205843 = CARTESIAN_POINT ( 'NONE',  ( 3.379784452013841367, -1.989113752706978433, 0.5454275443767720999 ) ) ;
#205844 = CARTESIAN_POINT ( 'NONE',  ( 7.321039761699430493, 7.643560598178549270, -0.7216878364870257245 ) ) ;
#205845 = CARTESIAN_POINT ( 'NONE',  ( 5.820193082016415609, 10.01225203898631655, 0.000000000000000000 ) ) ;
#205846 = CARTESIAN_POINT ( 'NONE',  ( 7.741342523278707866, 8.133913820021057006, 0.7216878364870458196 ) ) ;
#205847 = CARTESIAN_POINT ( 'NONE',  ( -1.364683531250012516, 3.551041667008086211, -0.7879004041258300672 ) ) ;
#205848 = CARTESIAN_POINT ( 'NONE',  ( -7.084991283289517661, 14.48020839276600213, 9.695715787647801065 ) ) ;
#205849 = CARTESIAN_POINT ( 'NONE',  ( 5.978782553502139940, 6.077593855281705260, -0.7216878364870257245 ) ) ;
#205850 = CARTESIAN_POINT ( 'NONE',  ( 5.283699308645180892, -2.063335151747126339, 0.6760268296895615148 ) ) ;
#205852 = CARTESIAN_POINT ( 'NONE',  ( 5.179192671508887180, 1.240781939916297372, 1.360553736468192554 ) ) ;
#205851 = CARTESIAN_POINT ( 'NONE',  ( 2.680963302752393140, 0.4848410213525467527, -0.1005551520456971076 ) ) ;
#205854 = CARTESIAN_POINT ( 'NONE',  ( 6.620655732516643965, 2.083750514537034970, 2.135603474206409835 ) ) ;
#205853 = DIRECTION ( 'NONE',  ( 0.000000000000000000, 1.000000000000000000, 0.000000000000000000 ) ) ;
#205855 = CARTESIAN_POINT ( 'NONE',  ( 6.603104432341277530, -0.4828188497946246382, 2.145653685147373313 ) ) ;
#205856 = CARTESIAN_POINT ( 'NONE',  ( 0.000000000000000000, 0.9330127018934565308, 0.000000000000000000 ) ) ;
#205857 = CARTESIAN_POINT ( 'NONE',  ( 6.596538519236475828, -0.5955016034951933213, -2.182694285642503562 ) ) ;
#205858 = CARTESIAN_POINT ( 'NONE',  ( -4.712061673757400371, 7.041017223283659199, 1.411098259540758182 ) ) ;
#205859 = CARTESIAN_POINT ( 'NONE',  ( -0.9999999999999965583, 6.120000000000022311, 1.226552901175238481E-14 ) ) ;
#205860 = CARTESIAN_POINT ( 'NONE',  ( 6.606590233575550641, 6.765807905838774339, 0.03828827652692379235 ) ) ;
#205861 = CARTESIAN_POINT ( 'NONE',  ( -3.811250578772981346, 6.500190537660166079, -1.082531754730546636 ) ) ;
#205862 = CARTESIAN_POINT ( 'NONE',  ( 0.5043727151736315806, -1.897847990334254886, -0.2338014693106793551 ) ) ;
#205863 = CARTESIAN_POINT ( 'NONE',  ( 1.445802646165544880, 1.767618460842989014, 0.09138547110125286310 ) ) ;
#205864 = CARTESIAN_POINT ( 'NONE',  ( 6.024093331079843239, -1.997604944964962437, 0.2488386476607491182 ) ) ;
#205866 = CARTESIAN_POINT ( 'NONE',  ( 3.251485182540703622, 1.868192404686802810, -0.4227579483004426653 ) ) ;
#205865 = CARTESIAN_POINT ( 'NONE',  ( -4.243338890952916387, 4.052909582307567149, -0.7216878364870207285 ) ) ;
#205867 = CARTESIAN_POINT ( 'NONE',  ( 3.277320446201373638, 4.846626492033466072, 1.599625672291267398 ) ) ;
#205868 = CARTESIAN_POINT ( 'NONE',  ( 4.105875410593727182, 0.6658617523271005423, -1.853701319000864656 ) ) ;
#205869 = CARTESIAN_POINT ( 'NONE',  ( 0.2641366190093488164, 0.6592694798918593557, -2.015615888626711705 ) ) ;
#205870 = CARTESIAN_POINT ( 'NONE',  ( -4.485049888022365927, 4.126979712314507331, 0.7998128361456341429 ) ) ;
#205871 = CARTESIAN_POINT ( 'NONE',  ( 2.412791964582483129, 1.669947582624079274, 0.8431454209596804805 ) ) ;
#205873 = VERTEX_POINT ( 'NONE', #33110 ) ;
#205872 = CARTESIAN_POINT ( 'NONE',  ( 5.953657690368134858, 0.4940546211441557700, -1.652608054245385372 ) ) ;
#205875 = CARTESIAN_POINT ( 'NONE',  ( 4.744990575102895569, 5.598539094783909320, -1.082531754730548412 ) ) ;
#205874 = CARTESIAN_POINT ( 'NONE',  ( 2.842613246588860942, 2.190307313262893185, 0.2694104812042824038 ) ) ;
#205876 = CARTESIAN_POINT ( 'NONE',  ( 1.364683531249988535, 3.217708333674748289, -0.7879004041258239610 ) ) ;
#205877 = CARTESIAN_POINT ( 'NONE',  ( 6.109812101310618360, 0.5708666350849945781, -1.876949146916474298 ) ) ;
#205878 = CARTESIAN_POINT ( 'NONE',  ( 7.065770611016287006, 11.39514947949436774, 1.040834085586084257E-14 ) ) ;
#205880 = CARTESIAN_POINT ( 'NONE',  ( -9.938290294017125603, 11.55342575023019691, -1.199719254218441611 ) ) ;
#205879 = CIRCLE ( 'NONE', #84673, 11.95586206896552284 ) ;
#205881 = CARTESIAN_POINT ( 'NONE',  ( 0.2376451031371469291, -9.050179744156142903, -9.497303347810662544 ) ) ;
#205882 = CARTESIAN_POINT ( 'NONE',  ( -3.255929445576174697, 6.950334786480839355, -0.7998128361456282587 ) ) ;
#205883 = CARTESIAN_POINT ( 'NONE',  ( -10.55905904256947636, -5.631911363926716874, 0.4368516432692268747 ) ) ;
#205884 = EDGE_LOOP ( 'NONE', ( #162824, #57447, #153461, #145228, #66608 ) ) ;
#205885 = CARTESIAN_POINT ( 'NONE',  ( 2.295452831283749440, -1.850383948470477602, 0.9288054807428181014 ) ) ;
#205887 = CARTESIAN_POINT ( 'NONE',  ( 0.7499999999999885647, 3.316666666666689967, -1.299038105676658228 ) ) ;
#205886 = CIRCLE ( 'NONE', #60703, 10.24999999999999822 ) ;
#205888 = CARTESIAN_POINT ( 'NONE',  ( 5.172599298813543633, 5.993452922492633839, -1.199719254218452047 ) ) ;
#205889 = CARTESIAN_POINT ( 'NONE',  ( 4.041212305325117882, 6.872442235258051646, -1.199719254218448494 ) ) ;
#205891 = EDGE_CURVE ( 'NONE', #152360, #130259, #13655, .T. ) ;
#205890 = CARTESIAN_POINT ( 'NONE',  ( 0.1354234094306828728, -0.09670520914860020190, 2.017474364592846570 ) ) ;
#205892 = CARTESIAN_POINT ( 'NONE',  ( -1.364683531249997417, 3.509375000341423245, 1.214306433183764966E-14 ) ) ;
#205893 = EDGE_CURVE ( 'NONE', #49215, #42278, #79176, .T. ) ;
#205895 = CARTESIAN_POINT ( 'NONE',  ( 9.164948653157988900, 11.71552606681625619, -1.443375672974057666 ) ) ;
#205894 = DIRECTION ( 'NONE',  ( 0.000000000000000000, 1.000000000000000000, 0.000000000000000000 ) ) ;
#205896 = CARTESIAN_POINT ( 'NONE',  ( 5.448592227559037049, 1.351948914259465173, 1.495821383734572851 ) ) ;
#205897 = CARTESIAN_POINT ( 'NONE',  ( 4.469893758321111576, -0.8975064867107468425, 1.692437687186749917 ) ) ;
#205898 = CARTESIAN_POINT ( 'NONE',  ( 6.539320575229249144, 2.442570667128646900, 2.385998263081292148 ) ) ;
#205899 = CARTESIAN_POINT ( 'NONE',  ( 2.261505105119133052, 2.148611799745976381, -0.4309092228176118478 ) ) ;
#205900 = CARTESIAN_POINT ( 'NONE',  ( -1.499999999999997780, 2.431250000682817713, 1.214306433183764966E-14 ) ) ;
#205901 = CARTESIAN_POINT ( 'NONE',  ( 1.933716311909070784, -1.854087253938462299, 0.4680378644332865989 ) ) ;
#205902 = CARTESIAN_POINT ( 'NONE',  ( -6.715366157470410435, 6.729015360003925750, -0.7998128361456291469 ) ) ;
#205904 = CARTESIAN_POINT ( 'NONE',  ( 0.2105648349144396136, 1.930425396462841725, 0.5826343419270895163 ) ) ;
#205903 = CARTESIAN_POINT ( 'NONE',  ( 1.833030277982334422, 9.001999999999998892, -2.500000000000000444 ) ) ;
#205905 = CARTESIAN_POINT ( 'NONE',  ( -1.364683531250014514, 9.151041667008060543, -0.7879004041258335089 ) ) ;
#205907 = CARTESIAN_POINT ( 'NONE',  ( -5.010620288702242853, 8.003418215864698482, -1.199719254218453823 ) ) ;
#205906 = CARTESIAN_POINT ( 'NONE',  ( 5.636325218313963603, 0.4264374063192889475, 2.149501299143250055 ) ) ;
#205909 = ORIENTED_EDGE ( 'NONE', *, *, #147648, .T. ) ;
#205908 = CARTESIAN_POINT ( 'NONE',  ( 3.117853853556023846, -0.8486709934477435491, -1.501428560464845630 ) ) ;
#205910 = CARTESIAN_POINT ( 'NONE',  ( 5.906510592826289319, -2.110524776404258507, -0.2060971850248518311 ) ) ;
#205911 = CARTESIAN_POINT ( 'NONE',  ( 4.039439701867726384, 6.800097854565950506, 1.199719254218462483 ) ) ;
#205912 = CARTESIAN_POINT ( 'NONE',  ( -1.320903661431851450, 13.37576698399828956, 0.3874755904549384566 ) ) ;
#205913 = CARTESIAN_POINT ( 'NONE',  ( 10.59782195348455680, 13.80000000000000249, -3.302675849420335208 ) ) ;
#205914 = DIRECTION ( 'NONE',  ( 0.000000000000000000, 0.000000000000000000, 1.000000000000000000 ) ) ;
#205915 = CARTESIAN_POINT ( 'NONE',  ( 5.412729640353754590, 7.337937218544611895, 1.599625672291267398 ) ) ;
#205916 = CARTESIAN_POINT ( 'NONE',  ( 0.1399997263886038068, 0.2431072571701595186, -2.034387401959360187 ) ) ;
#205917 = VERTEX_POINT ( 'NONE', #213956 ) ;
#205918 = DIRECTION ( 'NONE',  ( 0.000000000000000000, 0.000000000000000000, 1.000000000000000000 ) ) ;
#205919 = ORIENTED_EDGE ( 'NONE', *, *, #135941, .T. ) ;
#205920 = CARTESIAN_POINT ( 'NONE',  ( 2.648825499136245654, 0.2233988552288330709, 1.797577217741084921 ) ) ;
#205921 = CIRCLE ( 'NONE', #57196, 2.350000000000000533 ) ;
#205922 = ORIENTED_EDGE ( 'NONE', *, *, #124338, .T. ) ;
#205923 = CARTESIAN_POINT ( 'NONE',  ( 9.511208455186636712, 11.05516360492796935, 1.199719254218453823 ) ) ;
#205924 = CARTESIAN_POINT ( 'NONE',  ( 4.441177836928239309, 7.339068688795062911, 1.199719254218452047 ) ) ;
#205925 = CARTESIAN_POINT ( 'NONE',  ( 4.336430608486574911, 1.111010274217393956, -1.430681851146862416 ) ) ;
#205926 = CARTESIAN_POINT ( 'NONE',  ( 6.604230223188150894, 9.758666789477915771, -1.082531754730548412 ) ) ;
#205927 = CARTESIAN_POINT ( 'NONE',  ( 5.096939404094710468, 4.911127157724081371, 0.000000000000000000 ) ) ;
#205928 = CARTESIAN_POINT ( 'NONE',  ( 5.891030527642284298, 5.977876296848656956, -0.06656325335930267373 ) ) ;
#205930 = CARTESIAN_POINT ( 'NONE',  ( -0.6823417656250039265, 14.81770833367473195, -1.181850606188755259 ) ) ;
#205929 = CARTESIAN_POINT ( 'NONE',  ( 4.914427440023315441, 0.7117315627661743305, 1.719784830429422984 ) ) ;
#205931 = CARTESIAN_POINT ( 'NONE',  ( 3.058105062934213692, -1.138753297271431375, 1.540237303602323804 ) ) ;
#205932 = CARTESIAN_POINT ( 'NONE',  ( 0.8678470384533981674, 0.8956018474440343713, 1.590720368640268001 ) ) ;
#205933 = PLANE ( 'NONE',  #118394 ) ;
#205934 = CARTESIAN_POINT ( 'NONE',  ( -11.97711842482174305, 7.451475930019106464, -0.9249707317075172019 ) ) ;
#205935 = MECHANICAL_DESIGN_GEOMETRIC_PRESENTATION_REPRESENTATION (  '', ( #178280 ), #202351 ) ;
#205936 = CARTESIAN_POINT ( 'NONE',  ( 5.582388601459258304, 7.396495182493852738, 1.242574333668546638 ) ) ;
#205937 = CARTESIAN_POINT ( 'NONE',  ( 6.204464077730128757, 7.037555732820855781, 1.030856974308017149 ) ) ;
#205938 = CARTESIAN_POINT ( 'NONE',  ( -10.99944587961302034, -9.906575223978485667, 0.1104109902703137719 ) ) ;
#205939 = CARTESIAN_POINT ( 'NONE',  ( 1.394453263437886604E-15, -2.668749999044085275, 3.474999999999999645 ) ) ;
#205940 = CARTESIAN_POINT ( 'NONE',  ( 7.958272981541723468, 8.386999354661243800, 1.040834085586084257E-14 ) ) ;
#205941 = CARTESIAN_POINT ( 'NONE',  ( 5.647300209178060193, 1.738727086691471024, -0.9248740175569410971 ) ) ;
#205942 = CARTESIAN_POINT ( 'NONE',  ( -5.101945877444165944, 4.846691699973280976, 0.000000000000000000 ) ) ;
#205943 = PRESENTATION_STYLE_ASSIGNMENT (( #87936 ) ) ;
#205944 = CARTESIAN_POINT ( 'NONE',  ( 1.130938551725582109, -1.889365942417848832, 0.8953178049561462126 ) ) ;
#205945 = CARTESIAN_POINT ( 'NONE',  ( 6.000991310419570901, 1.574649422783209740, -1.109465276731670613 ) ) ;
#205946 = CARTESIAN_POINT ( 'NONE',  ( -4.855791571988752331, 8.816840600628864877, 0.7998128361456481317 ) ) ;
#205947 = CARTESIAN_POINT ( 'NONE',  ( 2.115964440355810439, -0.8579360106165806465, -1.611413330227830176 ) ) ;
#205948 = CARTESIAN_POINT ( 'NONE',  ( 2.930518499080053907, 1.225513248159842083, -1.835134156090315605 ) ) ;
#205949 = CARTESIAN_POINT ( 'NONE',  ( 1.394453263437886604E-15, -1.618749999044085230, 3.474999999999999645 ) ) ;
#205950 = CARTESIAN_POINT ( 'NONE',  ( 1.019614524654769872, -0.4619345408787678964, 1.855657206939323789 ) ) ;
#205951 = CARTESIAN_POINT ( 'NONE',  ( 2.066797411385603578, 1.461431172244957333, -1.320572070109968799 ) ) ;
#205952 = CARTESIAN_POINT ( 'NONE',  ( 2.472129730261590552, -1.859182766463037151, -0.5613441811427360983 ) ) ;
#205953 = ORIENTED_EDGE ( 'NONE', *, *, #24366, .T. ) ;
#205954 = CARTESIAN_POINT ( 'NONE',  ( -0.3423093779010150106, 2.999999999999981792, -0.3423093779010167315 ) ) ;
#205956 = CARTESIAN_POINT ( 'NONE',  ( 6.350447304104193336, -1.851927549110881976, -0.1832485138882292142 ) ) ;
#205955 = CARTESIAN_POINT ( 'NONE',  ( -4.411198876399886615, 6.239761003923544713, -1.599625672291271394 ) ) ;
#205957 = CARTESIAN_POINT ( 'NONE',  ( 5.747730777550676073, 5.670383760089384495, 0.000000000000000000 ) ) ;
#205958 = DIRECTION ( 'NONE',  ( 0.9055141421511273547, -0.4243160830846600673, -2.465190328815662439E-32 ) ) ;
#205959 = CARTESIAN_POINT ( 'NONE',  ( 10.40996301719436090, 11.03937836301526687, 0.000000000000000000 ) ) ;
#205960 = CARTESIAN_POINT ( 'NONE',  ( -6.622231685632140596, 6.690634819517756959, 0.000000000000000000 ) ) ;
#205961 = CARTESIAN_POINT ( 'NONE',  ( 2.173600921376659834, 1.351110561487681716, 1.725424542402646422 ) ) ;
#205962 = CARTESIAN_POINT ( 'NONE',  ( 4.216222584169931231, 4.021273891060765493, 1.214306433183764966E-14 ) ) ;
#205963 = CARTESIAN_POINT ( 'NONE',  ( 6.038177310039780643, 8.137902509836795417, -1.599625672291283607 ) ) ;
#205964 = CARTESIAN_POINT ( 'NONE',  ( 0.000000000000000000, 2.499999999999998668, 0.000000000000000000 ) ) ;
#205965 = CARTESIAN_POINT ( 'NONE',  ( 2.789462663364688844, 1.291185895303394116, 1.290987730777813702 ) ) ;
#205966 = CARTESIAN_POINT ( 'NONE',  ( 5.327991180046136144, 5.318337252916436775, -0.7216878364870514817 ) ) ;
#205967 = CARTESIAN_POINT ( 'NONE',  ( -9.246297574839990929, 11.81043314211192019, 1.443375672974076540 ) ) ;
#205968 = CARTESIAN_POINT ( 'NONE',  ( -5.031572470839103417, 8.001347149079229837, -1.166850223539055875 ) ) ;
#205969 = DIRECTION ( 'NONE',  ( 1.000000000000000000, 0.000000000000000000, 0.000000000000000000 ) ) ;
#205970 = CARTESIAN_POINT ( 'NONE',  ( 9.101601193475611140, 9.512956235343358102, -0.7998128361456221525 ) ) ;
#205971 = CARTESIAN_POINT ( 'NONE',  ( 2.438006290551326671, 0.9082397578730906362, -1.698968261161729831 ) ) ;
#205972 = CARTESIAN_POINT ( 'NONE',  ( 6.244970037249994554, -0.2844439363869250559, -1.940879991452467479 ) ) ;
#205973 = CARTESIAN_POINT ( 'NONE',  ( -1.500000000000015099, 15.47916666666666430, -0.8660254037844309360 ) ) ;
#205974 = CARTESIAN_POINT ( 'NONE',  ( -7.711890448074853133, 7.891627032375787998, -0.7998128361456291469 ) ) ;
#205975 = CARTESIAN_POINT ( 'NONE',  ( 4.467575310902914154, 5.170924936596891008, 1.199719254218464037 ) ) ;
#205976 = CARTESIAN_POINT ( 'NONE',  ( -5.112833325684916552, 7.058334528089422300, -1.443375672974066548 ) ) ;
#205977 = CARTESIAN_POINT ( 'NONE',  ( 8.204655514564224816, 12.72384853363364066, 1.040834085586084257E-14 ) ) ;
#205978 = CARTESIAN_POINT ( 'NONE',  ( -1.493132593725482682, 4.435476081035520046, -0.1629718138060227417 ) ) ;
#205979 = CARTESIAN_POINT ( 'NONE',  ( 5.436411051413860385, -1.154718516627372127, 1.718110687276501958 ) ) ;
#205981 = CARTESIAN_POINT ( 'NONE',  ( -1.364683531250012516, 2.592708333674753174, 0.7879004041258379498 ) ) ;
#205980 = CARTESIAN_POINT ( 'NONE',  ( 0.8547319020580852467, 0.3593373433725781108, -1.805665335529122784 ) ) ;
#205982 = CARTESIAN_POINT ( 'NONE',  ( 5.449893634413335519, -2.076765696135183248, -0.9856196477224605790 ) ) ;
#205983 = CARTESIAN_POINT ( 'NONE',  ( 5.477130870240836558, 9.333810415348903433, -0.7216878364870267237 ) ) ;
#205985 = CARTESIAN_POINT ( 'NONE',  ( 1.224999999999971223, 1.354166666666710483, 0.7072540797572898219 ) ) ;
#205984 = CARTESIAN_POINT ( 'NONE',  ( 3.919715808126649659, 7.587102519540811940, 0.000000000000000000 ) ) ;
#205986 = CARTESIAN_POINT ( 'NONE',  ( 6.620655732516684822, -0.005281389526603020787, 2.273887028200880511 ) ) ;
#205987 = DIRECTION ( 'NONE',  ( 0.000000000000000000, 1.000000000000000000, 0.000000000000000000 ) ) ;
#205988 = CARTESIAN_POINT ( 'NONE',  ( -7.598418745816086783, 7.829519723065708092, 0.000000000000000000 ) ) ;
#205989 = CARTESIAN_POINT ( 'NONE',  ( 4.540924088961058480, -1.502189473471927439, -1.230693300551897185 ) ) ;
#205990 = EDGE_LOOP ( 'NONE', ( #95947, #161044 ) ) ;
#205991 = CARTESIAN_POINT ( 'NONE',  ( 8.066738210006674237, 11.39464976410773467, 1.082531754730558626 ) ) ;
#205992 = VERTEX_POINT ( 'NONE', #146895 ) ;
#205993 = CARTESIAN_POINT ( 'NONE',  ( 6.293217207623316156, -0.1008467329366956045, -1.909883259500498198 ) ) ;
#205994 = CARTESIAN_POINT ( 'NONE',  ( 0.8731895615166852531, 1.663438651979048277, -0.4559567554138827528 ) ) ;
#205995 = CARTESIAN_POINT ( 'NONE',  ( 5.436732529336289588, -1.586671906620169104, 1.244382051841623538 ) ) ;
#205997 = DIRECTION ( 'NONE',  ( 0.000000000000000000, 0.000000000000000000, 1.000000000000000000 ) ) ;
#205996 = CARTESIAN_POINT ( 'NONE',  ( -9.515124878692420296, 9.995400534762978850, 1.040834085586084257E-14 ) ) ;
#205998 = CARTESIAN_POINT ( 'NONE',  ( 1.642778471875001811, -1.480208332855375453, 2.845375778867859751 ) ) ;
#206000 = CARTESIAN_POINT ( 'NONE',  ( 1.357869778638900904, 0.7128107867309957379, 1.620144791207811297 ) ) ;
#205999 = CARTESIAN_POINT ( 'NONE',  ( 2.291069257668688408, 1.616616537889125516, 1.325633359429157831 ) ) ;
#206001 = LINE ( 'NONE', #71719, #57363 ) ;
#206003 = CARTESIAN_POINT ( 'NONE',  ( 4.576316751016760165, -2.222806176453680393, -0.5595744876762742681 ) ) ;
#206002 = CARTESIAN_POINT ( 'NONE',  ( 4.760848217054122422, 5.583353003765119560, -1.199719254218452047 ) ) ;
#206004 = CARTESIAN_POINT ( 'NONE',  ( 2.308218407481243961, 1.554217257889878301, 0.7831649204469055547 ) ) ;
#206005 = CARTESIAN_POINT ( 'NONE',  ( 3.330499290451326200, 7.037332938835193730, -0.7998128361456291469 ) ) ;
#206006 = CARTESIAN_POINT ( 'NONE',  ( 4.389807875774629942, 8.343469298370917997, 0.7998128361456271485 ) ) ;
#206007 = CARTESIAN_POINT ( 'NONE',  ( 2.424751807388926039, 0.7370815838836901612, 1.569499502796549262 ) ) ;
#206008 = CARTESIAN_POINT ( 'NONE',  ( -0.6801582343750368631, 2.130208333674714183, -1.178068619123862515 ) ) ;
#206009 = CARTESIAN_POINT ( 'NONE',  ( 1.433807476322545904, 1.104820645310525373, 1.497481488779895731 ) ) ;
#206010 = CARTESIAN_POINT ( 'NONE',  ( 2.559224761666531567, 1.745036862030847624, -1.291676481929154408 ) ) ;
#206011 = CARTESIAN_POINT ( 'NONE',  ( 6.322179702674084467, 6.270297829408224111, 1.040834085586084257E-14 ) ) ;
#206012 = CARTESIAN_POINT ( 'NONE',  ( 3.960172920142067898, -1.157100329752266621, 1.651342637023434090 ) ) ;
#206013 = CARTESIAN_POINT ( 'NONE',  ( 2.375000000000001776, 2.052068128417950277, -1.362642298365709419E-13 ) ) ;
#206014 = CARTESIAN_POINT ( 'NONE',  ( -1.500000000000013101, 2.410416667349482456, -0.8660254037844313801 ) ) ;
#206015 = CARTESIAN_POINT ( 'NONE',  ( 1.202032481184050816, -1.926566264184792709, -0.002868833312720530347 ) ) ;
#206016 = CARTESIAN_POINT ( 'NONE',  ( 1.364683531249996529, 13.71354166700806765, 0.7879004041258405033 ) ) ;
#206017 = CARTESIAN_POINT ( 'NONE',  ( 4.764059104694277735, 0.6956466834483631123, -2.109775416031458128 ) ) ;
#206018 = EDGE_LOOP ( 'NONE', ( #131518, #124612, #61506, #114626, #124147 ) ) ;
#206019 = FILL_AREA_STYLE ('',( #158363 ) ) ;
#206020 = CARTESIAN_POINT ( 'NONE',  ( 0.7499999999999867883, 0.3166666666666873020, -1.299038105676652899 ) ) ;
#206021 = CARTESIAN_POINT ( 'NONE',  ( 8.613507663383630941, 8.943513783569379427, -0.7998128361456221525 ) ) ;
#206022 = CARTESIAN_POINT ( 'NONE',  ( 0.6823417656249882723, -0.3239583329919110133, -1.181850606188749264 ) ) ;
#206023 = CARTESIAN_POINT ( 'NONE',  ( 6.152596803620836496, 2.197069216644991663, 0.3270334163130541594 ) ) ;
#206024 = CARTESIAN_POINT ( 'NONE',  ( 4.404711838702720428, 0.5211615849865286476, 1.891323523724611766 ) ) ;
#206025 = CARTESIAN_POINT ( 'NONE',  ( 10.23604278863759909, 11.04439746293979496, 0.000000000000000000 ) ) ;
#206026 = EDGE_CURVE ( 'NONE', #7711, #54188, #65577, .T. ) ;
#206027 = CARTESIAN_POINT ( 'NONE',  ( 1.836970198721030181E-16, 13.49999999999999822, 1.500000000000000222 ) ) ;
#206028 = CARTESIAN_POINT ( 'NONE',  ( 5.536487020692383076, 2.227601090660180638, 0.3946122451431322009 ) ) ;
#206029 = PRESENTATION_LAYER_ASSIGNMENT (  '', '', ( #195536 ) ) ;
#206030 = CARTESIAN_POINT ( 'NONE',  ( -6.183927461608886844, 7.347575139032721303, 1.082531754730548412 ) ) ;
#206031 = CARTESIAN_POINT ( 'NONE',  ( 3.490735631032083841, 2.011810643276640054, 0.4545708190045735786 ) ) ;
#206032 = CARTESIAN_POINT ( 'NONE',  ( -4.367698041896780126, 8.247398148854895084, 0.7998128361456481317 ) ) ;
#206033 =( BOUNDED_CURVE ( )  B_SPLINE_CURVE ( 2, ( #58161, #91756, #6181, #157809, #9407, #175130, #138357, #75478, #10460 ),
 .UNSPECIFIED., .F., .F. ) 
 B_SPLINE_CURVE_WITH_KNOTS ( ( 3, 2, 2, 2, 3 ),
 ( 0.7031250000000002220, 0.7083333333333333703, 0.7187500000000000000, 0.7291666666666666297, 0.7343749999999997780 ),
 .UNSPECIFIED. ) 
 CURVE ( )  GEOMETRIC_REPRESENTATION_ITEM ( )  RATIONAL_B_SPLINE_CURVE ( ( 0.9330127018922194093, 0.9330127018922221849, 1.000000000000000000, 0.8660254037844387076, 1.000000000000000000, 0.8660254037844387076, 1.000000000000000000, 0.9330127018922221849, 0.9330127018922194093 ) ) 
 REPRESENTATION_ITEM ( '' )  );
#206034 = AXIS2_PLACEMENT_3D ( 'NONE', #178642, #6774, #95274 ) ;
#206035 = CARTESIAN_POINT ( 'NONE',  ( -1.201851678989727383E-14, 3.118750000682814161, -1.732050807568863648 ) ) ;
#206036 = CARTESIAN_POINT ( 'NONE',  ( 0.6823417656249899377, 3.738541667008085767, -1.181850606188754593 ) ) ;
#206037 = CARTESIAN_POINT ( 'NONE',  ( 4.569519670753737550, 1.814867081516871261, -0.4525428206468632975 ) ) ;
#206038 = CARTESIAN_POINT ( 'NONE',  ( 3.568775204899740316, -0.8506723435033979319, 1.511049830170706931 ) ) ;
#206039 = CARTESIAN_POINT ( 'NONE',  ( 2.436699184107835592, -1.290689972581187339, -1.167790367532922646 ) ) ;
#206040 = CARTESIAN_POINT ( 'NONE',  ( 0.8906306365582180584, -0.5635816346751547634, -2.221901885516941899 ) ) ;
#206041 = CARTESIAN_POINT ( 'NONE',  ( 0.8860939741733677710, 1.483344945610004295, 1.634051305214024641 ) ) ;
#206042 = CARTESIAN_POINT ( 'NONE',  ( 4.265234282975380431, 2.027484720304991495, -0.5098422324811486828 ) ) ;
#206043 = CARTESIAN_POINT ( 'NONE',  ( 5.156170417566459108, -1.405356202774979524, 1.340433341176451520 ) ) ;
#206045 = EDGE_LOOP ( 'NONE', ( #80785, #38094, #145530, #61259, #92788 ) ) ;
#206044 = DIRECTION ( 'NONE',  ( 0.000000000000000000, 0.000000000000000000, -1.000000000000000000 ) ) ;
#206046 = CARTESIAN_POINT ( 'NONE',  ( 0.2642963535325442703, 1.880433764241522088, -0.7283817610406128074 ) ) ;
#206047 = CARTESIAN_POINT ( 'NONE',  ( -0.1577409392781377873, -1.310076727147227560, -1.668215054097483385 ) ) ;
#206048 = FACE_OUTER_BOUND ( 'NONE', #92398, .T. ) ;
#206049 = FACE_OUTER_BOUND ( 'NONE', #95349, .T. ) ;
#206050 = CARTESIAN_POINT ( 'NONE',  ( -7.828943636887387925, 11.22118577875556156, 1.199719254218453823 ) ) ;
#206051 = CARTESIAN_POINT ( 'NONE',  ( 6.446011968293428041, 9.607765498729298415, -1.199719254218440723 ) ) ;
#206052 = CARTESIAN_POINT ( 'NONE',  ( 4.055160972438559774, -1.518969423100406946, -1.012540670841777013 ) ) ;
#206053 = CARTESIAN_POINT ( 'NONE',  ( 2.257103711190447282, -1.706036888594957723, 1.399758388914617013 ) ) ;
#206054 = ORIENTED_EDGE ( 'NONE', *, *, #211770, .F. ) ;
#206055 = CARTESIAN_POINT ( 'NONE',  ( -5.126391479298592735, 5.153413945369351268, 0.000000000000000000 ) ) ;
#206056 = CARTESIAN_POINT ( 'NONE',  ( -0.3909723190920246227, -8.176244038172828965, -9.516020521606723293 ) ) ;
#206057 = CARTESIAN_POINT ( 'NONE',  ( 3.285556943750000514, -2.151041666188709733, 1.896917185911906500 ) ) ;
#206058 = CARTESIAN_POINT ( 'NONE',  ( -7.263417608619167076, 9.497073181520933716, -1.599625672291263179 ) ) ;
#206059 = CARTESIAN_POINT ( 'NONE',  ( 1.687766420876281037, 1.931502627210328837, -0.5905180581586618738 ) ) ;
#206060 = CARTESIAN_POINT ( 'NONE',  ( -5.496904935697871863, 5.377753611261092637, 0.7998128361456281477 ) ) ;
#206061 = CARTESIAN_POINT ( 'NONE',  ( 2.852234624111050110, -1.855622028292166714, -0.1419291048156411938 ) ) ;
#206062 = CARTESIAN_POINT ( 'NONE',  ( 2.191614386903386613, 5.708633884695917260, -0.7998128361456281477 ) ) ;
#206063 = CARTESIAN_POINT ( 'NONE',  ( 1.843739406749204335, 8.920000000000001705, 0.7750000000000004663 ) ) ;
#206064 = EDGE_LOOP ( 'NONE', ( #152002, #39429, #61575, #192476 ) ) ;
#206065 = CARTESIAN_POINT ( 'NONE',  ( -3.741160322367112379, 6.452105245148518797, 1.199719254218464037 ) ) ;
#206066 = CARTESIAN_POINT ( 'NONE',  ( -7.472515219426274946, 11.86968485597268064, 0.000000000000000000 ) ) ;
#206067 = CARTESIAN_POINT ( 'NONE',  ( 5.619710272201024814, -1.780234218580947436, 0.4041525643716862848 ) ) ;
#206068 = VECTOR ( 'NONE', #30646, 1000.000000000000114 ) ;
#206070 = CARTESIAN_POINT ( 'NONE',  ( -4.613696345000219523, 7.131516869168907924, -1.371494837298018243 ) ) ;
#206069 = CARTESIAN_POINT ( 'NONE',  ( -8.072954122294394352, 8.383144328957069291, -0.7998128361456362523 ) ) ;
#206071 = CARTESIAN_POINT ( 'NONE',  ( 6.587573780899039555, 6.778200402807202707, -0.2451836268814889253 ) ) ;
#206072 = CARTESIAN_POINT ( 'NONE',  ( 0.3855818064394588851, -0.09363725165581829324, 1.731465614217362559 ) ) ;
#206073 = CARTESIAN_POINT ( 'NONE',  ( 6.615202361034350886, -1.784545987531281019, 0.4526050685512914007 ) ) ;
#206074 = CARTESIAN_POINT ( 'NONE',  ( 4.899205829341429563, 1.920759858200033587, -1.278847778945918279 ) ) ;
#206075 = CARTESIAN_POINT ( 'NONE',  ( 4.692003678781083487, 7.631698837623355658, -1.199719254218450271 ) ) ;
#206076 = CARTESIAN_POINT ( 'NONE',  ( 6.766866382711775429, -1.973269837180600561, -0.8828958408187634888 ) ) ;
#206077 = CARTESIAN_POINT ( 'NONE',  ( 5.632522751473472589, 8.658694745772667289, -1.199719254218440723 ) ) ;
#206078 = CARTESIAN_POINT ( 'NONE',  ( 5.782642724008081103, -2.244312133422786015, 0.4951331349164668216 ) ) ;
#206079 = FACE_OUTER_BOUND ( 'NONE', #154756, .T. ) ;
#206080 = CARTESIAN_POINT ( 'NONE',  ( -6.261886844665283114, 8.398896966899865646, 1.599625672291269396 ) ) ;
#206081 = CARTESIAN_POINT ( 'NONE',  ( 5.981297838379462384, 1.727768277425823396, -0.7175292643646775659 ) ) ;
#206082 = VECTOR ( 'NONE', #171038, 1000.000000000000000 ) ;
#206084 = CARTESIAN_POINT ( 'NONE',  ( -3.984117037569407938, 5.741498858621315371, 1.599625672291270506 ) ) ;
#206083 = CARTESIAN_POINT ( 'NONE',  ( 4.025576834063953946, -0.3218090080209669024, 1.884953445776993863 ) ) ;
#206085 = CARTESIAN_POINT ( 'NONE',  ( 4.776106669258010307, 1.268914099295117781, 1.805409367619143390 ) ) ;
#206086 = CARTESIAN_POINT ( 'NONE',  ( 4.909417703775454278, -2.009542366629351484, 0.6670832617777838758 ) ) ;
#206087 = CARTESIAN_POINT ( 'NONE',  ( 1.224999999999984768, 0.1875000006827803878, -5.377642775528101993E-14 ) ) ;
#206088 = CARTESIAN_POINT ( 'NONE',  ( -9.860732380151581822, 3.579270011397724272, 6.765084847522528477 ) ) ;
#206089 = CARTESIAN_POINT ( 'NONE',  ( 4.543390873910903238, 7.354354215321133204, 1.082531754730548412 ) ) ;
#206090 = TOROIDAL_SURFACE ( 'NONE', #112788, 2.600000000000000089, 0.1000000000000000056 ) ;
#206091 = CARTESIAN_POINT ( 'NONE',  ( -4.895902867866254837, 7.765618208269001066, 1.082531754730549967 ) ) ;
#206092 = CARTESIAN_POINT ( 'NONE',  ( 2.837322237161111094, 0.2816050128923338058, 2.290267077920715710 ) ) ;
#206094 = EDGE_CURVE ( 'NONE', #93282, #67678, #106819, .T. ) ;
#206093 = CARTESIAN_POINT ( 'NONE',  ( 3.982823771651412770, 1.862158852298421152, 0.6176278068941787325 ) ) ;
#206095 = CARTESIAN_POINT ( 'NONE',  ( -4.878955176071358757, 6.785476686873604280, -1.599625672291271394 ) ) ;
#206096 = CARTESIAN_POINT ( 'NONE',  ( 6.807491137956053429, -1.653082740107037152, -1.233284719700310506 ) ) ;
#206097 = CARTESIAN_POINT ( 'NONE',  ( 2.901081683644319842, 5.368050483351580304, 1.082531754730548412 ) ) ;
#206098 = CARTESIAN_POINT ( 'NONE',  ( 5.063044020060520900, 4.871582543017558109, 0.7998128361456352531 ) ) ;
#206099 = ORIENTED_EDGE ( 'NONE', *, *, #61570, .F. ) ;
#206100 = CARTESIAN_POINT ( 'NONE',  ( 5.278529876733943915, -0.4946281652532491524, -1.954780475499573900 ) ) ;
#206101 = CARTESIAN_POINT ( 'NONE',  ( -8.350932551013499960, 11.83017284523606172, -1.199719254218446718 ) ) ;
#206102 =( NAMED_UNIT ( * ) PLANE_ANGLE_UNIT ( ) SI_UNIT ( $, .RADIAN. ) );
#206103 = CARTESIAN_POINT ( 'NONE',  ( -10.99931038725301846, 6.873658557531565627, -3.960823121322395224 ) ) ;
#206104 = CARTESIAN_POINT ( 'NONE',  ( 1.569424903267138571, 1.913428125876670549, 1.025899993198212901 ) ) ;
#206105 = CARTESIAN_POINT ( 'NONE',  ( -10.12374542407608402, 0.2401923788623722134, 4.551898349974277558 ) ) ;
#206106 = B_SPLINE_CURVE_WITH_KNOTS ( 'NONE', 3,
 ( #205838, #57471, #123631, #189594, #201555, #44433, #178691, #125749 ),
 .UNSPECIFIED., .F., .F.,
 ( 4, 2, 2, 4 ),
 ( 0.000000000000000000, 0.0003954713701971531467, 0.0005932070552957296929, 0.0007909427403943062934 ),
 .UNSPECIFIED. ) ;
#206107 = CARTESIAN_POINT ( 'NONE',  ( 1.499999999999987121, 0.07708333401615156955, -0.8660254037844323793 ) ) ;
#206108 = CARTESIAN_POINT ( 'NONE',  ( 4.121519629048689001E-15, 14.55305236562702831, -11.95586206896554771 ) ) ;
#206109 = CARTESIAN_POINT ( 'NONE',  ( 10.85353573482951717, -6.836568542495036205, -0.4635785636673637189 ) ) ;
#206110 = CARTESIAN_POINT ( 'NONE',  ( 5.420206975164616026, 7.644856803259713729, 1.330009527941821368 ) ) ;
#206111 = CARTESIAN_POINT ( 'NONE',  ( 1.405620310220422109, -0.5036079032930698141, 1.998149085168912986 ) ) ;
#206113 = CARTESIAN_POINT ( 'NONE',  ( -2.460826785407679740, 8.202405370174460586, -2.499999999999995115 ) ) ;
#206112 = CARTESIAN_POINT ( 'NONE',  ( -0.02224634325202062834, 1.297472808610355521, -2.537530276547406149 ) ) ;
#206114 = CARTESIAN_POINT ( 'NONE',  ( 1.364683531249986537, 0.1552083336747499542, -0.7879004041258309554 ) ) ;
#206115 = CARTESIAN_POINT ( 'NONE',  ( -1.500095892183268109, 3.249791167484341159, 0.08036760724049506199 ) ) ;
#206116 = EDGE_CURVE ( 'NONE', #154752, #110280, #63436, .T. ) ;
#206117 = ORIENTED_EDGE ( 'NONE', *, *, #48694, .F. ) ;
#206118 = CARTESIAN_POINT ( 'NONE',  ( 3.686107007616833631, 1.064666855108999721, 1.588282736317746302 ) ) ;
#206119 =( BOUNDED_SURFACE ( )  B_SPLINE_SURFACE ( 3, 2, ( 
 ( #75925, #43447, #59670 ),
 ( #14092, #44512, #46637 ),
 ( #160376, #76978, #45577 ),
 ( #80182, #29311, #211236 ),
 ( #61808, #28241, #209097 ),
 ( #62862, #127978, #146287 ),
 ( #193930, #11978, #110629 ),
 ( #111693, #130087, #176630 ) ),
 .UNSPECIFIED., .F., .F., .T. ) 
 B_SPLINE_SURFACE_WITH_KNOTS ( ( 4, 2, 2, 4 ),
 ( 3, 3 ),
 ( 0.000000000000000000, 0.0002568729646053923097, 0.0005137459292107846194, 0.001027491858421569239 ),
 ( 0.000000000000000000, 1.000000000000000000 ),
 .UNSPECIFIED. ) 
 GEOMETRIC_REPRESENTATION_ITEM ( )  RATIONAL_B_SPLINE_SURFACE ( (
 ( 1.000000000000000000, 0.3826834323651031600, 1.000000000000000000),
 ( 1.000000000000000000, 0.3847114443838287601, 1.000000000000000000),
 ( 1.000000000000000000, 0.4039255759070156659, 1.000000000000000000),
 ( 1.000000000000000000, 0.4557194474500481651, 1.000000000000000000),
 ( 1.000000000000000000, 0.4874388927525016291, 1.000000000000000000),
 ( 1.000000000000000000, 0.5833547384513821932, 1.000000000000000000),
 ( 1.000000000000000000, 0.6470545345839008311, 1.000000000000000000),
 ( 1.000000000000000000, 0.7045118851637607316, 1.000000000000000000) ) ) 
 REPRESENTATION_ITEM ( '' )  SURFACE ( )  );
#206120 = CARTESIAN_POINT ( 'NONE',  ( 5.119873625132255412, -0.9486883152997215296, -1.493885749217472636 ) ) ;
#206121 = CARTESIAN_POINT ( 'NONE',  ( 5.631432701629774051, 7.663367133358481631, 1.599625672291269396 ) ) ;
#206122 = CARTESIAN_POINT ( 'NONE',  ( -5.115504031057831469, 4.862509545855891346, 0.7998128361456341429 ) ) ;
#206124 = CARTESIAN_POINT ( 'NONE',  ( 0.2685667436414033160, -0.2372314691254543417, -1.900927335933370488 ) ) ;
#206123 = CARTESIAN_POINT ( 'NONE',  ( -0.2123833161804513925, 7.036763569728186951, -3.929715952998865891 ) ) ;
#206125 = CARTESIAN_POINT ( 'NONE',  ( -1.402160292154681736E-14, 0.08750000000001964540, -1.732050807568870754 ) ) ;
#206126 = CARTESIAN_POINT ( 'NONE',  ( 0.4146172280090759665, 0.7909515328246279342, 1.913518691844050323 ) ) ;
#206127 = CARTESIAN_POINT ( 'NONE',  ( 1.364683531249986537, -0.8239583329919186738, 0.7879004041258500513 ) ) ;
#206128 = CARTESIAN_POINT ( 'NONE',  ( 6.350466393003619814, 0.5888352225367661230, 1.775644890098279749 ) ) ;
#206129 = CARTESIAN_POINT ( 'NONE',  ( 2.683998146737070378, -0.9385614705539682134, 1.565816405032012470 ) ) ;
#206131 = CARTESIAN_POINT ( 'NONE',  ( 6.453003701063230402, 6.772902045581084884, 0.3391303328579304277 ) ) ;
#206130 = CARTESIAN_POINT ( 'NONE',  ( 5.953802724510455668, 0.6443607167232848765, -2.110727517106169682 ) ) ;
#206132 = CARTESIAN_POINT ( 'NONE',  ( 1.364683531249988757, 0.8843750003414210248, 0.000000000000000000 ) ) ;
#206133 = CARTESIAN_POINT ( 'NONE',  ( 2.928243574330684496, 1.101304876339922467, 1.743887257993762763 ) ) ;
#206134 = CARTESIAN_POINT ( 'NONE',  ( -6.795661308947694934, 8.951357498570873261, -1.599625672291263179 ) ) ;
#206135 = CARTESIAN_POINT ( 'NONE',  ( 9.053093885623066939, 11.58502883802551153, -1.599625672291262513 ) ) ;
#206136 = CARTESIAN_POINT ( 'NONE',  ( 4.599240423533799138, 6.388866465587985211, 1.599625672291267175 ) ) ;
#206137 = CARTESIAN_POINT ( 'NONE',  ( 0.7026770610618976454, -0.7276074859871292100, -2.035605373553108777 ) ) ;
#206138 = CARTESIAN_POINT ( 'NONE',  ( 5.283670394142272464, -1.967056725255760474, 0.6460906113585006549 ) ) ;
#206139 = CARTESIAN_POINT ( 'NONE',  ( -0.6823417656250003738, 0.03020833367475134201, -1.181850606188749264 ) ) ;
#206140 = CARTESIAN_POINT ( 'NONE',  ( 3.673254355229157664, 0.05708692194854488033, -2.161017345153878999 ) ) ;
#206141 = CARTESIAN_POINT ( 'NONE',  ( -4.721755537811513470, 8.238515690766082145, -0.6557258408305451924 ) ) ;
#206144 = ADVANCED_FACE ( 'NONE', ( #117622 ), #17892, .T. ) ;
#206143 = CARTESIAN_POINT ( 'NONE',  ( 2.295295855072278624, -1.753792786583353580, 0.8793850528211948347 ) ) ;
#206142 = CARTESIAN_POINT ( 'NONE',  ( 4.459631813825579272, -1.562525726068206833, -1.279702784981617825 ) ) ;
#206145 = PRODUCT_DEFINITION_SHAPE ( 'NONE', 'NONE',  #141784 ) ;
#206146 = EDGE_CURVE ( 'NONE', #198869, #178392, #170560, .T. ) ;
#206149 = CARTESIAN_POINT ( 'NONE',  ( 5.992340707560151358, 8.014150130285418783, 1.443375672974062551 ) ) ;
#206148 = CARTESIAN_POINT ( 'NONE',  ( -1.737499999999997824, -0.2916666666666657415, 3.009438278150925683 ) ) ;
#206147 = CARTESIAN_POINT ( 'NONE',  ( -0.3282377607281303233, 1.551335450315375786, 1.224999999999979217 ) ) ;
#206150 = CARTESIAN_POINT ( 'NONE',  ( -5.447343857640614573, 9.577261277214532242, -0.7998128361456362523 ) ) ;
#206151 = CARTESIAN_POINT ( 'NONE',  ( 1.921111612355221654, -1.799121770747251547, 0.9110121207814986244 ) ) ;
#206152 = B_SPLINE_CURVE_WITH_KNOTS ( 'NONE', 3,
 ( #206516, #46183, #190265, #157797 ),
 .UNSPECIFIED., .F., .F.,
 ( 4, 4 ),
 ( 0.000000000000000000, 6.033646489354576486E-05 ),
 .UNSPECIFIED. ) ;
#206154 = CARTESIAN_POINT ( 'NONE',  ( 2.000000000000012434, 0.09816220177719153783, 0.5999999999999995337 ) ) ;
#206153 = CARTESIAN_POINT ( 'NONE',  ( -5.928993247877788697, 5.811580298812519807, 0.7998128361456341429 ) ) ;
#206155 = CARTESIAN_POINT ( 'NONE',  ( 5.801015586618943232, -0.2871438832755985882, -1.890612906794430614 ) ) ;
#206156 = DIRECTION ( 'NONE',  ( -1.000000000000000000, 0.000000000000000000, 0.000000000000000000 ) ) ;
#206157 = CARTESIAN_POINT ( 'NONE',  ( 4.148431815657221300, 7.783661518334664464, 1.040834085586084257E-14 ) ) ;
#206159 = CARTESIAN_POINT ( 'NONE',  ( 3.128529964930275131, 0.4926631579876327716, 1.955168413974050834 ) ) ;
#206158 = CARTESIAN_POINT ( 'NONE',  ( -7.822691444960709006, 10.14955932391940330, -1.443375672974058777 ) ) ;
#206160 = CARTESIAN_POINT ( 'NONE',  ( -1.201851678989727383E-14, 3.587500000000020339, -1.732050807568863648 ) ) ;
#206161 = CARTESIAN_POINT ( 'NONE',  ( -1.364683531250000748, 14.42187500034139447, 0.000000000000000000 ) ) ;
#206162 = CARTESIAN_POINT ( 'NONE',  ( 5.895441327320324554, 1.309037806329484521, 1.123130245766153612 ) ) ;
#206163 = CARTESIAN_POINT ( 'NONE',  ( 6.230854113932139171, 9.427024345299638952, 1.199719254218452047 ) ) ;
#206164 = CARTESIAN_POINT ( 'NONE',  ( 8.432808358020015049, 11.82173160345663376, 1.082531754730546636 ) ) ;
#206165 = CARTESIAN_POINT ( 'NONE',  ( -0.4000000000000214495, 3.322650755865464767, 0.5865692111442306622 ) ) ;
#206166 = CARTESIAN_POINT ( 'NONE',  ( 4.727732462671866642, -1.149354582003499159, -1.475719300151681512 ) ) ;
#206167 = CARTESIAN_POINT ( 'NONE',  ( 1.692325190600419305, 1.023896122633965566, -1.799289093316607469 ) ) ;
#206168 = CARTESIAN_POINT ( 'NONE',  ( -6.522881301506166629, 9.663759714182251770, 1.082531754730549967 ) ) ;
#206169 = ORIENTED_EDGE ( 'NONE', *, *, #192402, .F. ) ;
#206170 = CARTESIAN_POINT ( 'NONE',  ( 4.065465959251388206, 5.836405933916976707, -1.599625672291269396 ) ) ;
#206171 = CARTESIAN_POINT ( 'NONE',  ( 1.734723475976807094E-15, 1.000000000000000888, 0.000000000000000000 ) ) ;
#206172 = CARTESIAN_POINT ( 'NONE',  ( 0.4920785707626255112, -1.005892833030905598, 1.506422592618541278 ) ) ;
#206173 = CARTESIAN_POINT ( 'NONE',  ( 5.194182247366878613, 6.192872389083746043, 1.082531754730549078 ) ) ;
#206174 = CARTESIAN_POINT ( 'NONE',  ( 5.602074566136501232, 5.729665287594564838, 0.6253354971682704155 ) ) ;
#206175 = ORIENTED_EDGE ( 'NONE', *, *, #169774, .T. ) ;
#206176 = CARTESIAN_POINT ( 'NONE',  ( 8.554831740098659765, 10.04335378727902395, 1.082531754730558626 ) ) ;
#206177 = AXIS2_PLACEMENT_3D ( 'NONE', #100046, #149874, #69648 ) ;
#206178 = CARTESIAN_POINT ( 'NONE',  ( 6.903072767652295383, 11.20533532890304684, 1.040834085586084257E-14 ) ) ;
#206179 = CARTESIAN_POINT ( 'NONE',  ( 5.659766488261158024, 1.145116341927857384, 1.535488998638125047 ) ) ;
#206180 = CARTESIAN_POINT ( 'NONE',  ( -11.55950211276791073, 13.79999999999998472, 3.221476510067111665 ) ) ;
#206181 = DIRECTION ( 'NONE',  ( -0.9632918427306595976, 0.000000000000000000, -0.2684563758389253985 ) ) ;
#206182 =( LENGTH_UNIT ( ) NAMED_UNIT ( * ) SI_UNIT ( .MILLI., .METRE. ) );
#206184 = ORIENTED_EDGE ( 'NONE', *, *, #8819, .T. ) ;
#206183 = CARTESIAN_POINT ( 'NONE',  ( 4.744990575102895569, 5.598539094783909320, -1.082531754730548412 ) ) ;
#206185 = CARTESIAN_POINT ( 'NONE',  ( -8.107412671292051343, 10.48173408797264194, 1.443375672974090751 ) ) ;
#206186 = CARTESIAN_POINT ( 'NONE',  ( 2.835029207381420502, 0.2633842809251253358, 2.145520918749081574 ) ) ;
#206187 = CARTESIAN_POINT ( 'NONE',  ( -7.621091744657483069, 8.063897588288083895, 0.7216878364870317197 ) ) ;
#206188 = CARTESIAN_POINT ( 'NONE',  ( 6.455090533882185788, 8.624301270986276080, -1.443375672974078761 ) ) ;
#206189 = CARTESIAN_POINT ( 'NONE',  ( -2.428882075142555497, 5.985446187641602300, 1.040834085586084257E-14 ) ) ;
#206190 = CARTESIAN_POINT ( 'NONE',  ( 6.176747059734422507, -1.734417727105644680, -0.5698399933231483860 ) ) ;
#206191 = CARTESIAN_POINT ( 'NONE',  ( 11.74191529183257821, 6.810689793464089981, -0.9382034048196972176 ) ) ;
#206192 = CARTESIAN_POINT ( 'NONE',  ( 0.6671782056521896598, 0.1977593025605048904, -1.961437444221861837 ) ) ;
#206193 = CARTESIAN_POINT ( 'NONE',  ( 3.586107075002854305, 1.066394011600999780, 1.587261316105821551 ) ) ;
#206194 = ORIENTED_EDGE ( 'NONE', *, *, #4984, .T. ) ;
#206195 = CARTESIAN_POINT ( 'NONE',  ( -6.755832246681736208, 14.48046842831809577, -9.927744205739022831 ) ) ;
#206196 = CARTESIAN_POINT ( 'NONE',  ( 4.984792273111487759, 1.884092017856910273, 0.5737924883163454393 ) ) ;
#206197 = ORIENTED_EDGE ( 'NONE', *, *, #73178, .F. ) ;
#206198 = CARTESIAN_POINT ( 'NONE',  ( 0.1990292396216531146, -0.5187523925454742280, 1.871322268447791703 ) ) ;
#206199 = VERTEX_POINT ( 'NONE', #3761 ) ;
#206200 = CARTESIAN_POINT ( 'NONE',  ( -6.134138155540168391, 6.121192367743780949, 0.000000000000000000 ) ) ;
#206202 = CARTESIAN_POINT ( 'NONE',  ( 6.981856502304780498, -6.709867743870614021, -6.429544252030573226 ) ) ;
#206201 = CARTESIAN_POINT ( 'NONE',  ( -4.773352600463090845, 7.726605912919016106, 1.199719254218452935 ) ) ;
#206203 = CARTESIAN_POINT ( 'NONE',  ( 5.844973620822823790, 9.833236634353070826, 0.7216878364870317197 ) ) ;
#206205 = ORIENTED_EDGE ( 'NONE', *, *, #96785, .F. ) ;
#206204 = CARTESIAN_POINT ( 'NONE',  ( 3.510326737904199135, -1.910220267131033323, -0.09114558060911714943 ) ) ;
#206206 = CARTESIAN_POINT ( 'NONE',  ( 1.097021799178355739, -0.5375665728563281398, -2.140183485690804410 ) ) ;
#206207 = CARTESIAN_POINT ( 'NONE',  ( 7.694877102302470462, -5.389939693150867406, 7.860745937262088923 ) ) ;
#206208 = CARTESIAN_POINT ( 'NONE',  ( 6.182294962360654900, 1.036951722903585837, 1.725357817989848996 ) ) ;
#206209 = FACE_OUTER_BOUND ( 'NONE', #60735, .T. ) ;
#206210 = CARTESIAN_POINT ( 'NONE',  ( 6.709597972018079837, -0.3944863986210072060, 1.789098616620278470 ) ) ;
#206211 = CARTESIAN_POINT ( 'NONE',  ( -1.500000000000001332, 2.244000000000016648, -2.508000000000002228 ) ) ;
#206212 = CARTESIAN_POINT ( 'NONE',  ( 1.697802635435996743, -1.498143435978617655, -1.429203828351800487 ) ) ;
#206213 = CARTESIAN_POINT ( 'NONE',  ( -5.738125327081750271, 7.717565519727259904, 1.599625672291269396 ) ) ;
#206214 = MECHANICAL_DESIGN_GEOMETRIC_PRESENTATION_REPRESENTATION (  '', ( #188901 ), #102484 ) ;
#206215 = CARTESIAN_POINT ( 'NONE',  ( -5.250728612101474901, 7.694385777474874288, -1.211319784145984846 ) ) ;
#206216 = FACE_BOUND ( 'NONE', #10872, .T. ) ;
#206217 = CARTESIAN_POINT ( 'NONE',  ( 4.286349120214771879, 8.152491073559232859, -0.7998128361456221525 ) ) ;
#206218 = FILL_AREA_STYLE ('',( #74104 ) ) ;
#206219 = CARTESIAN_POINT ( 'NONE',  ( 3.418064124421011041, 7.001842221884225559, -0.7216878364870338292 ) ) ;
#206220 = CARTESIAN_POINT ( 'NONE',  ( 0.003376046620569739427, -7.161464053357565973, 9.586610838029432813 ) ) ;
#206221 = AXIS2_PLACEMENT_3D ( 'NONE', #202260, #22445, #90698 ) ;
#206222 = CARTESIAN_POINT ( 'NONE',  ( -7.664830294503444996, -9.999999999999994671, 7.777967379493320621 ) ) ;
#206223 = CARTESIAN_POINT ( 'NONE',  ( -8.012344526598182026E-15, 11.60937500034140157, -1.575800808251669460 ) ) ;
#206225 = CARTESIAN_POINT ( 'NONE',  ( -5.498713818794216834, 8.572860667638675380, -1.199719254218452047 ) ) ;
#206224 = CARTESIAN_POINT ( 'NONE',  ( 6.825078400183556937, 1.282741234726336943, 1.971047034039685952 ) ) ;
#206226 = CARTESIAN_POINT ( 'NONE',  ( 5.326719796100753967, 0.6952390240965979906, -1.588890972402807966 ) ) ;
#206227 = CARTESIAN_POINT ( 'NONE',  ( -3.578462479003122976, 6.262291094557191684, 1.199719254218464037 ) ) ;
#206228 = CARTESIAN_POINT ( 'NONE',  ( 1.991162705694597301, 0.1987741427678466066, 2.060657922996151914 ) ) ;
#206229 = CARTESIAN_POINT ( 'NONE',  ( 3.550509549652399066, -1.420143166946661317, 1.570484981737807706 ) ) ;
#206230 = CARTESIAN_POINT ( 'NONE',  ( 6.154511665599609493, 9.267681812253174556, 1.199719254218462483 ) ) ;
#206231 = CARTESIAN_POINT ( 'NONE',  ( 0.000000000000000000, 9.799999999999998934, 0.000000000000000000 ) ) ;
#206232 = CARTESIAN_POINT ( 'NONE',  ( 1.938274800925225527, -1.057869798513750847, 1.661026717510836637 ) ) ;
#206233 = CARTESIAN_POINT ( 'NONE',  ( 5.684994455280509840, 6.294486374732538359, 1.096603583888225764 ) ) ;
#206235 = CARTESIAN_POINT ( 'NONE',  ( 0.1055216070770526038, 1.418477292093557329, 1.282857148695019989 ) ) ;
#206234 = CARTESIAN_POINT ( 'NONE',  ( -1.737500000000000266, -1.108333333333332726, -3.009438278150923907 ) ) ;
#206236 = CARTESIAN_POINT ( 'NONE',  ( 4.119262515598776098, -2.194098707595509623, 0.6636001952689452033 ) ) ;
#206237 = CARTESIAN_POINT ( 'NONE',  ( 1.418276456094772708, 1.227529518603141190, -1.351586893430449576 ) ) ;
#206238 = CIRCLE ( 'NONE', #168222, 0.1399999999999995137 ) ;
#206239 = CARTESIAN_POINT ( 'NONE',  ( 4.908934136599710563, 7.884784371745123366, 1.199719254218451159 ) ) ;
#206240 = CARTESIAN_POINT ( 'NONE',  ( 5.111060722227499298, 8.906728576000002562, -0.7216878364870267237 ) ) ;
#206241 = CARTESIAN_POINT ( 'NONE',  ( -7.374745490829552885, 10.69128794168811680, -1.199719254218446718 ) ) ;
#206242 = ADVANCED_FACE ( 'NONE', ( #152193 ), #9966, .T. ) ;
#206243 = CARTESIAN_POINT ( 'NONE',  ( 2.426041559740747200, -1.990683941386611311, 0.2996653706425453367 ) ) ;
#206244 = CARTESIAN_POINT ( 'NONE',  ( 2.799599750139214471, -1.450362073461785473, -1.321114446766240347 ) ) ;
#206245 = CARTESIAN_POINT ( 'NONE',  ( -8.857554428429624593, 9.228235009456373206, 0.7998128361456462443 ) ) ;
#206246 = CARTESIAN_POINT ( 'NONE',  ( -7.063961727919978451, 8.200042423116789436, 1.199719254218450271 ) ) ;
#206247 = CARTESIAN_POINT ( 'NONE',  ( -15.75000000000000000, 10.90000000000000036, 1.099999999999996758 ) ) ;
#206249 = CARTESIAN_POINT ( 'NONE',  ( 4.785902253289605390, -0.8326956132961546020, 1.561725933240491360 ) ) ;
#206248 = CARTESIAN_POINT ( 'NONE',  ( 6.246049398119083662, 0.6547385654485110562, 1.985528007121174943 ) ) ;
#206250 = CARTESIAN_POINT ( 'NONE',  ( 3.486133158594716510E-16, 2.312499999999992006, 1.224999999999971889 ) ) ;
#206251 = CARTESIAN_POINT ( 'NONE',  ( 1.306853331985533107, 1.934050699793531836, 1.030479497498619557 ) ) ;
#206252 = CARTESIAN_POINT ( 'NONE',  ( 5.718645868333249283, -0.03627580822302550745, 1.740135244698801431 ) ) ;
#206253 = EDGE_CURVE ( 'NONE', #54971, #117563, #70621, .T. ) ;
#206254 = CARTESIAN_POINT ( 'NONE',  ( 9.088043039861931405, 9.497138389460751284, 1.040834085586084257E-14 ) ) ;
#206255 = CARTESIAN_POINT ( 'NONE',  ( 0.2331713839410966271, 5.723577825403736163, -2.547423061495857954 ) ) ;
#206256 = CARTESIAN_POINT ( 'NONE',  ( 6.574781987728091970, -0.9847942639734930115, 2.074158207377621910 ) ) ;
#206257 = CARTESIAN_POINT ( 'NONE',  ( 1.394453263437886604E-15, -1.268749999044084253, 3.474999999999999645 ) ) ;
#206258 = CARTESIAN_POINT ( 'NONE',  ( 6.028594920762765597, 1.707543762964639722, -0.2996114793598329551 ) ) ;
#206259 = CARTESIAN_POINT ( 'NONE',  ( 5.318865801915546143, -1.576246948875639209, 1.493384065191505350 ) ) ;
#206260 = CARTESIAN_POINT ( 'NONE',  ( -5.558479791478509568, 5.587240632920778438, 0.000000000000000000 ) ) ;
#206261 = CARTESIAN_POINT ( 'NONE',  ( 6.473846665049121540, -0.8576149079453172508, 1.823233050095712349 ) ) ;
#206262 = CARTESIAN_POINT ( 'NONE',  ( 3.000000000000002665, -1.776620610948833047E-13, -2.052068128417948945 ) ) ;
#206263 = DIRECTION ( 'NONE',  ( -0.000000000000000000, -0.000000000000000000, -1.000000000000000000 ) ) ;
#206264 = CARTESIAN_POINT ( 'NONE',  ( 3.979452554116496898, 1.814262220864255815, -0.6480193189529972475 ) ) ;
#206265 = CARTESIAN_POINT ( 'NONE',  ( -6.009258394948636914E-15, 11.71875000068279604, -1.732050807568875195 ) ) ;
#206266 = CARTESIAN_POINT ( 'NONE',  ( 1.454100989278300560, -1.612054358864203785, -1.528463602881096284 ) ) ;
#206267 = EDGE_LOOP ( 'NONE', ( #39133, #49059, #12053, #11986 ) ) ;
#206268 = CARTESIAN_POINT ( 'NONE',  ( -1.201851678989727383E-14, 4.337500000000023448, -1.732050807568863648 ) ) ;
#206269 = CARTESIAN_POINT ( 'NONE',  ( 4.578903193113299963, 6.365139696764064325, 1.599625672291267398 ) ) ;
#206270 = CARTESIAN_POINT ( 'NONE',  ( 7.318703993278529829, 7.432909501780090800, 1.040834085586084257E-14 ) ) ;
#206271 = EDGE_CURVE ( 'NONE', #62806, #198880, #127254, .T. ) ;
#206272 = CARTESIAN_POINT ( 'NONE',  ( 3.071146466883535098, -1.680802468121232573, 1.452339882875167021 ) ) ;
#206273 = CARTESIAN_POINT ( 'NONE',  ( -7.185458225562757484, 11.32685899655781903, 0.7216878364870458196 ) ) ;
#206274 = DIRECTION ( 'NONE',  ( 0.000000000000000000, -1.000000000000000000, 0.000000000000000000 ) ) ;
#206275 = CARTESIAN_POINT ( 'NONE',  ( 6.561783159334121152, 8.678499657355050800, -1.443375672974057666 ) ) ;
#206276 = ADVANCED_FACE ( 'NONE', ( #119751 ), #137014, .F. ) ;
#206277 = CARTESIAN_POINT ( 'NONE',  ( -9.937763408692600109, 10.69640485300394417, -0.7216878364870267237 ) ) ;
#206278 = CARTESIAN_POINT ( 'NONE',  ( 6.590672070018850803, 7.822110515511036866, -1.082531754730548412 ) ) ;
#206279 = CARTESIAN_POINT ( 'NONE',  ( 1.037732671793228700, -1.587836052788630603, 1.242728777923551409 ) ) ;
#206281 = CARTESIAN_POINT ( 'NONE',  ( 6.602015036461629904, 0.7930265726678319416, -1.904331891608399996 ) ) ;
#206280 = CARTESIAN_POINT ( 'NONE',  ( 7.567422294721922960, 11.98040977715095323, 0.7998128361456462443 ) ) ;
#206282 = CARTESIAN_POINT ( 'NONE',  ( 6.821160681006788629, 8.091013894996997635, 1.082531754730549967 ) ) ;
#206283 = CARTESIAN_POINT ( 'NONE',  ( 6.128409194715155550, 0.1798751216713200540, 1.731140798666473968 ) ) ;
#206284 = CARTESIAN_POINT ( 'NONE',  ( 1.364683531249988535, 2.905208333674754506, -0.7879004041258239610 ) ) ;
#206285 = CARTESIAN_POINT ( 'NONE',  ( 1.352431244980515146, -1.399367522912741135, 1.083307108726710100 ) ) ;
#206286 = CARTESIAN_POINT ( 'NONE',  ( 6.504571816962987363, -1.679391772619584833, 0.4319377402999846627 ) ) ;
#206287 = CARTESIAN_POINT ( 'NONE',  ( 6.304260172732157663, 1.282988983046409848, -1.176258868317042294 ) ) ;
#206288 = CARTESIAN_POINT ( 'NONE',  ( 3.861076399890978283, 0.2801353988391065419, -2.275111823818583456 ) ) ;
#206289 = CARTESIAN_POINT ( 'NONE',  ( 1.364683531249986537, 0.1552083336747499542, -0.7879004041258309554 ) ) ;
#206290 = CARTESIAN_POINT ( 'NONE',  ( 2.150122221082468865, -1.423577340559305071, 1.167554138749151926 ) ) ;
#206291 = CARTESIAN_POINT ( 'NONE',  ( 9.531545685607134999, 11.07889037375188401, 1.199719254218450271 ) ) ;
#206292 = DIRECTION ( 'NONE',  ( 0.000000000000000000, -1.445602896647338917E-16, 1.000000000000000000 ) ) ;
#206293 = CARTESIAN_POINT ( 'NONE',  ( 3.065264358586119009, 0.2694654384877669395, -1.805464241506696155 ) ) ;
#206294 = CARTESIAN_POINT ( 'NONE',  ( 4.061172775696818782, -1.158689426361030561, 1.650081270007992318 ) ) ;
#206295 = CARTESIAN_POINT ( 'NONE',  ( -8.455481356417053007, 13.01647868246193518, 0.7998128361456341429 ) ) ;
#206297 = CARTESIAN_POINT ( 'NONE',  ( 1.499999999999959588, 6.999999999999999112, -10.89724735885168805 ) ) ;
#206296 = CARTESIAN_POINT ( 'NONE',  ( 3.274574482517400575, -1.349127789868936222, 1.816123189252472958 ) ) ;
#206298 = CARTESIAN_POINT ( 'NONE',  ( 5.877981411467888329, 1.251756350581848309, 1.693418440539447234 ) ) ;
#206299 = CARTESIAN_POINT ( 'NONE',  ( 9.633311866038676285, 13.62946609490282235, 8.224406077922058245 ) ) ;
#206300 =( BOUNDED_SURFACE ( )  B_SPLINE_SURFACE ( 1, 2, ( 
 ( #124127, #7048, #53697, #37440, #73124, #190089, #107853, #203119, #70980, #173879, #91560, #54761, #157616, #9213, #120910, #75284, #186882, #143528, #26523, #60094, #209524, #145666, #95828, #96898, #30819, #10270, #27594, #211664, #108919, #76345, #92632, #44942, #174941, #61165, #162947, #128397, #93692, #127327, #158673, #113190, #59027, #179196, #142453, #210610, #159735, #111049, #193297, #77412, #43874, #78477, #129460, #177056, #109990, #28673, #11333, #144596, #195443, #94758, #160807, #62238, #208461, #126253, #112125, #12398, #194364, #46006, #178129, #192212, #29745, #176002, #161885, #13472, #79548, #47073, #63300, #14527, #80624, #207408, #125185, #191146, #42812, #50248, #131548, #133668, #36109, #149892, #147761, #1458, #146714, #97957, #31879, #150959, #164013, #148813, #384, #83799, #66457, #197549, #199671, #115313, #183437, #100062, #213778, #64369, #15588, #212731, #180255, #32931, #49193, #99006, #181303, #48146, #17710, #130515, #67523, #51315, #196504, #165061, #117442, #101112, #35040, #118508, #16654, #116370, #114259, #82740, #132598, #198601, #182358, #167199, #18786, #33987, #84871, #65401, #166125, #2524, #81675, #68600, #134723, #200729, #52379, #184491, #102193, #168260, #19859, #186634, #202864, #201796, #171459, #152021, #23048, #205004, #135773, #54511, #6799, #40411, #188771, #57714, #38261, #203930, #53436, #104337, #71797, #5720, #170382, #122812, #172540, #70724, #106513, #87005, #55577, #154152, #85946, #137910, #21970, #153077, #88078, #206080, #4654, #136838, #121732, #187699, #119574, #120656, #39326, #24125, #90227, #189838, #123871, #103264, #105421, #156291, #185560, #169326, #37188, #89164, #20911, #155218, #41486, #72875, #138981, #56650, #7875, #107597, #3589, #173628, #73963, #140057, #69665, #143276, #93439, #109736, #76093, #110795, #161630, #27337, #142196, #77154, #191952, #176798, #13223, #43618, #209265, #28414, #141142, #108661, #144347, #60911, #127069, #193031, #44687, #58778, #94508, #208210, #59842, #128144, #124931, #79297, #174688, #26263, #175744 ),
 ( #92382, #190893, #210347, #78225, #125994, #25199, #157361, #160546, #159478, #12152, #158416, #207154, #11076, #42558, #8953, #61988, #194105, #45753, #111872, #10018, #177877, #29488, #95581, #145414, #211415, #63044, #129212, #195188, #46822, #112937, #91303, #75030, #32675, #48942, #180005, #131311, #84620, #31627, #15340, #197302, #115060, #212476, #97702, #181058, #117186, #67275, #68348, #2272, #196253, #213531, #183187, #80364, #47898, #64120, #16403, #146461, #98754, #134480, #99813, #65153, #164811, #130263, #150710, #30563, #200484, #114010, #182106, #82481, #148570, #139, #66204, #81429, #49995, #100867, #132349, #147511, #198355, #116116, #33735, #166953, #165878, #17465, #83549, #163762, #149629, #1212, #133413, #199420, #51063, #34792, #18544, #52130, #178950, #96643, #162698, #14270, #43105, #204473, #56126, #57193, #89714, #175230, #174171, #207701, #24672, #105993, #108146, #10559, #124415, #122284, #190374, #118257, #72350, #6279, #125478, #138454, #123354, #189320, #58259, #40958, #172013, #25743, #155764, #157911, #74512, #188242, #35867, #39882, #184240, #154695, #7348, #23606, #73427, #139529, #22528, #206628, #101942, #42033, #91854, #168008, #205554, #9506, #75578, #141687, #92918, #158963, #107066, #90778, #88637, #173091, #156840, #8426, #140616, #59321, #191439, #109219, #26815, #76632, #142747, #208756, #60381, #128681, #144885, #61454, #12685, #180535, #127621, #111344, #78761, #210891, #93986, #193585, #62518, #213016, #163235, #164290, #98235, #77702, #95046, #64651, #176287, #143822, #160028, #112409, #27891, #194650, #15878, #195729, #161096, #46293, #11628, #32158, #126544, #81963, #209819, #63590, #178420, #30030, #96115, #162171, #177349, #145942, #196787, #13757, #28962, #79833, #211953, #129746, #48428, #47366, #113479, #179486, #45229, #31108, #97180, #14817, #80909, #146999, #130792, #114542, #148048, #192506, #44157, #110278, #99298, #136061, #83020, #149094, #150183, #182653, #53734, #52663, #86231, #117735, #198887, #201017, #103554, #2813, #676, #68886, #214056 ) ),
 .UNSPECIFIED., .F., .F., .F. ) 
 B_SPLINE_SURFACE_WITH_KNOTS ( ( 2, 2 ),
 ( 3, 2, 2, 2, 2, 2, 2, 2, 2, 2, 2, 2, 2, 2, 2, 2, 2, 2, 2, 2, 2, 2, 2, 2, 2, 2, 2, 2, 2, 2, 2, 2, 2, 2, 2, 2, 2, 2, 2, 2, 2, 2, 2, 2, 2, 2, 2, 2, 2, 2, 2, 2, 2, 2, 2, 2, 2, 2, 2, 2, 2, 2, 2, 2, 2, 2, 2, 2, 2, 2, 2, 2, 2, 2, 2, 2, 2, 2, 2, 2, 2, 2, 2, 2, 2, 2, 2, 2, 2, 2, 2, 2, 2, 2, 2, 2, 2, 2, 2, 2, 2, 2, 2, 2, 2, 2, 2, 2, 2, 2, 2, 2, 2, 2, 2, 2, 2, 2, 2, 2, 3 ),
 ( 0.000000000000000000, 1.000000000000000000 ),
 ( 0.000000000000000000, 0.008333333333333333218, 0.01666666666666666644, 0.02500000000000000139, 0.03333333333333333287, 0.04166666666666666435, 0.05000000000000000278, 0.05833333333333333426, 0.06666666666666666574, 0.07499999999999999722, 0.08333333333333332871, 0.09166666666666666019, 0.1000000000000000056, 0.1083333333333333370, 0.1166666666666666685, 0.1250000000000000000, 0.1333333333333333315, 0.1416666666666666630, 0.1499999999999999944, 0.1583333333333333259, 0.1666666666666666574, 0.1749999999999999889, 0.1833333333333333204, 0.1916666666666666796, 0.2000000000000000111, 0.2083333333333333426, 0.2166666666666666741, 0.2250000000000000056, 0.2333333333333333370, 0.2416666666666666685, 0.2500000000000000000, 0.2583333333333333592, 0.2666666666666666630, 0.2750000000000000222, 0.2833333333333333259, 0.2916666666666666852, 0.2999999999999999889, 0.3083333333333333481, 0.3166666666666666519, 0.3250000000000000111, 0.3333333333333333148, 0.3416666666666666741, 0.3499999999999999778, 0.3583333333333333370, 0.3666666666666666408, 0.3750000000000000000, 0.3833333333333333592, 0.3916666666666666630, 0.4000000000000000222, 0.4083333333333333259, 0.4166666666666666852, 0.4249999999999999889, 0.4333333333333333481, 0.4416666666666666519, 0.4500000000000000111, 0.4583333333333333148, 0.4666666666666666741, 0.4749999999999999778, 0.4833333333333333370, 0.4916666666666666408, 0.5000000000000000000, 0.5083333333333333037, 0.5166666666666667185, 0.5250000000000000222, 0.5333333333333333259, 0.5416666666666666297, 0.5500000000000000444, 0.5583333333333333481, 0.5666666666666666519, 0.5749999999999999556, 0.5833333333333333703, 0.5916666666666666741, 0.5999999999999999778, 0.6083333333333332815, 0.6166666666666666963, 0.6250000000000000000, 0.6333333333333333037, 0.6416666666666667185, 0.6500000000000000222, 0.6583333333333333259, 0.6666666666666666297, 0.6750000000000000444, 0.6833333333333333481, 0.6916666666666666519, 0.6999999999999999556, 0.7083333333333333703, 0.7166666666666666741, 0.7249999999999999778, 0.7333333333333332815, 0.7416666666666666963, 0.7500000000000000000, 0.7583333333333333037, 0.7666666666666667185, 0.7750000000000000222, 0.7833333333333333259, 0.7916666666666666297, 0.8000000000000000444, 0.8083333333333333481, 0.8166666666666666519, 0.8249999999999999556, 0.8333333333333333703, 0.8416666666666666741, 0.8499999999999999778, 0.8583333333333332815, 0.8666666666666666963, 0.8750000000000000000, 0.8833333333333333037, 0.8916666666666667185, 0.9000000000000000222, 0.9083333333333333259, 0.9166666666666666297, 0.9250000000000000444, 0.9333333333333333481, 0.9416666666666666519, 0.9499999999999999556, 0.9583333333333333703, 0.9666666666666666741, 0.9749999999999999778, 0.9833333333333332815, 0.9916666666666666963, 1.000000000000000000 ),
 .UNSPECIFIED. ) 
 GEOMETRIC_REPRESENTATION_ITEM ( )  RATIONAL_B_SPLINE_SURFACE ( (
 ( 1.000000000000000000, 0.8660254037844387076, 1.000000000000000000, 0.8660254037844387076, 1.000000000000000000, 0.8660254037844387076, 1.000000000000000000, 0.8660254037844387076, 1.000000000000000000, 0.8660254037844387076, 1.000000000000000000, 0.8660254037844387076, 1.000000000000000000, 0.8660254037844387076, 1.000000000000000000, 0.8660254037844387076, 1.000000000000000000, 0.8660254037844387076, 1.000000000000000000, 0.8660254037844387076, 1.000000000000000000, 0.8660254037844387076, 1.000000000000000000, 0.8660254037844387076, 1.000000000000000000, 0.8660254037844387076, 1.000000000000000000, 0.8660254037844387076, 1.000000000000000000, 0.8660254037844387076, 1.000000000000000000, 0.8660254037844387076, 1.000000000000000000, 0.8660254037844387076, 1.000000000000000000, 0.8660254037844387076, 1.000000000000000000, 0.8660254037844387076, 1.000000000000000000, 0.8660254037844387076, 1.000000000000000000, 0.8660254037844387076, 1.000000000000000000, 0.8660254037844387076, 1.000000000000000000, 0.8660254037844387076, 1.000000000000000000, 0.8660254037844387076, 1.000000000000000000, 0.8660254037844387076, 1.000000000000000000, 0.8660254037844387076, 1.000000000000000000, 0.8660254037844387076, 1.000000000000000000, 0.8660254037844387076, 1.000000000000000000, 0.8660254037844387076, 1.000000000000000000, 0.8660254037844387076, 1.000000000000000000, 0.8660254037844387076, 1.000000000000000000, 0.8660254037844387076, 1.000000000000000000, 0.8660254037844387076, 1.000000000000000000, 0.8660254037844387076, 1.000000000000000000, 0.8660254037844387076, 1.000000000000000000, 0.8660254037844387076, 1.000000000000000000, 0.8660254037844387076, 1.000000000000000000, 0.8660254037844387076, 1.000000000000000000, 0.8660254037844387076, 1.000000000000000000, 0.8660254037844387076, 1.000000000000000000, 0.8660254037844387076, 1.000000000000000000, 0.8660254037844387076, 1.000000000000000000, 0.8660254037844387076, 1.000000000000000000, 0.8660254037844387076, 1.000000000000000000, 0.8660254037844387076, 1.000000000000000000, 0.8660254037844387076, 1.000000000000000000, 0.8660254037844387076, 1.000000000000000000, 0.8660254037844387076, 1.000000000000000000, 0.8660254037844387076, 1.000000000000000000, 0.8660254037844387076, 1.000000000000000000, 0.8660254037844387076, 1.000000000000000000, 0.8660254037844387076, 1.000000000000000000, 0.8660254037844387076, 1.000000000000000000, 0.8660254037844387076, 1.000000000000000000, 0.8660254037844387076, 1.000000000000000000, 0.8660254037844387076, 1.000000000000000000, 0.8660254037844387076, 1.000000000000000000, 0.8660254037844387076, 1.000000000000000000, 0.8660254037844387076, 1.000000000000000000, 0.8660254037844387076, 1.000000000000000000, 0.8660254037844387076, 1.000000000000000000, 0.8660254037844387076, 1.000000000000000000, 0.8660254037844387076, 1.000000000000000000, 0.8660254037844387076, 1.000000000000000000, 0.8660254037844387076, 1.000000000000000000, 0.8660254037844387076, 1.000000000000000000, 0.8660254037844387076, 1.000000000000000000, 0.8660254037844387076, 1.000000000000000000, 0.8660254037844387076, 1.000000000000000000, 0.8660254037844387076, 1.000000000000000000, 0.8660254037844387076, 1.000000000000000000, 0.8660254037844387076, 1.000000000000000000, 0.8660254037844387076, 1.000000000000000000, 0.8660254037844387076, 1.000000000000000000, 0.8660254037844387076, 1.000000000000000000, 0.8660254037844387076, 1.000000000000000000, 0.8660254037844387076, 1.000000000000000000, 0.8660254037844387076, 1.000000000000000000, 0.8660254037844387076, 1.000000000000000000, 0.8660254037844387076, 1.000000000000000000, 0.8660254037844387076, 1.000000000000000000, 0.8660254037844387076, 1.000000000000000000, 0.8660254037844387076, 1.000000000000000000, 0.8660254037844387076, 1.000000000000000000, 0.8660254037844387076, 1.000000000000000000, 0.8660254037844387076, 1.000000000000000000, 0.8660254037844387076, 1.000000000000000000, 0.8660254037844387076, 1.000000000000000000, 0.8660254037844387076, 1.000000000000000000, 0.8660254037844387076, 1.000000000000000000, 0.8660254037844387076, 1.000000000000000000, 0.8660254037844387076, 1.000000000000000000, 0.8660254037844387076, 1.000000000000000000, 0.8660254037844387076, 1.000000000000000000, 0.8660254037844387076, 1.000000000000000000, 0.8660254037844387076, 1.000000000000000000, 0.8660254037844387076, 1.000000000000000000, 0.8660254037844387076, 1.000000000000000000, 0.8660254037844387076, 1.000000000000000000, 0.8660254037844387076, 1.000000000000000000, 0.8660254037844387076, 1.000000000000000000, 0.8660254037844387076, 1.000000000000000000, 0.8660254037844387076, 1.000000000000000000, 0.8660254037844387076, 1.000000000000000000, 0.8660254037844387076, 1.000000000000000000, 0.8660254037844387076, 1.000000000000000000, 0.8660254037844387076, 1.000000000000000000, 0.8660254037844387076, 1.000000000000000000, 0.8660254037844387076, 1.000000000000000000, 0.8660254037844387076, 1.000000000000000000, 0.8660254037844387076, 1.000000000000000000, 0.8660254037844387076, 1.000000000000000000, 0.8660254037844387076, 1.000000000000000000, 0.8660254037844387076, 1.000000000000000000, 0.8660254037844387076, 1.000000000000000000, 0.8660254037844387076, 1.000000000000000000, 0.8660254037844387076, 1.000000000000000000, 0.8660254037844387076, 1.000000000000000000, 0.8660254037844387076, 1.000000000000000000, 0.8660254037844387076, 1.000000000000000000),
 ( 1.000000000000000000, 0.8660254037844387076, 1.000000000000000000, 0.8660254037844387076, 1.000000000000000000, 0.8660254037844387076, 1.000000000000000000, 0.8660254037844387076, 1.000000000000000000, 0.8660254037844387076, 1.000000000000000000, 0.8660254037844387076, 1.000000000000000000, 0.8660254037844387076, 1.000000000000000000, 0.8660254037844387076, 1.000000000000000000, 0.8660254037844387076, 1.000000000000000000, 0.8660254037844387076, 1.000000000000000000, 0.8660254037844387076, 1.000000000000000000, 0.8660254037844387076, 1.000000000000000000, 0.8660254037844387076, 1.000000000000000000, 0.8660254037844387076, 1.000000000000000000, 0.8660254037844387076, 1.000000000000000000, 0.8660254037844387076, 1.000000000000000000, 0.8660254037844387076, 1.000000000000000000, 0.8660254037844387076, 1.000000000000000000, 0.8660254037844387076, 1.000000000000000000, 0.8660254037844387076, 1.000000000000000000, 0.8660254037844387076, 1.000000000000000000, 0.8660254037844387076, 1.000000000000000000, 0.8660254037844387076, 1.000000000000000000, 0.8660254037844387076, 1.000000000000000000, 0.8660254037844387076, 1.000000000000000000, 0.8660254037844387076, 1.000000000000000000, 0.8660254037844387076, 1.000000000000000000, 0.8660254037844387076, 1.000000000000000000, 0.8660254037844387076, 1.000000000000000000, 0.8660254037844387076, 1.000000000000000000, 0.8660254037844387076, 1.000000000000000000, 0.8660254037844387076, 1.000000000000000000, 0.8660254037844387076, 1.000000000000000000, 0.8660254037844387076, 1.000000000000000000, 0.8660254037844387076, 1.000000000000000000, 0.8660254037844387076, 1.000000000000000000, 0.8660254037844387076, 1.000000000000000000, 0.8660254037844387076, 1.000000000000000000, 0.8660254037844387076, 1.000000000000000000, 0.8660254037844387076, 1.000000000000000000, 0.8660254037844387076, 1.000000000000000000, 0.8660254037844387076, 1.000000000000000000, 0.8660254037844387076, 1.000000000000000000, 0.8660254037844387076, 1.000000000000000000, 0.8660254037844387076, 1.000000000000000000, 0.8660254037844387076, 1.000000000000000000, 0.8660254037844387076, 1.000000000000000000, 0.8660254037844387076, 1.000000000000000000, 0.8660254037844387076, 1.000000000000000000, 0.8660254037844387076, 1.000000000000000000, 0.8660254037844387076, 1.000000000000000000, 0.8660254037844387076, 1.000000000000000000, 0.8660254037844387076, 1.000000000000000000, 0.8660254037844387076, 1.000000000000000000, 0.8660254037844387076, 1.000000000000000000, 0.8660254037844387076, 1.000000000000000000, 0.8660254037844387076, 1.000000000000000000, 0.8660254037844387076, 1.000000000000000000, 0.8660254037844387076, 1.000000000000000000, 0.8660254037844387076, 1.000000000000000000, 0.8660254037844387076, 1.000000000000000000, 0.8660254037844387076, 1.000000000000000000, 0.8660254037844387076, 1.000000000000000000, 0.8660254037844387076, 1.000000000000000000, 0.8660254037844387076, 1.000000000000000000, 0.8660254037844387076, 1.000000000000000000, 0.8660254037844387076, 1.000000000000000000, 0.8660254037844387076, 1.000000000000000000, 0.8660254037844387076, 1.000000000000000000, 0.8660254037844387076, 1.000000000000000000, 0.8660254037844387076, 1.000000000000000000, 0.8660254037844387076, 1.000000000000000000, 0.8660254037844387076, 1.000000000000000000, 0.8660254037844387076, 1.000000000000000000, 0.8660254037844387076, 1.000000000000000000, 0.8660254037844387076, 1.000000000000000000, 0.8660254037844387076, 1.000000000000000000, 0.8660254037844387076, 1.000000000000000000, 0.8660254037844387076, 1.000000000000000000, 0.8660254037844387076, 1.000000000000000000, 0.8660254037844387076, 1.000000000000000000, 0.8660254037844387076, 1.000000000000000000, 0.8660254037844387076, 1.000000000000000000, 0.8660254037844387076, 1.000000000000000000, 0.8660254037844387076, 1.000000000000000000, 0.8660254037844387076, 1.000000000000000000, 0.8660254037844387076, 1.000000000000000000, 0.8660254037844387076, 1.000000000000000000, 0.8660254037844387076, 1.000000000000000000, 0.8660254037844387076, 1.000000000000000000, 0.8660254037844387076, 1.000000000000000000, 0.8660254037844387076, 1.000000000000000000, 0.8660254037844387076, 1.000000000000000000, 0.8660254037844387076, 1.000000000000000000, 0.8660254037844387076, 1.000000000000000000, 0.8660254037844387076, 1.000000000000000000, 0.8660254037844387076, 1.000000000000000000, 0.8660254037844387076, 1.000000000000000000, 0.8660254037844387076, 1.000000000000000000, 0.8660254037844387076, 1.000000000000000000, 0.8660254037844387076, 1.000000000000000000, 0.8660254037844387076, 1.000000000000000000, 0.8660254037844387076, 1.000000000000000000, 0.8660254037844387076, 1.000000000000000000, 0.8660254037844387076, 1.000000000000000000, 0.8660254037844387076, 1.000000000000000000, 0.8660254037844387076, 1.000000000000000000, 0.8660254037844387076, 1.000000000000000000, 0.8660254037844387076, 1.000000000000000000, 0.8660254037844387076, 1.000000000000000000, 0.8660254037844387076, 1.000000000000000000, 0.8660254037844387076, 1.000000000000000000, 0.8660254037844387076, 1.000000000000000000, 0.8660254037844387076, 1.000000000000000000, 0.8660254037844387076, 1.000000000000000000, 0.8660254037844387076, 1.000000000000000000, 0.8660254037844387076, 1.000000000000000000, 0.8660254037844387076, 1.000000000000000000, 0.8660254037844387076, 1.000000000000000000, 0.8660254037844387076, 1.000000000000000000) ) ) 
 REPRESENTATION_ITEM ( '' )  SURFACE ( )  );
#206301 = CARTESIAN_POINT ( 'NONE',  ( 2.980987059868035693, 1.948563265827065960, 0.6999735360200682877 ) ) ;
#206302 = CARTESIAN_POINT ( 'NONE',  ( 4.813308228051395687, 5.574280006603454574, 1.199719254218462483 ) ) ;
#206303 = CARTESIAN_POINT ( 'NONE',  ( 1.360316468749957597, 0.3177083336747154596, -0.7853790794158961308 ) ) ;
#206304 = CARTESIAN_POINT ( 'NONE',  ( 4.477262591527907176, -1.894555094343739476, -0.9525379817736513433 ) ) ;
#206305 = AXIS2_PLACEMENT_3D ( 'NONE', #182445, #53525, #103346 ) ;
#206307 = CARTESIAN_POINT ( 'NONE',  ( 1.119610834840406577, -1.879747399699664978, 0.4211694731556160365 ) ) ;
#206306 = CARTESIAN_POINT ( 'NONE',  ( -10.10098813738111545, 11.74323990082152491, -1.199719254218441611 ) ) ;
#206308 = CARTESIAN_POINT ( 'NONE',  ( -4.492547798081878874, 6.334668079219206049, 1.599625672291263179 ) ) ;
#206309 = CARTESIAN_POINT ( 'NONE',  ( 7.587759525142423911, 12.00413654597487501, 0.7998128361456462443 ) ) ;
#206310 = CARTESIAN_POINT ( 'NONE',  ( 4.489158259456265121, 7.291082831790689056, -1.082531754730548412 ) ) ;
#206311 = CARTESIAN_POINT ( 'NONE',  ( 4.959245870426344460, 6.614204113168008270, 1.243730795111185339 ) ) ;
#206312 = CARTESIAN_POINT ( 'NONE',  ( -3.475000000000000533, -1.706249999044083587, 0.000000000000000000 ) ) ;
#206313 = CARTESIAN_POINT ( 'NONE',  ( -4.603156847039612920, 5.329103395422994716, 1.199719254218462483 ) ) ;
#206314 = CARTESIAN_POINT ( 'NONE',  ( 0.1588220795745398928, 2.216043539545629937, 0.1551192601621682043 ) ) ;
#206315 = CARTESIAN_POINT ( 'NONE',  ( 1.747240475267642257, -1.779442529384717808, 1.126025380906693352 ) ) ;
#206316 = CARTESIAN_POINT ( 'NONE',  ( -3.654804927335652209, 6.421633627603656080, 1.199719254218452935 ) ) ;
#206317 = CARTESIAN_POINT ( 'NONE',  ( 8.925345196497941558, 9.307324238869423283, 1.040834085586084257E-14 ) ) ;
#206318 = CARTESIAN_POINT ( 'NONE',  ( 5.823074758751579871, -1.681767765412798710, -0.7970822532109583802 ) ) ;
#206319 = CARTESIAN_POINT ( 'NONE',  ( 7.558834334818744338, 8.777393797832065303, 1.199719254218462483 ) ) ;
#206320 = CARTESIAN_POINT ( 'NONE',  ( -5.939880696562884310, 9.943961556049767836, 0.7216878364870267237 ) ) ;
#206321 = CARTESIAN_POINT ( 'NONE',  ( -9.002250809794013264, 9.604973487622245898, -0.7216878364870267237 ) ) ;
#206322 = CARTESIAN_POINT ( 'NONE',  ( 0.1586465271753433603, 2.115359532055087310, 0.1496401998123952359 ) ) ;
#206323 = CARTESIAN_POINT ( 'NONE',  ( -7.533490631048818109, 8.818102486758951031, -1.199719254218452047 ) ) ;
#206325 = CARTESIAN_POINT ( 'NONE',  ( 2.769914238037580745, -1.940913097850523128, 0.2850433363836765155 ) ) ;
#206324 = CARTESIAN_POINT ( 'NONE',  ( -1.225000000000052269, -0.4791666666666582475, 0.7072540797572637317 ) ) ;
#206326 = CARTESIAN_POINT ( 'NONE',  ( 2.096749907087645415, -0.5762017740289016032, -2.083436276955972222 ) ) ;
#206328 = CARTESIAN_POINT ( 'NONE',  ( -5.472563271839127275, 6.275773694203630626, -1.010060153610029321 ) ) ;
#206327 = CARTESIAN_POINT ( 'NONE',  ( -4.447956913735107598, 7.346977611736363656, 1.199719254218452935 ) ) ;
#206329 = CARTESIAN_POINT ( 'NONE',  ( 0.6823417656249882723, 2.176041667008084435, -1.181850606188749264 ) ) ;
#206330 = CARTESIAN_POINT ( 'NONE',  ( 3.345385115808647392, 1.740516467222261499, -0.001323508237265763176 ) ) ;
#206331 = CARTESIAN_POINT ( 'NONE',  ( 4.853455804012203778, 8.606189504748821051, 0.7216878364870438212 ) ) ;
#206332 = CARTESIAN_POINT ( 'NONE',  ( -11.34338453707543515, 5.310936115193626961, -5.661293933977025183 ) ) ;
#206333 = AXIS2_PLACEMENT_3D ( 'NONE', #97490, #192821, #146250 ) ;
#206334 = CARTESIAN_POINT ( 'NONE',  ( 2.811874868751465417, -1.677748492350576770, 1.117661080827489606 ) ) ;
#206335 = CARTESIAN_POINT ( 'NONE',  ( -2.449742653233043743, 3.299999999999976730, -0.4000000000000339950 ) ) ;
#206336 = CARTESIAN_POINT ( 'NONE',  ( 2.817209029084859928, -0.1949976385870570150, 1.961808326198757335 ) ) ;
#206337 = TOROIDAL_SURFACE ( 'NONE', #119981, 12.17999951260719804, 0.5000000000000008882 ) ;
#206340 = VERTEX_POINT ( 'NONE', #199854 ) ;
#206339 = CARTESIAN_POINT ( 'NONE',  ( -4.150204419558982671, 7.856005899545188242, 0.7216878364870338292 ) ) ;
#206338 = DIRECTION ( 'NONE',  ( -1.000000000000000000, 0.000000000000000000, 0.000000000000000000 ) ) ;
#206341 = CARTESIAN_POINT ( 'NONE',  ( -6.929625909916163451, 7.257187447756535903, 0.7216878364870317197 ) ) ;
#206342 = CARTESIAN_POINT ( 'NONE',  ( 6.333594036239346359, 7.418223126147930557, 1.199719254218453823 ) ) ;
#206343 = CARTESIAN_POINT ( 'NONE',  ( -7.130662446144611977, 7.283804040115648526, 0.000000000000000000 ) ) ;
#206344 = CARTESIAN_POINT ( 'NONE',  ( 2.807290699014941548, 1.731141667658737449, -1.040073625836896554 ) ) ;
#206345 = DIRECTION ( 'NONE',  ( -1.000000000000000000, 0.000000000000000000, 0.000000000000000000 ) ) ;
#206346 = CARTESIAN_POINT ( 'NONE',  ( 5.421043267468262705, 2.129509263528307716, 0.8893739899358196199 ) ) ;
#206348 = ADVANCED_FACE ( 'NONE', ( #185730 ), #214025, .T. ) ;
#206347 = CARTESIAN_POINT ( 'NONE',  ( -6.827626583076781053, -7.154544010627095219, -6.720112740279224006 ) ) ;
#206349 = CARTESIAN_POINT ( 'NONE',  ( 3.379693149055284174, -1.891888713350448947, 0.5187481205842571219 ) ) ;
#206350 = CARTESIAN_POINT ( 'NONE',  ( 8.910733272679570049, 11.41894145625809820, -1.599625672291255185 ) ) ;
#206351 = CARTESIAN_POINT ( 'NONE',  ( 0.5455463417442986129, -1.458554840210561476, 1.392547631435703037 ) ) ;
#206352 = VERTEX_POINT ( 'NONE', #150066 ) ;
#206353 = CARTESIAN_POINT ( 'NONE',  ( 2.079462195143897851, 1.640249684897076898, 1.338979269010678985 ) ) ;
#206355 = CARTESIAN_POINT ( 'NONE',  ( -5.696397096036042385, 9.797547045350714967, -0.7998128361456231517 ) ) ;
#206354 = CARTESIAN_POINT ( 'NONE',  ( -3.918470089549458635, 4.530302178351167441, -1.199719254218452047 ) ) ;
#206356 = CARTESIAN_POINT ( 'NONE',  ( 2.062219658421380775, -1.683061746929171321, -0.7467898329211535291 ) ) ;
#206357 = ORIENTED_EDGE ( 'NONE', *, *, #174601, .F. ) ;
#206358 = CARTESIAN_POINT ( 'NONE',  ( -10.47097470845587175, 11.11055866948701443, 1.040834085586084257E-14 ) ) ;
#206359 = CARTESIAN_POINT ( 'NONE',  ( 9.842318685493841812, 11.92143744661629867, 6.868033326349857859 ) ) ;
#206360 = CARTESIAN_POINT ( 'NONE',  ( 3.357788437482766675, -1.608272433257527556, -1.382313803475518244 ) ) ;
#206361 = CARTESIAN_POINT ( 'NONE',  ( 6.615187027077672255, -1.883050660437551205, 0.4742715046822160718 ) ) ;
#206362 = CARTESIAN_POINT ( 'NONE',  ( -11.48243876534946040, 11.37999999999999901, -3.200000000000001510 ) ) ;
#206363 = CARTESIAN_POINT ( 'NONE',  ( 6.252281394196331554, 10.44607872653774372, 1.040834085586084257E-14 ) ) ;
#206364 = CARTESIAN_POINT ( 'NONE',  ( 7.388267364804250725, 7.584343111885245570, -0.7998128361456341429 ) ) ;
#206365 = ORIENTED_EDGE ( 'NONE', *, *, #41220, .T. ) ;
#206366 = CARTESIAN_POINT ( 'NONE',  ( 3.831368270176987334, -1.905513148489059283, 0.7852520889023787420 ) ) ;
#206368 = CARTESIAN_POINT ( 'NONE',  ( 0.8898994657863326108, -0.4472179738511591895, -1.785967584704901912 ) ) ;
#206367 = CARTESIAN_POINT ( 'NONE',  ( -7.202405917357668663, 9.425892875049191488, 1.599625672291295375 ) ) ;
#206369 = CARTESIAN_POINT ( 'NONE',  ( 1.364683531249990311, 4.884375000341417916, 1.214306433183764966E-14 ) ) ;
#206370 = CARTESIAN_POINT ( 'NONE',  ( -0.7807912181424305764, 13.24045051524828942, -1.280767376876722041 ) ) ;
#206371 = CARTESIAN_POINT ( 'NONE',  ( 1.331021600797330118, 2.127646391749141941, 0.5858054460900484761 ) ) ;
#206372 = CARTESIAN_POINT ( 'NONE',  ( 3.286655449121218542, -2.228332854187901280, -0.3904065581350114611 ) ) ;
#206373 = CARTESIAN_POINT ( 'NONE',  ( -7.646435448427427062, 10.90429654226522693, 1.082531754730549967 ) ) ;
#206374 = CARTESIAN_POINT ( 'NONE',  ( 3.744242849288460295, 0.9642487561531964957, -1.533428966541541039 ) ) ;
#206375 = CARTESIAN_POINT ( 'NONE',  ( 2.588968054610871317, 1.620874238694985925, 1.020808031020562501 ) ) ;
#206376 = CARTESIAN_POINT ( 'NONE',  ( 4.387213907293201487, 0.09840592021137170575, 2.068135374880715638 ) ) ;
#206377 = CARTESIAN_POINT ( 'NONE',  ( 1.364683531249990311, 2.946875000341416140, 1.214306433183764966E-14 ) ) ;
#206378 = AXIS2_PLACEMENT_3D ( 'NONE', #129753, #110286, #176295 ) ;
#206379 = CARTESIAN_POINT ( 'NONE',  ( 3.028153684870387607, 1.096474020163393792, -1.638230769948149534 ) ) ;
#206380 = CARTESIAN_POINT ( 'NONE',  ( 0.7625677631861004224, -1.397537113076696036, 1.326088851308028449 ) ) ;
#206381 = CARTESIAN_POINT ( 'NONE',  ( 3.520239479114236403, 1.187513476551487424, -1.445374034619356207 ) ) ;
#206382 = CARTESIAN_POINT ( 'NONE',  ( 2.649405215588944262, -1.917952202864357414, 1.283049733485057908 ) ) ;
#206383 = CARTESIAN_POINT ( 'NONE',  ( 3.789374314311170000, -1.720299746930791684, 0.7104884466354021155 ) ) ;
#206384 = CARTESIAN_POINT ( 'NONE',  ( -1.364683531250010295, 3.780208333674750953, 0.7879004041258379498 ) ) ;
#206385 = CARTESIAN_POINT ( 'NONE',  ( -5.759516327706961647, 5.613857225279885732, -0.7998128361456221525 ) ) ;
#206386 = CARTESIAN_POINT ( 'NONE',  ( 6.908042961362778733, 8.018137195466769285, 1.199719254218462483 ) ) ;
#206387 = CARTESIAN_POINT ( 'NONE',  ( 0.000000000000000000, 6.999999999999999112, 0.000000000000000000 ) ) ;
#206388 = CARTESIAN_POINT ( 'NONE',  ( 0.1531350777018150311, -1.689991139269167109, 1.256553844878212978 ) ) ;
#206389 = CARTESIAN_POINT ( 'NONE',  ( 3.185802909086945967, 5.700225246367978116, 1.082531754730546636 ) ) ;
#206391 = DIRECTION ( 'NONE',  ( 0.6783731810844091381, 0.000000000000000000, 0.7347175152297780176 ) ) ;
#206390 = CARTESIAN_POINT ( 'NONE',  ( 0.6823417656249917140, 4.155208333674755394, 1.181850606188765695 ) ) ;
#206392 = CARTESIAN_POINT ( 'NONE',  ( -1.887367962963634627, 8.990012987145949097, -0.7749999999999996891 ) ) ;
#206393 = CARTESIAN_POINT ( 'NONE',  ( 2.338272602237463360, -1.224740070204191289, -1.730971256048131401 ) ) ;
#206395 = EDGE_CURVE ( 'NONE', #74942, #191954, #200276, .T. ) ;
#206394 = CARTESIAN_POINT ( 'NONE',  ( 0.7033857886646873725, 1.779361102145039286, -0.9557781530431900263 ) ) ;
#206396 = CARTESIAN_POINT ( 'NONE',  ( -1.402160292154681736E-14, 1.196875000341419026, -1.575800808251659024 ) ) ;
#206397 = CIRCLE ( 'NONE', #189244, 0.08000000000000025147 ) ;
#206398 = CARTESIAN_POINT ( 'NONE',  ( -4.772106882330234612, 6.590544000850479200, -1.443375672974053447 ) ) ;
#206399 = CARTESIAN_POINT ( 'NONE',  ( 5.931855901178834323, 6.879252291918818152, 1.199719254218462483 ) ) ;
#206400 = CARTESIAN_POINT ( 'NONE',  ( 1.405796033167512116, -0.5266655099175953092, 2.096309153942426562 ) ) ;
#206403 = CARTESIAN_POINT ( 'NONE',  ( 4.094199201646931741, 4.839282492418613302, -1.082531754730543083 ) ) ;
#206402 = CARTESIAN_POINT ( 'NONE',  ( 6.825078400183548055, 2.461594334264828987, 2.239602747093616841 ) ) ;
#206401 = CARTESIAN_POINT ( 'NONE',  ( 4.766573523656222555, 7.718696989977711809, 1.199719254218452047 ) ) ;
#206404 = CARTESIAN_POINT ( 'NONE',  ( -0.2104748580754183807, 2.005809028216706924, -2.517884123765606663 ) ) ;
#206405 = CARTESIAN_POINT ( 'NONE',  ( 6.157435431667657610, 1.928259211291092123, -0.5899821858514133766 ) ) ;
#206407 = CARTESIAN_POINT ( 'NONE',  ( -5.682275777458886346, 7.722684055159061423, 1.443375672974058777 ) ) ;
#206406 = CARTESIAN_POINT ( 'NONE',  ( -8.297226821883391779, 11.66355314463053006, 1.082531754730549967 ) ) ;
#206408 = EDGE_CURVE ( 'NONE', #169055, #45206, #53618, .T. ) ;
#206409 = CARTESIAN_POINT ( 'NONE',  ( -1.734723475976807094E-15, 3.481548657788671619, -11.92000000000000171 ) ) ;
#206411 = CARTESIAN_POINT ( 'NONE',  ( -0.6823417656250039265, 11.06770833367473550, -1.181850606188755259 ) ) ;
#206410 = CARTESIAN_POINT ( 'NONE',  ( 0.1458946441583548470, -1.751458424797154523, -1.431810583859528974 ) ) ;
#206412 = CARTESIAN_POINT ( 'NONE',  ( -10.47097470845587175, 11.11055866948701443, 1.040834085586084257E-14 ) ) ;
#206414 = CARTESIAN_POINT ( 'NONE',  ( -0.1353477234830356701, -0.1462924468558861324, -1.883848219957585446 ) ) ;
#206413 = CARTESIAN_POINT ( 'NONE',  ( -6.371969008298464132, 6.536311385877402458, 1.040834085586084257E-14 ) ) ;
#206415 = CARTESIAN_POINT ( 'NONE',  ( 0.6823417656249882723, 0.7385416670080829915, -1.181850606188749264 ) ) ;
#206416 = CARTESIAN_POINT ( 'NONE',  ( 1.499999999999993117, 9.354166666666667851, 0.8660254037844408170 ) ) ;
#206417 = CARTESIAN_POINT ( 'NONE',  ( 11.94654170777226376, 11.15174326158935969, 1.134972293687618539 ) ) ;
#206418 = CARTESIAN_POINT ( 'NONE',  ( 2.332253321102405685, 1.672780984221501122, 0.4201815020834080427 ) ) ;
#206419 = CARTESIAN_POINT ( 'NONE',  ( 3.088225128862704949, 6.824956093640315302, 0.7998128361456281477 ) ) ;
#206420 = CARTESIAN_POINT ( 'NONE',  ( 4.908934136599710563, 7.884784371745123366, 1.199719254218451159 ) ) ;
#206421 = CARTESIAN_POINT ( 'NONE',  ( 1.299667926800106121, -1.769921777095804671, -0.007132476793576813211 ) ) ;
#206422 = CARTESIAN_POINT ( 'NONE',  ( 2.016272687986338852, -2.012595170092303043, 0.05167081324058443031 ) ) ;
#206423 = SURFACE_STYLE_USAGE ( .BOTH. , #109004 ) ;
#206424 = CARTESIAN_POINT ( 'NONE',  ( 4.175548122884573665, 3.973820352894515295, 1.214306433183764966E-14 ) ) ;
#206425 = CARTESIAN_POINT ( 'NONE',  ( 4.559734661428293201, 0.4870809927834463537, -2.152189095746533720 ) ) ;
#206426 = VERTEX_POINT ( 'NONE', #71973 ) ;
#206427 = CARTESIAN_POINT ( 'NONE',  ( 8.229436053370676518, 9.663725486096376827, 1.082531754730558626 ) ) ;
#206429 = CARTESIAN_POINT ( 'NONE',  ( 3.058220425488000327, -1.198843740453523043, 1.621196181159669347 ) ) ;
#206428 = CARTESIAN_POINT ( 'NONE',  ( 4.688201205076114597, 1.221562550966972527, 1.733079268972044895 ) ) ;
#206431 = ORIENTED_EDGE ( 'NONE', *, *, #21174, .T. ) ;
#206430 = CARTESIAN_POINT ( 'NONE',  ( 2.917991513842286277, -1.809334129394428947, 0.09316547460730231767 ) ) ;
#206432 = CARTESIAN_POINT ( 'NONE',  ( 4.224247379109608680, 7.085983154673295203, -1.199719254218452047 ) ) ;
#206433 = ORIENTED_EDGE ( 'NONE', *, *, #64524, .F. ) ;
#206434 = CARTESIAN_POINT ( 'NONE',  ( 1.692057038649401601, -1.861345348035767344, -0.1864469194169729449 ) ) ;
#206435 = ADVANCED_FACE ( 'NONE', ( #134896 ), #1637, .T. ) ;
#206436 = CARTESIAN_POINT ( 'NONE',  ( 6.428339884752386268, 1.046657586246093175, -1.495688092090130095 ) ) ;
#206438 = CARTESIAN_POINT ( 'NONE',  ( 2.958105166426743704, -1.137214127935105790, 1.541527475959689308 ) ) ;
#206437 = CARTESIAN_POINT ( 'NONE',  ( -3.898132859128961236, 4.506575409527250997, -1.199719254218452047 ) ) ;
#206439 = CARTESIAN_POINT ( 'NONE',  ( -11.41381675112453387, 10.19999999999999929, -3.704697986577184299 ) ) ;
#206440 = CARTESIAN_POINT ( 'NONE',  ( -0.6823417656250212460, 1.613541667008083769, 1.181850606188755259 ) ) ;
#206441 = CARTESIAN_POINT ( 'NONE',  ( 2.483409115735829786, 3.555461883994702532, -11.68352130004405431 ) ) ;
#206442 = CARTESIAN_POINT ( 'NONE',  ( 6.699137298928145690, 8.909022496873262753, 1.443375672974065660 ) ) ;
#206443 = CARTESIAN_POINT ( 'NONE',  ( -3.363831509966363598, 5.978201624052440266, -1.082531754730548412 ) ) ;
#206444 = CARTESIAN_POINT ( 'NONE',  ( -7.273023059088104425, 7.449891421883056530, 0.000000000000000000 ) ) ;
#206445 = CARTESIAN_POINT ( 'NONE',  ( 4.008146050417991546, -0.8085630067716749192, 1.960596031080278356 ) ) ;
#206447 = CARTESIAN_POINT ( 'NONE',  ( -10.48266952940149466, 5.268049057482275366, -5.154014898524191146 ) ) ;
#206446 = CARTESIAN_POINT ( 'NONE',  ( 2.019980081995985000, 3.974415841077576061, -11.36314192354172370 ) ) ;
#206448 = CARTESIAN_POINT ( 'NONE',  ( 3.919176214919489976, -0.1484353776938246439, 1.965847438023991423 ) ) ;
#206449 = CARTESIAN_POINT ( 'NONE',  ( 0.1584477454876299096, 2.008078640038186258, 0.1440931537372847071 ) ) ;
#206450 = VERTEX_POINT ( 'NONE', #67696 ) ;
#206451 = VECTOR ( 'NONE', #21806, 1000.000000000000000 ) ;
#206452 = CARTESIAN_POINT ( 'NONE',  ( -0.07047696482224277692, -1.639844204322737697, -1.338861086256079913 ) ) ;
#206453 = CARTESIAN_POINT ( 'NONE',  ( -0.5635687842576226902, 6.831326244322589503, -3.741768325763386915 ) ) ;
#206454 = CARTESIAN_POINT ( 'NONE',  ( 1.856005582152659317, -0.6995316168164237292, 1.948720873434762080 ) ) ;
#206455 = CARTESIAN_POINT ( 'NONE',  ( 7.517069824134078537, 7.734612647770044092, 0.000000000000000000 ) ) ;
#206456 = ORIENTED_EDGE ( 'NONE', *, *, #164554, .F. ) ;
#206457 = CARTESIAN_POINT ( 'NONE',  ( 6.039231080244466199, 6.010467446565510130, 0.7998128361456352531 ) ) ;
#206458 = CARTESIAN_POINT ( 'NONE',  ( 5.664274315459256748, 9.830346811336296398, -0.7998128361456481317 ) ) ;
#206460 = CARTESIAN_POINT ( 'NONE',  ( 4.482942347612929979, 8.381849838857084123, 1.040834085586084257E-14 ) ) ;
#206459 = CARTESIAN_POINT ( 'NONE',  ( 3.996100316046395484, -0.6559638842641742906, -1.985124821949519891 ) ) ;
#206461 = CARTESIAN_POINT ( 'NONE',  ( 6.393551957296131683, 9.616838495890963401, 1.199719254218452047 ) ) ;
#206464 = ORIENTED_EDGE ( 'NONE', *, *, #176359, .T. ) ;
#206463 = CARTESIAN_POINT ( 'NONE',  ( 0.5393639851597960000, -1.720521155456521400, 0.5669088471357224268 ) ) ;
#206462 = CARTESIAN_POINT ( 'NONE',  ( 1.694096453153286497, -1.816434584207878622, -0.1825648128309723117 ) ) ;
#206465 = CARTESIAN_POINT ( 'NONE',  ( 5.971336403843029217, 0.1662174427981797931, -2.200672837095698497 ) ) ;
#206466 = FILL_AREA_STYLE_COLOUR ( '', #99383 ) ;
#206467 = CARTESIAN_POINT ( 'NONE',  ( 4.471826267013489620, 2.141383520707430321, -0.5327586567505787629 ) ) ;
#206468 = CARTESIAN_POINT ( 'NONE',  ( 7.039708073993665494, 9.236078724457858158, 1.599625672291281386 ) ) ;
#206469 = CARTESIAN_POINT ( 'NONE',  ( -1.364683531250010740, 8.442708333674730170, 0.7879004041258445001 ) ) ;
#206470 = CARTESIAN_POINT ( 'NONE',  ( 3.141163725242692273, 0.04933110545866059571, 1.911816780882446221 ) ) ;
#206471 = CARTESIAN_POINT ( 'NONE',  ( 9.447334110624092673, 9.916311305349925220, -0.7998128361456281477 ) ) ;
#206472 = CARTESIAN_POINT ( 'NONE',  ( 5.424307079040113777, 1.017280057988108499, 1.803113764695261301 ) ) ;
#206474 = DIRECTION ( 'NONE',  ( 1.000000000000000000, -7.387867266669436732E-31, 0.000000000000000000 ) ) ;
#206473 = DIRECTION ( 'NONE',  ( -0.9999980456341538426, 0.000000000000000000, -0.001977050295949311660 ) ) ;
#206475 = CARTESIAN_POINT ( 'NONE',  ( 6.181208317857348256, 1.509947553572440704, 1.588605474358975478 ) ) ;
#206476 = ORIENTED_EDGE ( 'NONE', *, *, #57396, .T. ) ;
#206477 = VERTEX_POINT ( 'NONE', #204096 ) ;
#206478 = CARTESIAN_POINT ( 'NONE',  ( -3.240035523541588081, 6.723865844199796271, 0.7216878364870096263 ) ) ;
#206479 = CARTESIAN_POINT ( 'NONE',  ( 1.580803134831910928, -0.9624764945123421844, 1.305310695360492712 ) ) ;
#206480 = CARTESIAN_POINT ( 'NONE',  ( 5.357406976055401948, 6.279338222599979424, 1.199719254218452935 ) ) ;
#206481 = CARTESIAN_POINT ( 'NONE',  ( -3.285556943749998737, -1.917708332855377673, 1.896917185911908721 ) ) ;
#206482 = CARTESIAN_POINT ( 'NONE',  ( -5.029148636026397945, 4.832037928311032182, 0.7998128361456281477 ) ) ;
#206483 = CARTESIAN_POINT ( 'NONE',  ( -7.049876689426103127, 10.20831132343037062, -1.082531754730537976 ) ) ;
#206484 = CARTESIAN_POINT ( 'NONE',  ( 6.086684617892325733, 6.065829907154645539, -0.7998128361456481317 ) ) ;
#206485 = CARTESIAN_POINT ( 'NONE',  ( 6.121949425127414024, 2.040613181561203859, -0.3481179853092666865 ) ) ;
#206486 = CARTESIAN_POINT ( 'NONE',  ( 4.143132006054106142, -1.675477906314150056, 0.9507637539484592448 ) ) ;
#206487 = CARTESIAN_POINT ( 'NONE',  ( 0.05236148938883232462, -1.314980595004966002, 1.528755779884483523 ) ) ;
#206488 = CARTESIAN_POINT ( 'NONE',  ( 4.549612403093820312, 8.500000000000243361, -0.2314049244472246580 ) ) ;
#206489 = CARTESIAN_POINT ( 'NONE',  ( 3.464990776744291345, 6.200183785247111778, 1.199719254218452047 ) ) ;
#206490 = DIRECTION ( 'NONE',  ( -0.3281536732072464768, -0.000000000000000000, 0.9446243521954066358 ) ) ;
#206491 = CARTESIAN_POINT ( 'NONE',  ( 0.3752731597879420677, 2.043270790221253908, -0.7926104125151807178 ) ) ;
#206492 = CARTESIAN_POINT ( 'NONE',  ( 5.584540971669589737, -1.782103179330214449, -0.3958202769075992444 ) ) ;
#206493 = CARTESIAN_POINT ( 'NONE',  ( 6.211043768836185031, 6.418841616496599123, 0.7216878364870328300 ) ) ;
#206494 = CARTESIAN_POINT ( 'NONE',  ( 4.975479186090860928, 4.907073259968533385, 0.7216878364870317197 ) ) ;
#206495 = CARTESIAN_POINT ( 'NONE',  ( -4.457598643843001973, 8.422558527783969851, 0.000000000000000000 ) ) ;
#206496 = CARTESIAN_POINT ( 'NONE',  ( 3.366167277942881064, 7.149221934233827014, -0.7998128361456362523 ) ) ;
#206497 = ORIENTED_EDGE ( 'NONE', *, *, #31198, .F. ) ;
#206499 = CARTESIAN_POINT ( 'NONE',  ( 6.082294971626270197, 1.038730605371197324, 1.724430661308763213 ) ) ;
#206498 = CARTESIAN_POINT ( 'NONE',  ( 2.208333698829296310, 1.645431377724184463, 0.8263914577605266931 ) ) ;
#206500 = CARTESIAN_POINT ( 'NONE',  ( 0.8260327929942178349, -1.663255926670023976, 1.586464751714482979 ) ) ;
#206501 = CARTESIAN_POINT ( 'NONE',  ( 6.332860960579021814, -1.861707940517230764, -0.6185968553879470644 ) ) ;
#206502 = CARTESIAN_POINT ( 'NONE',  ( -5.555090253297260361, 7.504024600312024340, 1.599625672291269396 ) ) ;
#206503 = CARTESIAN_POINT ( 'NONE',  ( -5.947207536862552324, 6.164775583291447703, -0.3409585216945008046 ) ) ;
#206504 = CARTESIAN_POINT ( 'NONE',  ( -2.839543107058306592, 5.400218493954923815, -1.199719254218446718 ) ) ;
#206505 = CARTESIAN_POINT ( 'NONE',  ( 0.7661813929631040576, -2.060537521029872643, 0.2012509062776293156 ) ) ;
#206506 = CARTESIAN_POINT ( 'NONE',  ( -5.320648938720212051, 5.172121614787156929, 0.000000000000000000 ) ) ;
#206508 = CARTESIAN_POINT ( 'NONE',  ( 0.9185735243398345240, 1.726912363944958617, 0.7195956246372691156 ) ) ;
#206507 = CARTESIAN_POINT ( 'NONE',  ( 2.349268366499413840, 0.5549471352096692067, -2.015694315139557435 ) ) ;
#206509 = CARTESIAN_POINT ( 'NONE',  ( 2.372422516638694745, -0.4444355326964634090, 1.966343308868031103 ) ) ;
#206510 = CARTESIAN_POINT ( 'NONE',  ( 7.592202833972727660, 11.80139437303613015, -0.7216878364870267237 ) ) ;
#206511 = EDGE_LOOP ( 'NONE', ( #143011, #82172, #105522, #161971 ) ) ;
#206512 = CARTESIAN_POINT ( 'NONE',  ( -1.001543065824772872E-14, 4.384375000341417916, 1.575800808251672791 ) ) ;
#206513 = CARTESIAN_POINT ( 'NONE',  ( 2.489492129562159484, -1.735903792773977772, -0.1261859363600649764 ) ) ;
#206514 = CARTESIAN_POINT ( 'NONE',  ( 6.308621549060418054, 6.254479983525607523, 0.7998128361456341429 ) ) ;
#206516 = CARTESIAN_POINT ( 'NONE',  ( -3.469446951953614189E-15, 3.507114751586604129, 11.99288524841339054 ) ) ;
#206515 = CARTESIAN_POINT ( 'NONE',  ( 1.500000000000035971, 7.750000000000000000, 10.99818166789401275 ) ) ;
#206517 = CARTESIAN_POINT ( 'NONE',  ( 3.246439759211931175, 0.4201230555563889579, 1.672790298054289693 ) ) ;
#206518 = CARTESIAN_POINT ( 'NONE',  ( 2.929422067023911502, -1.473737196803912797, -1.622193633833472814 ) ) ;
#206519 = CARTESIAN_POINT ( 'NONE',  ( 5.338574060078519423, 2.173733305800494175, 0.3801736985692484305 ) ) ;
#206520 = CARTESIAN_POINT ( 'NONE',  ( -10.83922355283164407, 5.627439893072524235, -6.488667358217312220 ) ) ;
#206521 = PRESENTATION_LAYER_ASSIGNMENT (  '', '', ( #71682 ) ) ;
#206522 = CARTESIAN_POINT ( 'NONE',  ( 1.956167536658510953, -0.7342896127641992399, 2.043222018709658805 ) ) ;
#206523 = CARTESIAN_POINT ( 'NONE',  ( 1.453431991042982041, 0.5316948868413253759, -1.746555546766684675 ) ) ;
#206524 = CARTESIAN_POINT ( 'NONE',  ( 3.397769718358482738, -2.085282637925215177, 0.3663039253445389276 ) ) ;
#206525 = FACE_OUTER_BOUND ( 'NONE', #190720, .T. ) ;
#206526 = VERTEX_POINT ( 'NONE', #4824 ) ;
#206528 = CARTESIAN_POINT ( 'NONE',  ( -1.364683531250014514, 1.301041667008083325, -0.7879004041258289570 ) ) ;
#206527 = CARTESIAN_POINT ( 'NONE',  ( 3.105313311461850745, -0.4450742334846323756, 2.248595817482400783 ) ) ;
#206529 = CARTESIAN_POINT ( 'NONE',  ( 0.6125000000000019318, 2.666666666666678509, -1.060881119635941339 ) ) ;
#206530 = CARTESIAN_POINT ( 'NONE',  ( 4.701980345841006326, 4.380065246436280368, 0.7998128361456341429 ) ) ;
#206532 = ADVANCED_FACE ( 'NONE', ( #51495 ), #44629, .T. ) ;
#206531 = MECHANICAL_DESIGN_GEOMETRIC_PRESENTATION_REPRESENTATION (  '', ( #50847 ), #106258 ) ;
#206533 = CARTESIAN_POINT ( 'NONE',  ( 6.639320575229294086, -0.003630812595115453199, 2.203388474976493594 ) ) ;
#206534 = CARTESIAN_POINT ( 'NONE',  ( -6.738039156311804945, 6.963393225226301553, 1.040834085586084257E-14 ) ) ;
#206535 = CARTESIAN_POINT ( 'NONE',  ( 4.690757960648234359, 4.574898496952131133, 0.7216878364870317197 ) ) ;
#206536 = CARTESIAN_POINT ( 'NONE',  ( -5.707619481228817904, 8.642344580533519505, -1.082531754730537976 ) ) ;
#206537 = CARTESIAN_POINT ( 'NONE',  ( 2.957086901556340575, 6.464035461875470290, 0.7216878364870257245 ) ) ;
#206538 = ORIENTED_EDGE ( 'NONE', *, *, #164073, .F. ) ;
#206539 = CARTESIAN_POINT ( 'NONE',  ( 4.676407821165474488, 1.496050514612049742, 1.352155788975975437 ) ) ;
#206541 = CARTESIAN_POINT ( 'NONE',  ( 3.327062588944328603, -1.903923626093235955, -0.7937240881994469532 ) ) ;
#206540 = CARTESIAN_POINT ( 'NONE',  ( 5.229694566569264680, 7.124396299129368337, 1.599625672291267398 ) ) ;
#206542 = CARTESIAN_POINT ( 'NONE',  ( 7.828907357248368726, 8.098423103070084395, 0.7998128361456281477 ) ) ;
#206543 = CARTESIAN_POINT ( 'NONE',  ( 4.055297343818933697, 5.824542549245813383, 1.443375672974058777 ) ) ;
#206544 = CARTESIAN_POINT ( 'NONE',  ( 0.000000000000000000, -4.046874999522043659, -3.793834371823813001 ) ) ;
#206545 = CARTESIAN_POINT ( 'NONE',  ( -1.364683531250010295, 5.738541667008088432, -0.7879004041258300672 ) ) ;
#206546 = CARTESIAN_POINT ( 'NONE',  ( 6.351546390744762682, 2.185874319550953793, -0.1572705277706408500 ) ) ;
#206547 = CARTESIAN_POINT ( 'NONE',  ( 3.885388821667290493, -0.6351983117205138862, -1.913803978180687482 ) ) ;
#206548 = CARTESIAN_POINT ( 'NONE',  ( 3.157574601152390414, 0.8305207305269333151, 1.643389852989694200 ) ) ;
#206549 = AXIS2_PLACEMENT_3D ( 'NONE', #74678, #23777, #87723 ) ;
#206550 = CARTESIAN_POINT ( 'NONE',  ( 6.877010230629674759, 9.046264573866535486, 1.599625672291281386 ) ) ;
#206552 = EDGE_CURVE ( 'NONE', #176022, #170509, #6549, .T. ) ;
#206551 = SURFACE_STYLE_FILL_AREA ( #25666 ) ;
#206553 = CARTESIAN_POINT ( 'NONE',  ( 6.493173258741942178, 1.586635928914212013, -0.9027890188317910791 ) ) ;
#206554 = CARTESIAN_POINT ( 'NONE',  ( 0.03630054827139220924, -1.841026678340401679, 1.376304820193236189 ) ) ;
#206555 = CARTESIAN_POINT ( 'NONE',  ( -7.389357414647957256, 8.579670724299436557, 1.199719254218450271 ) ) ;
#206556 = CARTESIAN_POINT ( 'NONE',  ( 6.684454173705361768, -2.217265373380904681, -0.4495064082850850906 ) ) ;
#206557 = CARTESIAN_POINT ( 'NONE',  ( 1.647240615436126543, -1.778467030350115774, 1.127781350514756475 ) ) ;
#206558 = CARTESIAN_POINT ( 'NONE',  ( -5.448397627845328550, 7.449826213943242514, 1.599625672291263179 ) ) ;
#206559 = CARTESIAN_POINT ( 'NONE',  ( 8.925345196497941558, 9.307324238869423283, 1.040834085586084257E-14 ) ) ;
#206560 = CARTESIAN_POINT ( 'NONE',  ( 6.739811759324814133, 8.956476034002680109, -1.443375672974078761 ) ) ;
#206561 = DIRECTION ( 'NONE',  ( 1.000000000000000000, 0.000000000000000000, 0.000000000000000000 ) ) ;
#206562 = CARTESIAN_POINT ( 'NONE',  ( -6.388916700537716764, 8.476822122092563916, 1.599625672291283607 ) ) ;
#206563 = CARTESIAN_POINT ( 'NONE',  ( 0.000000000000000000, -8.233137084989849086, 0.000000000000000000 ) ) ;
#206564 = CARTESIAN_POINT ( 'NONE',  ( 6.439759776366765998, 9.496508258194486629, 1.082531754730558626 ) ) ;
#206565 = CARTESIAN_POINT ( 'NONE',  ( 4.313480937648101587, 7.206793636360196764, -1.001376897629567830 ) ) ;
#206566 = CARTESIAN_POINT ( 'NONE',  ( -4.412288926243578935, 7.235088616337731260, 1.199719254218464037 ) ) ;
#206568 = CARTESIAN_POINT ( 'NONE',  ( 3.850012423022421082, -1.533692773617735705, -1.607201352943017802 ) ) ;
#206567 = CARTESIAN_POINT ( 'NONE',  ( 2.303126745213024851, -0.3670769733005623814, -2.088442229865586697 ) ) ;
#206569 = CARTESIAN_POINT ( 'NONE',  ( 0.8147124124333324779, 2.026155960571228043, 0.8354305900151804964 ) ) ;
#206570 = CARTESIAN_POINT ( 'NONE',  ( 0.8212658843103730621, 2.040464674744349338, 0.8412164853940640175 ) ) ;
#206571 = CARTESIAN_POINT ( 'NONE',  ( -5.984998465789844069, 5.947196063035064206, 0.7998128361456281477 ) ) ;
#206572 = CARTESIAN_POINT ( 'NONE',  ( 4.334394203492665909, -1.131343785558375226, 1.602600411086833931 ) ) ;
#206573 = CARTESIAN_POINT ( 'NONE',  ( 9.185812768458653466, 10.67553530374532045, 1.199719254218453823 ) ) ;
#206574 = CARTESIAN_POINT ( 'NONE',  ( -1.364683531250012516, 0.7802083336747528408, 0.7879004041258379498 ) ) ;
#206575 = CARTESIAN_POINT ( 'NONE',  ( 6.610000000000006537, 0.6121396118998356783, 1.775466344933520846 ) ) ;
#206577 = ORIENTED_EDGE ( 'NONE', *, *, #43574, .F. ) ;
#206576 = CARTESIAN_POINT ( 'NONE',  ( -4.921246572080546500, 8.685278734161874681, 1.214306433183764966E-14 ) ) ;
#206578 = CARTESIAN_POINT ( 'NONE',  ( 2.918346969001627045, -2.117983955170518851, 0.1081942149789016649 ) ) ;
#206579 = CARTESIAN_POINT ( 'NONE',  ( -2.823841133396259639, 6.516508098929413961, -0.7998128361456481317 ) ) ;
#206580 = CARTESIAN_POINT ( 'NONE',  ( 6.051685545382852638, 0.6321331830463626789, -2.067208725892249799 ) ) ;
#206581 = CARTESIAN_POINT ( 'NONE',  ( 4.335397732480402055, 0.7831895168094182846, -1.666506522714307437 ) ) ;
#206582 = UNCERTAINTY_MEASURE_WITH_UNIT (LENGTH_MEASURE( 1.000000000000000082E-05 ), #123017, 'distance_accuracy_value', 'NONE');
#206583 = CARTESIAN_POINT ( 'NONE',  ( -5.862510748852908016, 6.029743210627831473, 0.3741650707956689081 ) ) ;
#206584 = CARTESIAN_POINT ( 'NONE',  ( -1.364683531250000748, 1.571875000341421691, 0.000000000000000000 ) ) ;
#206585 = CARTESIAN_POINT ( 'NONE',  ( -0.02444708455723310775, -1.687298116421297456, -0.4264520246781302593 ) ) ;
#206586 = CARTESIAN_POINT ( 'NONE',  ( 6.727182134110164746, 4.698490487241143043, 2.473633340027088678 ) ) ;
#206587 = CARTESIAN_POINT ( 'NONE',  ( 4.229780737783593203, 4.037091736943370535, -0.7216878364870188411 ) ) ;
#206588 = CARTESIAN_POINT ( 'NONE',  ( 8.776224899084628106, 13.27471476138783224, 8.184001253707569035 ) ) ;
#206589 = CARTESIAN_POINT ( 'NONE',  ( 4.663041391408608405, -1.929494027986548454, -0.9748474430888448561 ) ) ;
#206590 = CARTESIAN_POINT ( 'NONE',  ( -3.761497552787613330, 6.475832013972435242, 1.199719254218464037 ) ) ;
#206591 = CARTESIAN_POINT ( 'NONE',  ( 5.800157620552712778, -1.823839058171864203, 0.8595007112896931867 ) ) ;
#206592 = CARTESIAN_POINT ( 'NONE',  ( -8.988692655735990300, 9.589155641221221771, 0.7216878364870438212 ) ) ;
#206593 = CARTESIAN_POINT ( 'NONE',  ( 3.713887418366210280, -2.130098009959373151, 0.3673708613747132534 ) ) ;
#206594 = CARTESIAN_POINT ( 'NONE',  ( 3.919176214919489976, -0.1484353776938246439, 1.965847438023991423 ) ) ;
#206595 = CARTESIAN_POINT ( 'NONE',  ( -10.17567228521069467, -0.02076350362892331880, -2.500000000000000444 ) ) ;
#206596 = CARTESIAN_POINT ( 'NONE',  ( 1.097181765414790400, -0.5634973350938665693, -2.237626367659339088 ) ) ;
#206597 = B_SPLINE_CURVE_WITH_KNOTS ( 'NONE', 3,
 ( #516, #15725, #65533, #182489, #167330, #131679 ),
 .UNSPECIFIED., .F., .F.,
 ( 4, 2, 4 ),
 ( 0.0006378314054480077946, 0.0009584618939205538689, 0.001279092382393099943 ),
 .UNSPECIFIED. ) ;
#206598 = CARTESIAN_POINT ( 'NONE',  ( 3.391920509712963661, -0.8384013316644415292, 1.882726026762149285 ) ) ;
#206599 = CARTESIAN_POINT ( 'NONE',  ( 5.302268720778519295, 1.468090865803386880, -1.271420572733022780 ) ) ;
#206601 = ORIENTED_EDGE ( 'NONE', *, *, #72507, .T. ) ;
#206600 = CARTESIAN_POINT ( 'NONE',  ( -7.280365300414089802, 10.47721470291632784, 1.082531754730549967 ) ) ;
#206602 = CARTESIAN_POINT ( 'NONE',  ( -5.336015975430226099, 8.383046517047350932, -1.199719254218453823 ) ) ;
#206603 = CARTESIAN_POINT ( 'NONE',  ( 6.609999999999996767, 0.01081285896096208579, 1.720159828161059723 ) ) ;
#206605 = VERTEX_POINT ( 'NONE', #55748 ) ;
#206604 = CARTESIAN_POINT ( 'NONE',  ( -4.329849954717889915, 6.144853928627882489, 1.599625672291270506 ) ) ;
#206606 = CARTESIAN_POINT ( 'NONE',  ( -6.358410854684777291, 10.36197039720016022, -0.7216878364870267237 ) ) ;
#206607 = CARTESIAN_POINT ( 'NONE',  ( 2.011028756337205348, 1.635159560789069655, -1.482119803565529859 ) ) ;
#206608 = CARTESIAN_POINT ( 'NONE',  ( 3.285556943750000514, -3.201041666188709112, 1.896917185911906500 ) ) ;
#206609 = CARTESIAN_POINT ( 'NONE',  ( 6.842638302680406071, -1.923265442670134329, -0.3857968560932593660 ) ) ;
#206610 = CARTESIAN_POINT ( 'NONE',  ( 6.539320575229278454, 3.689604457162498630, 2.617406275049142916 ) ) ;
#206611 = CARTESIAN_POINT ( 'NONE',  ( 0.7499999999999902300, 5.097916667349482012, -1.299038105676658228 ) ) ;
#206612 = CYLINDRICAL_SURFACE ( 'NONE', #123758, 0.3999999999999997446 ) ;
#206615 = VECTOR ( 'NONE', #140764, 1000.000000000000000 ) ;
#206614 = CARTESIAN_POINT ( 'NONE',  ( 10.50000000000000178, 0.000000000000000000, 3.599999999999999201 ) ) ;
#206613 = DIRECTION ( 'NONE',  ( -0.7592566023653016805, -0.6507913734559627184, 4.115938288792108699E-15 ) ) ;
#206616 = CARTESIAN_POINT ( 'NONE',  ( 5.226429366918344144, 0.1390423275269437320, 1.835946739075666745 ) ) ;
#206617 = ORIENTED_EDGE ( 'NONE', *, *, #51475, .T. ) ;
#206618 = CARTESIAN_POINT ( 'NONE',  ( 1.920846698078120474, 1.922532266116746325, 0.7428477115608185244 ) ) ;
#206619 = CARTESIAN_POINT ( 'NONE',  ( -1.953008978358306879E-14, 0.7031250003414774019, 1.570758158831782270 ) ) ;
#206620 = CARTESIAN_POINT ( 'NONE',  ( -5.693534442735004752, 8.729875052244421951, 1.199719254218452047 ) ) ;
#206621 = CARTESIAN_POINT ( 'NONE',  ( -2.923234996448113687, 6.562191262498094702, -0.3692494997280490465 ) ) ;
#206622 = PRESENTATION_STYLE_ASSIGNMENT (( #140610 ) ) ;
#206623 = CARTESIAN_POINT ( 'NONE',  ( 4.137209430464448445, 7.978494768850520558, 1.040834085586084257E-14 ) ) ;
#206624 = CARTESIAN_POINT ( 'NONE',  ( 0.4794588345870378632, 1.923154262159839201, -0.7412630403166396986 ) ) ;
#206626 = CARTESIAN_POINT ( 'NONE',  ( 5.091278345985558396, -0.6575378499774006125, 1.720029930423284448 ) ) ;
#206625 = CARTESIAN_POINT ( 'NONE',  ( 4.866817647125399660, 4.983041418240444109, 0.6113003782640200612 ) ) ;
#206627 = CARTESIAN_POINT ( 'NONE',  ( 7.633404179693907388, 8.864391950186421454, -1.199719254218441611 ) ) ;
#206628 = CARTESIAN_POINT ( 'NONE',  ( -5.712781623311813384, 7.758274208654143855, -1.599625672291271394 ) ) ;
#206630 = ORIENTED_EDGE ( 'NONE', *, *, #169931, .T. ) ;
#206629 = CARTESIAN_POINT ( 'NONE',  ( -10.66594405399932910, -7.024005795609703284, 0.4637852190794224949 ) ) ;
#206631 = CARTESIAN_POINT ( 'NONE',  ( 4.758537496233657293, 0.8426522330295079799, 2.039869969286691731 ) ) ;
#206632 = CARTESIAN_POINT ( 'NONE',  ( 0.8081717762262634608, -2.151237856378166224, 0.2110218573620133986 ) ) ;
#206633 = CARTESIAN_POINT ( 'NONE',  ( -6.249945626219832739, 6.393950773452325542, 1.040834085586084257E-14 ) ) ;
#206634 = CARTESIAN_POINT ( 'NONE',  ( -0.2108831679770960255, -0.001785917861228669690, -1.896958272444612792 ) ) ;
#206635 = CARTESIAN_POINT ( 'NONE',  ( -0.03006412033006514162, -0.9462945741195265548, 1.780671068589256834 ) ) ;
#206636 = CARTESIAN_POINT ( 'NONE',  ( 6.170369307550806148, 10.21286493553572328, 0.7216878364870317197 ) ) ;
#206637 = DIRECTION ( 'NONE',  ( 1.000000000000000000, 0.000000000000000000, 0.000000000000000000 ) ) ;
#206638 = CARTESIAN_POINT ( 'NONE',  ( 6.094389051209717856, -1.018956457145767214, 1.618003106988876283 ) ) ;
#206639 = DIRECTION ( 'NONE',  ( 0.000000000000000000, 0.000000000000000000, 1.000000000000000000 ) ) ;
#206640 = CARTESIAN_POINT ( 'NONE',  ( 0.8658264364783776479, 0.9185255527898968930, 1.629538061279064642 ) ) ;
#206641 = MECHANICAL_DESIGN_GEOMETRIC_PRESENTATION_REPRESENTATION (  '', ( #109931 ), #33933 ) ;
#206642 = CARTESIAN_POINT ( 'NONE',  ( 1.973842561262352469, -0.8578407463649927456, 1.825077436249371354 ) ) ;
#206644 = CARTESIAN_POINT ( 'NONE',  ( 4.494815117402239935, -0.4609086856197233684, -2.054844913126519401 ) ) ;
#206643 = CARTESIAN_POINT ( 'NONE',  ( -9.501566725078754772, 9.979582688880366703, -0.7998128361456291469 ) ) ;
#206645 = CARTESIAN_POINT ( 'NONE',  ( 8.067265095331215718, 9.370563018429956870, 1.199719254218462483 ) ) ;
#206647 = CARTESIAN_POINT ( 'NONE',  ( -8.853638004923878313, 10.28799807962136548, 1.199719254218462483 ) ) ;
#206646 = CARTESIAN_POINT ( 'NONE',  ( 4.224247379109608680, 7.085983154673295203, -1.199719254218452047 ) ) ;
#206648 = LINE ( 'NONE', #58281, #106743 ) ;
#206650 = ADVANCED_FACE ( 'NONE', ( #38436 ), #36287, .T. ) ;
#206649 = CARTESIAN_POINT ( 'NONE',  ( 3.797132494115144308, -0.2020087959641834463, -2.009684039814496170 ) ) ;
#206651 = CARTESIAN_POINT ( 'NONE',  ( -1.201851678989727383E-14, 5.446875000341422357, -1.575800808251660134 ) ) ;
#206652 = CARTESIAN_POINT ( 'NONE',  ( 7.619319141200051604, 11.83303006480134911, 0.7216878364870438212 ) ) ;
#206653 = CARTESIAN_POINT ( 'NONE',  ( 4.481803774187195444, 1.408218611193782221, 1.640057829624480101 ) ) ;
#206654 = CARTESIAN_POINT ( 'NONE',  ( 7.201315867513990554, 8.430565262634994284, -1.199719254218452047 ) ) ;
#206655 = CARTESIAN_POINT ( 'NONE',  ( -1.500000000000011324, 5.420833333333356485, 0.8660254037844403729 ) ) ;
#206656 = CARTESIAN_POINT ( 'NONE',  ( 6.717138760927786834, 6.801359740696030443, -0.7998128361456481317 ) ) ;
#206657 = CARTESIAN_POINT ( 'NONE',  ( 7.090551149822722721, 11.21613407486112379, 0.7216878364870438212 ) ) ;
#206659 = CARTESIAN_POINT ( 'NONE',  ( 0.08058608058607380498, -8.407420853759283830, 10.99970480893082225 ) ) ;
#206658 = CARTESIAN_POINT ( 'NONE',  ( 1.487047289068929246, 2.092300142875534341, 0.5796043027312002272 ) ) ;
#206661 = CARTESIAN_POINT ( 'NONE',  ( 0.6086344939593493208, -0.2706599535906920040, 1.821105742621460744 ) ) ;
#206660 = CARTESIAN_POINT ( 'NONE',  ( -5.043269954603569083, 7.867270132804026872, 1.082531754730560403 ) ) ;
#206662 = EDGE_CURVE ( 'NONE', #102037, #169596, #116854, .T. ) ;
#206663 = CARTESIAN_POINT ( 'NONE',  ( 1.364683531249988757, 2.134375000341422357, 1.214306433183764966E-14 ) ) ;
#206664 = CARTESIAN_POINT ( 'NONE',  ( 3.386445149735781257, -0.4294187885149694517, -2.148908265708626697 ) ) ;
#206665 = CARTESIAN_POINT ( 'NONE',  ( 6.076298462418691315, 7.128931413452940014, -1.143247356662546732 ) ) ;
#206666 = CARTESIAN_POINT ( 'NONE',  ( 3.379979430277161079, 1.433683275776801214, 1.750306659111708463 ) ) ;
#206667 = CARTESIAN_POINT ( 'NONE',  ( -6.938021921891187382, 9.117444880338284818, -1.599625672291263179 ) ) ;
#206668 = CARTESIAN_POINT ( 'NONE',  ( 4.628138809701114020, 2.011451458044950069, 0.1435230606586651581 ) ) ;
#206669 = CARTESIAN_POINT ( 'NONE',  ( 0.6823417656249917140, 4.405208333674755394, 1.181850606188765695 ) ) ;
#206670 = CARTESIAN_POINT ( 'NONE',  ( 6.438112759045284683, 6.782534085545247393, 0.3978009605737874432 ) ) ;
#206671 = CARTESIAN_POINT ( 'NONE',  ( -0.7500000000000006661, 12.20833333333333570, -1.299038105676657340 ) ) ;
#206672 = CARTESIAN_POINT ( 'NONE',  ( 5.560252395380206991, 7.580323442733986283, 1.443375672974065660 ) ) ;
#206673 = CARTESIAN_POINT ( 'NONE',  ( 3.901397652722672582, -0.5159380698404272270, 1.692823668428977912 ) ) ;
#206674 = TOROIDAL_SURFACE ( 'NONE', #75268, 0.8300000000000010703, 0.08000000000000000167 ) ;
#206675 = CARTESIAN_POINT ( 'NONE',  ( 6.584456157731144899, 10.83361595066169514, -0.7998128361456291469 ) ) ;
#206676 = CARTESIAN_POINT ( 'NONE',  ( 1.219907122830860446, -2.054670964268051847, 0.4612076382107341277 ) ) ;
#206678 = CARTESIAN_POINT ( 'NONE',  ( -1.402160292154681736E-14, 1.837500000000019895, -1.732050807568863648 ) ) ;
#206677 = CARTESIAN_POINT ( 'NONE',  ( -0.6823417656250003738, 10.65104166700806765, 1.181850606188754593 ) ) ;
#206679 = CARTESIAN_POINT ( 'NONE',  ( 1.293335457286367784, -1.782033794834203766, 0.8390149815750718165 ) ) ;
#206680 = CARTESIAN_POINT ( 'NONE',  ( -4.146814880933400005, 5.931313009212638931, 1.599625672291270506 ) ) ;
#206681 = CARTESIAN_POINT ( 'NONE',  ( -0.5031024701319503079, 7.721748688245902770, -1.994341720826586561 ) ) ;
#206682 = EDGE_LOOP ( 'NONE', ( #159320, #1902, #53827, #84608, #192304 ) ) ;
#206683 = CARTESIAN_POINT ( 'NONE',  ( 6.751597309925441159, 9.860318714012938912, -1.082531754730537088 ) ) ;
#206684 = VECTOR ( 'NONE', #40204, 1000.000000000000000 ) ;
#206685 = CARTESIAN_POINT ( 'NONE',  ( 9.317477881089539338, 11.89347683273640932, 1.599625672291279388 ) ) ;
#206686 = CARTESIAN_POINT ( 'NONE',  ( 4.610133579271312954, -0.8000244862099057386, -1.691074300901610261 ) ) ;
#206687 = CARTESIAN_POINT ( 'NONE',  ( 4.715538499454675403, 4.395883092318884522, 1.214306433183764966E-14 ) ) ;
#206688 = ORIENTED_EDGE ( 'NONE', *, *, #111757, .T. ) ;
#206689 = CARTESIAN_POINT ( 'NONE',  ( 4.241125740018336643, -0.1978421677554068614, -2.060750949040678570 ) ) ;
#206690 = CARTESIAN_POINT ( 'NONE',  ( -0.6125000000000019318, 2.291666666666664298, 1.060881119635910252 ) ) ;
#206691 = EDGE_CURVE ( 'NONE', #213643, #62971, #128936, .T. ) ;
#206692 = CARTESIAN_POINT ( 'NONE',  ( -5.085717018457573957, 8.947437264926888290, 0.7216878364870267237 ) ) ;
#206693 = CARTESIAN_POINT ( 'NONE',  ( -2.494940289813118994, 3.447199233515649386, 11.73777120880565583 ) ) ;
#206694 = CARTESIAN_POINT ( 'NONE',  ( 8.535021395002688749, 9.916278701380017324, 1.199719254218462483 ) ) ;
#206695 = CARTESIAN_POINT ( 'NONE',  ( -8.157201976916404362, 12.66848607304450702, -0.7998128361456281477 ) ) ;
#206696 = CARTESIAN_POINT ( 'NONE',  ( 7.991605200612358573, 8.288237253661408843, 0.7998128361456281477 ) ) ;
#206697 = CARTESIAN_POINT ( 'NONE',  ( -4.953691873189081107, 6.621539441584240571, -1.250027308714734664 ) ) ;
#206698 = CARTESIAN_POINT ( 'NONE',  ( 1.364683531249992088, 5.696875000341418804, 1.214306433183764966E-14 ) ) ;
#206699 = CIRCLE ( 'NONE', #113400, 2.750000000000008438 ) ;
#206700 = CARTESIAN_POINT ( 'NONE',  ( -1.500000000000015099, 0.3791666666666850261, -0.8660254037844383745 ) ) ;
#206701 = CARTESIAN_POINT ( 'NONE',  ( 4.439869198996494681, 1.279870211898268550, 1.486999339763886097 ) ) ;
#206702 = CARTESIAN_POINT ( 'NONE',  ( 1.616564310028177243, 0.5879328921069119085, -1.928455639302439462 ) ) ;
#206703 = LINE ( 'NONE', #128739, #72624 ) ;
#206704 = CARTESIAN_POINT ( 'NONE',  ( -11.35610322553117513, 9.985783710708231453, 3.553412924323500199 ) ) ;
#206705 = CARTESIAN_POINT ( 'NONE',  ( 6.639320575229252341, 0.005161017367553630275, 1.896863882003448021 ) ) ;
#206706 = CARTESIAN_POINT ( 'NONE',  ( 0.4911964603225346115, 1.381658100223854380, 1.261112594198803061 ) ) ;
#206707 = CARTESIAN_POINT ( 'NONE',  ( 1.364683531249990311, 4.613541667008083103, 0.7879004041258500513 ) ) ;
#206708 = CARTESIAN_POINT ( 'NONE',  ( 2.566654749391559687, 0.6821283815301434350, 1.894225559998161668 ) ) ;
#206710 = CARTESIAN_POINT ( 'NONE',  ( 3.409862312649377003, -1.263030510572001885, -1.699084664797428479 ) ) ;
#206709 = CARTESIAN_POINT ( 'NONE',  ( -5.395781948558855845, 9.238903340053241209, 0.7216878364870458196 ) ) ;
#206711 = CARTESIAN_POINT ( 'NONE',  ( 4.914543119725925280, 0.7892175071393169317, 1.914236960262293508 ) ) ;
#206712 = CARTESIAN_POINT ( 'NONE',  ( 6.210516883511641772, 9.403297576475722508, 1.199719254218452047 ) ) ;
#206714 = DIRECTION ( 'NONE',  ( 0.000000000000000000, 1.000000000000000000, 0.000000000000000000 ) ) ;
#206713 = CARTESIAN_POINT ( 'NONE',  ( 6.597611690090901426, -2.090214587215084130, 0.04977907537380765746 ) ) ;
#206716 = ORIENTED_EDGE ( 'NONE', *, *, #168698, .F. ) ;
#206715 = CARTESIAN_POINT ( 'NONE',  ( 5.631824825758743991, -1.159798792365024145, -1.409841961918213427 ) ) ;
#206717 = CARTESIAN_POINT ( 'NONE',  ( 8.076906825439115423, 10.44614393447756129, -1.599625672291262513 ) ) ;
#206718 = CARTESIAN_POINT ( 'NONE',  ( -1.579999999999998073, 6.280000000000042881, -2.499999999999995115 ) ) ;
#206719 = CARTESIAN_POINT ( 'NONE',  ( -11.97929049433705728, 13.80000000000000071, 0.7046979865771805240 ) ) ;
#206720 = CARTESIAN_POINT ( 'NONE',  ( -10.14895191633106819, 2.999999999999999112, 7.601392964450658596 ) ) ;
#206722 =( BOUNDED_CURVE ( )  B_SPLINE_CURVE ( 2, ( #192021, #209329, #48734, #159542, #157428, #91367, #60977 ),
 .UNSPECIFIED., .F., .T. ) 
 B_SPLINE_CURVE_WITH_KNOTS ( ( 3, 2, 2, 3 ),
 ( 0.2678571428571428492, 0.2738095238095239470, 0.2797619047619049337, 0.2857142857142859760 ),
 .UNSPECIFIED. ) 
 CURVE ( )  GEOMETRIC_REPRESENTATION_ITEM ( )  RATIONAL_B_SPLINE_CURVE ( ( 1.000000000000000000, 0.8660254037844387076, 1.000000000000000000, 0.8660254037844387076, 1.000000000000000000, 0.8660254037844324904, 1.000000000000006217 ) ) 
 REPRESENTATION_ITEM ( '' )  );
#206721 = CARTESIAN_POINT ( 'NONE',  ( -1.402160292154681736E-14, 11.48437500034139980, 1.575800808251682339 ) ) ;
#206723 = CARTESIAN_POINT ( 'NONE',  ( 5.725241913846256914, 1.688569718951500986, 0.8975008795490189151 ) ) ;
#206724 = CARTESIAN_POINT ( 'NONE',  ( -7.621654909176601045, 12.04368116068139472, 0.7998128361456481317 ) ) ;
#206725 = CARTESIAN_POINT ( 'NONE',  ( 7.145310649601935182, 8.294949498412453437, -1.199719254218446718 ) ) ;
#206726 = CARTESIAN_POINT ( 'NONE',  ( -3.755786496842899057E-14, 2.609375000341406459, -1.570758158831778273 ) ) ;
#206727 = CARTESIAN_POINT ( 'NONE',  ( 4.338245966248566177, 4.163634503485842409, 1.214306433183764966E-14 ) ) ;
#206728 = CYLINDRICAL_SURFACE ( 'NONE', #6278, 1.850000000000000089 ) ;
#206729 = CARTESIAN_POINT ( 'NONE',  ( 3.486418057008484617, 7.219238166485217434, 1.040834085586084257E-14 ) ) ;
#206730 = EDGE_LOOP ( 'NONE', ( #172450, #162693, #131368, #148021, #160821, #168999, #108200, #41322 ) ) ;
#206731 = CARTESIAN_POINT ( 'NONE',  ( -7.449279056065764237, 7.655523418356991350, 0.7998128361456341429 ) ) ;
#206732 = CARTESIAN_POINT ( 'NONE',  ( 5.237907724141787291, 2.013986247903374327, -0.1017665992488273330 ) ) ;
#206733 = CARTESIAN_POINT ( 'NONE',  ( -0.07933191607319768635, -9.582912294610101966, -9.499668754598335596 ) ) ;
#206734 = CARTESIAN_POINT ( 'NONE',  ( -0.3868823266961807228, 2.515145635913766053, 11.70808416779825478 ) ) ;
#206735 = CARTESIAN_POINT ( 'NONE',  ( 0.000000000000000000, -7.473374494045017968, 9.579665964948883783 ) ) ;
#206736 = CARTESIAN_POINT ( 'NONE',  ( -4.446711195602239819, 8.131654128270509929, -0.7216878364870267237 ) ) ;
#206737 = CARTESIAN_POINT ( 'NONE',  ( 10.23604278863759909, 11.04439746293979496, 0.000000000000000000 ) ) ;
#206738 = CARTESIAN_POINT ( 'NONE',  ( 2.061320199224637051, 1.634538341387161475, 1.098309876814192565 ) ) ;
#206739 = CARTESIAN_POINT ( 'NONE',  ( 3.269157808572686896, 1.821735364950356484, -0.8647411805496332260 ) ) ;
#206740 = CARTESIAN_POINT ( 'NONE',  ( -7.182068686937172153, 9.402166106225269715, 1.599625672291283607 ) ) ;
#206741 = CARTESIAN_POINT ( 'NONE',  ( 6.827182134110239886, 1.995248472151121444, 2.590158597942037844 ) ) ;
#206742 = CARTESIAN_POINT ( 'NONE',  ( 3.785266741157941262, 1.586943040539133154, 1.511552532079393885 ) ) ;
#206743 = CARTESIAN_POINT ( 'NONE',  ( 1.532927541463139365, 1.041115454748538172, 1.384885517283059420 ) ) ;
#206744 = CARTESIAN_POINT ( 'NONE',  ( 2.256748493264736588, -1.490592131378381646, 1.220310119380305203 ) ) ;
#206745 = CARTESIAN_POINT ( 'NONE',  ( -7.323375529675950624, 11.69568855126397011, -0.7998128361456291469 ) ) ;
#206746 = FILL_AREA_STYLE_COLOUR ( '', #162537 ) ;
#206747 = CARTESIAN_POINT ( 'NONE',  ( 0.2329586101569866563, 0.008238550247445517935, -1.845944905557160398 ) ) ;
#206748 = DIRECTION ( 'NONE',  ( 0.000000000000000000, 1.000000000000000000, 0.000000000000000000 ) ) ;
#206749 = CARTESIAN_POINT ( 'NONE',  ( 8.067265095331215718, 9.370563018429956870, 1.199719254218462483 ) ) ;
#206750 = CARTESIAN_POINT ( 'NONE',  ( 5.015626762051672571, 7.938982758113895422, 1.199719254218462483 ) ) ;
#206751 = CARTESIAN_POINT ( 'NONE',  ( -11.41381675112453387, 10.89999999999998259, 3.704697986577180746 ) ) ;
#206752 = CARTESIAN_POINT ( 'NONE',  ( 5.397554552016216256, 7.390509292142662723, 1.443375672974065660 ) ) ;
#206754 = CARTESIAN_POINT ( 'NONE',  ( 3.299479658734363330, 1.818928663852859451, -0.8628815382619985375 ) ) ;
#206753 = CARTESIAN_POINT ( 'NONE',  ( 6.339398910184078417, 0.6979989802004606947, -1.704029730133400866 ) ) ;
#206755 = CARTESIAN_POINT ( 'NONE',  ( 4.534687899768989006, 2.230887184458398398, -0.5525863250545393068 ) ) ;
#206757 = CARTESIAN_POINT ( 'NONE',  ( 3.168646232094144199, 1.351176984073151788, -1.279899388936973192 ) ) ;
#206756 = CARTESIAN_POINT ( 'NONE',  ( -0.1288028175206621384, 0.6694653996850441491, -2.353626493485785343 ) ) ;
#206758 = CARTESIAN_POINT ( 'NONE',  ( 6.933015448541703485, 9.181880338089085214, 1.599625672291268286 ) ) ;
#206759 = CARTESIAN_POINT ( 'NONE',  ( -0.1290005225502675879, 5.719648796287211567, -2.768066027128403217 ) ) ;
#206760 = CARTESIAN_POINT ( 'NONE',  ( -8.193204901359996128, 8.453160561208463264, 1.040834085586084257E-14 ) ) ;
#206761 = CARTESIAN_POINT ( 'NONE',  ( -3.689227196694346400, 6.357829925235092716, -1.082531754730546636 ) ) ;
#206762 = CARTESIAN_POINT ( 'NONE',  ( 5.724191925653110857, 2.015179739716387974, 0.5568145835738461669 ) ) ;
#206763 = CARTESIAN_POINT ( 'NONE',  ( 5.992340707560147806, 8.974519344586754599, 1.082531754730558626 ) ) ;
#206764 = DIRECTION ( 'NONE',  ( -1.000000000000000000, 0.000000000000000000, 0.000000000000000000 ) ) ;
#206766 = CARTESIAN_POINT ( 'NONE',  ( 3.734381245560244089, 6.444196322207211836, 1.199719254218462483 ) ) ;
#206765 = CARTESIAN_POINT ( 'NONE',  ( 8.776573235218638303, 13.27486625357122385, -8.183627694784497919 ) ) ;
#206767 = CARTESIAN_POINT ( 'NONE',  ( 6.692093555742618882, -0.7303567666399125580, 1.561414089659449944 ) ) ;
#206768 = CARTESIAN_POINT ( 'NONE',  ( -3.601662362724658895, 7.353689856487406473, -0.7998128361456281477 ) ) ;
#206769 = CARTESIAN_POINT ( 'NONE',  ( 1.529482971743981734, -1.465093928883187901, 0.9274137557628134854 ) ) ;
#206770 = CARTESIAN_POINT ( 'NONE',  ( -6.427974226210522168, 6.671927150099951298, 0.000000000000000000 ) ) ;
#206771 = CARTESIAN_POINT ( 'NONE',  ( 1.500000000000023981, 5.535416667349482012, 0.8660254037844334896 ) ) ;
#206772 = PRESENTATION_STYLE_ASSIGNMENT (( #140760 ) ) ;
#206773 = CARTESIAN_POINT ( 'NONE',  ( 6.121977192509519661, 2.140326789316211453, -0.3632143409003502077 ) ) ;
#206774 = CARTESIAN_POINT ( 'NONE',  ( 4.969292227364340953, 0.1756445257206709631, -1.817221496977147854 ) ) ;
#206775 = CARTESIAN_POINT ( 'NONE',  ( 1.674581101246939374, 1.321464807213859505, -1.450045219730737633 ) ) ;
#206776 = CARTESIAN_POINT ( 'NONE',  ( 4.000000000000012434, 4.999999999999997335, 0.7500000000000006661 ) ) ;
#206777 = CARTESIAN_POINT ( 'NONE',  ( -10.32861409551237486, 10.94447128771960287, 1.040834085586084257E-14 ) ) ;
#206778 = CARTESIAN_POINT ( 'NONE',  ( 6.889514614038635187, 11.18951748302043114, -0.7998128361456291469 ) ) ;
#206779 = EDGE_CURVE ( 'NONE', #94956, #155561, #207335, .T. ) ;
#206780 = CARTESIAN_POINT ( 'NONE',  ( 3.914780425095893968, -0.6665358524936614293, -2.013057630646164942 ) ) ;
#206781 = CARTESIAN_POINT ( 'NONE',  ( -2.657034918598345730, 5.083329257464595408, -1.082531754730543971 ) ) ;
#206782 = FACE_OUTER_BOUND ( 'NONE', #178966, .T. ) ;
#206783 = CARTESIAN_POINT ( 'NONE',  ( -4.885033903151685841, 6.706220529795296592, -1.250124166851230845 ) ) ;
#206785 = AXIS2_PLACEMENT_3D ( 'NONE', #159158, #63787, #195932 ) ;
#206784 = AXIS2_PLACEMENT_3D ( 'NONE', #8280, #170785, #139373 ) ;
#206786 = CARTESIAN_POINT ( 'NONE',  ( 2.289971195246335078, -1.349064171463711936, -1.570471239911851669 ) ) ;
#206788 = CARTESIAN_POINT ( 'NONE',  ( 0.6823417656249882723, -1.094791666325249713, 1.181850606188755259 ) ) ;
#206787 = CARTESIAN_POINT ( 'NONE',  ( -11.78331023100045627, 13.79999999999999893, -1.800000000000001155 ) ) ;
#206790 = ORIENTED_EDGE ( 'NONE', *, *, #19444, .T. ) ;
#206789 = CARTESIAN_POINT ( 'NONE',  ( 3.739129200393681796, 2.109584919444119855, 0.6958237802787976545 ) ) ;
#206791 = CARTESIAN_POINT ( 'NONE',  ( 2.040019973291283151, -1.774186676285171460, 1.461575674325124252 ) ) ;
#206793 = CARTESIAN_POINT ( 'NONE',  ( 6.157095870780715074, 1.689533437190817722, -1.182850423791491856 ) ) ;
#206792 = CARTESIAN_POINT ( 'NONE',  ( 9.408995418203971894, 11.03987807840189816, 1.082531754730549967 ) ) ;
#206795 = CARTESIAN_POINT ( 'NONE',  ( 0.000000000000000000, -4.046874999522043659, -3.793834371823813001 ) ) ;
#206794 = CARTESIAN_POINT ( 'NONE',  ( 5.578253857379852576, 5.472660686556754861, -0.7998128361456481317 ) ) ;
#206796 = CARTESIAN_POINT ( 'NONE',  ( 6.374545129912787544, -0.09763137639631430664, -1.838803627010993313 ) ) ;
#206797 = CARTESIAN_POINT ( 'NONE',  ( -5.750949863820874697, 6.097589008447164893, -0.6582294942717293873 ) ) ;
#206798 = CARTESIAN_POINT ( 'NONE',  ( -0.2104748580754426390, 2.865278511227668634, -2.591885361450113834 ) ) ;
#206799 = CARTESIAN_POINT ( 'NONE',  ( 3.399128784836574990, 1.359029604673635871, 1.061868196530877384 ) ) ;
#206800 = CARTESIAN_POINT ( 'NONE',  ( 1.921111612355221654, -1.799121770747251547, 0.9110121207814986244 ) ) ;
#206801 = CARTESIAN_POINT ( 'NONE',  ( 3.006738235175490548, -2.214768494356106121, 0.6152039052057678425 ) ) ;
#206802 = CARTESIAN_POINT ( 'NONE',  ( 3.269090859574837804, -2.088958473869072741, -0.8692115097446629912 ) ) ;
#206803 = CARTESIAN_POINT ( 'NONE',  ( 5.356126594405285601, 2.103725632816171309, -0.1020696835895683885 ) ) ;
#206804 = CARTESIAN_POINT ( 'NONE',  ( -6.834718835064852449, 8.106831741398025315, 1.082531754730549078 ) ) ;
#206805 = CARTESIAN_POINT ( 'NONE',  ( 3.778344457583324711, -1.704853921413415296, -0.4744283172272641957 ) ) ;
#206807 = CARTESIAN_POINT ( 'NONE',  ( 6.339416484298314280, 0.8816828672218860463, -2.116228320707528976 ) ) ;
#206806 = CARTESIAN_POINT ( 'NONE',  ( 3.079110283634975964, 6.606396074300548982, 0.7216878364870257245 ) ) ;
#206808 = CARTESIAN_POINT ( 'NONE',  ( 5.490138966579363178, -0.4511402564183407127, -1.784887083484905768 ) ) ;
#206809 = CARTESIAN_POINT ( 'NONE',  ( -2.937312835655025101, 6.578615408239493867, 1.040834085586084257E-14 ) ) ;
#206810 = CARTESIAN_POINT ( 'NONE',  ( -0.7500000000000006661, 2.858333333333358706, -1.299038105676652011 ) ) ;
#206811 = CARTESIAN_POINT ( 'NONE',  ( 5.332042502257137606, 2.158596015244533373, 0.3771327725019049670 ) ) ;
#206812 = CARTESIAN_POINT ( 'NONE',  ( -4.406563619641430840, 5.099744630125142564, -1.199719254218446718 ) ) ;
#206813 = CARTESIAN_POINT ( 'NONE',  ( -0.8446225718669002624, 15.51843453237083459, 12.00404876522673447 ) ) ;
#206814 = CARTESIAN_POINT ( 'NONE',  ( 6.408651866624735405, 0.6456447432892989946, 1.967203394946090977 ) ) ;
#206815 = CARTESIAN_POINT ( 'NONE',  ( 0.1457207355009884908, 1.993892511249679034, -0.3006540981884687214 ) ) ;
#206816 = AXIS2_PLACEMENT_3D ( 'NONE', #12775, #144968, #59416 ) ;
#206817 = CARTESIAN_POINT ( 'NONE',  ( 1.364683531249990311, 5.113541667008084879, 0.7879004041258500513 ) ) ;
#206818 = CARTESIAN_POINT ( 'NONE',  ( 3.949766350991973596, 0.6478974803514454539, -1.814415559773856490 ) ) ;
#206819 = CARTESIAN_POINT ( 'NONE',  ( -1.402160292154681736E-14, 10.92187500034139802, 1.575800808251682339 ) ) ;
#206820 = CARTESIAN_POINT ( 'NONE',  ( -2.331639231870358930, 5.664070170583284103, -0.7216878364870267237 ) ) ;
#206821 = CARTESIAN_POINT ( 'NONE',  ( 6.469000917296717112, -1.638331675554663747, 1.346054232038436105 ) ) ;
#206823 = ORIENTED_EDGE ( 'NONE', *, *, #147049, .F. ) ;
#206822 = CARTESIAN_POINT ( 'NONE',  ( -3.609978820808566802, 4.211641957610042120, -7.499999999999991118 ) ) ;
#206825 = CARTESIAN_POINT ( 'NONE',  ( 7.960204194457795477E-16, 0.4330127018922214077, -6.500000000000000000 ) ) ;
#206824 = CARTESIAN_POINT ( 'NONE',  ( -4.665414256878304577, 5.575976400180357118, -1.082531754730549967 ) ) ;
#206826 = CARTESIAN_POINT ( 'NONE',  ( 4.325214697959421706, 5.004837554829479451, 1.199719254218462483 ) ) ;
#206827 = SURFACE_STYLE_USAGE ( .BOTH. , #11823 ) ;
#206828 = DIRECTION ( 'NONE',  ( -1.207943261119674327E-30, -2.168404344971008079E-15, -1.000000000000000000 ) ) ;
#206829 = CARTESIAN_POINT ( 'NONE',  ( 11.47058495203700623, 8.376874303918512510, -3.372313987538385405 ) ) ;
#206830 = DIRECTION ( 'NONE',  ( 0.000000000000000000, 1.000000000000000000, 0.000000000000000000 ) ) ;
#206832 = CARTESIAN_POINT ( 'NONE',  ( 1.346068015636435522, -0.8851805579040676886, 1.750911360861057142 ) ) ;
#206831 = CIRCLE ( 'NONE', #110128, 10.91999999999999105 ) ;
#206833 = CARTESIAN_POINT ( 'NONE',  ( -0.6823417656250003738, 1.530208333674752730, -1.181850606188749264 ) ) ;
#206834 = DIRECTION ( 'NONE',  ( -1.000000000000000000, 5.578564026256503701E-16, 1.479114197289397135E-31 ) ) ;
#206835 = CARTESIAN_POINT ( 'NONE',  ( 5.178158156489047315, -1.047961880893449882, -1.658324637040713867 ) ) ;
#206836 = CARTESIAN_POINT ( 'NONE',  ( -8.995998617867369873, 10.45408546138876993, 1.199719254218462483 ) ) ;
#206837 = CARTESIAN_POINT ( 'NONE',  ( -5.002595493318215070, 7.819816594637776674, 1.082531754730560403 ) ) ;
#206838 = CARTESIAN_POINT ( 'NONE',  ( 6.825078400183575589, -0.005632053428735600553, 2.144262460745151255 ) ) ;
#206840 = ORIENTED_EDGE ( 'NONE', *, *, #45988, .F. ) ;
#206839 = CARTESIAN_POINT ( 'NONE',  ( 0.3999999999999889200, 3.372708439410121439, -0.5000000000000368594 ) ) ;
#206842 = EDGE_CURVE ( 'NONE', #177962, #214172, #93617, .T. ) ;
#206841 = CARTESIAN_POINT ( 'NONE',  ( -1.201851678989727383E-14, 5.196875000341422357, -1.575800808251660134 ) ) ;
#206843 = CARTESIAN_POINT ( 'NONE',  ( 0.6670070365902281972, 0.1896921041569209765, -1.860926112923621201 ) ) ;
#206844 = CARTESIAN_POINT ( 'NONE',  ( 5.800041802258188106, -1.566351721726914725, 0.7437187281235900782 ) ) ;
#206846 = CARTESIAN_POINT ( 'NONE',  ( 3.579775959861815515, -1.078688530630707243, 1.907616655872627964 ) ) ;
#206845 = CARTESIAN_POINT ( 'NONE',  ( -4.757329562667670667E-14, 0.5781250003414447614, -1.570758158831812246 ) ) ;
#206847 = CARTESIAN_POINT ( 'NONE',  ( 4.366487424706978260, 1.084006333436113634, 2.037121594781437839 ) ) ;
#206848 = CARTESIAN_POINT ( 'NONE',  ( 0.4970371946629085769, 1.713755840317375601, -1.144362063176207922 ) ) ;
#206849 = CARTESIAN_POINT ( 'NONE',  ( 2.079929315299507753, -1.904492180933140322, -0.3787631973139488073 ) ) ;
#206850 = CARTESIAN_POINT ( 'NONE',  ( -3.890826896997578999, 7.483122446565064756, 0.7216878364870317197 ) ) ;
#206851 = CARTESIAN_POINT ( 'NONE',  ( 0.09321446940366702461, 13.36358420534790703, -1.376866309900354413 ) ) ;
#206852 = CARTESIAN_POINT ( 'NONE',  ( 5.431924468521282634, -2.068440459917933794, 0.4666711972392265650 ) ) ;
#206853 = SURFACE_STYLE_USAGE ( .BOTH. , #155991 ) ;
#206854 = CARTESIAN_POINT ( 'NONE',  ( 3.375625116643202972, -0.3961014713874110305, -1.976955985980306307 ) ) ;
#206855 = CARTESIAN_POINT ( 'NONE',  ( -4.351804119862249465, 7.060559992272473551, 1.082531754730560403 ) ) ;
#206856 = CARTESIAN_POINT ( 'NONE',  ( -7.228432174741334038, 8.462200954400218578, -1.199719254218452047 ) ) ;
#206857 = CARTESIAN_POINT ( 'NONE',  ( 7.913155211870404493, 12.38376484715752213, 0.7998128361456462443 ) ) ;
#206858 = CARTESIAN_POINT ( 'NONE',  ( 1.224926655537651676, -0.04696546880481740349, 1.825250005322680780 ) ) ;
#206859 = CARTESIAN_POINT ( 'NONE',  ( -6.798487682609798632, 6.896266815991691779, 0.7998128361456341429 ) ) ;
#206860 = DIRECTION ( 'NONE',  ( 8.638326563840814399E-31, -0.000000000000000000, 1.000000000000000000 ) ) ;
#206861 = CARTESIAN_POINT ( 'NONE',  ( -9.915825940873133959, 4.173851563286998356, 6.175246223022227809 ) ) ;
#206862 = ORIENTED_EDGE ( 'NONE', *, *, #92877, .T. ) ;
#206863 = CARTESIAN_POINT ( 'NONE',  ( 5.700091634879108859, -2.061077814751426818, -0.002399610236311285148 ) ) ;
#206864 = CARTESIAN_POINT ( 'NONE',  ( -5.763624699140874164, 8.777960344756069233, -1.082531754730549967 ) ) ;
#206865 = UNCERTAINTY_MEASURE_WITH_UNIT (LENGTH_MEASURE( 1.000000000000000082E-05 ), #5118, 'distance_accuracy_value', 'NONE');
#206866 = CARTESIAN_POINT ( 'NONE',  ( 5.980555156959511898, 9.991415093179179863, -0.7216878364870458196 ) ) ;
#206867 = CARTESIAN_POINT ( 'NONE',  ( -4.790108344329849110, 4.482881244673243337, 0.7998128361456341429 ) ) ;
#206868 = CARTESIAN_POINT ( 'NONE',  ( -3.923105346307911745, 5.670318552149568703, -1.599625672291283607 ) ) ;
#206869 = CARTESIAN_POINT ( 'NONE',  ( 4.371743357251212103, 0.4404049503993580639, -1.970906944672585315 ) ) ;
#206870 = CARTESIAN_POINT ( 'NONE',  ( 5.725276803944279180, 1.957897222332797504, 1.049153726691682831 ) ) ;
#206871 = STYLED_ITEM ( 'NONE', ( #23629 ), #39092 ) ;
#206873 = CARTESIAN_POINT ( 'NONE',  ( 7.890482213473377193, 11.18901776815221716, -1.082531754730543083 ) ) ;
#206872 = CARTESIAN_POINT ( 'NONE',  ( -3.654804927335652209, 6.421633627603656080, 1.199719254218452935 ) ) ;
#206874 = CARTESIAN_POINT ( 'NONE',  ( 4.482942347612929979, 8.381849838857084123, 1.040834085586084257E-14 ) ) ;
#206875 = CARTESIAN_POINT ( 'NONE',  ( 3.661055773700711224, -1.816817347422092555, -0.9728634070030485193 ) ) ;
#206876 = CARTESIAN_POINT ( 'NONE',  ( 3.498672800139957406, -1.986100699840901651, 0.3474671148789992836 ) ) ;
#206877 = VERTEX_POINT ( 'NONE', #206260 ) ;
#206878 = CARTESIAN_POINT ( 'NONE',  ( 4.813308228051395687, 5.574280006603454574, 1.199719254218462483 ) ) ;
#206880 = ORIENTED_EDGE ( 'NONE', *, *, #206146, .T. ) ;
#206879 = CARTESIAN_POINT ( 'NONE',  ( -5.582925393777276035, 9.735439736040634173, 0.7998128361456291469 ) ) ;
#206881 = CARTESIAN_POINT ( 'NONE',  ( 4.937886321289528979, 7.980522944944189234, -1.013380012275147291 ) ) ;
#206882 = CARTESIAN_POINT ( 'NONE',  ( 3.866564406427867251, -0.5879305547937460075, 1.928456347981069019 ) ) ;
#206883 = CARTESIAN_POINT ( 'NONE',  ( 2.238008233095424515, 0.4029187984595939409, 1.796341404040911804 ) ) ;
#206884 = CARTESIAN_POINT ( 'NONE',  ( 1.032322977361863847, -1.467698275133515695, -1.780829215104979157 ) ) ;
#206885 = CARTESIAN_POINT ( 'NONE',  ( 3.627688620108284745, 6.389997935838436227, 1.199719254218452047 ) ) ;
#206886 = CARTESIAN_POINT ( 'NONE',  ( 3.532649767544591590, 2.108058052951222283, 0.4773693597190583060 ) ) ;
#206887 = STYLED_ITEM ( 'NONE', ( #11435 ), #46551 ) ;
#206888 = CARTESIAN_POINT ( 'NONE',  ( -4.713430959045263435, 8.650753218861462202, 0.7998128361456481317 ) ) ;
#206889 = CARTESIAN_POINT ( 'NONE',  ( 3.392261881094984055, 0.05328783134446976599, 2.297904267588930960 ) ) ;
#206890 = EDGE_LOOP ( 'NONE', ( #162559, #89513, #137925, #34357 ) ) ;
#206891 = FACE_OUTER_BOUND ( 'NONE', #94305, .T. ) ;
#206892 = CARTESIAN_POINT ( 'NONE',  ( 2.781945002432617997, -0.9632652739061451364, 1.603442845774772474 ) ) ;
#206893 = CARTESIAN_POINT ( 'NONE',  ( 5.594591524781380443, -0.4782570758292312707, -1.912467619381743811 ) ) ;
#206895 = CARTESIAN_POINT ( 'NONE',  ( 9.883530794237934458, 10.63313346947350269, -0.7216878364870257245 ) ) ;
#206894 = CARTESIAN_POINT ( 'NONE',  ( -1.364683531250010295, 5.030208333674757171, 0.7879004041258379498 ) ) ;
#206897 = CARTESIAN_POINT ( 'NONE',  ( 0.2060869173217265982, -0.5842117877600698783, 2.128085570573131413 ) ) ;
#206896 = CARTESIAN_POINT ( 'NONE',  ( -5.412729640353771465, 7.337937218544611895, 1.599625672291269396 ) ) ;
#206898 = CARTESIAN_POINT ( 'NONE',  ( -3.797692425159308716, 7.444741906078900406, 0.000000000000000000 ) ) ;
#206899 = CARTESIAN_POINT ( 'NONE',  ( 5.854423403002611437, 5.724582146458163656, 1.040834085586084257E-14 ) ) ;
#206900 = CARTESIAN_POINT ( 'NONE',  ( -5.494078562035765501, 7.432844293840273231, -1.599625672291256295 ) ) ;
#206901 = CARTESIAN_POINT ( 'NONE',  ( 0.2999999999999758415, 3.214163249644268472, 0.5238375172406799507 ) ) ;
#206902 = CARTESIAN_POINT ( 'NONE',  ( 6.438353018038387887, 1.949953777973761015, 0.2897296601065552091 ) ) ;
#206903 = CARTESIAN_POINT ( 'NONE',  ( 5.408889320884306073, 1.750735854880939746, -1.503546334452151134 ) ) ;
#206904 = CARTESIAN_POINT ( 'NONE',  ( 5.617585446245374037, 0.3627780356338809464, -1.825160902907280613 ) ) ;
#206905 = CARTESIAN_POINT ( 'NONE',  ( 2.852447711054075796, -2.056726475855717773, -0.1563953359742433491 ) ) ;
#206906 = CARTESIAN_POINT ( 'NONE',  ( 6.697364695470787943, 7.876308901879812474, -1.082531754730543083 ) ) ;
#206907 = CARTESIAN_POINT ( 'NONE',  ( 6.994027139803230320, 9.253060644560830994, -1.599625672291267398 ) ) ;
#206908 =( BOUNDED_CURVE ( )  B_SPLINE_CURVE ( 2, ( #118381, #102072, #168137, #106392, #21846, #186511, #155096, #41366, #91180 ),
 .UNSPECIFIED., .F., .T. ) 
 B_SPLINE_CURVE_WITH_KNOTS ( ( 3, 2, 2, 2, 3 ),
 ( 0.5089285714285713969, 0.5119047619047618625, 0.5178571428571429047, 0.5238095238095238360, 0.5267857142857143016 ),
 .UNSPECIFIED. ) 
 CURVE ( )  GEOMETRIC_REPRESENTATION_ITEM ( )  RATIONAL_B_SPLINE_CURVE ( ( 0.9330127018922194093, 0.9330127018922194093, 1.000000000000000000, 0.8660254037844387076, 1.000000000000000000, 0.8660254037844387076, 1.000000000000000000, 0.9330127018922194093, 0.9330127018922194093 ) ) 
 REPRESENTATION_ITEM ( '' )  );
#206909 = CARTESIAN_POINT ( 'NONE',  ( 7.754900676892376055, 8.149731665903665601, 1.040834085586084257E-14 ) ) ;
#206910 = CARTESIAN_POINT ( 'NONE',  ( -1.364683531250012516, 3.092708333674755838, 0.7879004041258379498 ) ) ;
#206911 = CARTESIAN_POINT ( 'NONE',  ( -11.04536101718726293, 12.69999999999999929, -1.100000000000000311 ) ) ;
#206912 = CARTESIAN_POINT ( 'NONE',  ( 6.290620086616457662, 6.441404310581745563, 1.040834085586084257E-14 ) ) ;
#206913 = CARTESIAN_POINT ( 'NONE',  ( 4.914598841593178946, 0.8265366316180179362, 2.007889688367751724 ) ) ;
#206914 = DIRECTION ( 'NONE',  ( 0.7592566023653005702, 0.6507913734559639396, 0.000000000000000000 ) ) ;
#206916 = CARTESIAN_POINT ( 'NONE',  ( 3.544333174469185721, -1.503253232081468216, 1.062929765333266108 ) ) ;
#206915 = CARTESIAN_POINT ( 'NONE',  ( -2.765500147507697459, 5.209872024525476597, 1.082531754730560403 ) ) ;
#206917 = ADVANCED_FACE ( 'NONE', ( #122990 ), #41666, .T. ) ;
#206919 = CARTESIAN_POINT ( 'NONE',  ( 9.579665964948882007, -7.473374494045003757, 1.734723475976807094E-15 ) ) ;
#206918 = DIRECTION ( 'NONE',  ( -1.000000000000000000, 0.000000000000000000, 0.000000000000000000 ) ) ;
#206920 = CARTESIAN_POINT ( 'NONE',  ( 6.614806895146394972, -0.1608752592793839531, 2.155998228907447523 ) ) ;
#206921 = CARTESIAN_POINT ( 'NONE',  ( -3.059665831784952651E-14, 3.479999999999999538, 2.000000000000000000 ) ) ;
#206922 = CARTESIAN_POINT ( 'NONE',  ( 0.8083708232014105155, -2.251370329867402376, 0.2228818479251652163 ) ) ;
#206923 = CARTESIAN_POINT ( 'NONE',  ( -4.014048110574687911, 7.796590492392542870, 0.4333429611983550256 ) ) ;
#206924 = FACE_OUTER_BOUND ( 'NONE', #106977, .T. ) ;
#206925 = CARTESIAN_POINT ( 'NONE',  ( 6.604365638557201379, 6.767254738080503706, -0.09251035838216993545 ) ) ;
#206926 = CARTESIAN_POINT ( 'NONE',  ( -4.245111494410291897, 7.006361605903701495, 1.082531754730549967 ) ) ;
#206927 = CARTESIAN_POINT ( 'NONE',  ( -0.07574839183086683192, -0.8175154495408327726, -1.727131953450977253 ) ) ;
#206928 = CARTESIAN_POINT ( 'NONE',  ( 0.9711603072033472284, 1.707112214499702407, -0.4667758381974375648 ) ) ;
#206930 = CARTESIAN_POINT ( 'NONE',  ( 5.391275966583902957, -0.05175381893108904618, -2.012593086484148142 ) ) ;
#206929 = CIRCLE ( 'NONE', #72090, 0.07999999999999948819 ) ;
#206931 = CARTESIAN_POINT ( 'NONE',  ( 5.250031796989762967, 7.148123067953287446, 1.599625672291267398 ) ) ;
#206932 = CARTESIAN_POINT ( 'NONE',  ( 4.225680580359360228, -2.015911352056736661, 0.6092541954213681610 ) ) ;
#206934 = CARTESIAN_POINT ( 'NONE',  ( 3.796418445691573940, 1.352171417773648132, -1.357169225504866406 ) ) ;
#206933 = CARTESIAN_POINT ( 'NONE',  ( -3.972175818679615222, 4.696921878956699103, 1.082531754730558626 ) ) ;
#206935 = CARTESIAN_POINT ( 'NONE',  ( -0.02244404828160087226, 0.2256878572204877031, -2.222431841814066278 ) ) ;
#206936 = CARTESIAN_POINT ( 'NONE',  ( 4.088306882321583124, 1.055547913133596749, -1.662622193200061771 ) ) ;
#206937 = CARTESIAN_POINT ( 'NONE',  ( 5.220965578766386450, 1.526617224004393369, -1.322549803791906786 ) ) ;
#206938 = CARTESIAN_POINT ( 'NONE',  ( 2.694054421766533203, -1.865511834602461949, -0.1395888279770511053 ) ) ;
#206940 = ORIENTED_EDGE ( 'NONE', *, *, #100231, .F. ) ;
#206939 = CARTESIAN_POINT ( 'NONE',  ( 4.951616564603428472, 0.5366251361543332710, -1.639350107105986831 ) ) ;
#206942 = CARTESIAN_POINT ( 'NONE',  ( 4.039966587192259873, 5.736380323189513852, 1.443375672974062551 ) ) ;
#206941 = CARTESIAN_POINT ( 'NONE',  ( 2.491098823239074278, -0.3784457004711218042, -2.174036671264235387 ) ) ;
#206943 = CARTESIAN_POINT ( 'NONE',  ( -1.364683531250012516, 2.801041667008090652, -0.7879004041258289570 ) ) ;
#206944 = CARTESIAN_POINT ( 'NONE',  ( 6.742638286788313451, -1.923764577213080029, -0.3838556375530403630 ) ) ;
#206945 = CARTESIAN_POINT ( 'NONE',  ( 8.749089199520284410, 9.101692242395490240, 0.7998128361456481317 ) ) ;
#206946 = CARTESIAN_POINT ( 'NONE',  ( -8.805130697071332335, 12.36007068230351358, 1.199719254218462483 ) ) ;
#206947 = CARTESIAN_POINT ( 'NONE',  ( 10.50000000000000178, 13.39999999999998259, 3.599999999999999201 ) ) ;
#206948 = DIRECTION ( 'NONE',  ( -0.000000000000000000, -0.000000000000000000, 1.000000000000000000 ) ) ;
#206949 = CARTESIAN_POINT ( 'NONE',  ( -10.96785329849812562, -5.223431457505089526, 0.4373225248172959434 ) ) ;
#206951 = VECTOR ( 'NONE', #122942, 1000.000000000000000 ) ;
#206950 = AXIS2_PLACEMENT_3D ( 'NONE', #134372, #19499, #152714 ) ;
#206952 = CARTESIAN_POINT ( 'NONE',  ( 1.680221237283368696, -1.148429780529091948, -1.722445320287042447 ) ) ;
#206953 = CARTESIAN_POINT ( 'NONE',  ( -1.500000000000011324, 2.670833333333352044, 0.8660254037844403729 ) ) ;
#206954 = CARTESIAN_POINT ( 'NONE',  ( 5.666418135507635512, 8.698239360479199433, 1.199719254218462483 ) ) ;
#206955 = CARTESIAN_POINT ( 'NONE',  ( 3.715816618597135523, 6.492813934075403637, -1.199719254218453823 ) ) ;
#206956 = CARTESIAN_POINT ( 'NONE',  ( 0.1529977018510132181, 0.3474608822290006782, 1.989397386523162226 ) ) ;
#206957 = CARTESIAN_POINT ( 'NONE',  ( 0.4019237886466847653, 10.35491455036742714, 1.499999999999997113 ) ) ;
#206958 = CARTESIAN_POINT ( 'NONE',  ( 1.364683531249988535, 3.613541667008086211, 0.7879004041258500513 ) ) ;
#206960 = CARTESIAN_POINT ( 'NONE',  ( 8.920901888111986366, 12.39117405523060889, 1.082531754730546636 ) ) ;
#206959 = DIRECTION ( 'NONE',  ( -0.9962287396576089415, -0.08676576675286086504, 0.000000000000000000 ) ) ;
#206961 = CARTESIAN_POINT ( 'NONE',  ( 5.061874962716293780, 1.677747168027879709, -1.117663061872615771 ) ) ;
#206962 = CARTESIAN_POINT ( 'NONE',  ( 5.120295473698084798, 1.888475294726537079, 0.3208887515022250669 ) ) ;
#206963 = DIRECTION ( 'NONE',  ( 0.000000000000000000, 1.000000000000000000, -8.546850786086437571E-32 ) ) ;
#206964 = CARTESIAN_POINT ( 'NONE',  ( 2.173600921376659834, 1.351110561487681716, 1.725424542402646422 ) ) ;
#206965 = CARTESIAN_POINT ( 'NONE',  ( -5.124618876285511604, 5.081069565195706517, 0.7216878364870705775 ) ) ;
#206966 = CARTESIAN_POINT ( 'NONE',  ( -1.201851678989727383E-14, 1.743750000682815493, 1.732050807568877637 ) ) ;
#206967 = CARTESIAN_POINT ( 'NONE',  ( 2.759904966095374501, 0.6844231338998980618, -1.785916880244736715 ) ) ;
#206968 = CARTESIAN_POINT ( 'NONE',  ( -5.717788096661253761, 7.693838750903348789, 1.599625672291269396 ) ) ;
#206970 = CARTESIAN_POINT ( 'NONE',  ( 0.4215001937674204280, -1.427952733550428288, -1.423947716221201976 ) ) ;
#206969 = CARTESIAN_POINT ( 'NONE',  ( -2.480778921620681921, 5.838066475291996404, 1.040834085586084257E-14 ) ) ;
#206971 = CARTESIAN_POINT ( 'NONE',  ( -1.402160292154681736E-14, 9.484375000341398021, 1.575800808251682339 ) ) ;
#206973 = CARTESIAN_POINT ( 'NONE',  ( -5.824109505522200081, 8.952488968821326054, -1.199719254218452047 ) ) ;
#206972 = CARTESIAN_POINT ( 'NONE',  ( 2.894169963053084160, -0.6095376172369629808, -1.999899515593931199 ) ) ;
#206975 = ORIENTED_EDGE ( 'NONE', *, *, #151857, .F. ) ;
#206974 = CARTESIAN_POINT ( 'NONE',  ( 1.992754126006650806, 1.502677205460640764, -0.8464738358340985203 ) ) ;
#206976 = DIRECTION ( 'NONE',  ( 0.000000000000000000, -1.000000000000000000, 0.000000000000000000 ) ) ;
#206977 = CARTESIAN_POINT ( 'NONE',  ( 5.473741331615251227, 7.409117525016355010, -1.599625672291262513 ) ) ;
#206978 = CARTESIAN_POINT ( 'NONE',  ( -0.5368768833858145184, 13.37576698399828246, -1.254641125003840507 ) ) ;
#206979 = CARTESIAN_POINT ( 'NONE',  ( -0.9311234436981447038, -2.478119629485602715, -3.475000000000004086 ) ) ;
#206980 = CARTESIAN_POINT ( 'NONE',  ( 5.721791708487565131, 5.640121512849101570, 0.3304596318965865587 ) ) ;
#206981 = CARTESIAN_POINT ( 'NONE',  ( 3.994848817520957773, 7.812407387083109001, 1.040834085586084257E-14 ) ) ;
#206982 = ORIENTED_EDGE ( 'NONE', *, *, #27605, .F. ) ;
#206983 = CARTESIAN_POINT ( 'NONE',  ( -11.84668730067608422, 13.40000000000000036, -1.400000000000001688 ) ) ;
#206984 = EDGE_LOOP ( 'NONE', ( #99782, #106916, #88778, #3473 ) ) ;
#206985 = CARTESIAN_POINT ( 'NONE',  ( 2.560951022220711248, -1.505102882618135629, 1.007669420338821675 ) ) ;
#206986 = VERTEX_POINT ( 'NONE', #23227 ) ;
#206987 = CARTESIAN_POINT ( 'NONE',  ( 3.246287715468270108, 5.874753870433235825, 1.199719254218450271 ) ) ;
#206988 = CARTESIAN_POINT ( 'NONE',  ( 5.520104819419390907, 6.469152373191302985, 1.199719254218452935 ) ) ;
#206989 = CARTESIAN_POINT ( 'NONE',  ( 4.037629478943724592, -1.732251659483119433, 0.5297805909155322013 ) ) ;
#206990 = DIRECTION ( 'NONE',  ( 1.000000000000000000, 0.000000000000000000, -1.478457507935129867E-17 ) ) ;
#206991 = DIRECTION ( 'NONE',  ( 5.828670879282089587E-16, -0.8656921114426509023, 0.5005768354468322912 ) ) ;
#206992 = CARTESIAN_POINT ( 'NONE',  ( 5.568360837313221623, 6.179671487343128433, 0.8958872440008452953 ) ) ;
#206993 = CIRCLE ( 'NONE', #155063, 1.500000000000000222 ) ;
#206995 = CARTESIAN_POINT ( 'NONE',  ( -8.012344526598182026E-15, 14.29687500034139802, -1.575800808251669460 ) ) ;
#206994 = CARTESIAN_POINT ( 'NONE',  ( 3.877287848637627210, -0.1385928533646582361, 1.855967808809717789 ) ) ;
#206996 = CARTESIAN_POINT ( 'NONE',  ( 1.001416299785270247, -1.868574072159228994, 0.4210543004025939506 ) ) ;
#206997 = CARTESIAN_POINT ( 'NONE',  ( 1.061231560844998034, 0.3605832424212577769, -1.789441408372116182 ) ) ;
#206998 = CARTESIAN_POINT ( 'NONE',  ( 4.742863741006460465, 8.194075573275554802, 0.7225937585536055252 ) ) ;
#206999 = DIRECTION ( 'NONE',  ( -0.000000000000000000, -1.000000000000000000, -0.000000000000000000 ) ) ;
#207000 = CARTESIAN_POINT ( 'NONE',  ( 5.355423173304108886, 7.585870477640591858, 1.239999553246450725 ) ) ;
#207001 = CARTESIAN_POINT ( 'NONE',  ( 7.576886519560940947, 14.99604748842864410, 10.16829559912798686 ) ) ;
#207002 = LINE ( 'NONE', #58633, #202142 ) ;
#207003 = CARTESIAN_POINT ( 'NONE',  ( -4.151108609992611775, 3.976305524690391113, 0.4518923928031730042 ) ) ;
#207004 = CARTESIAN_POINT ( 'NONE',  ( 7.212574532790092974, 9.437756259720353924, -1.443375672974057666 ) ) ;
#207005 = CARTESIAN_POINT ( 'NONE',  ( 5.383641442822343137, -1.871314765454759055, 0.6142198095173864170 ) ) ;
#207006 = CARTESIAN_POINT ( 'NONE',  ( -3.602716132929368875, 5.226254793216122074, 1.599625672291267398 ) ) ;
#207007 = CARTESIAN_POINT ( 'NONE',  ( -3.888022742048568681, 7.337601240860233354, -0.7289588026271909271 ) ) ;
#207008 = CARTESIAN_POINT ( 'NONE',  ( 0.8321122680391360715, 2.060015930055682620, 0.3555243805062404117 ) ) ;
#207009 = CARTESIAN_POINT ( 'NONE',  ( 6.387721611049761883, 1.328912806184729734, 1.394852177740999233 ) ) ;
#207010 = CARTESIAN_POINT ( 'NONE',  ( -5.904739593951539689, 6.847616600153594746, 1.199719254218450271 ) ) ;
#207011 = CARTESIAN_POINT ( 'NONE',  ( 1.746812667857342349, -1.544096848276183209, 0.9736100143667850704 ) ) ;
#207012 = CARTESIAN_POINT ( 'NONE',  ( 3.651171877326536030, -1.804458330144659950, 1.270265763067345066 ) ) ;
#207013 = CARTESIAN_POINT ( 'NONE',  ( 0.4019237886466778820, 9.854914550367428916, 1.500000000000001554 ) ) ;
#207014 = CARTESIAN_POINT ( 'NONE',  ( 0.6504702201592416078, 1.884490048413577368, 0.3244712162126031085 ) ) ;
#207015 = ORIENTED_EDGE ( 'NONE', *, *, #122495, .F. ) ;
#207016 = CARTESIAN_POINT ( 'NONE',  ( 1.047236342219150407, 1.738656489303032737, -0.9252727719080054980 ) ) ;
#207017 = CARTESIAN_POINT ( 'NONE',  ( 2.911592935152186090, -0.9596169164145462727, -1.688359700174842271 ) ) ;
#207018 = ORIENTED_EDGE ( 'NONE', *, *, #20246, .F. ) ;
#207019 = CARTESIAN_POINT ( 'NONE',  ( -1.115562610750309283E-14, 11.81250000000000000, 1.500000000000001554 ) ) ;
#207021 = CARTESIAN_POINT ( 'NONE',  ( 6.174622966819019787, 1.250768081284852951, -1.378062710742117059 ) ) ;
#207020 = CARTESIAN_POINT ( 'NONE',  ( -3.332271893908731464, 7.109677319527304640, -0.7998128361456481317 ) ) ;
#207022 = CARTESIAN_POINT ( 'NONE',  ( 3.901714345682657292, 7.774026846596938434, 0.7998128361456271485 ) ) ;
#207023 = CARTESIAN_POINT ( 'NONE',  ( -11.52469724861193967, 13.87999993351231254, -3.346365485506884063 ) ) ;
#207024 = CARTESIAN_POINT ( 'NONE',  ( -7.800371912476627756, -5.581885079358433366, -7.755938900619404386 ) ) ;
#207025 = CARTESIAN_POINT ( 'NONE',  ( -7.123883369337781879, 7.275895117174344229, 0.7998128361456341429 ) ) ;
#207026 = CARTESIAN_POINT ( 'NONE',  ( 2.595491417077447238, -0.6846416945752286098, 2.081959150545972914 ) ) ;
#207027 = SURFACE_STYLE_USAGE ( .BOTH. , #70604 ) ;
#207028 = AXIS2_PLACEMENT_3D ( 'NONE', #197858, #133977, #49490 ) ;
#207029 = CARTESIAN_POINT ( 'NONE',  ( 11.00057242252828260, -6.459673408256681348, -0.07917133907639190005 ) ) ;
#207030 = CARTESIAN_POINT ( 'NONE',  ( 11.41381675112453742, 19.00000000000000000, 3.704697986577180746 ) ) ;
#207031 = CARTESIAN_POINT ( 'NONE',  ( 3.246530741642670304, 0.4443377543969920795, 1.770662692542070538 ) ) ;
#207032 = DIRECTION ( 'NONE',  ( -0.000000000000000000, -1.000000000000000000, -0.000000000000000000 ) ) ;
#207033 = CARTESIAN_POINT ( 'NONE',  ( -8.500599126088349777, 12.86119004717103209, 1.040834085586084257E-14 ) ) ;
#207034 = CARTESIAN_POINT ( 'NONE',  ( -5.249610431062532889, 7.793670086080374482, -1.296690129572550365 ) ) ;
#207035 = DIRECTION ( 'NONE',  ( -0.000000000000000000, -1.000000000000000000, -0.000000000000000000 ) ) ;
#207036 = CARTESIAN_POINT ( 'NONE',  ( 8.052653171512838881, 11.48218023581863001, -1.199719254218446718 ) ) ;
#207037 = CARTESIAN_POINT ( 'NONE',  ( 0.6274103741727736772, -1.829744589303895275, 0.6030480328435404713 ) ) ;
#207038 = CARTESIAN_POINT ( 'NONE',  ( 5.875826477234549650, -1.914729252524836056, 0.4262945716600323731 ) ) ;
#207039 = AXIS2_PLACEMENT_3D ( 'NONE', #16434, #182137, #164842 ) ;
#207040 = CARTESIAN_POINT ( 'NONE',  ( -1.500000000000008216, 14.49999999999999822, 3.469446951953614189E-15 ) ) ;
#207041 = CARTESIAN_POINT ( 'NONE',  ( -7.446452682403657874, 9.710614100936176385, -1.599625672291263179 ) ) ;
#207042 = CARTESIAN_POINT ( 'NONE',  ( 5.332434488876471868, 5.115595079977664383, 0.7998128361456341429 ) ) ;
#207043 = EDGE_CURVE ( 'NONE', #29614, #162002, #56746, .T. ) ;
#207044 = CARTESIAN_POINT ( 'NONE',  ( -4.733205024502264102, 7.575804057677677505, 1.082531754730549967 ) ) ;
#207045 = DIRECTION ( 'NONE',  ( 0.000000000000000000, 1.000000000000000000, 0.000000000000000000 ) ) ;
#207046 = CARTESIAN_POINT ( 'NONE',  ( -1.420000000000001039, 6.280000000000042881, -2.499999999999995115 ) ) ;
#207047 = CARTESIAN_POINT ( 'NONE',  ( 5.612195314557796522, 2.068136773602911038, -0.09592777784667855245 ) ) ;
#207048 = CARTESIAN_POINT ( 'NONE',  ( -1.402160292154681736E-14, 2.259375000341416140, -1.575800808251660134 ) ) ;
#207049 = CARTESIAN_POINT ( 'NONE',  ( 5.045646660657260973, -1.666335398280174074, 1.583644221457411794 ) ) ;
#207050 = CARTESIAN_POINT ( 'NONE',  ( 7.782016984564065432, 8.181367358187307204, 0.7216878364870458196 ) ) ;
#207052 = DIRECTION ( 'NONE',  ( 0.7592566023652990159, -0.6507913734559659380, 0.000000000000000000 ) ) ;
#207051 = CARTESIAN_POINT ( 'NONE',  ( 4.990809943606266508, 6.915973915664348937, -1.443375672974068769 ) ) ;
#207053 = CARTESIAN_POINT ( 'NONE',  ( 0.04153208042980033321, -1.776208762584199574, -1.448543121555950774 ) ) ;
#207054 = CARTESIAN_POINT ( 'NONE',  ( -0.02890288085937701978, -9.971207159576024992, -9.579616049094559216 ) ) ;
#207055 = CARTESIAN_POINT ( 'NONE',  ( -7.262327558775498737, 8.501745569106741840, 1.199719254218452047 ) ) ;
#207056 = CARTESIAN_POINT ( 'NONE',  ( 4.365135538708351248, 1.883338149218495516, -0.4730343525067778332 ) ) ;
#207057 = ORIENTED_EDGE ( 'NONE', *, *, #140442, .T. ) ;
#207059 = EDGE_CURVE ( 'NONE', #52075, #15498, #77337, .T. ) ;
#207058 = CARTESIAN_POINT ( 'NONE',  ( 8.053180056393003383, 12.33920113252646367, 1.040834085586084257E-14 ) ) ;
#207060 = ORIENTED_EDGE ( 'NONE', *, *, #129145, .F. ) ;
#207061 = CARTESIAN_POINT ( 'NONE',  ( 6.258066496116281741, 0.7254575739856858885, -1.769658340881982816 ) ) ;
#207062 = CARTESIAN_POINT ( 'NONE',  ( 6.334932600541999470, 0.1746011871221597178, 1.715888227437605718 ) ) ;
#207063 = CARTESIAN_POINT ( 'NONE',  ( 5.612517632836663495, 1.944729323200469873, 0.5331731267440716904 ) ) ;
#207065 = CARTESIAN_POINT ( 'NONE',  ( 6.938893903907228378E-15, 10.64264068711930733, 1.214306433183764966E-14 ) ) ;
#207064 = CARTESIAN_POINT ( 'NONE',  ( -7.991641480251377772, 11.41099992934688956, 1.199719254218453823 ) ) ;
#207066 = CARTESIAN_POINT ( 'NONE',  ( -3.285556943750000070, -1.596874999522043037, 0.000000000000000000 ) ) ;
#207068 = CARTESIAN_POINT ( 'NONE',  ( 6.608682216863940084, 1.309337763449496705, -1.190854552318038051 ) ) ;
#207067 = CARTESIAN_POINT ( 'NONE',  ( 2.185595087713845697, -0.8928614526015861141, 1.890522631819052002 ) ) ;
#207069 = CARTESIAN_POINT ( 'NONE',  ( 5.608046130584797950, -0.04667949407829303371, 2.016033753796213635 ) ) ;
#207071 = CARTESIAN_POINT ( 'NONE',  ( 2.537429240164018385, -1.699656577751871289, -1.538240582240576693 ) ) ;
#207070 = CARTESIAN_POINT ( 'NONE',  ( 4.655245641445829641, 6.524482229810530498, 1.599625672291269396 ) ) ;
#207072 = CARTESIAN_POINT ( 'NONE',  ( 2.694910210795556260, -0.5461130550479543766, 1.652493440627414323 ) ) ;
#207073 = CARTESIAN_POINT ( 'NONE',  ( 5.900277318768097246, 7.249539301847896411, -1.301905728482563251 ) ) ;
#207074 = CARTESIAN_POINT ( 'NONE',  ( 1.897353599431324866, 0.1640088499204050976, 1.726041979094733447 ) ) ;
#207075 = CARTESIAN_POINT ( 'NONE',  ( 0.6801582343749900117, 1.588541667008100511, -1.178068619123890270 ) ) ;
#207076 = CARTESIAN_POINT ( 'NONE',  ( 1.873285555135986824, -0.2318667498520594894, 1.846494694648516788 ) ) ;
#207077 = CARTESIAN_POINT ( 'NONE',  ( 2.031898538270035637, 2.078123050159206286, -0.6288832818364347155 ) ) ;
#207078 = CARTESIAN_POINT ( 'NONE',  ( 3.819546216251490822, -1.394084564108012403, -1.457236891723237449 ) ) ;
#207079 = CARTESIAN_POINT ( 'NONE',  ( 3.875000000000003553, 2.052068128417946724, -2.337016516192933888E-13 ) ) ;
#207080 = AXIS2_PLACEMENT_3D ( 'NONE', #130687, #109102, #196677 ) ;
#207081 = CARTESIAN_POINT ( 'NONE',  ( -0.7500000000000006661, 2.389583334016155636, -1.299038105676652011 ) ) ;
#207082 = CARTESIAN_POINT ( 'NONE',  ( 1.237189336409921570, -1.742702465754492058, 0.8212270227533255973 ) ) ;
#207084 = B_SPLINE_CURVE_WITH_KNOTS ( 'NONE', 3,
 ( #185041, #87569, #152559, #5208, #7358, #38816, #21461 ),
 .UNSPECIFIED., .F., .F.,
 ( 4, 3, 4 ),
 ( 3.314949680323544927E-05, 0.0009000000012044580581, 0.001958074173707496923 ),
 .UNSPECIFIED. ) ;
#207083 = CARTESIAN_POINT ( 'NONE',  ( -1.364683531250014514, 14.83854166700806410, -0.7879004041258335089 ) ) ;
#207085 = CARTESIAN_POINT ( 'NONE',  ( 3.639129310729662503, 2.110331241038451822, 0.6939571745526812441 ) ) ;
#207086 = ORIENTED_EDGE ( 'NONE', *, *, #3092, .T. ) ;
#207087 = CARTESIAN_POINT ( 'NONE',  ( -1.394453263437886604E-15, 2.375000000682794266, 1.224999999999975220 ) ) ;
#207088 = CARTESIAN_POINT ( 'NONE',  ( -1.500000000000015099, 0.6291666666666863028, -0.8660254037844313801 ) ) ;
#207090 = ADVANCED_FACE ( 'NONE', ( #127251 ), #188948, .T. ) ;
#207089 = CARTESIAN_POINT ( 'NONE',  ( 6.913768267964901071, 10.15348118167935709, -1.199719254218441611 ) ) ;
#207091 = CARTESIAN_POINT ( 'NONE',  ( 1.364683531249986537, 0.1135416670080857532, 0.7879004041258500513 ) ) ;
#207092 = CARTESIAN_POINT ( 'NONE',  ( 5.959279902674206042, -1.877032357297861109, 1.187784507339540108 ) ) ;
#207093 = CARTESIAN_POINT ( 'NONE',  ( 4.650807877244386823, -0.4278111053654386486, -1.914496481071884970 ) ) ;
#207095 = CARTESIAN_POINT ( 'NONE',  ( -6.778713617152821058, 7.971215977175476475, 1.082531754730549967 ) ) ;
#207094 = CARTESIAN_POINT ( 'NONE',  ( 9.002250809793993724, 11.52571191622492464, -1.443375672974057666 ) ) ;
#207096 = CARTESIAN_POINT ( 'NONE',  ( -1.425126390603233428, 3.734596776778838390, -0.4909503797920832247 ) ) ;
#207097 = CARTESIAN_POINT ( 'NONE',  ( 5.554102117330329769, 2.260170762534471578, -0.1031424389980051676 ) ) ;
#207098 = CIRCLE ( 'NONE', #169069, 2.000000000000000000 ) ;
#207099 = CARTESIAN_POINT ( 'NONE',  ( -4.963693636378939011, 8.805076652501815815, 0.7216878364870267237 ) ) ;
#207100 = CARTESIAN_POINT ( 'NONE',  ( 2.102078608570765450, 0.7915390796853873923, -1.904948021121543711 ) ) ;
#207101 = CARTESIAN_POINT ( 'NONE',  ( -7.203459687562382641, 7.298457811777897319, -0.7998128361456291469 ) ) ;
#207102 = ORIENTED_EDGE ( 'NONE', *, *, #17820, .T. ) ;
#207104 = EDGE_CURVE ( 'NONE', #144299, #183707, #43801, .T. ) ;
#207103 = CARTESIAN_POINT ( 'NONE',  ( 1.499999999999989120, 2.556250000682817713, 1.214306433183764966E-14 ) ) ;
#207105 = CARTESIAN_POINT ( 'NONE',  ( -1.364683531249997417, 3.821875000341416584, 1.214306433183764966E-14 ) ) ;
#207106 = CARTESIAN_POINT ( 'NONE',  ( 4.253091631423633778, -1.553859266942819284, -1.041061106808522929 ) ) ;
#207107 = CARTESIAN_POINT ( 'NONE',  ( 3.094086244858067047, -0.3350832708051197373, 1.701246549458427015 ) ) ;
#207108 = CARTESIAN_POINT ( 'NONE',  ( 0.6270410820986601630, 0.1761543355088228957, 2.285679397864130102 ) ) ;
#207109 = CARTESIAN_POINT ( 'NONE',  ( 1.325528760500709780, -0.05309137938146882979, 2.206304558879538025 ) ) ;
#207110 = CARTESIAN_POINT ( 'NONE',  ( 4.124618644571789616, 0.1043759322204278750, 2.088280726629719197 ) ) ;
#207111 = CARTESIAN_POINT ( 'NONE',  ( 5.788998755281030029, 1.472039788614720290, 1.266697539889444446 ) ) ;
#207112 = EDGE_CURVE ( 'NONE', #119686, #214172, #127721, .T. ) ;
#207114 = VERTEX_POINT ( 'NONE', #192136 ) ;
#207113 = CARTESIAN_POINT ( 'NONE',  ( 0.000000000000000000, 4.000000000000002665, 1.105031132475055157E-32 ) ) ;
#207115 = PRESENTATION_STYLE_ASSIGNMENT (( #106477 ) ) ;
#207116 = CARTESIAN_POINT ( 'NONE',  ( 0.03578008775950020093, -1.617816776142148250, 1.203357013023528932 ) ) ;
#207117 = CARTESIAN_POINT ( 'NONE',  ( -0.05226516427493665962, -1.936187138999283297, 0.8653993394739032397 ) ) ;
#207118 = CARTESIAN_POINT ( 'NONE',  ( 2.449293598294706414E-16, 0.000000000000000000, 2.000000000000000000 ) ) ;
#207119 = CARTESIAN_POINT ( 'NONE',  ( -11.86145016429273014, 12.69999999999999929, -1.100000000000000311 ) ) ;
#207120 = CARTESIAN_POINT ( 'NONE',  ( -7.669108446824431269, 12.09904362127053545, -0.7998128361456291469 ) ) ;
#207121 = CARTESIAN_POINT ( 'NONE',  ( 5.960781091502512119, 10.10599504006161986, 0.7998128361456462443 ) ) ;
#207122 = DIRECTION ( 'NONE',  ( 0.000000000000000000, 0.8000000000040162762, -0.5999999999946449281 ) ) ;
#207123 = CARTESIAN_POINT ( 'NONE',  ( 3.949673224339702138, 0.6133576713117370183, -1.719707012317383432 ) ) ;
#207124 = CARTESIAN_POINT ( 'NONE',  ( 2.292262453775519404, -0.9438808975747980945, 1.994871701834355804 ) ) ;
#207125 = ORIENTED_EDGE ( 'NONE', *, *, #182709, .T. ) ;
#207126 = CARTESIAN_POINT ( 'NONE',  ( -8.093291352714894415, 8.406871097780989288, -0.7998128361456362523 ) ) ;
#207127 = CARTESIAN_POINT ( 'NONE',  ( -1.642778471875000035, -1.655208332855377051, -2.845375778867859751 ) ) ;
#207128 = CARTESIAN_POINT ( 'NONE',  ( -9.182950115157607840, 9.607863310639020327, 0.7998128361456462443 ) ) ;
#207129 = CARTESIAN_POINT ( 'NONE',  ( 1.582292005822239167, 1.041880795974026608, 1.730197787189115433 ) ) ;
#207130 = CARTESIAN_POINT ( 'NONE',  ( 1.050790385994986975, 15.00000000000000711, -12.64745918785790835 ) ) ;
#207131 = EDGE_LOOP ( 'NONE', ( #161900, #96760, #19050, #167234 ) ) ;
#207132 = CARTESIAN_POINT ( 'NONE',  ( -5.646044625448194410, 5.551749915969804938, 0.000000000000000000 ) ) ;
#207133 = CARTESIAN_POINT ( 'NONE',  ( 3.221387034570993624, 0.2776250501920934921, -1.840009301959115051 ) ) ;
#207134 = CARTESIAN_POINT ( 'NONE',  ( 2.367870383881045981, 5.914265881169853856, 0.000000000000000000 ) ) ;
#207135 = TOROIDAL_SURFACE ( 'NONE', #96471, 2.400000000000000355, 0.1000000000000000056 ) ;
#207136 = CARTESIAN_POINT ( 'NONE',  ( 0.000000000000000000, -2.856854249492362996, 0.000000000000000000 ) ) ;
#207137 = ORIENTED_EDGE ( 'NONE', *, *, #77201, .T. ) ;
#207138 = CARTESIAN_POINT ( 'NONE',  ( -5.525111292768871252, 6.404716915440499037, -1.199719254218446718 ) ) ;
#207139 = CARTESIAN_POINT ( 'NONE',  ( -8.402302512167102222, 10.82577223566020841, -1.599625672291263179 ) ) ;
#207140 = CARTESIAN_POINT ( 'NONE',  ( 4.371595934376539816, 1.770262903079304451, -0.4459408992859363319 ) ) ;
#207143 = EDGE_LOOP ( 'NONE', ( #73306, #76457, #115324, #2458 ) ) ;
#207142 = CARTESIAN_POINT ( 'NONE',  ( 1.467252801262404871, -3.037869857053148603, 3.165465571089816521 ) ) ;
#207141 = CARTESIAN_POINT ( 'NONE',  ( -6.064239847062411926, 10.29697326487330500, 0.000000000000000000 ) ) ;
#207144 = CARTESIAN_POINT ( 'NONE',  ( 6.098455030413784783, 7.112933956528650015, -1.126327413477963502 ) ) ;
#207145 = CARTESIAN_POINT ( 'NONE',  ( 6.819686488043297246, -1.560180513003786462, 1.276622200526676743 ) ) ;
#207146 = CARTESIAN_POINT ( 'NONE',  ( 5.261588992693945421, 0.9106475924270783784, 1.600083007495013643 ) ) ;
#207147 = CARTESIAN_POINT ( 'NONE',  ( 4.582853619701852566, -2.237698958467302823, -0.5636369891960175682 ) ) ;
#207148 = CARTESIAN_POINT ( 'NONE',  ( 5.391302360089590628, 6.318882837306503575, -1.199719254218452047 ) ) ;
#207149 = CARTESIAN_POINT ( 'NONE',  ( 0.4036811037357163623, -0.5522049309486184443, 1.985320814919430132 ) ) ;
#207150 = CARTESIAN_POINT ( 'NONE',  ( 7.820355676984174664, 8.018169799436671852, -0.7998128361456281477 ) ) ;
#207151 = VECTOR ( 'NONE', #213833, 1000.000000000000000 ) ;
#207152 = CARTESIAN_POINT ( 'NONE',  ( 5.642068729656325665, -0.04839715497878017969, -2.298027403377851385 ) ) ;
#207153 = CARTESIAN_POINT ( 'NONE',  ( -1.945698667645833879, -3.232243495192120619, 2.663941817279478208 ) ) ;
#207154 = CARTESIAN_POINT ( 'NONE',  ( -2.979759899953417612, 6.698413326579433225, 0.7998128361456352531 ) ) ;
#207155 = CARTESIAN_POINT ( 'NONE',  ( 6.016445890116215445, 1.255022122864515310, -1.387330985440645037 ) ) ;
#207156 = ORIENTED_EDGE ( 'NONE', *, *, #190135, .F. ) ;
#207158 = CARTESIAN_POINT ( 'NONE',  ( -4.773352600463090845, 7.726605912919016106, 1.199719254218452935 ) ) ;
#207157 = CARTESIAN_POINT ( 'NONE',  ( 2.144650067465687648, 1.855875215511919363, 0.4610605321611755958 ) ) ;
#207159 = CARTESIAN_POINT ( 'NONE',  ( 4.406973378220558679, 1.706932345810768359, -1.398813476408675260 ) ) ;
#207160 = CARTESIAN_POINT ( 'NONE',  ( 4.364542673910889015, -2.054697287276555873, -0.5108639600793271063 ) ) ;
#207161 = CARTESIAN_POINT ( 'NONE',  ( -1.752700365193352367E-14, 0.6250000006827908239, 1.414508159514579644 ) ) ;
#207162 = CARTESIAN_POINT ( 'NONE',  ( 6.883263157960368694, 4.693146704925188040, 2.608790034323371643 ) ) ;
#207163 = CARTESIAN_POINT ( 'NONE',  ( 4.651856102820254968, 7.480896982382013505, -1.082531754730548412 ) ) ;
#207164 = CARTESIAN_POINT ( 'NONE',  ( -5.167065940139584868, 6.161236697318522637, 1.082531754730549078 ) ) ;
#207165 = CARTESIAN_POINT ( 'NONE',  ( 2.362750734746793757, 0.9868518204677073635, 2.086042234993300770 ) ) ;
#207166 = CARTESIAN_POINT ( 'NONE',  ( 3.103904542773823660, 0.7086415210641981988, -1.829580771271981154 ) ) ;
#207167 = CARTESIAN_POINT ( 'NONE',  ( 11.48243876534946217, 11.29999999999998117, 3.199999999999997957 ) ) ;
#207168 = CARTESIAN_POINT ( 'NONE',  ( 6.719587945281444874, 0.3584770237896938716, -2.031047634367310284 ) ) ;
#207169 = CARTESIAN_POINT ( 'NONE',  ( 2.901081683644312736, 6.328419697652925002, 0.7216878364870338292 ) ) ;
#207170 = CARTESIAN_POINT ( 'NONE',  ( 4.065465959251388206, 5.836405933916976707, -1.599625672291269396 ) ) ;
#207171 = ORIENTED_EDGE ( 'NONE', *, *, #7685, .T. ) ;
#207172 = CARTESIAN_POINT ( 'NONE',  ( 4.909388789075159742, -1.913262893431907141, 0.6371506334161003426 ) ) ;
#207173 = CARTESIAN_POINT ( 'NONE',  ( -7.974166903131914452, 12.45494515362926435, -0.7998128361456281477 ) ) ;
#207174 = DIRECTION ( 'NONE',  ( -0.1470157664651973450, 0.7071067811865536790, 0.6916548014802195166 ) ) ;
#207175 = CARTESIAN_POINT ( 'NONE',  ( -10.45142907045522129, 5.144535043903895932, -5.216774619840575333 ) ) ;
#207176 = CARTESIAN_POINT ( 'NONE',  ( 2.507895228403643539, 5.869702166538802501, -0.7216878364870267237 ) ) ;
#207177 = CARTESIAN_POINT ( 'NONE',  ( 2.325261487346420797, -1.983500291700568852, -0.8831872222036639686 ) ) ;
#207178 = EDGE_CURVE ( 'NONE', #53708, #203895, #86849, .T. ) ;
#207179 = CARTESIAN_POINT ( 'NONE',  ( -4.385872067527455620, 14.53055287205049240, -11.17868682968782856 ) ) ;
#207180 = DIRECTION ( 'NONE',  ( 0.000000000000000000, 1.000000000000000000, 0.000000000000000000 ) ) ;
#207181 = CARTESIAN_POINT ( 'NONE',  ( 5.652821694808577213, 7.451312062667313718, 1.328372732707931103 ) ) ;
#207182 = AXIS2_PLACEMENT_3D ( 'NONE', #118296, #116162, #179 ) ;
#207183 = CARTESIAN_POINT ( 'NONE',  ( 1.159529407832321501, 0.4047576141815812378, -2.020457351226915055 ) ) ;
#207185 = FACE_OUTER_BOUND ( 'NONE', #24490, .T. ) ;
#207184 = FACE_OUTER_BOUND ( 'NONE', #140863, .T. ) ;
#207186 = CARTESIAN_POINT ( 'NONE',  ( -1.364683531250000748, 0.2593750003414205252, 0.000000000000000000 ) ) ;
#207187 = EDGE_LOOP ( 'NONE', ( #184941, #35646, #179807, #88063 ) ) ;
#207188 = CARTESIAN_POINT ( 'NONE',  ( 3.035702773332124238, -1.842316306609870891, 0.5122265333450184421 ) ) ;
#207189 = CARTESIAN_POINT ( 'NONE',  ( 4.785902253289605390, -0.8326956132961546020, 1.561725933240491360 ) ) ;
#207190 = CARTESIAN_POINT ( 'NONE',  ( 5.189738938980948291, 9.276722205444929870, 0.000000000000000000 ) ) ;
#207191 = CARTESIAN_POINT ( 'NONE',  ( -4.253507506385335368, 5.985511395581417204, 1.599625672291267398 ) ) ;
#207193 = CARTESIAN_POINT ( 'NONE',  ( 0.09280537598354164641, 1.668161973260675834, 0.9417010505823987243 ) ) ;
#207192 = CARTESIAN_POINT ( 'NONE',  ( -10.50000000000000000, 0.000000000000000000, -3.600000000000002309 ) ) ;
#207194 = AXIS2_PLACEMENT_3D ( 'NONE', #115942, #20495, #86580 ) ;
#207195 = CARTESIAN_POINT ( 'NONE',  ( -1.500000000000001332, 0.1500000000000251132, 0.000000000000000000 ) ) ;
#207196 = CARTESIAN_POINT ( 'NONE',  ( 0.9419464005683108043, 1.389173191389100337, 1.535309223701806447 ) ) ;
#207197 = CARTESIAN_POINT ( 'NONE',  ( 1.364683531249986981, -1.053124999658580752, 0.000000000000000000 ) ) ;
#207198 = CARTESIAN_POINT ( 'NONE',  ( 6.069203928793593050, 0.1358119448514639727, -1.865795782587629681 ) ) ;
#207199 = CARTESIAN_POINT ( 'NONE',  ( 2.121465551170404140, -1.771062468586531047, 0.4427346646293239818 ) ) ;
#207201 = CARTESIAN_POINT ( 'NONE',  ( 4.661274270878652537, 8.290979908523663511, 0.5017903844357074483 ) ) ;
#207200 = CARTESIAN_POINT ( 'NONE',  ( 5.760442859251142522, 0.8911043219209063837, 2.019162844794204048 ) ) ;
#207202 = CARTESIAN_POINT ( 'NONE',  ( 1.364683531249986537, 0.3635416670080869328, 0.7879004041258500513 ) ) ;
#207203 = ADVANCED_FACE ( 'NONE', ( #209447 ), #202189, .T. ) ;
#207204 = CARTESIAN_POINT ( 'NONE',  ( 3.490735631032083841, 2.011810643276640054, 0.4545708190045735786 ) ) ;
#207205 = CARTESIAN_POINT ( 'NONE',  ( -6.028571859570855729, 10.18508426947466816, 0.000000000000000000 ) ) ;
#207206 = CARTESIAN_POINT ( 'NONE',  ( 7.228468454380276853, 11.58496363008569574, 1.040834085586084257E-14 ) ) ;
#207207 = CARTESIAN_POINT ( 'NONE',  ( 4.924636110261781496, 6.768494766770632332, 1.599625672291267175 ) ) ;
#207208 = CARTESIAN_POINT ( 'NONE',  ( -7.385065802799712031, -6.893137084989842123, -8.044078759455182137 ) ) ;
#207209 = CARTESIAN_POINT ( 'NONE',  ( 7.693325821111733021, 7.940244644243982464, -0.7998128361456341429 ) ) ;
#207210 = CARTESIAN_POINT ( 'NONE',  ( 5.529760519541640384, 1.996289034380031913, -0.5486624943154896350 ) ) ;
#207211 = CARTESIAN_POINT ( 'NONE',  ( 0.6823417656249899377, 0.6552083336747518416, 1.181850606188755259 ) ) ;
#207212 = CARTESIAN_POINT ( 'NONE',  ( 2.636181727411972098, 1.021492356387411427, -1.905029093917938399 ) ) ;
#207213 = CARTESIAN_POINT ( 'NONE',  ( -5.076314662610137418, 7.858265529090583179, 1.124058833742283436 ) ) ;
#207215 = CARTESIAN_POINT ( 'NONE',  ( 2.594135478747404022, 0.9273930874063830432, -1.728848471177657942 ) ) ;
#207214 = CARTESIAN_POINT ( 'NONE',  ( 3.615882686718306260, -0.5843173316345972035, 1.933312988646131103 ) ) ;
#207216 = CARTESIAN_POINT ( 'NONE',  ( 6.720655732516620517, 2.957990990047154600, 2.526349433132681011 ) ) ;
#207217 = EDGE_CURVE ( 'NONE', #54318, #149901, #199808, .T. ) ;
#207219 = CARTESIAN_POINT ( 'NONE',  ( 5.816084710582486217, 9.729256562414162701, 1.040834085586084257E-14 ) ) ;
#207218 = CARTESIAN_POINT ( 'NONE',  ( 1.001543065824772753E-15, -2.012499999999999289, 4.012584370867899430 ) ) ;
#207220 = CARTESIAN_POINT ( 'NONE',  ( -7.279802135894939852, 7.457800344824362604, -0.7998128361456362523 ) ) ;
#207221 = CARTESIAN_POINT ( 'NONE',  ( 1.569546381206438967, 1.394087592100446971, 1.457234012747665508 ) ) ;
#207223 = CARTESIAN_POINT ( 'NONE',  ( 5.759372899636661991, 2.159370146098410714, -0.3733810082120898599 ) ) ;
#207222 = CARTESIAN_POINT ( 'NONE',  ( -4.554649539187067830, 7.401175998105142817, 1.199719254218464037 ) ) ;
#207224 = DIRECTION ( 'NONE',  ( 0.8164965809277251463, 0.000000000000000000, 0.5773502691896270633 ) ) ;
#207225 = CARTESIAN_POINT ( 'NONE',  ( 6.328373294368253354, -0.9077179077918960948, -1.683272687665722467 ) ) ;
#207226 = CARTESIAN_POINT ( 'NONE',  ( -2.764973262183167968, 5.313220341600567664, 1.199719254218462483 ) ) ;
#207227 = CARTESIAN_POINT ( 'NONE',  ( 4.134873662043553111, 7.767843672452050541, -0.7216878364870197293 ) ) ;
#207229 = CARTESIAN_POINT ( 'NONE',  ( 2.759388848745081280, 1.913798524274639812, -0.6352183541234107667 ) ) ;
#207228 = CARTESIAN_POINT ( 'NONE',  ( -8.527715432871366019, 10.01171809551380143, 1.082531754730558626 ) ) ;
#207230 = CARTESIAN_POINT ( 'NONE',  ( -1.499999999999997780, 3.400000000000021227, 1.214306433183764966E-14 ) ) ;
#207231 = CARTESIAN_POINT ( 'NONE',  ( -1.364683531250014514, 13.65104166700806765, -0.7879004041258335089 ) ) ;
#207232 = CARTESIAN_POINT ( 'NONE',  ( -0.01747323780270595983, -0.1290080397739183926, -1.696210917522892325 ) ) ;
#207233 = CARTESIAN_POINT ( 'NONE',  ( 7.212011367826596242, 7.378711115411311638, 0.000000000000000000 ) ) ;
#207234 = CARTESIAN_POINT ( 'NONE',  ( 8.242994207428692377, 12.56065097540143327, -0.7216878364870328300 ) ) ;
#207235 = FACE_OUTER_BOUND ( 'NONE', #103648, .T. ) ;
#207236 = CARTESIAN_POINT ( 'NONE',  ( 4.235518730357812345, -1.288231833625707701, -1.356488508162751128 ) ) ;
#207237 = PRESENTATION_STYLE_ASSIGNMENT (( #157448 ) ) ;
#207238 = CARTESIAN_POINT ( 'NONE',  ( 1.323191598296684646, -1.869966582492128548, -0.8887066864656999465 ) ) ;
#207239 = CARTESIAN_POINT ( 'NONE',  ( 6.619590326553026038, 0.3579758704960536719, -2.039031579972025554 ) ) ;
#207240 = EDGE_LOOP ( 'NONE', ( #121850, #5287, #61953, #130242, #89950, #187815 ) ) ;
#207241 = CARTESIAN_POINT ( 'NONE',  ( 5.401997860402196316, 5.267028690082820930, 0.000000000000000000 ) ) ;
#207242 = CARTESIAN_POINT ( 'NONE',  ( 0.03503794071320948805, -0.08894543905034424380, 1.809493548878613023 ) ) ;
#207243 = CARTESIAN_POINT ( 'NONE',  ( 4.353576723319599218, 8.093273587265928271, -0.7216878364870357165 ) ) ;
#207244 = CARTESIAN_POINT ( 'NONE',  ( 11.88209931242717943, 7.837836862524945936, -1.732717975941681532 ) ) ;
#207245 = ORIENTED_EDGE ( 'NONE', *, *, #6214, .T. ) ;
#207246 = CARTESIAN_POINT ( 'NONE',  ( 9.544576953896278582, 10.23768732240824164, 0.000000000000000000 ) ) ;
#207247 = EDGE_CURVE ( 'NONE', #55414, #114731, #16905, .T. ) ;
#207249 = CARTESIAN_POINT ( 'NONE',  ( 9.237182729612253951, 9.671134694169463586, 0.7998128361456462443 ) ) ;
#207248 = CARTESIAN_POINT ( 'NONE',  ( 1.662477996687723669, -0.7030478115006146833, -1.831755296705489977 ) ) ;
#207250 = CARTESIAN_POINT ( 'NONE',  ( 4.956599115817130752, -1.805213640821627052, -0.6413244422398997058 ) ) ;
#207251 = CARTESIAN_POINT ( 'NONE',  ( -0.5999334525453070555, -3.113692707265594439, 3.364453219699692355 ) ) ;
#207252 = CARTESIAN_POINT ( 'NONE',  ( 10.18233705906309972, 11.83814697611718714, 1.199719254218450271 ) ) ;
#207253 = CARTESIAN_POINT ( 'NONE',  ( -10.40709887848274562, 1.794419290072776896, 5.561702625701074432 ) ) ;
#207255 = EDGE_LOOP ( 'NONE', ( #26134, #102939, #94773, #36372 ) ) ;
#207254 = CARTESIAN_POINT ( 'NONE',  ( 3.660338286009610975, 6.253849852777763729, -1.082531754730543083 ) ) ;
#207256 = CARTESIAN_POINT ( 'NONE',  ( -7.022760382198764084, 11.13704484596649635, 0.7216878364870458196 ) ) ;
#207257 = CARTESIAN_POINT ( 'NONE',  ( 2.922914210685311431, 2.035003303901411265, 0.7295308445595325431 ) ) ;
#207258 = CARTESIAN_POINT ( 'NONE',  ( -5.822300622425855110, 5.757381912443740646, 0.7998128361456281477 ) ) ;
#207259 = CARTESIAN_POINT ( 'NONE',  ( 5.090160327287878594, 4.903218234782778850, -0.7998128361456481317 ) ) ;
#207260 = CARTESIAN_POINT ( 'NONE',  ( -0.03470293633787284449, -1.699275230904277789, 1.268407768021381221 ) ) ;
#207261 = CARTESIAN_POINT ( 'NONE',  ( 4.700122295916242088, -1.825221593135372578, -0.04401369772454033491 ) ) ;
#207262 = CARTESIAN_POINT ( 'NONE',  ( 8.858328068414154544, 13.09032149711157444, 7.626023304531035052 ) ) ;
#207263 = CARTESIAN_POINT ( 'NONE',  ( 0.8957027828950543391, -0.7134963830764933235, 1.837871659531468804 ) ) ;
#207264 = CARTESIAN_POINT ( 'NONE',  ( 3.849791259674230748, -1.322437695595569673, -1.381667681676468140 ) ) ;
#207265 = ORIENTED_EDGE ( 'NONE', *, *, #155215, .T. ) ;
#207266 = CARTESIAN_POINT ( 'NONE',  ( 0.4499999960734538673, 4.000000000000008882, 0.9281957781481324776 ) ) ;
#207267 = CARTESIAN_POINT ( 'NONE',  ( 4.756286019550246102, -1.969087757444639042, -0.05037552155932183140 ) ) ;
#207268 = ORIENTED_EDGE ( 'NONE', *, *, #240, .F. ) ;
#207269 = CARTESIAN_POINT ( 'NONE',  ( 6.374560617330069512, -0.09999853314933374038, -1.939619642457596660 ) ) ;
#207270 = ORIENTED_EDGE ( 'NONE', *, *, #171420, .F. ) ;
#207271 = CARTESIAN_POINT ( 'NONE',  ( -6.231907884136888676, 7.299589282028351001, -1.199719254218453823 ) ) ;
#207273 = CARTESIAN_POINT ( 'NONE',  ( 6.328397690248316110, -1.000878058022572903, -1.869571840794107986 ) ) ;
#207272 = CARTESIAN_POINT ( 'NONE',  ( -5.093022980588950865, 5.970890227889075419, -1.199719254218453823 ) ) ;
#207274 = CARTESIAN_POINT ( 'NONE',  ( 5.519577934094840543, 9.453608333170423705, 0.7216878364870317197 ) ) ;
#207276 = VERTEX_POINT ( 'NONE', #22757 ) ;
#207275 = CARTESIAN_POINT ( 'NONE',  ( 3.668532269402470458, 0.6909111621477401766, 1.783275653667259597 ) ) ;
#207277 = EDGE_CURVE ( 'NONE', #141384, #44750, #94540, .T. ) ;
#207278 = CARTESIAN_POINT ( 'NONE',  ( 11.41267819554179042, 3.447199233515649386, -3.708203932499494648 ) ) ;
#207279 = TOROIDAL_SURFACE ( 'NONE', #113985, 2.600000000000000089, 0.1000000000000000056 ) ;
#207280 = CARTESIAN_POINT ( 'NONE',  ( 7.518896314322763175, -5.199789852012120406, 8.029456579251585069 ) ) ;
#207281 = CARTESIAN_POINT ( 'NONE',  ( 5.531894615797754433, -1.963542475010676469, 0.4432068886008522779 ) ) ;
#207282 = CARTESIAN_POINT ( 'NONE',  ( -15.75000000000000000, 12.30000000000000071, -0.7000000000000009548 ) ) ;
#207283 = CARTESIAN_POINT ( 'NONE',  ( 6.604126001430527637, -1.825160783932573860, 0.05055279568313279792 ) ) ;
#207284 = CARTESIAN_POINT ( 'NONE',  ( 6.727182134110221590, 3.706444386917655542, 2.325533714637216143 ) ) ;
#207285 = CARTESIAN_POINT ( 'NONE',  ( 1.557173632797459462, 1.693725193156172315, -1.190412882225246438 ) ) ;
#207286 = CARTESIAN_POINT ( 'NONE',  ( -5.876569516519495551, 8.943415971659659292, 1.199719254218452047 ) ) ;
#207287 = CARTESIAN_POINT ( 'NONE',  ( -6.033312665451926904, 7.071988487544162538, -1.043104321438679039 ) ) ;
#207288 = CARTESIAN_POINT ( 'NONE',  ( 1.217323170181688008, 2.861755683774202641, -0.7749999999999910294 ) ) ;
#207289 = CARTESIAN_POINT ( 'NONE',  ( -2.458659901369638412, -3.215527211319108680, 2.374326415922315636 ) ) ;
#207290 = CARTESIAN_POINT ( 'NONE',  ( 6.959412922516382771, 7.013736585890911535, 0.7998128361456341429 ) ) ;
#207291 = CARTESIAN_POINT ( 'NONE',  ( 0.000000000000000000, -5.166862915010145052, 0.000000000000000000 ) ) ;
#207292 = ADVANCED_FACE ( 'NONE', ( #146165 ), #195962, .T. ) ;
#207293 = CARTESIAN_POINT ( 'NONE',  ( 4.909461021924254709, 5.860697626067345567, 1.082531754730549078 ) ) ;
#207294 = DIRECTION ( 'NONE',  ( 0.000000000000000000, 0.000000000000000000, 1.000000000000000000 ) ) ;
#207295 = CARTESIAN_POINT ( 'NONE',  ( -1.364683531250000748, 11.67187500034139802, 0.000000000000000000 ) ) ;
#207297 = CARTESIAN_POINT ( 'NONE',  ( -7.469616286486262524, 7.679250187180907794, 0.7998128361456341429 ) ) ;
#207296 = CARTESIAN_POINT ( 'NONE',  ( 6.825078400183575589, 6.038285016609903799, 2.450557349082567171 ) ) ;
#207298 =( GEOMETRIC_REPRESENTATION_CONTEXT ( 3 ) GLOBAL_UNCERTAINTY_ASSIGNED_CONTEXT ( ( #45165 ) ) GLOBAL_UNIT_ASSIGNED_CONTEXT ( ( #210151, #127961, #194987 ) ) REPRESENTATION_CONTEXT ( 'NONE', 'WORKASPACE' ) );
#207299 = CARTESIAN_POINT ( 'NONE',  ( 5.291581958225426874, 1.307657812419236176, -1.139094164941084841 ) ) ;
#207300 = CARTESIAN_POINT ( 'NONE',  ( -3.716906668440817185, 7.488141546489591072, 0.7998128361456341429 ) ) ;
#207301 = CARTESIAN_POINT ( 'NONE',  ( 2.834898843300116766, -1.979765732921334731, -0.6052725283285932401 ) ) ;
#207302 =( BOUNDED_SURFACE ( )  B_SPLINE_SURFACE ( 1, 2, ( 
 ( #212921, #196690, #128584, #114439, #180439, #32056, #210797, #209718, #115493, #112312, #93889, #178327, #159929, #77602, #11532, #193493, #64555, #130698, #120841, #2710, #184674, #102372, #200909, #100242, #50433, #116552, #82921, #1645, #68784, #569, #70912, #83985, #34170, #135954, #182544, #3768, #166310, #36296, #152201, #134903, #69843, #66636, #198784, #20041, #17899, #16839, #201969, #18973, #150073, #168442, #67703, #133850, #199860, #51503, #148994, #117629, #35227, #33117, #183620, #54690, #52558, #101303, #118690, #119759, #21089, #99194, #86128, #167383, #53627, #185738, #151143, #169507, #137022, #103447, #85057, #37371, #87192, #165245, #153257, #203049, #4832, #132781, #140248, #8068, #122999, #171639, #142388, #39509, #105608, #138092, #90409, #73059, #92566, #56829, #55757, #75220, #60031, #23236, #191079, #74154, #91489, #174877, #121913, #172726, #187882, #206269, #57894, #188956, #208397, #40596, #58966, #124057, #204105, #42746, #170569, #26457, #157550, #190023, #88266, #106701, #41675, #24304, #156479, #89347, #107786, #108851, #173811, #155396, #38444, #158606, #25390, #207345, #9146, #205188, #141331, #154334, #125121, #186816, #139158, #10205, #76280, #6978, #104524, #22151, #5909, #71982, #211597, #192146, #144533, #30751, #114194, #47007, #62176, #28608, #48083, #97891, #79483, #178062, #110984, #128335, #210542, #163952, #43810, #95764, #77348, #180194, #11270, #109923, #93626, #145602, #80552, #78412, #147697, #63233, #194298, #13407, #212664, #31815, #175934, #161817, #61102, #129396, #14461, #29680, #15527, #81613, #196439, #94697, #179129, #64306, #126182, #45943, #213715, #195375, #112062, #113123, #96832, #162882, #176990, #27527, #193232, #44879, #143460, #146649, #12332, #159668, #130451, #209458, #127261, #160738, #198541, #69604, #167142, #184434, #53378, #148755, #51254, #325, #18727, #84811, #1399, #86949, #67460, #151959, #150900, #16589, #135711, #49132, #119513, #36051, #68537, #181240, #133606, #2461, #199611, #183376, #82671, #134665, #201737, #200668, #66395, #131485, #37124, #117379, #85883, #149829, #83737, #34982, #32868, #3529, #153017, #166067, #101053, #103203, #100000, #52318, #115250, #19799, #118447, #102131, #197490, #168200, #185499, #169265, #20851, #65338, #182298, #98944, #164998, #132543, #50187, #116308, #33926, #17654, #42493, #136777, #188715, #170321, #141080, #104277, #70667, #186575, #172481, #173568, #171397, #137852, #202806, #189777, #204941, #55517, #156237, #203873, #121673, #105360, #187639, #120598, #5658, #6742, #92323, #39266, #122753, #38203, #91241, #26206, #22988, #89106, #190834, #155160, #138924, #54455, #25139, #56592, #90171, #21909, #72820, #123816, #207089, #140000, #40351, #106457, #58718, #108602, #24068, #7814, #73907, #206021, #57657, #174630, #88019, #41428, #154090, #124868, #71738, #107536, #157301, #8891, #74970, #4593, #77091, #142137, #129143, #144289, #209207, #95518, #143218, #60847, #44621, #127010, #59782, #159413, #160484, #31560, #192968, #179936, #177811, #110736, #45690, #30495, #146393, #9957, #194038, #93377, #111805, #46757, #61922, #80296, #196187, #14202, #176736, #211349, #96579, #158365, #12091, #113941, #29427, #78158, #161566, #13154, #94445, #28349, #76034, #11015, #210282, #109679, #128082, #79231, #64049, #145348, #27271, #112868, #208152, #62974, #162626, #195118, #178883, #212407, #130194, #47829, #125939, #191897, #43559, #175682, #119252, #33666, #184178, #50996, #48871, #101874, #81361, #151707, #2203, #100798, #213465, #99740, #117116, #165812, #1146, #114989, #183119, #167941, #166884, #98684, #163692, #69343, #17395, #118189, #182037, #116049, #133344, #32609, #199349, #200416, #67208, #19542, #135453, #85619, #71, #150642, #35797, #97635, #83479, #53119, #34726, #149561, #18474, #84553, #68279, #82414, #185236, #164740, #16331, #180988, #134412, #198286, #3276, #52062, #148503, #201477, #15274, #66134, #147440, #65089, #131245, #197232, #132280, #49928, #186308, #138657, #56329, #187381, #58460, #39012, #123554, #204678, #202543, #41163, #20601, #90980, #155966, #40082, #152755 ),
 ( #55262, #154899, #4337, #189517, #124615, #137591, #121409, #8629, #71481, #171135, #86687, #205760, #22728, #122488, #102943, #105094, #7552, #24874, #172219, #88842, #153832, #173292, #74710, #188450, #6482, #21649, #72559, #106194, #140813, #169002, #23808, #54192, #157041, #136524, #70405, #120332, #89913, #57390, #203609, #170062, #37944, #73638, #139736, #87755, #107273, #5402, #206826, #36859, #104017, #92051, #191633, #192700, #63781, #27006, #212145, #210013, #142947, #77899, #62706, #178617, #42228, #13946, #46482, #93112, #29157, #128867, #190573, #44354, #146132, #144019, #110476, #61655, #11822, #126740, #175422, #108345, #43296, #109417, #141882, #94183, #76826, #96311, #60582, #59514, #78958, #174365, #159154, #194850, #127822, #95248, #30227, #125672, #176476, #10754, #193777, #45423, #28087, #25944, #160223, #112605, #111539, #207891, #162366, #158108, #80029, #161296, #177548, #9697, #12882, #145080, #211083, #75774, #208946, #149303, #200166, #133090, #130989, #195927, #101622, #132030, #150385, #214251, #148248, #33415, #97374, #1956, #151453, #16073, #65882, #167687, #164487, #49670, #179678, #84301, #115793, #884, #47564, #198040, #34479, #117938, #50734, #181782, #32358, #51820, #19289, #83221, #99494, #114734, #165551, #17144, #85371, #113675, #66951, #81100, #183932, #15010, #31299, #163431, #199088, #68017, #82157, #48619, #147189, #100551, #116860, #180732, #182861, #98422, #166624, #18216, #134158, #213214, #196979, #35544, #3025, #129939, #64843, #121163, #37693, #55014, #56081, #105941, #135215, #203362, #86442, #187132, #72301, #71229, #39833, #154648, #171965, #20357, #5152, #152507, #38761, #104842, #169821, #73376, #21408, #122238, #170887, #168754, #188197, #201230, #23556, #6230, #22480, #119006, #87518, #88591, #153583, #137344, #102696, #138407, #89663, #204426, #4091, #69093, #7298, #155715, #139481, #52871, #184984, #36610, #186058, #70162, #136273, #202293, #53945, #120082, #103770, #182481, #98079, #2646, #34109, #133788, #114379, #66576, #167320, #36228, #183555, #198723, #165182, #184611, #19977, #1580, #100181, #33055, #50369, #132718, #86061, #180374, #17836, #213902, #102307, #147886, #31998, #15718, #67641, #68719, #508, #181425, #164134, #18907, #166246, #99133, #199796, #16776, #82860, #148936, #116492, #81803, #49317, #83919, #135891, #150010, #69783, #51441, #117560, #35162, #134841, #168381, #65525, #101238, #197673, #84991, #151082, #200844, #152138, #3706, #118625, #52495, #48265, #131670, #115434, #55692, #160405, #158288, #121847, #9878, #23170, #138028, #186755, #12008, #54628, #120775, #153197, #105539, #88200, #110657, #71918, #70846, #93299, #78082, #38378, #209129, #92238, #53562, #5848, #109599, #192884, #125859, #204042, #104459, #126927, #176658, #75954, #39445, #170506, #187818, #171573, #28271, #119695, #142057, #4768, #44541, #87127, #185679, #169444, #208071, #159335, #154273, #22088, #37308, #175604, #59697, #191816, #43481, #27193, #10931, #77007, #143134, #103382, #202988, #60767, #201909, #94363, #21029, #136961, #141369, #108892, #105649, #24341, #25424, #23274, #93664, #106739, #56867, #158645, #73095, #26495, #188994, #207381, #174915, #91531, #92602, #89385, #7019, #42783, #205226, #139196, #123043, #40637, #190061, #10243, #192184, #75255, #140290, #157589, #172768, #41713, #76319, #126223, #155434, #59002, #60067, #43848, #187917, #90451, #156517, #142424, #109962, #57933, #206309, #8108, #208433, #39548, #159706, #11305, #175972, #27566, #74196, #173848, #125158, #77383, #143500, #55796, #124097, #121951, #171677, #107823, #9184, #191117, #16626, #195416, #129433, #193268, #98980, #165033, #47046, #13445, #181276, #48119, #96869, #163986, #145640, #113162, #44914, #115285, #144568, #97928, #111022, #79522, #82709, #209496, #213751, #162919, #114231, #197523, #78450, #179166, #210581, #14499, #80591, #211635, #61136, #63271, #81648, #146687, #160777, #65373, #177027, #49167, #180229, #212703, #28644, #30790, #64344, #130490, #196477, #12370, #31852, #131520, #15561, #62212, #127298, #32902, #147735, #94731, #128369, #194336 ) ),
 .UNSPECIFIED., .F., .F., .T. ) 
 B_SPLINE_SURFACE_WITH_KNOTS ( ( 2, 2 ),
 ( 3, 2, 2, 2, 2, 2, 2, 2, 2, 2, 2, 2, 2, 2, 2, 2, 2, 2, 2, 2, 2, 2, 2, 2, 2, 2, 2, 2, 2, 2, 2, 2, 2, 2, 2, 2, 2, 2, 2, 2, 2, 2, 2, 2, 2, 2, 2, 2, 2, 2, 2, 2, 2, 2, 2, 2, 2, 2, 2, 2, 2, 2, 2, 2, 2, 2, 2, 2, 2, 2, 2, 2, 2, 2, 2, 2, 2, 2, 2, 2, 2, 2, 2, 2, 2, 2, 2, 2, 2, 2, 2, 2, 2, 2, 2, 2, 2, 2, 2, 2, 2, 2, 2, 2, 2, 2, 2, 2, 2, 2, 2, 2, 2, 2, 2, 2, 2, 2, 2, 2, 2, 2, 2, 2, 2, 2, 2, 2, 2, 2, 2, 2, 2, 2, 2, 2, 2, 2, 2, 2, 2, 2, 2, 2, 2, 2, 2, 2, 2, 2, 2, 2, 2, 2, 2, 2, 2, 2, 2, 2, 2, 2, 2, 2, 2, 2, 2, 2, 2, 2, 2, 2, 2, 2, 2, 2, 2, 2, 2, 2, 2, 2, 2, 2, 2, 2, 2, 2, 2, 2, 2, 2, 2, 2, 2, 2, 2, 2, 2, 2, 2, 2, 2, 2, 2, 2, 2, 2, 2, 2, 2, 2, 2, 2, 2, 2, 2, 2, 2, 2, 2, 2, 2, 2, 2, 2, 2, 2, 2, 2, 2, 2, 2, 2, 2, 2, 2, 2, 2, 2, 3 ),
 ( 0.000000000000000000, 1.000000000000000000 ),
 ( 0.000000000000000000, 0.004166666666666666609, 0.008333333333333333218, 0.01250000000000000069, 0.01666666666666666644, 0.02083333333333333218, 0.02500000000000000139, 0.02916666666666666713, 0.03333333333333333287, 0.03749999999999999861, 0.04166666666666666435, 0.04583333333333333010, 0.05000000000000000278, 0.05416666666666666852, 0.05833333333333333426, 0.06250000000000000000, 0.06666666666666666574, 0.07083333333333333148, 0.07499999999999999722, 0.07916666666666666297, 0.08333333333333332871, 0.08749999999999999445, 0.09166666666666666019, 0.09583333333333333981, 0.1000000000000000056, 0.1041666666666666713, 0.1083333333333333370, 0.1125000000000000028, 0.1166666666666666685, 0.1208333333333333343, 0.1250000000000000000, 0.1291666666666666796, 0.1333333333333333315, 0.1375000000000000111, 0.1416666666666666630, 0.1458333333333333426, 0.1499999999999999944, 0.1541666666666666741, 0.1583333333333333259, 0.1625000000000000056, 0.1666666666666666574, 0.1708333333333333370, 0.1749999999999999889, 0.1791666666666666685, 0.1833333333333333204, 0.1875000000000000000, 0.1916666666666666796, 0.1958333333333333315, 0.2000000000000000111, 0.2041666666666666630, 0.2083333333333333426, 0.2124999999999999944, 0.2166666666666666741, 0.2208333333333333259, 0.2250000000000000056, 0.2291666666666666574, 0.2333333333333333370, 0.2374999999999999889, 0.2416666666666666685, 0.2458333333333333204, 0.2500000000000000000, 0.2541666666666666519, 0.2583333333333333592, 0.2625000000000000111, 0.2666666666666666630, 0.2708333333333333148, 0.2750000000000000222, 0.2791666666666666741, 0.2833333333333333259, 0.2874999999999999778, 0.2916666666666666852, 0.2958333333333333370, 0.2999999999999999889, 0.3041666666666666408, 0.3083333333333333481, 0.3125000000000000000, 0.3166666666666666519, 0.3208333333333333592, 0.3250000000000000111, 0.3291666666666666630, 0.3333333333333333148, 0.3375000000000000222, 0.3416666666666666741, 0.3458333333333333259, 0.3499999999999999778, 0.3541666666666666852, 0.3583333333333333370, 0.3624999999999999889, 0.3666666666666666408, 0.3708333333333333481, 0.3750000000000000000, 0.3791666666666666519, 0.3833333333333333592, 0.3875000000000000111, 0.3916666666666666630, 0.3958333333333333148, 0.4000000000000000222, 0.4041666666666666741, 0.4083333333333333259, 0.4124999999999999778, 0.4166666666666666852, 0.4208333333333333370, 0.4249999999999999889, 0.4291666666666666408, 0.4333333333333333481, 0.4375000000000000000, 0.4416666666666666519, 0.4458333333333333592, 0.4500000000000000111, 0.4541666666666666630, 0.4583333333333333148, 0.4625000000000000222, 0.4666666666666666741, 0.4708333333333333259, 0.4749999999999999778, 0.4791666666666666852, 0.4833333333333333370, 0.4874999999999999889, 0.4916666666666666408, 0.4958333333333333481, 0.5000000000000000000, 0.5041666666666666519, 0.5083333333333333037, 0.5124999999999999556, 0.5166666666666667185, 0.5208333333333333703, 0.5250000000000000222, 0.5291666666666666741, 0.5333333333333333259, 0.5374999999999999778, 0.5416666666666666297, 0.5458333333333332815, 0.5500000000000000444, 0.5541666666666666963, 0.5583333333333333481, 0.5625000000000000000, 0.5666666666666666519, 0.5708333333333333037, 0.5749999999999999556, 0.5791666666666667185, 0.5833333333333333703, 0.5875000000000000222, 0.5916666666666666741, 0.5958333333333333259, 0.5999999999999999778, 0.6041666666666666297, 0.6083333333333332815, 0.6125000000000000444, 0.6166666666666666963, 0.6208333333333333481, 0.6250000000000000000, 0.6291666666666666519, 0.6333333333333333037, 0.6374999999999999556, 0.6416666666666667185, 0.6458333333333333703, 0.6500000000000000222, 0.6541666666666666741, 0.6583333333333333259, 0.6624999999999999778, 0.6666666666666666297, 0.6708333333333332815, 0.6750000000000000444, 0.6791666666666666963, 0.6833333333333333481, 0.6875000000000000000, 0.6916666666666666519, 0.6958333333333333037, 0.6999999999999999556, 0.7041666666666667185, 0.7083333333333333703, 0.7125000000000000222, 0.7166666666666666741, 0.7208333333333333259, 0.7249999999999999778, 0.7291666666666666297, 0.7333333333333332815, 0.7375000000000000444, 0.7416666666666666963, 0.7458333333333333481, 0.7500000000000000000, 0.7541666666666666519, 0.7583333333333333037, 0.7624999999999999556, 0.7666666666666667185, 0.7708333333333333703, 0.7750000000000000222, 0.7791666666666666741, 0.7833333333333333259, 0.7874999999999999778, 0.7916666666666666297, 0.7958333333333332815, 0.8000000000000000444, 0.8041666666666666963, 0.8083333333333333481, 0.8125000000000000000, 0.8166666666666666519, 0.8208333333333333037, 0.8249999999999999556, 0.8291666666666667185, 0.8333333333333333703, 0.8375000000000000222, 0.8416666666666666741, 0.8458333333333333259, 0.8499999999999999778, 0.8541666666666666297, 0.8583333333333332815, 0.8625000000000000444, 0.8666666666666666963, 0.8708333333333333481, 0.8750000000000000000, 0.8791666666666666519, 0.8833333333333333037, 0.8874999999999999556, 0.8916666666666667185, 0.8958333333333333703, 0.9000000000000000222, 0.9041666666666666741, 0.9083333333333333259, 0.9124999999999999778, 0.9166666666666666297, 0.9208333333333332815, 0.9250000000000000444, 0.9291666666666666963, 0.9333333333333333481, 0.9375000000000000000, 0.9416666666666666519, 0.9458333333333333037, 0.9499999999999999556, 0.9541666666666667185, 0.9583333333333333703, 0.9625000000000000222, 0.9666666666666666741, 0.9708333333333333259, 0.9749999999999999778, 0.9791666666666666297, 0.9833333333333332815, 0.9875000000000000444, 0.9916666666666666963, 0.9958333333333333481, 1.000000000000000000 ),
 .UNSPECIFIED. ) 
 GEOMETRIC_REPRESENTATION_ITEM ( )  RATIONAL_B_SPLINE_SURFACE ( (
 ( 1.000000000000000000, 0.8660254037844387076, 1.000000000000000000, 0.8660254037844387076, 1.000000000000000000, 0.8660254037844387076, 1.000000000000000000, 0.8660254037844387076, 1.000000000000000000, 0.8660254037844387076, 1.000000000000000000, 0.8660254037844387076, 1.000000000000000000, 0.8660254037844387076, 1.000000000000000000, 0.8660254037844387076, 1.000000000000000000, 0.8660254037844387076, 1.000000000000000000, 0.8660254037844387076, 1.000000000000000000, 0.8660254037844387076, 1.000000000000000000, 0.8660254037844387076, 1.000000000000000000, 0.8660254037844387076, 1.000000000000000000, 0.8660254037844387076, 1.000000000000000000, 0.8660254037844387076, 1.000000000000000000, 0.8660254037844387076, 1.000000000000000000, 0.8660254037844387076, 1.000000000000000000, 0.8660254037844387076, 1.000000000000000000, 0.8660254037844387076, 1.000000000000000000, 0.8660254037844387076, 1.000000000000000000, 0.8660254037844387076, 1.000000000000000000, 0.8660254037844387076, 1.000000000000000000, 0.8660254037844387076, 1.000000000000000000, 0.8660254037844387076, 1.000000000000000000, 0.8660254037844387076, 1.000000000000000000, 0.8660254037844387076, 1.000000000000000000, 0.8660254037844387076, 1.000000000000000000, 0.8660254037844387076, 1.000000000000000000, 0.8660254037844387076, 1.000000000000000000, 0.8660254037844387076, 1.000000000000000000, 0.8660254037844387076, 1.000000000000000000, 0.8660254037844387076, 1.000000000000000000, 0.8660254037844387076, 1.000000000000000000, 0.8660254037844387076, 1.000000000000000000, 0.8660254037844387076, 1.000000000000000000, 0.8660254037844387076, 1.000000000000000000, 0.8660254037844387076, 1.000000000000000000, 0.8660254037844387076, 1.000000000000000000, 0.8660254037844387076, 1.000000000000000000, 0.8660254037844387076, 1.000000000000000000, 0.8660254037844387076, 1.000000000000000000, 0.8660254037844387076, 1.000000000000000000, 0.8660254037844387076, 1.000000000000000000, 0.8660254037844387076, 1.000000000000000000, 0.8660254037844387076, 1.000000000000000000, 0.8660254037844387076, 1.000000000000000000, 0.8660254037844387076, 1.000000000000000000, 0.8660254037844387076, 1.000000000000000000, 0.8660254037844387076, 1.000000000000000000, 0.8660254037844387076, 1.000000000000000000, 0.8660254037844387076, 1.000000000000000000, 0.8660254037844387076, 1.000000000000000000, 0.8660254037844387076, 1.000000000000000000, 0.8660254037844387076, 1.000000000000000000, 0.8660254037844387076, 1.000000000000000000, 0.8660254037844387076, 1.000000000000000000, 0.8660254037844387076, 1.000000000000000000, 0.8660254037844387076, 1.000000000000000000, 0.8660254037844387076, 1.000000000000000000, 0.8660254037844387076, 1.000000000000000000, 0.8660254037844387076, 1.000000000000000000, 0.8660254037844387076, 1.000000000000000000, 0.8660254037844387076, 1.000000000000000000, 0.8660254037844387076, 1.000000000000000000, 0.8660254037844387076, 1.000000000000000000, 0.8660254037844387076, 1.000000000000000000, 0.8660254037844387076, 1.000000000000000000, 0.8660254037844387076, 1.000000000000000000, 0.8660254037844387076, 1.000000000000000000, 0.8660254037844387076, 1.000000000000000000, 0.8660254037844387076, 1.000000000000000000, 0.8660254037844387076, 1.000000000000000000, 0.8660254037844387076, 1.000000000000000000, 0.8660254037844387076, 1.000000000000000000, 0.8660254037844387076, 1.000000000000000000, 0.8660254037844387076, 1.000000000000000000, 0.8660254037844387076, 1.000000000000000000, 0.8660254037844387076, 1.000000000000000000, 0.8660254037844387076, 1.000000000000000000, 0.8660254037844387076, 1.000000000000000000, 0.8660254037844387076, 1.000000000000000000, 0.8660254037844387076, 1.000000000000000000, 0.8660254037844387076, 1.000000000000000000, 0.8660254037844387076, 1.000000000000000000, 0.8660254037844387076, 1.000000000000000000, 0.8660254037844387076, 1.000000000000000000, 0.8660254037844387076, 1.000000000000000000, 0.8660254037844387076, 1.000000000000000000, 0.8660254037844387076, 1.000000000000000000, 0.8660254037844387076, 1.000000000000000000, 0.8660254037844387076, 1.000000000000000000, 0.8660254037844387076, 1.000000000000000000, 0.8660254037844387076, 1.000000000000000000, 0.8660254037844387076, 1.000000000000000000, 0.8660254037844387076, 1.000000000000000000, 0.8660254037844387076, 1.000000000000000000, 0.8660254037844387076, 1.000000000000000000, 0.8660254037844387076, 1.000000000000000000, 0.8660254037844387076, 1.000000000000000000, 0.8660254037844387076, 1.000000000000000000, 0.8660254037844387076, 1.000000000000000000, 0.8660254037844387076, 1.000000000000000000, 0.8660254037844387076, 1.000000000000000000, 0.8660254037844387076, 1.000000000000000000, 0.8660254037844387076, 1.000000000000000000, 0.8660254037844387076, 1.000000000000000000, 0.8660254037844387076, 1.000000000000000000, 0.8660254037844387076, 1.000000000000000000, 0.8660254037844387076, 1.000000000000000000, 0.8660254037844387076, 1.000000000000000000, 0.8660254037844387076, 1.000000000000000000, 0.8660254037844387076, 1.000000000000000000, 0.8660254037844387076, 1.000000000000000000, 0.8660254037844387076, 1.000000000000000000, 0.8660254037844387076, 1.000000000000000000, 0.8660254037844387076, 1.000000000000000000, 0.8660254037844387076, 1.000000000000000000, 0.8660254037844387076, 1.000000000000000000, 0.8660254037844387076, 1.000000000000000000, 0.8660254037844387076, 1.000000000000000000, 0.8660254037844387076, 1.000000000000000000, 0.8660254037844387076, 1.000000000000000000, 0.8660254037844387076, 1.000000000000000000, 0.8660254037844387076, 1.000000000000000000, 0.8660254037844387076, 1.000000000000000000, 0.8660254037844387076, 1.000000000000000000, 0.8660254037844387076, 1.000000000000000000, 0.8660254037844387076, 1.000000000000000000, 0.8660254037844387076, 1.000000000000000000, 0.8660254037844387076, 1.000000000000000000, 0.8660254037844387076, 1.000000000000000000, 0.8660254037844387076, 1.000000000000000000, 0.8660254037844387076, 1.000000000000000000, 0.8660254037844387076, 1.000000000000000000, 0.8660254037844387076, 1.000000000000000000, 0.8660254037844387076, 1.000000000000000000, 0.8660254037844387076, 1.000000000000000000, 0.8660254037844387076, 1.000000000000000000, 0.8660254037844387076, 1.000000000000000000, 0.8660254037844387076, 1.000000000000000000, 0.8660254037844387076, 1.000000000000000000, 0.8660254037844387076, 1.000000000000000000, 0.8660254037844387076, 1.000000000000000000, 0.8660254037844387076, 1.000000000000000000, 0.8660254037844387076, 1.000000000000000000, 0.8660254037844387076, 1.000000000000000000, 0.8660254037844387076, 1.000000000000000000, 0.8660254037844387076, 1.000000000000000000, 0.8660254037844387076, 1.000000000000000000, 0.8660254037844387076, 1.000000000000000000, 0.8660254037844387076, 1.000000000000000000, 0.8660254037844387076, 1.000000000000000000, 0.8660254037844387076, 1.000000000000000000, 0.8660254037844387076, 1.000000000000000000, 0.8660254037844387076, 1.000000000000000000, 0.8660254037844387076, 1.000000000000000000, 0.8660254037844387076, 1.000000000000000000, 0.8660254037844387076, 1.000000000000000000, 0.8660254037844387076, 1.000000000000000000, 0.8660254037844387076, 1.000000000000000000, 0.8660254037844387076, 1.000000000000000000, 0.8660254037844387076, 1.000000000000000000, 0.8660254037844387076, 1.000000000000000000, 0.8660254037844387076, 1.000000000000000000, 0.8660254037844387076, 1.000000000000000000, 0.8660254037844387076, 1.000000000000000000, 0.8660254037844387076, 1.000000000000000000, 0.8660254037844387076, 1.000000000000000000, 0.8660254037844387076, 1.000000000000000000, 0.8660254037844387076, 1.000000000000000000, 0.8660254037844387076, 1.000000000000000000, 0.8660254037844387076, 1.000000000000000000, 0.8660254037844387076, 1.000000000000000000, 0.8660254037844387076, 1.000000000000000000, 0.8660254037844387076, 1.000000000000000000, 0.8660254037844387076, 1.000000000000000000, 0.8660254037844387076, 1.000000000000000000, 0.8660254037844387076, 1.000000000000000000, 0.8660254037844387076, 1.000000000000000000, 0.8660254037844387076, 1.000000000000000000, 0.8660254037844387076, 1.000000000000000000, 0.8660254037844387076, 1.000000000000000000, 0.8660254037844387076, 1.000000000000000000, 0.8660254037844387076, 1.000000000000000000, 0.8660254037844387076, 1.000000000000000000, 0.8660254037844387076, 1.000000000000000000, 0.8660254037844387076, 1.000000000000000000, 0.8660254037844387076, 1.000000000000000000, 0.8660254037844387076, 1.000000000000000000, 0.8660254037844387076, 1.000000000000000000, 0.8660254037844387076, 1.000000000000000000, 0.8660254037844387076, 1.000000000000000000, 0.8660254037844387076, 1.000000000000000000, 0.8660254037844387076, 1.000000000000000000, 0.8660254037844387076, 1.000000000000000000, 0.8660254037844387076, 1.000000000000000000, 0.8660254037844387076, 1.000000000000000000, 0.8660254037844387076, 1.000000000000000000, 0.8660254037844387076, 1.000000000000000000, 0.8660254037844387076, 1.000000000000000000, 0.8660254037844387076, 1.000000000000000000, 0.8660254037844387076, 1.000000000000000000, 0.8660254037844387076, 1.000000000000000000, 0.8660254037844387076, 1.000000000000000000, 0.8660254037844387076, 1.000000000000000000, 0.8660254037844387076, 1.000000000000000000, 0.8660254037844387076, 1.000000000000000000, 0.8660254037844387076, 1.000000000000000000, 0.8660254037844387076, 1.000000000000000000, 0.8660254037844387076, 1.000000000000000000, 0.8660254037844387076, 1.000000000000000000, 0.8660254037844387076, 1.000000000000000000, 0.8660254037844387076, 1.000000000000000000, 0.8660254037844387076, 1.000000000000000000, 0.8660254037844387076, 1.000000000000000000, 0.8660254037844387076, 1.000000000000000000, 0.8660254037844387076, 1.000000000000000000, 0.8660254037844387076, 1.000000000000000000, 0.8660254037844387076, 1.000000000000000000, 0.8660254037844387076, 1.000000000000000000, 0.8660254037844387076, 1.000000000000000000, 0.8660254037844387076, 1.000000000000000000, 0.8660254037844387076, 1.000000000000000000, 0.8660254037844387076, 1.000000000000000000, 0.8660254037844387076, 1.000000000000000000, 0.8660254037844387076, 1.000000000000000000, 0.8660254037844387076, 1.000000000000000000, 0.8660254037844387076, 1.000000000000000000, 0.8660254037844387076, 1.000000000000000000, 0.8660254037844387076, 1.000000000000000000, 0.8660254037844387076, 1.000000000000000000, 0.8660254037844387076, 1.000000000000000000, 0.8660254037844387076, 1.000000000000000000, 0.8660254037844387076, 1.000000000000000000, 0.8660254037844387076, 1.000000000000000000, 0.8660254037844387076, 1.000000000000000000, 0.8660254037844387076, 1.000000000000000000, 0.8660254037844387076, 1.000000000000000000, 0.8660254037844387076, 1.000000000000000000, 0.8660254037844387076, 1.000000000000000000),
 ( 1.000000000000000000, 0.8660254037844387076, 1.000000000000000000, 0.8660254037844387076, 1.000000000000000000, 0.8660254037844387076, 1.000000000000000000, 0.8660254037844387076, 1.000000000000000000, 0.8660254037844387076, 1.000000000000000000, 0.8660254037844387076, 1.000000000000000000, 0.8660254037844387076, 1.000000000000000000, 0.8660254037844387076, 1.000000000000000000, 0.8660254037844387076, 1.000000000000000000, 0.8660254037844387076, 1.000000000000000000, 0.8660254037844387076, 1.000000000000000000, 0.8660254037844387076, 1.000000000000000000, 0.8660254037844387076, 1.000000000000000000, 0.8660254037844387076, 1.000000000000000000, 0.8660254037844387076, 1.000000000000000000, 0.8660254037844387076, 1.000000000000000000, 0.8660254037844387076, 1.000000000000000000, 0.8660254037844387076, 1.000000000000000000, 0.8660254037844387076, 1.000000000000000000, 0.8660254037844387076, 1.000000000000000000, 0.8660254037844387076, 1.000000000000000000, 0.8660254037844387076, 1.000000000000000000, 0.8660254037844387076, 1.000000000000000000, 0.8660254037844387076, 1.000000000000000000, 0.8660254037844387076, 1.000000000000000000, 0.8660254037844387076, 1.000000000000000000, 0.8660254037844387076, 1.000000000000000000, 0.8660254037844387076, 1.000000000000000000, 0.8660254037844387076, 1.000000000000000000, 0.8660254037844387076, 1.000000000000000000, 0.8660254037844387076, 1.000000000000000000, 0.8660254037844387076, 1.000000000000000000, 0.8660254037844387076, 1.000000000000000000, 0.8660254037844387076, 1.000000000000000000, 0.8660254037844387076, 1.000000000000000000, 0.8660254037844387076, 1.000000000000000000, 0.8660254037844387076, 1.000000000000000000, 0.8660254037844387076, 1.000000000000000000, 0.8660254037844387076, 1.000000000000000000, 0.8660254037844387076, 1.000000000000000000, 0.8660254037844387076, 1.000000000000000000, 0.8660254037844387076, 1.000000000000000000, 0.8660254037844387076, 1.000000000000000000, 0.8660254037844387076, 1.000000000000000000, 0.8660254037844387076, 1.000000000000000000, 0.8660254037844387076, 1.000000000000000000, 0.8660254037844387076, 1.000000000000000000, 0.8660254037844387076, 1.000000000000000000, 0.8660254037844387076, 1.000000000000000000, 0.8660254037844387076, 1.000000000000000000, 0.8660254037844387076, 1.000000000000000000, 0.8660254037844387076, 1.000000000000000000, 0.8660254037844387076, 1.000000000000000000, 0.8660254037844387076, 1.000000000000000000, 0.8660254037844387076, 1.000000000000000000, 0.8660254037844387076, 1.000000000000000000, 0.8660254037844387076, 1.000000000000000000, 0.8660254037844387076, 1.000000000000000000, 0.8660254037844387076, 1.000000000000000000, 0.8660254037844387076, 1.000000000000000000, 0.8660254037844387076, 1.000000000000000000, 0.8660254037844387076, 1.000000000000000000, 0.8660254037844387076, 1.000000000000000000, 0.8660254037844387076, 1.000000000000000000, 0.8660254037844387076, 1.000000000000000000, 0.8660254037844387076, 1.000000000000000000, 0.8660254037844387076, 1.000000000000000000, 0.8660254037844387076, 1.000000000000000000, 0.8660254037844387076, 1.000000000000000000, 0.8660254037844387076, 1.000000000000000000, 0.8660254037844387076, 1.000000000000000000, 0.8660254037844387076, 1.000000000000000000, 0.8660254037844387076, 1.000000000000000000, 0.8660254037844387076, 1.000000000000000000, 0.8660254037844387076, 1.000000000000000000, 0.8660254037844387076, 1.000000000000000000, 0.8660254037844387076, 1.000000000000000000, 0.8660254037844387076, 1.000000000000000000, 0.8660254037844387076, 1.000000000000000000, 0.8660254037844387076, 1.000000000000000000, 0.8660254037844387076, 1.000000000000000000, 0.8660254037844387076, 1.000000000000000000, 0.8660254037844387076, 1.000000000000000000, 0.8660254037844387076, 1.000000000000000000, 0.8660254037844387076, 1.000000000000000000, 0.8660254037844387076, 1.000000000000000000, 0.8660254037844387076, 1.000000000000000000, 0.8660254037844387076, 1.000000000000000000, 0.8660254037844387076, 1.000000000000000000, 0.8660254037844387076, 1.000000000000000000, 0.8660254037844387076, 1.000000000000000000, 0.8660254037844387076, 1.000000000000000000, 0.8660254037844387076, 1.000000000000000000, 0.8660254037844387076, 1.000000000000000000, 0.8660254037844387076, 1.000000000000000000, 0.8660254037844387076, 1.000000000000000000, 0.8660254037844387076, 1.000000000000000000, 0.8660254037844387076, 1.000000000000000000, 0.8660254037844387076, 1.000000000000000000, 0.8660254037844387076, 1.000000000000000000, 0.8660254037844387076, 1.000000000000000000, 0.8660254037844387076, 1.000000000000000000, 0.8660254037844387076, 1.000000000000000000, 0.8660254037844387076, 1.000000000000000000, 0.8660254037844387076, 1.000000000000000000, 0.8660254037844387076, 1.000000000000000000, 0.8660254037844387076, 1.000000000000000000, 0.8660254037844387076, 1.000000000000000000, 0.8660254037844387076, 1.000000000000000000, 0.8660254037844387076, 1.000000000000000000, 0.8660254037844387076, 1.000000000000000000, 0.8660254037844387076, 1.000000000000000000, 0.8660254037844387076, 1.000000000000000000, 0.8660254037844387076, 1.000000000000000000, 0.8660254037844387076, 1.000000000000000000, 0.8660254037844387076, 1.000000000000000000, 0.8660254037844387076, 1.000000000000000000, 0.8660254037844387076, 1.000000000000000000, 0.8660254037844387076, 1.000000000000000000, 0.8660254037844387076, 1.000000000000000000, 0.8660254037844387076, 1.000000000000000000, 0.8660254037844387076, 1.000000000000000000, 0.8660254037844387076, 1.000000000000000000, 0.8660254037844387076, 1.000000000000000000, 0.8660254037844387076, 1.000000000000000000, 0.8660254037844387076, 1.000000000000000000, 0.8660254037844387076, 1.000000000000000000, 0.8660254037844387076, 1.000000000000000000, 0.8660254037844387076, 1.000000000000000000, 0.8660254037844387076, 1.000000000000000000, 0.8660254037844387076, 1.000000000000000000, 0.8660254037844387076, 1.000000000000000000, 0.8660254037844387076, 1.000000000000000000, 0.8660254037844387076, 1.000000000000000000, 0.8660254037844387076, 1.000000000000000000, 0.8660254037844387076, 1.000000000000000000, 0.8660254037844387076, 1.000000000000000000, 0.8660254037844387076, 1.000000000000000000, 0.8660254037844387076, 1.000000000000000000, 0.8660254037844387076, 1.000000000000000000, 0.8660254037844387076, 1.000000000000000000, 0.8660254037844387076, 1.000000000000000000, 0.8660254037844387076, 1.000000000000000000, 0.8660254037844387076, 1.000000000000000000, 0.8660254037844387076, 1.000000000000000000, 0.8660254037844387076, 1.000000000000000000, 0.8660254037844387076, 1.000000000000000000, 0.8660254037844387076, 1.000000000000000000, 0.8660254037844387076, 1.000000000000000000, 0.8660254037844387076, 1.000000000000000000, 0.8660254037844387076, 1.000000000000000000, 0.8660254037844387076, 1.000000000000000000, 0.8660254037844387076, 1.000000000000000000, 0.8660254037844387076, 1.000000000000000000, 0.8660254037844387076, 1.000000000000000000, 0.8660254037844387076, 1.000000000000000000, 0.8660254037844387076, 1.000000000000000000, 0.8660254037844387076, 1.000000000000000000, 0.8660254037844387076, 1.000000000000000000, 0.8660254037844387076, 1.000000000000000000, 0.8660254037844387076, 1.000000000000000000, 0.8660254037844387076, 1.000000000000000000, 0.8660254037844387076, 1.000000000000000000, 0.8660254037844387076, 1.000000000000000000, 0.8660254037844387076, 1.000000000000000000, 0.8660254037844387076, 1.000000000000000000, 0.8660254037844387076, 1.000000000000000000, 0.8660254037844387076, 1.000000000000000000, 0.8660254037844387076, 1.000000000000000000, 0.8660254037844387076, 1.000000000000000000, 0.8660254037844387076, 1.000000000000000000, 0.8660254037844387076, 1.000000000000000000, 0.8660254037844387076, 1.000000000000000000, 0.8660254037844387076, 1.000000000000000000, 0.8660254037844387076, 1.000000000000000000, 0.8660254037844387076, 1.000000000000000000, 0.8660254037844387076, 1.000000000000000000, 0.8660254037844387076, 1.000000000000000000, 0.8660254037844387076, 1.000000000000000000, 0.8660254037844387076, 1.000000000000000000, 0.8660254037844387076, 1.000000000000000000, 0.8660254037844387076, 1.000000000000000000, 0.8660254037844387076, 1.000000000000000000, 0.8660254037844387076, 1.000000000000000000, 0.8660254037844387076, 1.000000000000000000, 0.8660254037844387076, 1.000000000000000000, 0.8660254037844387076, 1.000000000000000000, 0.8660254037844387076, 1.000000000000000000, 0.8660254037844387076, 1.000000000000000000, 0.8660254037844387076, 1.000000000000000000, 0.8660254037844387076, 1.000000000000000000, 0.8660254037844387076, 1.000000000000000000, 0.8660254037844387076, 1.000000000000000000, 0.8660254037844387076, 1.000000000000000000, 0.8660254037844387076, 1.000000000000000000, 0.8660254037844387076, 1.000000000000000000, 0.8660254037844387076, 1.000000000000000000, 0.8660254037844387076, 1.000000000000000000, 0.8660254037844387076, 1.000000000000000000, 0.8660254037844387076, 1.000000000000000000, 0.8660254037844387076, 1.000000000000000000, 0.8660254037844387076, 1.000000000000000000, 0.8660254037844387076, 1.000000000000000000, 0.8660254037844387076, 1.000000000000000000, 0.8660254037844387076, 1.000000000000000000, 0.8660254037844387076, 1.000000000000000000, 0.8660254037844387076, 1.000000000000000000, 0.8660254037844387076, 1.000000000000000000, 0.8660254037844387076, 1.000000000000000000, 0.8660254037844387076, 1.000000000000000000, 0.8660254037844387076, 1.000000000000000000, 0.8660254037844387076, 1.000000000000000000, 0.8660254037844387076, 1.000000000000000000, 0.8660254037844387076, 1.000000000000000000, 0.8660254037844387076, 1.000000000000000000, 0.8660254037844387076, 1.000000000000000000, 0.8660254037844387076, 1.000000000000000000, 0.8660254037844387076, 1.000000000000000000, 0.8660254037844387076, 1.000000000000000000, 0.8660254037844387076, 1.000000000000000000, 0.8660254037844387076, 1.000000000000000000, 0.8660254037844387076, 1.000000000000000000, 0.8660254037844387076, 1.000000000000000000, 0.8660254037844387076, 1.000000000000000000, 0.8660254037844387076, 1.000000000000000000, 0.8660254037844387076, 1.000000000000000000, 0.8660254037844387076, 1.000000000000000000, 0.8660254037844387076, 1.000000000000000000, 0.8660254037844387076, 1.000000000000000000, 0.8660254037844387076, 1.000000000000000000, 0.8660254037844387076, 1.000000000000000000, 0.8660254037844387076, 1.000000000000000000, 0.8660254037844387076, 1.000000000000000000, 0.8660254037844387076, 1.000000000000000000, 0.8660254037844387076, 1.000000000000000000, 0.8660254037844387076, 1.000000000000000000, 0.8660254037844387076, 1.000000000000000000, 0.8660254037844387076, 1.000000000000000000, 0.8660254037844387076, 1.000000000000000000, 0.8660254037844387076, 1.000000000000000000) ) ) 
 REPRESENTATION_ITEM ( '' )  SURFACE ( )  );
#207303 = CARTESIAN_POINT ( 'NONE',  ( 3.532911237611217281, -1.729578172696862426, 1.220892919093808482 ) ) ;
#207304 = CARTESIAN_POINT ( 'NONE',  ( 7.426115451983150706, 9.686887332112256388, -1.599625672291262513 ) ) ;
#207305 = CARTESIAN_POINT ( 'NONE',  ( 1.364683531249988535, 3.613541667008086211, 0.7879004041258499402 ) ) ;
#207306 = CARTESIAN_POINT ( 'NONE',  ( 1.657020797538899748, 1.613050045282127032, -1.129676354644502556 ) ) ;
#207307 = CARTESIAN_POINT ( 'NONE',  ( 6.089152713731276201, 6.031799978164165132, 0.2946234760112295126 ) ) ;
#207309 = CARTESIAN_POINT ( 'NONE',  ( -0.01753026575586694516, -1.247696154478775021, 1.449428981083925150 ) ) ;
#207308 = CARTESIAN_POINT ( 'NONE',  ( 3.475000000000000533, -0.8458333333333335480, -2.006292185433951047 ) ) ;
#207310 = CARTESIAN_POINT ( 'NONE',  ( 3.750172280943805170, 0.8240398376481252729, 2.139190334408520577 ) ) ;
#207311 = CARTESIAN_POINT ( 'NONE',  ( 1.805030607383810715, 1.517133602069477893, 1.015288170653723343 ) ) ;
#207312 = B_SPLINE_CURVE_WITH_KNOTS ( 'NONE', 3,
 ( #92175, #125794, #191756, #187500 ),
 .UNSPECIFIED., .F., .F.,
 ( 4, 4 ),
 ( 6.133173666733493856E-19, 0.0003197243294386109026 ),
 .UNSPECIFIED. ) ;
#207313 = CARTESIAN_POINT ( 'NONE',  ( 6.017840079619279692, 8.114175741012878973, -1.599625672291281386 ) ) ;
#207315 = EDGE_CURVE ( 'NONE', #189233, #145242, #37739, .T. ) ;
#207314 = CARTESIAN_POINT ( 'NONE',  ( 4.948362878863507675, 8.716914425408678113, -0.7216878364870267237 ) ) ;
#207316 = CARTESIAN_POINT ( 'NONE',  ( -6.669721502918952716, 9.868759955792373972, 1.199719254218452047 ) ) ;
#207317 = CARTESIAN_POINT ( 'NONE',  ( 2.478773383088346716, -1.385198452255667290, 1.461135165768602029 ) ) ;
#207318 =( BOUNDED_SURFACE ( )  B_SPLINE_SURFACE ( 3, 3, ( 
 ( #139440, #122199, #205475, #169782, #54976, #21371, #80550, #196437, #144531, #323, #131483 ),
 ( #32866, #210540, #115248, #82669, #179127, #29678, #30749, #14459, #132541, #97889, #48081 ),
 ( #162879, #78410, #180191, #148753, #116306, #114192, #98942, #49130, #198539, #65336, #181238 ),
 ( #161815, #197487, #50185, #164996, #16587, #62174, #146647, #66393, #13405, #96830, #163950 ),
 ( #63231, #160736, #182296, #212662, #33923, #129394, #95762, #31813, #195373, #64304, #15525 ),
 ( #79481, #130449, #47005, #12330, #213713, #128333, #81611, #145599, #147695, #194296, #45941 ),
 ( #112060, #178060, #211595, #113121, #104274, #134663, #202804, #153015, #55515, #102129, #84809 ) ),
 .UNSPECIFIED., .T., .F., .F. ) 
 B_SPLINE_SURFACE_WITH_KNOTS ( ( 4, 3, 4 ),
 ( 4, 1, 1, 1, 1, 1, 1, 1, 4 ),
 ( 0.000000000000000000, 0.5000000000000000000, 1.000000000000000000 ),
 ( 0.000000000000000000, 0.2254704865597413344, 0.3973194950497592193, 0.5246576192285303808, 0.6166070239209043846, 0.6823180413592140336, 0.7309932997181896042, 0.7717238569598857678, 1.000000000000000000 ),
 .UNSPECIFIED. ) 
 GEOMETRIC_REPRESENTATION_ITEM ( )  RATIONAL_B_SPLINE_SURFACE ( (
 ( 1.000000000000000000, 1.000000000000000000, 1.000000000000000222, 0.9999999999999997780, 1.000000000000000444, 0.9999999999999996669, 1.000000000000000222, 1.000000000000000222, 1.000000000000000222, 1.000000000000000222, 1.000000000000000222),
 ( 0.3333333333333333703, 0.3333333333333334259, 0.3333333333333333703, 0.3333333333333333703, 0.3333333333333334814, 0.3333333333333332038, 0.3333333333333334814, 0.3333333333333334259, 0.3333333333333334259, 0.3333333333333334259, 0.3333333333333334259),
 ( 0.3333333333333333703, 0.3333333333333334259, 0.3333333333333333703, 0.3333333333333333703, 0.3333333333333334814, 0.3333333333333332038, 0.3333333333333334814, 0.3333333333333334259, 0.3333333333333334259, 0.3333333333333334259, 0.3333333333333334259),
 ( 1.000000000000000000, 1.000000000000000000, 1.000000000000000222, 0.9999999999999997780, 1.000000000000000444, 0.9999999999999996669, 1.000000000000000222, 1.000000000000000222, 1.000000000000000222, 1.000000000000000222, 1.000000000000000222),
 ( 0.3333333333333333703, 0.3333333333333334259, 0.3333333333333333703, 0.3333333333333333703, 0.3333333333333334814, 0.3333333333333332038, 0.3333333333333334814, 0.3333333333333334259, 0.3333333333333334259, 0.3333333333333334259, 0.3333333333333334259),
 ( 0.3333333333333333703, 0.3333333333333334259, 0.3333333333333333703, 0.3333333333333333703, 0.3333333333333334814, 0.3333333333333332038, 0.3333333333333334814, 0.3333333333333334259, 0.3333333333333334259, 0.3333333333333334259, 0.3333333333333334259),
 ( 1.000000000000000000, 1.000000000000000000, 1.000000000000000222, 0.9999999999999997780, 1.000000000000000444, 0.9999999999999996669, 1.000000000000000222, 1.000000000000000222, 1.000000000000000222, 1.000000000000000222, 1.000000000000000222) ) ) 
 REPRESENTATION_ITEM ( '' )  SURFACE ( )  );
#207319 = CARTESIAN_POINT ( 'NONE',  ( 2.272246806564695021, -0.9202570425024100276, -1.732484491337261456 ) ) ;
#207320 = CARTESIAN_POINT ( 'NONE',  ( -7.862839020921525091, 11.26073039346208660, -1.199719254218446718 ) ) ;
#207321 = CARTESIAN_POINT ( 'NONE',  ( -7.074657228232555717, 7.148188275893099686, 1.040834085586084257E-14 ) ) ;
#207322 = CARTESIAN_POINT ( 'NONE',  ( 0.07516593201277278757, 5.721767059778611220, -2.638283098249011971 ) ) ;
#207324 = CARTESIAN_POINT ( 'NONE',  ( 4.012378993168019825, 1.251447367628313767, -1.251755930634059100 ) ) ;
#207323 = CARTESIAN_POINT ( 'NONE',  ( 5.156232390734752258, -1.514662699498746878, 1.441270160984737370 ) ) ;
#207325 = CARTESIAN_POINT ( 'NONE',  ( 4.898866473728816118, 4.866114554557366745, 0.6591557868584748681 ) ) ;
#207326 = CARTESIAN_POINT ( 'NONE',  ( 6.404234474585668302, 1.703059896339639057, -1.534467582428314270 ) ) ;
#207327 = CARTESIAN_POINT ( 'NONE',  ( 6.052664191884576717, -1.496297717267160765, -0.8884939375988825105 ) ) ;
#207328 = STYLED_ITEM ( 'NONE', ( #19080 ), #43714 ) ;
#207329 = CARTESIAN_POINT ( 'NONE',  ( 7.401861798056875053, 10.72292363345333399, -1.199719254218441611 ) ) ;
#207330 = CARTESIAN_POINT ( 'NONE',  ( 5.959697520924294167, -2.181652697926935502, -0.7244182876006750593 ) ) ;
#207331 =( BOUNDED_SURFACE ( )  B_SPLINE_SURFACE ( 3, 2, ( 
 ( #89970, #187441, #72618 ),
 ( #138717, #23863, #156022 ),
 ( #70465, #39068, #57452 ),
 ( #41223, #123612, #189575 ),
 ( #107328, #152818, #4394 ),
 ( #168685, #200100, #66877 ) ),
 .UNSPECIFIED., .F., .F., .F. ) 
 B_SPLINE_SURFACE_WITH_KNOTS ( ( 4, 2, 4 ),
 ( 3, 3 ),
 ( 6.938893903907228378E-18, 0.002403677751102688189, 0.004807355502205369439 ),
 ( 0.000000000000000000, 1.000000000000000000 ),
 .UNSPECIFIED. ) 
 GEOMETRIC_REPRESENTATION_ITEM ( )  RATIONAL_B_SPLINE_SURFACE ( (
 ( 1.000000000000000000, 0.7789607113619931855, 1.000000000000000000),
 ( 1.000000000000000000, 0.7844575505960370565, 1.000000000000000000),
 ( 1.000000000000000000, 0.7910273759749103517, 1.000000000000000000),
 ( 1.000000000000000000, 0.8087931444451713636, 1.000000000000000000),
 ( 1.000000000000000000, 0.8199986536747382315, 1.000000000000000000),
 ( 1.000000000000000000, 0.8356624583022107533, 1.000000000000000000) ) ) 
 REPRESENTATION_ITEM ( '' )  SURFACE ( )  );
#207332 = CARTESIAN_POINT ( 'NONE',  ( -0.1232117409455633916, -0.1621322592461546530, -2.156395338765437764 ) ) ;
#207333 = CARTESIAN_POINT ( 'NONE',  ( 5.852856049955673434, -0.7765510095132116541, 1.550312759826449671 ) ) ;
#207334 = CARTESIAN_POINT ( 'NONE',  ( 5.986835238096758438, 2.090873126042319896, 0.5847848357620232251 ) ) ;
#207335 = LINE ( 'NONE', #76271, #44160 ) ;
#207336 = CARTESIAN_POINT ( 'NONE',  ( 0.2162074652159052257, 1.082675745310441862, -1.819457589102360551 ) ) ;
#207337 = CARTESIAN_POINT ( 'NONE',  ( 6.062500000000003553, -1.451031289061355478, -1.451031289060867868 ) ) ;
#207338 = FACE_OUTER_BOUND ( 'NONE', #191167, .T. ) ;
#207339 = CARTESIAN_POINT ( 'NONE',  ( 3.926716319054617266, 1.828954700887480245, 0.6050711068611572818 ) ) ;
#207340 = CARTESIAN_POINT ( 'NONE',  ( -1.402160292154681736E-14, 10.59375000068279782, 1.732050807568881190 ) ) ;
#207341 = CARTESIAN_POINT ( 'NONE',  ( 0.9091800373960364778, -0.5448693228766487984, -2.153321320651789161 ) ) ;
#207342 = EDGE_LOOP ( 'NONE', ( #201364, #36456 ) ) ;
#207343 = CIRCLE ( 'NONE', #141692, 0.07999999999999946043 ) ;
#207344 = CARTESIAN_POINT ( 'NONE',  ( 1.499999999999990896, 4.025000000000021672, 1.214306433183764966E-14 ) ) ;
#207345 = CARTESIAN_POINT ( 'NONE',  ( 5.983225862332436584, 5.874851682342960402, 0.7998128361456341429 ) ) ;
#207346 = CARTESIAN_POINT ( 'NONE',  ( 5.608269097547198712, 9.694731047113750222, -0.7998128361456281477 ) ) ;
#207347 = CARTESIAN_POINT ( 'NONE',  ( 2.614199364429617756, -0.6941352821057051870, 2.110140411616817868 ) ) ;
#207349 = CARTESIAN_POINT ( 'NONE',  ( -0.02900071798682749002, 0.2267074960015900975, -2.207170277039482986 ) ) ;
#207348 = CIRCLE ( 'NONE', #110484, 0.08000000000000012657 ) ;
#207350 = CARTESIAN_POINT ( 'NONE',  ( 7.619319141200072920, 7.991553207595983643, 0.7216878364870317197 ) ) ;
#207351 = CARTESIAN_POINT ( 'NONE',  ( -10.11401940567025548, 10.90203684947788076, 1.040834085586084257E-14 ) ) ;
#207352 = CARTESIAN_POINT ( 'NONE',  ( 6.211043768836173484, 8.339580045099285854, 1.443375672974065660 ) ) ;
#207353 = CARTESIAN_POINT ( 'NONE',  ( 1.195935645703485539, 1.779627574718087635, 0.9480385367472210500 ) ) ;
#207355 = CARTESIAN_POINT ( 'NONE',  ( 6.742638559370645268, -2.022111636011727498, -0.4062529910623476903 ) ) ;
#207354 = CARTESIAN_POINT ( 'NONE',  ( 7.892817981449907982, 12.36003807833360391, 0.7998128361456462443 ) ) ;
#207356 = CARTESIAN_POINT ( 'NONE',  ( 7.200788982189461507, 8.533913579710086239, -1.082531754730548412 ) ) ;
#207358 = EDGE_CURVE ( 'NONE', #86318, #170765, #80064, .T. ) ;
#207357 = CARTESIAN_POINT ( 'NONE',  ( -2.505492374191539362, 3.019799309333035975, 11.78741486269014516 ) ) ;
#207359 = CARTESIAN_POINT ( 'NONE',  ( -1.364683531250000748, 1.009375000341421247, 0.000000000000000000 ) ) ;
#207360 = CARTESIAN_POINT ( 'NONE',  ( 1.914973420724352726, -0.2224279105748054597, 1.755648307094020311 ) ) ;
#207361 = CARTESIAN_POINT ( 'NONE',  ( 0.6685925339881376717, 1.356301626434471164, 1.492253803477984642 ) ) ;
#207362 = CARTESIAN_POINT ( 'NONE',  ( 5.284588373313929388, 1.531378566088846371, -0.8270805780791794515 ) ) ;
#207363 = CARTESIAN_POINT ( 'NONE',  ( 4.107168962890386688, -0.3918867163640211704, 2.258474592593032959 ) ) ;
#207364 = CARTESIAN_POINT ( 'NONE',  ( -1.364683531250014514, -0.01145833299191483488, -0.7879004041258359514 ) ) ;
#207365 = CARTESIAN_POINT ( 'NONE',  ( 2.800538183361205302, 1.555518290611109800, 0.9846574483025125613 ) ) ;
#207366 = EDGE_CURVE ( 'NONE', #108613, #4315, #25093, .T. ) ;
#207367 = CARTESIAN_POINT ( 'NONE',  ( 8.536830278099042602, 13.11138575775759563, -0.7998128361456352531 ) ) ;
#207368 = CARTESIAN_POINT ( 'NONE',  ( 2.731258071184277103, -1.704167518380688140, 0.6551187846031493178 ) ) ;
#207369 = CARTESIAN_POINT ( 'NONE',  ( 3.973279856364997809, -1.994869694282218386, -0.2930714778977619450 ) ) ;
#207370 = CARTESIAN_POINT ( 'NONE',  ( -9.642873567817536795, 12.27310513391906532, 1.599625672291281386 ) ) ;
#207372 = DIRECTION ( 'NONE',  ( -5.551115123125766062E-17, 0.000000000000000000, 1.000000000000000000 ) ) ;
#207371 = CARTESIAN_POINT ( 'NONE',  ( 2.659333574217698004, -1.968172486592324244, -1.115815620033432154 ) ) ;
#207373 = CARTESIAN_POINT ( 'NONE',  ( 5.262764605058766421, -1.527415466006694533, 1.450107492850923441 ) ) ;
#207374 = CARTESIAN_POINT ( 'NONE',  ( 9.482679952114482447, 14.00853213111861351, 8.402045824544956076 ) ) ;
#207375 = CARTESIAN_POINT ( 'NONE',  ( 2.330607996690749140, -1.275545549462468120, 1.630658604070814199 ) ) ;
#207376 = CARTESIAN_POINT ( 'NONE',  ( 4.878236342818665250, 4.585697242910212523, 1.040834085586084257E-14 ) ) ;
#207377 = CARTESIAN_POINT ( 'NONE',  ( 0.6801582343749935644, 0.2552083336747196229, 1.178068619123780802 ) ) ;
#207378 = CARTESIAN_POINT ( 'NONE',  ( 4.600305182625006317, -0.9987976242244799296, 1.870504488178956759 ) ) ;
#207379 = CARTESIAN_POINT ( 'NONE',  ( 0.9438256413601053829, 0.7817106414217175336, -1.760949446298063936 ) ) ;
#207380 = CARTESIAN_POINT ( 'NONE',  ( -4.655245641445871385, 6.524482229810530498, 1.599625672291263179 ) ) ;
#207381 = CARTESIAN_POINT ( 'NONE',  ( 9.271078113646423091, 9.710679308875986848, 1.040834085586084257E-14 ) ) ;
#207382 = CARTESIAN_POINT ( 'NONE',  ( 6.170369307550831017, 6.371388078330353366, 0.7216878364870328300 ) ) ;
#207383 = CARTESIAN_POINT ( 'NONE',  ( 1.737499999999999378, -0.7729166657107523486, -3.009438278150925683 ) ) ;
#207384 = CARTESIAN_POINT ( 'NONE',  ( -4.548924232584923288, 5.265832011892554121, -1.199719254218446718 ) ) ;
#207385 = CARTESIAN_POINT ( 'NONE',  ( 5.871359616481898414, -1.819694913365289768, -1.088597390283413402 ) ) ;
#207386 = CARTESIAN_POINT ( 'NONE',  ( 1.782391780347460486, -1.127077160282144552, 1.778786634185139270 ) ) ;
#207387 = CARTESIAN_POINT ( 'NONE',  ( -5.387385936583832802, 7.378645907471495846, -1.599625672291271394 ) ) ;
#207388 = CARTESIAN_POINT ( 'NONE',  ( 7.751511138711133064, 10.06651563329490529, -1.599625672291262513 ) ) ;
#207389 = CARTESIAN_POINT ( 'NONE',  ( 6.561375291409637711, 1.546756896810308035, 1.034385502077879382 ) ) ;
#207390 = CARTESIAN_POINT ( 'NONE',  ( 7.938462636001388795, 9.220293482545153907, -1.199719254218441611 ) ) ;
#207391 = CARTESIAN_POINT ( 'NONE',  ( 11.94651559118242190, 9.948693441210290089, 1.135242698369639980 ) ) ;
#207392 = CARTESIAN_POINT ( 'NONE',  ( -5.171509248969888617, 4.998125310078441075, 0.7998128361456281477 ) ) ;
#207393 = CARTESIAN_POINT ( 'NONE',  ( -8.731087737520713432, 10.24898578427137963, 1.082531754730558626 ) ) ;
#207394 =( BOUNDED_SURFACE ( )  B_SPLINE_SURFACE ( 3, 2, ( 
 ( #106629, #187812, #122926 ),
 ( #205118, #121841, #25317 ),
 ( #24233, #123985, #38371 ),
 ( #172658, #9074, #7991 ),
 ( #5841, #189952, #74082 ),
 ( #140173, #188884, #71912 ) ),
 .UNSPECIFIED., .F., .F., .T. ) 
 B_SPLINE_SURFACE_WITH_KNOTS ( ( 4, 2, 4 ),
 ( 3, 3 ),
 ( -4.065758146820641628E-19, 0.0003831416164015016010, 0.0007662832328030036357 ),
 ( 0.000000000000000000, 1.000000000000000000 ),
 .UNSPECIFIED. ) 
 GEOMETRIC_REPRESENTATION_ITEM ( )  RATIONAL_B_SPLINE_SURFACE ( (
 ( 1.000000000000000000, 0.7071067811865475727, 1.000000000000000000),
 ( 1.000000000000000000, 0.6829713513656306967, 1.000000000000000000),
 ( 1.000000000000000000, 0.6534833722368420528, 1.000000000000000000),
 ( 1.000000000000000000, 0.6054027484666428816, 1.000000000000000000),
 ( 1.000000000000000000, 0.5875453974412050417, 1.000000000000000000),
 ( 1.000000000000000000, 0.5879095031487528988, 1.000000000000000000) ) ) 
 REPRESENTATION_ITEM ( '' )  SURFACE ( )  );
#207395 = CARTESIAN_POINT ( 'NONE',  ( 0.6508261300204335464, 2.090236094481153550, 0.3566229023672163878 ) ) ;
#207396 = CARTESIAN_POINT ( 'NONE',  ( 0.000000000000000000, 2.099999999999997868, 0.000000000000000000 ) ) ;
#207398 = CARTESIAN_POINT ( 'NONE',  ( 3.226955236329264398, -1.811681696138227160, -0.7532884077038404236 ) ) ;
#207397 = CARTESIAN_POINT ( 'NONE',  ( -0.6125000000000105915, 0.04166666666666901664, 1.060881119635925796 ) ) ;
#207399 = CARTESIAN_POINT ( 'NONE',  ( 0.6905621207787122628, -2.145541755201633372, -0.2633910710312590275 ) ) ;
#207401 = CARTESIAN_POINT ( 'NONE',  ( -6.137267537028628261, 5.996416355291856348, 0.05987573180751305790 ) ) ;
#207400 = CARTESIAN_POINT ( 'NONE',  ( -5.822300622425855110, 5.757381912443740646, 0.7998128361456281477 ) ) ;
#207402 = CARTESIAN_POINT ( 'NONE',  ( -1.201851678989727383E-14, 1.571875000341420581, 1.575800808251672791 ) ) ;
#207403 = CARTESIAN_POINT ( 'NONE',  ( 2.097218849865792212, -1.740012409040556429, 0.04131442251954255129 ) ) ;
#207404 = CARTESIAN_POINT ( 'NONE',  ( 6.995644074971448134, 7.263932296995902149, -0.7216878364870257245 ) ) ;
#207405 = CARTESIAN_POINT ( 'NONE',  ( -11.43645483535884999, 5.654992568747732484, -5.469194708833876817 ) ) ;
#207406 = CARTESIAN_POINT ( 'NONE',  ( 2.688827190807027367, -1.158510681541668141, -1.649829502315000251 ) ) ;
#207407 = CARTESIAN_POINT ( 'NONE',  ( 6.825078400183582694, 7.051583320515966591, 2.842498375355909435 ) ) ;
#207408 = CARTESIAN_POINT ( 'NONE',  ( -5.957882158562513908, 5.915560371269843465, -0.7998128361456362523 ) ) ;
#207409 = CARTESIAN_POINT ( 'NONE',  ( 2.571113415349820297, 0.09854779587974149546, -1.969128565948689458 ) ) ;
#207411 = CARTESIAN_POINT ( 'NONE',  ( -4.773879485787619892, 7.623257595843924150, 1.082531754730549967 ) ) ;
#207410 = CARTESIAN_POINT ( 'NONE',  ( 6.345967646908174054, -1.254484226688237447, -1.443505786478386899 ) ) ;
#207412 = CARTESIAN_POINT ( 'NONE',  ( -5.682275777458886346, 7.722684055159061423, 1.443375672974058777 ) ) ;
#207413 = CARTESIAN_POINT ( 'NONE',  ( 5.417364897112183719, 8.477953592343014932, 1.199719254218451159 ) ) ;
#207414 = CARTESIAN_POINT ( 'NONE',  ( -5.498713818794216834, 8.572860667638675380, -1.199719254218452047 ) ) ;
#207415 = CARTESIAN_POINT ( 'NONE',  ( 2.543622981932230243, -1.883669348803659549, 0.7290701893776069253 ) ) ;
#207416 = CARTESIAN_POINT ( 'NONE',  ( 7.721398836998391246, -5.907420853759296264, 7.721398836998372595 ) ) ;
#207417 = CARTESIAN_POINT ( 'NONE',  ( 5.245303717312764569, -1.982421492789496753, 1.180877550764187545 ) ) ;
#207418 = CARTESIAN_POINT ( 'NONE',  ( 6.566857081534598350, 1.454584517406570132, -1.316677807353151097 ) ) ;
#207419 = CARTESIAN_POINT ( 'NONE',  ( 3.116010788575247936, 1.952738871351952232, -0.1875660449981580158 ) ) ;
#207420 = CARTESIAN_POINT ( 'NONE',  ( 7.587759525142423911, 12.00413654597487501, 0.7998128361456462443 ) ) ;
#207421 = CARTESIAN_POINT ( 'NONE',  ( 0.3346115673153668424, 0.6298721381652396811, -1.915601020889952322 ) ) ;
#207422 = ORIENTED_EDGE ( 'NONE', *, *, #41266, .T. ) ;
#207423 = CARTESIAN_POINT ( 'NONE',  ( 2.712237125307418228, 1.172176456337461037, -1.763091465072692987 ) ) ;
#207425 = CARTESIAN_POINT ( 'NONE',  ( -6.938021921891187382, 9.117444880338284818, -1.599625672291263179 ) ) ;
#207424 = CARTESIAN_POINT ( 'NONE',  ( -4.081167932913447594, 4.720116328942494555, -1.199719254218452047 ) ) ;
#207426 = CARTESIAN_POINT ( 'NONE',  ( 1.921575063125853022, 1.060747535801230379, -1.504664925706208578 ) ) ;
#207427 = EDGE_LOOP ( 'NONE', ( #177781, #62082 ) ) ;
#207428 = CARTESIAN_POINT ( 'NONE',  ( -8.435144125996554720, 12.99275191363802229, 0.7998128361456341429 ) ) ;
#207429 = CARTESIAN_POINT ( 'NONE',  ( 10.70559879711738560, 9.877729115460759601, 5.430853593049171479 ) ) ;
#207430 = CARTESIAN_POINT ( 'NONE',  ( 2.566775492539817627, 0.7186216927172992541, 1.995234744298620910 ) ) ;
#207431 = CARTESIAN_POINT ( 'NONE',  ( 1.499999999999990896, 4.056250000682819490, 1.214306433183764966E-14 ) ) ;
#207432 = CARTESIAN_POINT ( 'NONE',  ( 8.613507663383630941, 8.943513783569379427, -0.7998128361456221525 ) ) ;
#207433 = CARTESIAN_POINT ( 'NONE',  ( 6.984385409695311964, 8.177479728513226576, 1.199719254218452935 ) ) ;
#207434 = CARTESIAN_POINT ( 'NONE',  ( 4.235659074092642307, -1.418359850100110009, -1.495269491646352256 ) ) ;
#207435 = CIRCLE ( 'NONE', #183168, 2.750000000000000000 ) ;
#207437 = CARTESIAN_POINT ( 'NONE',  ( 1.698526806778306586, 1.531337151408303621, 1.022036240780115346 ) ) ;
#207436 = CARTESIAN_POINT ( 'NONE',  ( -7.232384877886063990, 10.52520055992070525, -1.199719254218446718 ) ) ;
#207438 = CARTESIAN_POINT ( 'NONE',  ( -1.364683531249997417, 4.259375000341424133, 1.214306433183764966E-14 ) ) ;
#207439 = CARTESIAN_POINT ( 'NONE',  ( -3.122502256758252770E-14, 3.499999999999961364, -3.816391647148975608E-14 ) ) ;
#207440 = DIRECTION ( 'NONE',  ( -0.000000000000000000, -1.000000000000000000, -0.000000000000000000 ) ) ;
#207441 = CARTESIAN_POINT ( 'NONE',  ( 11.04978080397792972, 13.60844524987713022, 1.057339094031727988 ) ) ;
#207442 = CARTESIAN_POINT ( 'NONE',  ( 1.348561525465460820, 2.204488851003219896, 0.1053889787279923829 ) ) ;
#207443 = CARTESIAN_POINT ( 'NONE',  ( 2.847247395794590297, -1.882567391055539385, 1.254484791939513899 ) ) ;
#207444 = CARTESIAN_POINT ( 'NONE',  ( -8.514157279702033065, 9.995900250149611921, -1.082531754730543971 ) ) ;
#207445 = CARTESIAN_POINT ( 'NONE',  ( 3.638735373827857167, 1.721918111813141916, 0.5631709482423822299 ) ) ;
#207446 = CARTESIAN_POINT ( 'NONE',  ( 3.116317603207694464, 1.870113986138211670, 0.4147879586954768549 ) ) ;
#207447 = CARTESIAN_POINT ( 'NONE',  ( 3.982925052038261526, 1.964963782255540359, 0.6523228965355857278 ) ) ;
#207448 = CARTESIAN_POINT ( 'NONE',  ( 0.6823417656249899377, 3.238541667008085323, -1.181850606188754593 ) ) ;
#207449 = CARTESIAN_POINT ( 'NONE',  ( 2.852367248507085229, 0.6625980423298013511, 1.856917580869015039 ) ) ;
#207450 = CARTESIAN_POINT ( 'NONE',  ( 1.360239512323542010, 0.7782574302275366840, 1.762357998526616232 ) ) ;
#207451 = CARTESIAN_POINT ( 'NONE',  ( 4.135518821028766112, -1.289757458839156934, -1.355179912160727085 ) ) ;
#207452 = AXIS2_PLACEMENT_3D ( 'NONE', #130219, #29450, #213492 ) ;
#207454 = CARTESIAN_POINT ( 'NONE',  ( 5.258270873920524835, 7.671714958958308017, -1.216365610458163715 ) ) ;
#207453 = CARTESIAN_POINT ( 'NONE',  ( 1.963905137100800724, 0.3917726540721230832, -2.274054798471192296 ) ) ;
#207455 = CARTESIAN_POINT ( 'NONE',  ( 3.912436197073854593, 0.6682525715841195479, 1.737132965711101873 ) ) ;
#207456 = CARTESIAN_POINT ( 'NONE',  ( -0.6823417656249969321, 4.467708333674755394, -1.181850606188749264 ) ) ;
#207457 = CARTESIAN_POINT ( 'NONE',  ( -4.273844736805832767, 6.009238164405336313, 1.599625672291267398 ) ) ;
#207458 = CARTESIAN_POINT ( 'NONE',  ( 5.341022448779654930, 8.318611059296550536, 1.199719254218462483 ) ) ;
#207459 = DIRECTION ( 'NONE',  ( 0.000000000000000000, -1.000000000000000000, 0.000000000000000000 ) ) ;
#207460 = CARTESIAN_POINT ( 'NONE',  ( 0.3464870678724129016, 2.100606130083045198, 0.1525024232564754778 ) ) ;
#207462 = CARTESIAN_POINT ( 'NONE',  ( 1.499999999999993117, 8.854166666666666075, 0.8660254037844408170 ) ) ;
#207461 = CARTESIAN_POINT ( 'NONE',  ( -0.6823417656249969321, 4.530208333674755394, -1.181850606188749264 ) ) ;
#207463 = CARTESIAN_POINT ( 'NONE',  ( 6.679002375395027613, -0.09866081283815136826, -2.159460157733564145 ) ) ;
#207464 = CARTESIAN_POINT ( 'NONE',  ( 2.162495577681341707, 2.120227376586072854, 0.04728746717985036346 ) ) ;
#207465 = CARTESIAN_POINT ( 'NONE',  ( 6.621752733038558603, -0.4373435798001067965, 1.978785184894470639 ) ) ;
#207466 = CARTESIAN_POINT ( 'NONE',  ( -0.6823417656250246877, -0.4489583329919111243, 1.181850606188755259 ) ) ;
#207467 = CARTESIAN_POINT ( 'NONE',  ( -4.202664430556263930, 5.926194473780837413, 1.443375672974064550 ) ) ;
#207468 = CARTESIAN_POINT ( 'NONE',  ( 5.473741331615251227, 7.409117525016355010, -1.599625672291262513 ) ) ;
#207469 = CARTESIAN_POINT ( 'NONE',  ( 0.9136071317731933039, -0.3180670004044767740, 2.137961049616762921 ) ) ;
#207472 = CARTESIAN_POINT ( 'NONE',  ( 2.724825686666657809, 6.122787701178987518, 0.000000000000000000 ) ) ;
#207471 = CARTESIAN_POINT ( 'NONE',  ( 6.825078400183556937, 1.282741234726336943, 1.971047034039685952 ) ) ;
#207470 = CARTESIAN_POINT ( 'NONE',  ( 5.203297092594585393, 9.292540051327542017, 0.7998128361456341429 ) ) ;
#207473 = CARTESIAN_POINT ( 'NONE',  ( -4.516801452008150086, 5.298631777878131111, 1.199719254218452935 ) ) ;
#207474 = CARTESIAN_POINT ( 'NONE',  ( 4.452361426671761713, -1.313546101436880109, 1.530156479064001207 ) ) ;
#207476 = CARTESIAN_POINT ( 'NONE',  ( -6.360183458142173230, 9.473945563590925545, 1.082531754730549967 ) ) ;
#207475 = CARTESIAN_POINT ( 'NONE',  ( -7.687109909268394325, 11.91211929421440097, 0.000000000000000000 ) ) ;
#207478 = CARTESIAN_POINT ( 'NONE',  ( 0.6823417656249969321, 10.77604166700806765, -1.181850606188757036 ) ) ;
#207477 = CARTESIAN_POINT ( 'NONE',  ( 0.5676901151186209971, 0.2185747425910676001, -2.251950761720759253 ) ) ;
#207479 = CARTESIAN_POINT ( 'NONE',  ( -10.30827686509187835, 10.92074451889568643, 1.040834085586084257E-14 ) ) ;
#207481 = CARTESIAN_POINT ( 'NONE',  ( 6.310172759758509109, 1.158674036163497734, -1.650093421473826316 ) ) ;
#207480 = CARTESIAN_POINT ( 'NONE',  ( -4.053524740361572398, 7.672936597156388316, 0.7216878364870317197 ) ) ;
#207482 = CARTESIAN_POINT ( 'NONE',  ( -1.364683531250012516, 1.092708333674754506, 0.7879004041258379498 ) ) ;
#207483 = CARTESIAN_POINT ( 'NONE',  ( -0.04341786867410972472, -5.575210796978270267, 11.00023563321887643 ) ) ;
#207484 = EDGE_CURVE ( 'NONE', #74385, #192349, #104890, .T. ) ;
#207485 = CARTESIAN_POINT ( 'NONE',  ( -1.402160292154681736E-14, 8.812500000000003553, 1.732050807568881190 ) ) ;
#207486 = CARTESIAN_POINT ( 'NONE',  ( 2.824480366436402878, 1.624150206794371609, 0.5811974035451406007 ) ) ;
#207487 = CARTESIAN_POINT ( 'NONE',  ( 4.934241560730721510, 4.721313007132757811, 0.000000000000000000 ) ) ;
#207488 = CARTESIAN_POINT ( 'NONE',  ( 5.285699784481295183, 7.260012063351913625, 1.599625672291268286 ) ) ;
#207489 = CARTESIAN_POINT ( 'NONE',  ( 1.475481261428980506, 1.048764899322068622, 1.425360520505250417 ) ) ;
#207490 = CARTESIAN_POINT ( 'NONE',  ( 2.262359935378143394, 2.012689932058016495, 0.04726890441942610543 ) ) ;
#207491 = FILL_AREA_STYLE_COLOUR ( '', #78291 ) ;
#207492 = CARTESIAN_POINT ( 'NONE',  ( 4.260898339918250066, -1.637375743694971408, 1.479669880875638999 ) ) ;
#207493 = ORIENTED_EDGE ( 'NONE', *, *, #201124, .F. ) ;
#207494 = CARTESIAN_POINT ( 'NONE',  ( -0.7500000000000249800, -1.058333333333314030, 1.299038105676659116 ) ) ;
#207495 = CARTESIAN_POINT ( 'NONE',  ( 7.578644679914694926, 11.78557652663510424, 0.7216878364870438212 ) ) ;
#207497 = CARTESIAN_POINT ( 'NONE',  ( 3.339470413395662085, 0.4871825726840799398, -1.956567533273507964 ) ) ;
#207496 = CARTESIAN_POINT ( 'NONE',  ( 4.178469031319306914, 1.000645923475869559, 1.869553197578948334 ) ) ;
#207499 = ORIENTED_EDGE ( 'NONE', *, *, #181839, .F. ) ;
#207498 = CARTESIAN_POINT ( 'NONE',  ( 3.937629537800376500, -1.731762593766679403, 0.5317277010480087052 ) ) ;
#207500 = CARTESIAN_POINT ( 'NONE',  ( 3.901714345682657292, 7.774026846596938434, 0.7998128361456271485 ) ) ;
#207501 = EDGE_CURVE ( 'NONE', #121080, #104249, #205749, .T. ) ;
#207502 = ORIENTED_EDGE ( 'NONE', *, *, #22175, .T. ) ;
#207503 = VECTOR ( 'NONE', #4788, 1000.000000000000000 ) ;
#207504 = CARTESIAN_POINT ( 'NONE',  ( 0.8482696660519238874, 0.5391449902514727777, 1.791282564952957124 ) ) ;
#207505 = CARTESIAN_POINT ( 'NONE',  ( 4.729096653068339151, 4.411700938201493116, -0.7998128361456211532 ) ) ;
#207506 = EDGE_CURVE ( 'NONE', #158047, #133272, #172014, .T. ) ;
#207507 = CARTESIAN_POINT ( 'NONE',  ( 6.305291373979138747, 1.520805759102667132, 1.009792402853857407 ) ) ;
#207509 = CARTESIAN_POINT ( 'NONE',  ( 2.694441388940031601, 1.384233754937878258, -1.324569364742228972 ) ) ;
#207508 = CARTESIAN_POINT ( 'NONE',  ( -4.060830702492950195, 4.696389560118578999, -1.199719254218452047 ) ) ;
#207510 = CYLINDRICAL_SURFACE ( 'NONE', #71891, 0.3999999999999996891 ) ;
#207511 = CARTESIAN_POINT ( 'NONE',  ( -1.402160292154681736E-14, 1.009375000341417916, -1.575800808251659024 ) ) ;
#207512 = CARTESIAN_POINT ( 'NONE',  ( 2.315885204923604057, 3.829536045110822684, -11.43841291973004992 ) ) ;
#207513 = ORIENTED_EDGE ( 'NONE', *, *, #16160, .T. ) ;
#207514 = CARTESIAN_POINT ( 'NONE',  ( 5.533136088152891929, 9.469426179571447832, -0.7216878364870458196 ) ) ;
#207515 = CARTESIAN_POINT ( 'NONE',  ( -4.123088112331656951, 6.864000993478624579, 1.082531754730549967 ) ) ;
#207516 = CARTESIAN_POINT ( 'NONE',  ( -6.774234028683526532, 7.932303117332766718, 1.199719254218452047 ) ) ;
#207517 = CARTESIAN_POINT ( 'NONE',  ( 2.988655875014298857, -1.259908772670719657, 1.705623289672608678 ) ) ;
#207519 = CARTESIAN_POINT ( 'NONE',  ( -9.997720234198379075, 5.662301760159435204, -5.943093865039206669 ) ) ;
#207518 = CARTESIAN_POINT ( 'NONE',  ( -0.02948999725180430354, 5.724051133006486936, -2.520349822069901879 ) ) ;
#207520 = CARTESIAN_POINT ( 'NONE',  ( 4.270748893545842861, -1.838291250766799223, -0.7124064801689540261 ) ) ;
#207521 = CARTESIAN_POINT ( 'NONE',  ( 0.1057268774627964369, 1.494660468187744229, 1.348908602934977496 ) ) ;
#207522 = ORIENTED_EDGE ( 'NONE', *, *, #190633, .T. ) ;
#207523 = CARTESIAN_POINT ( 'NONE',  ( 0.1404439707000069981, 0.8148842331482269996, 1.954324566802398744 ) ) ;
#207524 = CARTESIAN_POINT ( 'NONE',  ( -0.4579269463803092299, 6.472105396648015763, -3.262807195530565973 ) ) ;
#207525 = CARTESIAN_POINT ( 'NONE',  ( 1.240778115703184303, -2.019486815914430355, -0.4554155650244652853 ) ) ;
#207526 = CARTESIAN_POINT ( 'NONE',  ( 2.167823750104383773, -1.194498894885902329, 1.531050872003832497 ) ) ;
#207527 = EDGE_LOOP ( 'NONE', ( #36493, #134314, #191689, #150046 ) ) ;
#207528 = CARTESIAN_POINT ( 'NONE',  ( 6.052789233858158369, 6.026285292448116948, 0.000000000000000000 ) ) ;
#207529 = CARTESIAN_POINT ( 'NONE',  ( 6.444921918449731280, 8.612437886315108315, 1.599625672291268286 ) ) ;
#207531 = CARTESIAN_POINT ( 'NONE',  ( 7.305145839664861640, 7.417091655897478653, 0.7998128361456341429 ) ) ;
#207530 = CARTESIAN_POINT ( 'NONE',  ( 4.154300538700359091, -1.549125135342351856, 1.404095012314343416 ) ) ;
#207532 = CARTESIAN_POINT ( 'NONE',  ( 4.462041952228939401, 6.299077925724123617, -1.443375672974068769 ) ) ;
#207534 = ORIENTED_EDGE ( 'NONE', *, *, #139088, .T. ) ;
#207533 = CARTESIAN_POINT ( 'NONE',  ( 0.7151241933986829391, 1.480140477221444373, 1.044027612606616140 ) ) ;
#207535 = CARTESIAN_POINT ( 'NONE',  ( 5.338574060078519423, 2.173733305800494175, 0.3801736985692484305 ) ) ;
#207536 = CARTESIAN_POINT ( 'NONE',  ( -0.1531059978909564412, -6.764708007038255921, -10.99917004716958857 ) ) ;
#207537 = CARTESIAN_POINT ( 'NONE',  ( 3.698430944683338328, -2.204125419102770600, -0.1106900096672913392 ) ) ;
#207538 = CARTESIAN_POINT ( 'NONE',  ( 4.318600669050584706, 4.999583595936801572, 2.420000000000000373 ) ) ;
#207539 = CARTESIAN_POINT ( 'NONE',  ( 2.965378323150099860, -1.564627974442783342, -1.099164922500090347 ) ) ;
#207540 = CARTESIAN_POINT ( 'NONE',  ( 10.07100917685271035, 10.64393221595000938, 0.7998128361456462443 ) ) ;
#207541 = CARTESIAN_POINT ( 'NONE',  ( 4.896967953096117654, 0.3505727482827174502, 2.040303948762006492 ) ) ;
#207543 = CARTESIAN_POINT ( 'NONE',  ( 2.606508400632711719, -0.8264410288459265175, -1.997682696722333784 ) ) ;
#207542 = CARTESIAN_POINT ( 'NONE',  ( 1.559074708514246010, 8.689926414953912825, -2.502785155726127808 ) ) ;
#207544 = CARTESIAN_POINT ( 'NONE',  ( 5.284801750429747536, 1.933107837519608685, -1.032524723389722787 ) ) ;
#207545 = ORIENTED_EDGE ( 'NONE', *, *, #72642, .F. ) ;
#207546 =( NAMED_UNIT ( * ) PLANE_ANGLE_UNIT ( ) SI_UNIT ( $, .RADIAN. ) );
#207547 = FACE_OUTER_BOUND ( 'NONE', #31465, .T. ) ;
#207548 = CARTESIAN_POINT ( 'NONE',  ( 3.953084306836263995, 6.769626237021087789, 1.199719254218452047 ) ) ;
#207549 = CARTESIAN_POINT ( 'NONE',  ( 0.6823417656249969321, 15.08854166700806410, -1.181850606188757036 ) ) ;
#207550 = CARTESIAN_POINT ( 'NONE',  ( -8.595506201384022660, 11.05117653974661529, 1.443375672974064550 ) ) ;
#207551 = CARTESIAN_POINT ( 'NONE',  ( 5.923986774528332333, 5.876015756563318426, -0.7998128361456481317 ) ) ;
#207552 = CARTESIAN_POINT ( 'NONE',  ( 5.823117640241993520, -1.869163851432435575, -0.8903994044791310181 ) ) ;
#207553 = CARTESIAN_POINT ( 'NONE',  ( 4.758382555496592836, 0.7388506920381915366, 1.779377657810585767 ) ) ;
#207554 = CARTESIAN_POINT ( 'NONE',  ( 0.4742327405582689170, -2.001515332587662233, -0.2440062454662216829 ) ) ;
#207555 =( NAMED_UNIT ( * ) PLANE_ANGLE_UNIT ( ) SI_UNIT ( $, .RADIAN. ) );
#207556 = CARTESIAN_POINT ( 'NONE',  ( 6.318982112420993502, 9.529840343536603697, -1.199719254218452047 ) ) ;
#207557 = CARTESIAN_POINT ( 'NONE',  ( -4.168895032367330167, 3.976329666238523242, -0.6109567437776577403 ) ) ;
#207558 = CARTESIAN_POINT ( 'NONE',  ( 5.418793955257063644, -1.429144796294969932, 1.355356204701572143 ) ) ;
#207559 = CARTESIAN_POINT ( 'NONE',  ( 6.632792736454030447, -2.050728487082712270, 1.024446431767987331 ) ) ;
#207560 = CARTESIAN_POINT ( 'NONE',  ( 4.688025921862073453, -0.8580590012943272171, 1.611482198803436905 ) ) ;
#207561 = CARTESIAN_POINT ( 'NONE',  ( 4.895902868310594513, 8.725987423088758632, 0.000000000000000000 ) ) ;
#207563 = EDGE_CURVE ( 'NONE', #133392, #209973, #54969, .T. ) ;
#207562 = CARTESIAN_POINT ( 'NONE',  ( 2.968872451268290913, 5.447139712246216625, -1.082531754730543971 ) ) ;
#207564 = CARTESIAN_POINT ( 'NONE',  ( -5.631432701629818460, 7.663367133358481631, 1.599625672291263179 ) ) ;
#207565 = CARTESIAN_POINT ( 'NONE',  ( 4.041212305325117882, 6.872442235258051646, -1.199719254218448494 ) ) ;
#207566 =( BOUNDED_SURFACE ( )  B_SPLINE_SURFACE ( 3, 2, ( 
 ( #19842, #199653, #70707 ),
 ( #35024, #198585, #36092 ),
 ( #53419, #167182, #3574 ),
 ( #182341, #150945, #136820 ),
 ( #49178, #165044, #101096 ),
 ( #181286, #32913, #102176 ) ),
 .UNSPECIFIED., .F., .F., .F. ) 
 B_SPLINE_SURFACE_WITH_KNOTS ( ( 4, 2, 4 ),
 ( 3, 3 ),
 ( 0.000000000000000000, 0.0003766365702389426712, 0.0007532731404778853423 ),
 ( 0.000000000000000000, 1.000000000000000000 ),
 .UNSPECIFIED. ) 
 GEOMETRIC_REPRESENTATION_ITEM ( )  RATIONAL_B_SPLINE_SURFACE ( (
 ( 1.000000000000000000, 0.7452309222762957264, 1.000000000000000000),
 ( 1.000000000000000000, 0.7451892422674152305, 1.000000000000000000),
 ( 1.000000000000000000, 0.7429606254235439078, 1.000000000000000000),
 ( 1.000000000000000000, 0.7311462761268936461, 1.000000000000000000),
 ( 1.000000000000000000, 0.7212257702788928970, 1.000000000000000000),
 ( 1.000000000000000000, 0.7071067811865474617, 1.000000000000000000) ) ) 
 REPRESENTATION_ITEM ( '' )  SURFACE ( )  );
#207567 = ORIENTED_EDGE ( 'NONE', *, *, #144969, .T. ) ;
#207569 = CARTESIAN_POINT ( 'NONE',  ( -0.09313581672419719848, -0.4459848746838651623, -1.970588110806646753 ) ) ;
#207568 = CARTESIAN_POINT ( 'NONE',  ( 2.595044651933966495, -0.5755060336137384214, 1.749081985381637061 ) ) ;
#207570 = CARTESIAN_POINT ( 'NONE',  ( 0.5800033175489105464, 1.582751930679682228, -1.666757776657208145 ) ) ;
#207571 = CARTESIAN_POINT ( 'NONE',  ( 5.682460714699895554, 1.171467074228413674, -1.573401077569417605 ) ) ;
#207572 = CARTESIAN_POINT ( 'NONE',  ( -5.422371370461663176, 8.413518134592214537, -1.199719254218446718 ) ) ;
#207573 = DIRECTION ( 'NONE',  ( -0.03984146075563027578, 0.000000000000000000, 0.9992060137953822085 ) ) ;
#207574 = CARTESIAN_POINT ( 'NONE',  ( -3.623053363349869382, 5.249981562040033189, 1.599625672291267398 ) ) ;
#207575 = CARTESIAN_POINT ( 'NONE',  ( 0.1685321339487330372, -0.8835925182541467526, -1.870455940253319183 ) ) ;
#207576 = CARTESIAN_POINT ( 'NONE',  ( -5.472651281771599763, 6.413789912602166687, 1.199719254218452935 ) ) ;
#207578 = CARTESIAN_POINT ( 'NONE',  ( 1.656895194024514906, -1.602792776363659133, -0.9643473572949823325 ) ) ;
#207577 = CARTESIAN_POINT ( 'NONE',  ( 2.419574211619343274, -1.206166186839405352, -1.707533215648052050 ) ) ;
#207579 = CARTESIAN_POINT ( 'NONE',  ( 1.985703663612121472, 1.880146017696176619, 0.7282698753105636413 ) ) ;
#207580 = CARTESIAN_POINT ( 'NONE',  ( -1.364683531250010740, 4.092708333674752730, 0.7879004041258379498 ) ) ;
#207581 = CARTESIAN_POINT ( 'NONE',  ( 1.751089554790756342, 1.735802523247106377, -0.1280615824842730732 ) ) ;
#207582 = CARTESIAN_POINT ( 'NONE',  ( 5.555090253297246150, 7.504024600312024340, 1.599625672291267398 ) ) ;
#207584 = CARTESIAN_POINT ( 'NONE',  ( 1.499999999999990896, 8.627523663848661428, 2.580000000000000515 ) ) ;
#207583 = CARTESIAN_POINT ( 'NONE',  ( 0.000000000000000000, -3.042800438942089514, 3.475000000000000089 ) ) ;
#207585 = CARTESIAN_POINT ( 'NONE',  ( 2.384998569339055408, 1.577468512335476358, -0.6981430484895093658 ) ) ;
#207587 = EDGE_CURVE ( 'NONE', #41289, #207114, #48521, .T. ) ;
#207586 = CARTESIAN_POINT ( 'NONE',  ( 2.226364491882920404, 2.126620374013419301, 0.5291077681483095096 ) ) ;
#207588 = CARTESIAN_POINT ( 'NONE',  ( 5.584669497696876483, -2.152379054646291756, -0.4867646435422824935 ) ) ;
#207589 = CARTESIAN_POINT ( 'NONE',  ( -10.67060214796032724, 5.239869845146935212, -6.813287888368859235 ) ) ;
#207590 = CARTESIAN_POINT ( 'NONE',  ( 2.377987901236592982, -2.106814941015792808, 0.5239127008311114109 ) ) ;
#207591 = CARTESIAN_POINT ( 'NONE',  ( 0.7326872660318053398, 0.1314506862302306234, 1.821024990000128518 ) ) ;
#207592 = CARTESIAN_POINT ( 'NONE',  ( 3.432911303685074689, -1.728510519573158266, 1.222591858268074150 ) ) ;
#207593 = CARTESIAN_POINT ( 'NONE',  ( 6.539320575229256249, 6.037491965140660000, 2.591644950450102680 ) ) ;
#207594 = VERTEX_POINT ( 'NONE', #45321 ) ;
#207596 = CARTESIAN_POINT ( 'NONE',  ( 1.364683531249988535, 1.676041667008085101, 0.7879004041258500513 ) ) ;
#207595 = CARTESIAN_POINT ( 'NONE',  ( 3.562334897874219308, -1.538608923441080689, 1.699488912218325654 ) ) ;
#207597 = CARTESIAN_POINT ( 'NONE',  ( 5.366329872910639232, 5.155139694684188534, 1.040834085586084257E-14 ) ) ;
#207598 = CARTESIAN_POINT ( 'NONE',  ( 5.444044349889116674, -1.407711435423303792, -1.718264895412445536 ) ) ;
#207599 = CARTESIAN_POINT ( 'NONE',  ( -6.453317930424837812, 7.591587675992828466, 1.082531754730549967 ) ) ;
#207600 = AXIS2_PLACEMENT_3D ( 'NONE', #163718, #62999, #81387 ) ;
#207601 = CARTESIAN_POINT ( 'NONE',  ( 3.660338286009610975, 6.253849852777763729, -1.082531754730543083 ) ) ;
#207602 = CARTESIAN_POINT ( 'NONE',  ( -6.033015167956800262, 9.021972881716168402, -1.082531754730537976 ) ) ;
#207603 = CARTESIAN_POINT ( 'NONE',  ( 6.825078400183575589, 6.038285016609903799, 2.450557349082567171 ) ) ;
#207604 = VERTEX_POINT ( 'NONE', #30123 ) ;
#207605 = CARTESIAN_POINT ( 'NONE',  ( 4.395157833011634096, -0.8647231026696032830, -1.821742675176166060 ) ) ;
#207607 = CARTESIAN_POINT ( 'NONE',  ( 3.344635507851092981, -2.031254381041375456, -0.3572892473815546532 ) ) ;
#207606 = CARTESIAN_POINT ( 'NONE',  ( 6.311484202361478779, 7.322151976631905868, -1.199719254218446718 ) ) ;
#207608 = CARTESIAN_POINT ( 'NONE',  ( 5.833751235630055376, 10.02806988486892514, 0.7998128361456331437 ) ) ;
#207609 = CARTESIAN_POINT ( 'NONE',  ( 8.174640274396848483, 8.501778173076651512, 0.7998128361456291469 ) ) ;
#207611 = ADVANCED_FACE ( 'NONE', ( #160122 ), #166176, .F. ) ;
#207610 = CARTESIAN_POINT ( 'NONE',  ( 3.285556943750000070, -2.384374999522043126, 0.000000000000000000 ) ) ;
#207612 = CARTESIAN_POINT ( 'NONE',  ( 0.6823417656249917140, 5.092708333674749177, 1.181850606188765695 ) ) ;
#207613 = CARTESIAN_POINT ( 'NONE',  ( 6.632779825423476439, -1.959453823303359377, 0.9815127000676395763 ) ) ;
#207614 = CARTESIAN_POINT ( 'NONE',  ( 3.164685561777963230, 1.281361203394768111, 1.556908733426412450 ) ) ;
#207615 = CARTESIAN_POINT ( 'NONE',  ( 2.208333698829296310, 1.645431377724184463, 0.8263914577605266931 ) ) ;
#207616 = EDGE_CURVE ( 'NONE', #183713, #151085, #41585, .T. ) ;
#207617 = CARTESIAN_POINT ( 'NONE',  ( 6.819914962873951936, 7.915321197229798322, -1.199719254218446718 ) ) ;
#207618 =( LENGTH_UNIT ( ) NAMED_UNIT ( * ) SI_UNIT ( .MILLI., .METRE. ) );
#207619 = CARTESIAN_POINT ( 'NONE',  ( 5.983392046985362533, 1.685759371660649375, -0.7011634845648377912 ) ) ;
#207620 = CARTESIAN_POINT ( 'NONE',  ( -8.050844288416501016, 8.287073179441051707, 1.040834085586084257E-14 ) ) ;
#207622 = CARTESIAN_POINT ( 'NONE',  ( -3.955946960137363799, 7.837298230127379917, 0.7998128361456352531 ) ) ;
#207621 = CARTESIAN_POINT ( 'NONE',  ( 6.051720714260678591, 0.6634699467917944959, -2.163057363297292035 ) ) ;
#207623 = CARTESIAN_POINT ( 'NONE',  ( 1.998786363724443182, -0.5629491194198692483, -2.029361489363819882 ) ) ;
#207624 = CARTESIAN_POINT ( 'NONE',  ( -4.938913097128142304, 8.984092056616635347, -0.7998128361456362523 ) ) ;
#207625 = CARTESIAN_POINT ( 'NONE',  ( 9.413438726589914651, 9.876766690643398405, 0.000000000000000000 ) ) ;
#207626 = CARTESIAN_POINT ( 'NONE',  ( 5.980555156959511898, 9.991415093179179863, -0.7216878364870458196 ) ) ;
#207627 = CARTESIAN_POINT ( 'NONE',  ( -7.389357414647957256, 8.579670724299436557, 1.199719254218450271 ) ) ;
#207628 = CARTESIAN_POINT ( 'NONE',  ( 0.000000000000000000, 2.000000000000001776, 0.000000000000000000 ) ) ;
#207629 = CARTESIAN_POINT ( 'NONE',  ( 8.120970824461352322, 9.537182719035495637, -1.082531754730543083 ) ) ;
#207630 = CARTESIAN_POINT ( 'NONE',  ( 4.024405658984873568, 7.794362949307388710, 0.3537781459504486525 ) ) ;
#207631 = CARTESIAN_POINT ( 'NONE',  ( -5.773074481320628948, 5.629675071162500544, 0.000000000000000000 ) ) ;
#207632 = CARTESIAN_POINT ( 'NONE',  ( 2.602056794214495650, 1.574129494629309622, 1.567664267292529612 ) ) ;
#207633 = EDGE_CURVE ( 'NONE', #71186, #116404, #58450, .T. ) ;
#207634 = CARTESIAN_POINT ( 'NONE',  ( 0.1005910224048736229, -2.206496634663042133, -0.04943112074598519229 ) ) ;
#207635 = CARTESIAN_POINT ( 'NONE',  ( -6.134138155540168391, 6.121192367743780949, 0.000000000000000000 ) ) ;
#207636 = CARTESIAN_POINT ( 'NONE',  ( 6.647575389402066826, 6.649926130590872120, 1.040834085586084257E-14 ) ) ;
#207637 = CARTESIAN_POINT ( 'NONE',  ( 4.492601031306558745, 1.923586649950057792, 0.3847822903023030428 ) ) ;
#207638 = CARTESIAN_POINT ( 'NONE',  ( 9.297140650669039275, 11.86975006391249643, 1.599625672291281386 ) ) ;
#207639 = CARTESIAN_POINT ( 'NONE',  ( -4.916288619803077964, 6.680904680207828683, 1.249144131323683515 ) ) ;
#207640 = CARTESIAN_POINT ( 'NONE',  ( -1.532410409194660650, 1.041802156240292376, 1.385306760018483407 ) ) ;
#207641 = CARTESIAN_POINT ( 'NONE',  ( -1.402160292154681736E-14, 0.5718750003414239114, 1.575800808251672791 ) ) ;
#207642 = CARTESIAN_POINT ( 'NONE',  ( -5.655159470675923394, 5.770309935309573923, 0.000000000000000000 ) ) ;
#207644 = EDGE_LOOP ( 'NONE', ( #155043, #145240, #86813, #84248, #72456, #110695, #73559, #198251, #1618 ) ) ;
#207643 = CARTESIAN_POINT ( 'NONE',  ( -6.236387472606158333, 7.338502141871059870, -1.082531754730544860 ) ) ;
#207645 = CARTESIAN_POINT ( 'NONE',  ( 3.392942708002244068, -2.044739723715986113, -0.5619712599038150236 ) ) ;
#207646 = CARTESIAN_POINT ( 'NONE',  ( -4.274563570058511175, 8.209017608368725405, 0.000000000000000000 ) ) ;
#207647 = CARTESIAN_POINT ( 'NONE',  ( 5.172814640947125397, -2.034155943344346795, -0.7319064324283753864 ) ) ;
#207648 = CARTESIAN_POINT ( 'NONE',  ( 3.684953445348177148, 1.336164438771630714, 1.267087564277062484 ) ) ;
#207649 = CARTESIAN_POINT ( 'NONE',  ( 4.944546133779973651, -1.457238331152037825, 1.394083050251286870 ) ) ;
#207650 = CARTESIAN_POINT ( 'NONE',  ( -5.512743837300482674, 6.249232958799082027, 0.9732600881407500459 ) ) ;
#207651 = CARTESIAN_POINT ( 'NONE',  ( -0.6823417656250212460, 1.113541667008083325, 1.181850606188755259 ) ) ;
#207652 = CARTESIAN_POINT ( 'NONE',  ( 6.597592293924691376, -1.739768381213904647, 0.05089061930978015791 ) ) ;
#207653 = CARTESIAN_POINT ( 'NONE',  ( 6.827182134110234557, 2.482032550715262964, 2.096239902261677113 ) ) ;
#207654 = CARTESIAN_POINT ( 'NONE',  ( 3.931501358282940117, 4.649468341827285300, -1.082531754730543083 ) ) ;
#207655 = DIRECTION ( 'NONE',  ( -0.8583236685137344280, 0.5131086435338277907, 0.000000000000000000 ) ) ;
#207656 = EDGE_CURVE ( 'NONE', #96576, #90728, #187735, .T. ) ;
#207657 = AXIS2_PLACEMENT_3D ( 'NONE', #97034, #60231, #142591 ) ;
#207658 = CARTESIAN_POINT ( 'NONE',  ( 4.206063578812153203, -2.156103337031569200, 0.1562769059922017589 ) ) ;
#207659 = CARTESIAN_POINT ( 'NONE',  ( 5.237657596305253627, -1.897407540178517316, -0.6818907625677357309 ) ) ;
#207660 = CARTESIAN_POINT ( 'NONE',  ( -7.321039761255057066, 11.48503745486550365, 0.000000000000000000 ) ) ;
#207661 = CARTESIAN_POINT ( 'NONE',  ( 3.168983506954273999, -1.996715753333128118, -0.8287754370841573515 ) ) ;
#207663 = CARTESIAN_POINT ( 'NONE',  ( 3.655507913172794332, 0.4821067936548150135, -1.911365640376050612 ) ) ;
#207662 = B_SPLINE_CURVE_WITH_KNOTS ( 'NONE', 3,
 ( #97176, #132880, #163230, #182648, #14812, #80903 ),
 .UNSPECIFIED., .F., .F.,
 ( 4, 2, 4 ),
 ( 0.001279092382393099943, 0.001599469101539996744, 0.001919845820686893545 ),
 .UNSPECIFIED. ) ;
#207664 = DIRECTION ( 'NONE',  ( -1.000000000000000000, 0.000000000000000000, -2.168404344971003504E-14 ) ) ;
#207665 = CARTESIAN_POINT ( 'NONE',  ( 1.026927485578407406, 1.372003256358475864, -1.855264817478113226 ) ) ;
#207666 = CARTESIAN_POINT ( 'NONE',  ( 2.425137330123087853, -0.003247232972201920167, 2.060967562036238210 ) ) ;
#207667 = CARTESIAN_POINT ( 'NONE',  ( 5.161643714676827699, 0.9607356898342777063, 1.687723941809249117 ) ) ;
#207670 = EDGE_LOOP ( 'NONE', ( #192325, #121346 ) ) ;
#207669 = CARTESIAN_POINT ( 'NONE',  ( -6.783773251375875724, -6.684699875907230471, 6.634380621478824125 ) ) ;
#207668 = CARTESIAN_POINT ( 'NONE',  ( -7.659993601596706725, 11.88048360193076647, -0.7216878364870267237 ) ) ;
#207671 = CARTESIAN_POINT ( 'NONE',  ( -6.469175572376043348, 7.576401584974034265, 1.199719254218452047 ) ) ;
#207672 = CARTESIAN_POINT ( 'NONE',  ( 11.91294103507080315, 9.985399100435895292, 1.446263142085468134 ) ) ;
#207674 = ORIENTED_EDGE ( 'NONE', *, *, #75725, .F. ) ;
#207673 = CARTESIAN_POINT ( 'NONE',  ( -3.969505113751027547, 7.853116076009993840, 1.214306433183764966E-14 ) ) ;
#207675 = CARTESIAN_POINT ( 'NONE',  ( -8.473482818416682605, 8.988077497682020578, -0.7216878364870267237 ) ) ;
#207676 = CARTESIAN_POINT ( 'NONE',  ( 2.292262453775519404, -0.9438808975747980945, 1.994871701834355804 ) ) ;
#207677 = CARTESIAN_POINT ( 'NONE',  ( -3.285556943750000070, -0.4593749995220435256, 0.000000000000000000 ) ) ;
#207678 = CARTESIAN_POINT ( 'NONE',  ( 6.596542563702321615, 1.939940506139478327, 0.2910815776849539627 ) ) ;
#207679 = CARTESIAN_POINT ( 'NONE',  ( -0.1290005225502676156, 1.324981729379502537, -2.425680704180297464 ) ) ;
#207680 = CARTESIAN_POINT ( 'NONE',  ( -1.500000000000011324, 4.702083334016148974, 0.8660254037844403729 ) ) ;
#207681 =( LENGTH_UNIT ( ) NAMED_UNIT ( * ) SI_UNIT ( .MILLI., .METRE. ) );
#207683 = CARTESIAN_POINT ( 'NONE',  ( -1.426686711745821290, 7.396164654317650466, -4.272688476054423035 ) ) ;
#207682 = CARTESIAN_POINT ( 'NONE',  ( 0.1749903794560592474, 0.7218944060462629819, -2.038148089257747930 ) ) ;
#207684 = CARTESIAN_POINT ( 'NONE',  ( 5.208873985248447802, -0.2666229848188906848, 1.821608446441948193 ) ) ;
#207685 = VERTEX_POINT ( 'NONE', #202996 ) ;
#207686 = CARTESIAN_POINT ( 'NONE',  ( 2.061468863205512925, 0.3533766173234990093, -2.030202010101101795 ) ) ;
#207687 = CARTESIAN_POINT ( 'NONE',  ( -0.6801582343750438575, -0.5677083329919535570, 1.178068619123803451 ) ) ;
#207688 = ADVANCED_FACE ( 'NONE', ( #120783 ), #186761, .F. ) ;
#207689 = CARTESIAN_POINT ( 'NONE',  ( -5.194745412330402878, 9.212286747694129474, 0.000000000000000000 ) ) ;
#207690 = CARTESIAN_POINT ( 'NONE',  ( 10.91927143613603945, -9.998067526917994385, -0.1131244342389418484 ) ) ;
#207691 = CARTESIAN_POINT ( 'NONE',  ( 6.451439665316073935, -1.893653415279672902, 0.9546920624979161607 ) ) ;
#207692 = CARTESIAN_POINT ( 'NONE',  ( 11.05216697254199865, 8.017870898877115238, 4.562987691682096170 ) ) ;
#207693 = CARTESIAN_POINT ( 'NONE',  ( 3.988069740714122791, 7.804498464141805592, 0.7998128361456321445 ) ) ;
#207694 = CARTESIAN_POINT ( 'NONE',  ( 0.6200826401135750565, -1.101877700393244952, -1.741386573944928795 ) ) ;
#207697 = CARTESIAN_POINT ( 'NONE',  ( 4.704558828624370470, 1.604442792107749760, 0.9031527321438773681 ) ) ;
#207696 = CARTESIAN_POINT ( 'NONE',  ( 2.488518357381704238, 1.804271297518467820, 0.4556280478851971183 ) ) ;
#207695 = CARTESIAN_POINT ( 'NONE',  ( -0.5000000000000091038, 3.949999999999960654, 0.3999999999999455103 ) ) ;
#207698 = CARTESIAN_POINT ( 'NONE',  ( 5.445571254183207088, 9.504916896522420444, -0.7998128361456281477 ) ) ;
#207699 = CARTESIAN_POINT ( 'NONE',  ( -4.970620135051034616, 8.062850052469723749, -1.111334424012894617 ) ) ;
#207700 = MECHANICAL_DESIGN_GEOMETRIC_PRESENTATION_REPRESENTATION (  '', ( #86633 ), #148944 ) ;
#207701 = CARTESIAN_POINT ( 'NONE',  ( -6.330731382938325602, 6.350551133041632212, 0.7998128361456281477 ) ) ;
#207703 = VERTEX_POINT ( 'NONE', #10145 ) ;
#207702 = DIRECTION ( 'NONE',  ( -1.000000000000000000, 0.000000000000000000, 0.000000000000000000 ) ) ;
#207704 = CARTESIAN_POINT ( 'NONE',  ( 4.846401659255799466, 2.200796399388889935, 0.1645688927329121420 ) ) ;
#207705 = CARTESIAN_POINT ( 'NONE',  ( 0.1753634416057497925, 0.0001173177735149660839, -2.144164757042037017 ) ) ;
#207706 = CARTESIAN_POINT ( 'NONE',  ( -5.910991785878175975, 6.958873840688411860, -1.082531754730544860 ) ) ;
#207707 = CARTESIAN_POINT ( 'NONE',  ( 6.451413702892147661, -1.613775625804831693, 0.8233398690262339059 ) ) ;
#207708 = CARTESIAN_POINT ( 'NONE',  ( -0.08279552664090458758, -1.841734517378278424, 0.8216794407479923734 ) ) ;
#207709 = DIRECTION ( 'NONE',  ( -0.000000000000000000, 1.000000000000000000, -0.000000000000000000 ) ) ;
#207710 = DIRECTION ( 'NONE',  ( 0.000000000000000000, 1.000000000000000000, 0.000000000000000000 ) ) ;
#207711 = CARTESIAN_POINT ( 'NONE',  ( 5.936178161767468708, -1.066166440211462563, -1.587280745415058814 ) ) ;
#207712 = DIRECTION ( 'NONE',  ( 0.000000000000000000, 0.000000000000000000, 1.000000000000000000 ) ) ;
#207713 = CARTESIAN_POINT ( 'NONE',  ( 0.9009904985227291663, 1.526999960511504772, 1.080287613699250304 ) ) ;
#207714 = CARTESIAN_POINT ( 'NONE',  ( 2.149625371984189126, 1.976669504256656218, -0.3981124878784659815 ) ) ;
#207716 = CARTESIAN_POINT ( 'NONE',  ( 4.512399653719460169, -0.8998888299811370617, -1.904278430835882885 ) ) ;
#207715 = CARTESIAN_POINT ( 'NONE',  ( -7.557780564614042795, 10.90482886110335414, -1.199719254218446718 ) ) ;
#207717 = CARTESIAN_POINT ( 'NONE',  ( 8.015895134177609904, 10.37496362800581018, 1.599625672291281386 ) ) ;
#207719 = CARTESIAN_POINT ( 'NONE',  ( -6.679363233026820446, 10.94434087183997129, 0.000000000000000000 ) ) ;
#207718 = CARTESIAN_POINT ( 'NONE',  ( 1.499999999999987121, -0.4958333333333110882, 0.8660254037844524744 ) ) ;
#207720 = CARTESIAN_POINT ( 'NONE',  ( 3.515882793631277536, -0.5824337298786783634, 1.934013565619496999 ) ) ;
#207721 = CARTESIAN_POINT ( 'NONE',  ( -0.6823417656249969321, 5.467708333674756283, -1.181850606188749264 ) ) ;
#207722 = CARTESIAN_POINT ( 'NONE',  ( 8.920901888111989919, 11.43080484092926241, 1.443375672974076540 ) ) ;
#207723 = CARTESIAN_POINT ( 'NONE',  ( 4.675171183009182663, 0.005162144975975196948, -2.161773191939574179 ) ) ;
#207724 = CARTESIAN_POINT ( 'NONE',  ( -1.907519672996887294, 3.236073672982363369, 0.4612874649729363785 ) ) ;
#207725 = CARTESIAN_POINT ( 'NONE',  ( -0.7500000000000215383, 5.441666666666685082, 1.299038105676671107 ) ) ;
#207726 = CARTESIAN_POINT ( 'NONE',  ( 6.540882763950133238, 6.595727744222092959, 0.000000000000000000 ) ) ;
#207727 = CARTESIAN_POINT ( 'NONE',  ( 7.415946836550712185, 10.63539316174243865, 1.082531754730558626 ) ) ;
#207729 = CARTESIAN_POINT ( 'NONE',  ( -0.1360919303236346745, -7.795524846228471638, 10.99936842639231571 ) ) ;
#207728 = CARTESIAN_POINT ( 'NONE',  ( 2.488948079679761172, 2.105553563057678712, 0.5292575070172370610 ) ) ;
#207731 = CARTESIAN_POINT ( 'NONE',  ( 0.6261898170028465938, 0.1349980957352381883, 1.836376839866371569 ) ) ;
#207730 = CARTESIAN_POINT ( 'NONE',  ( -7.049876689426113785, 8.287572894827684777, -1.082531754730544860 ) ) ;
#207732 = CARTESIAN_POINT ( 'NONE',  ( -1.364683531250014514, 1.738541667008085545, -0.7879004041258289570 ) ) ;
#207733 = CARTESIAN_POINT ( 'NONE',  ( 1.716621854089026344, 2.046377219401524616, 0.7848826361863747714 ) ) ;
#207734 = CARTESIAN_POINT ( 'NONE',  ( 6.883263157960364254, 2.038911835798001171, 2.358809022084580764 ) ) ;
#207735 = CARTESIAN_POINT ( 'NONE',  ( 3.274574482517400575, -1.349127789868936222, 1.816123189252472958 ) ) ;
#207736 = CARTESIAN_POINT ( 'NONE',  ( -7.263417608619167076, 9.497073181520933716, -1.599625672291263179 ) ) ;
#207737 = CARTESIAN_POINT ( 'NONE',  ( -0.6823417656250212460, 4.363541667008085767, 1.181850606188767472 ) ) ;
#207738 = CARTESIAN_POINT ( 'NONE',  ( 5.638349000628050334, 7.351887578364292075, 1.232751772250343381 ) ) ;
#207739 = CARTESIAN_POINT ( 'NONE',  ( 1.499999999999997113, 12.64583333333333215, -0.8660254037844378194 ) ) ;
#207740 = CARTESIAN_POINT ( 'NONE',  ( 5.722950238744187956, 9.690876021928001904, 0.7216878364870317197 ) ) ;
#207741 = CARTESIAN_POINT ( 'NONE',  ( 4.604631121011967920, 1.368492104089440442, -1.122162792211104820 ) ) ;
#207742 = CARTESIAN_POINT ( 'NONE',  ( 8.666686507633574621, 11.13422023037111330, 1.599625672291281386 ) ) ;
#207743 = CARTESIAN_POINT ( 'NONE',  ( 0.6046866811788155216, -0.7097959115549393738, -1.982883793842766362 ) ) ;
#207745 = CARTESIAN_POINT ( 'NONE',  ( -1.500000000000013101, 1.420833333333354043, 0.8660254037844403729 ) ) ;
#207744 = CARTESIAN_POINT ( 'NONE',  ( -1.364683531250000748, 10.35937500034139802, 0.000000000000000000 ) ) ;
#207746 = CARTESIAN_POINT ( 'NONE',  ( -5.743814354044916470, 6.730146830254374990, -1.199719254218453823 ) ) ;
#207747 = CARTESIAN_POINT ( 'NONE',  ( 6.398064575937244314, -0.9530261711272209890, -1.777004751544956962 ) ) ;
#207748 = VERTEX_POINT ( 'NONE', #24247 ) ;
#207749 = CARTESIAN_POINT ( 'NONE',  ( 7.632877294813741109, 8.007371053478589573, 1.040834085586084257E-14 ) ) ;
#207750 = EDGE_CURVE ( 'NONE', #78850, #56668, #155313, .T. ) ;
#207751 = CARTESIAN_POINT ( 'NONE',  ( 8.561083932025322696, 12.07534945641652158, -1.199719254218446718 ) ) ;
#207752 = CARTESIAN_POINT ( 'NONE',  ( 5.119927267529915227, -1.001353885182048931, -1.579878405157906673 ) ) ;
#207753 = CARTESIAN_POINT ( 'NONE',  ( 3.959880360806608213, -0.6057208360459276353, 1.979630382156400303 ) ) ;
#207754 = AXIS2_PLACEMENT_3D ( 'NONE', #29413, #110722, #95504 ) ;
#207755 = CARTESIAN_POINT ( 'NONE',  ( -6.089020385868862739, 8.197219431637373432, -1.443375672974066548 ) ) ;
#207756 = CARTESIAN_POINT ( 'NONE',  ( 8.158255747121103241, 10.54105100977322174, 1.599625672291281386 ) ) ;
#207757 = CARTESIAN_POINT ( 'NONE',  ( -9.642873567817536795, 12.27310513391906532, 1.599625672291281386 ) ) ;
#207758 = CARTESIAN_POINT ( 'NONE',  ( 8.167861197590044142, 8.493869250135347215, 0.000000000000000000 ) ) ;
#207759 = CARTESIAN_POINT ( 'NONE',  ( -4.911494110671301705, 4.698710846044690470, -0.3627449832724688461 ) ) ;
#207760 = CARTESIAN_POINT ( 'NONE',  ( 0.6823417656249899377, 5.488541667008087543, -1.181850606188754593 ) ) ;
#207761 = CARTESIAN_POINT ( 'NONE',  ( 3.965250677406896962, 1.681448970545707855, 1.010551734412237446 ) ) ;
#207762 = CARTESIAN_POINT ( 'NONE',  ( 1.528672481244568448, 1.986742605292156405, -0.3418812301651391605 ) ) ;
#207763 = EDGE_CURVE ( 'NONE', #202900, #112905, #2922, .T. ) ;
#207764 = CARTESIAN_POINT ( 'NONE',  ( 1.299038105676669330, 5.999999999999998224, 0.7500000000000006661 ) ) ;
#207765 = CARTESIAN_POINT ( 'NONE',  ( 6.639320575229254118, 2.070803455257670844, 2.204946390281757207 ) ) ;
#207766 = CARTESIAN_POINT ( 'NONE',  ( 0.6670070365902281972, 0.1896921041569209765, -1.860926112923621201 ) ) ;
#207767 = CARTESIAN_POINT ( 'NONE',  ( -1.201851678989727383E-14, 3.696875000341422801, -1.575800808251660134 ) ) ;
#207768 = CARTESIAN_POINT ( 'NONE',  ( 3.322524176979495980, -0.8198387518110359373, -1.838900561053190774 ) ) ;
#207770 = CARTESIAN_POINT ( 'NONE',  ( 3.849298028564145380, 0.2572143275579537591, -2.101468238826177615 ) ) ;
#207769 = CARTESIAN_POINT ( 'NONE',  ( -5.205967797967562483, 8.057084283395347768, 1.082531754730548412 ) ) ;
#207771 = CARTESIAN_POINT ( 'NONE',  ( 3.566232916275655640, 7.382631845622076305, 0.2048419657294417440 ) ) ;
#207772 = CARTESIAN_POINT ( 'NONE',  ( 4.633297751427938316, 0.003287558298453730800, -2.070544812459538253 ) ) ;
#207773 = CARTESIAN_POINT ( 'NONE',  ( 5.096939404094710468, 4.911127157724081371, 0.000000000000000000 ) ) ;
#207775 = FACE_OUTER_BOUND ( 'NONE', #207527, .T. ) ;
#207774 = CARTESIAN_POINT ( 'NONE',  ( 6.544877668737552945, -1.678188448499055685, -1.246566921223101865 ) ) ;
#207777 = ORIENTED_EDGE ( 'NONE', *, *, #31316, .T. ) ;
#207776 = CARTESIAN_POINT ( 'NONE',  ( 5.069292194207453583, 0.1776299070984053985, -1.816928125296768393 ) ) ;
#207778 = CARTESIAN_POINT ( 'NONE',  ( 9.399880572976245574, 9.860948844760784482, 0.7998128361456462443 ) ) ;
#207779 = CARTESIAN_POINT ( 'NONE',  ( 2.030969412801289842, 8.463209591663510167, -2.499999999999995115 ) ) ;
#207780 = AXIS2_PLACEMENT_3D ( 'NONE', #118108, #99660, #198208 ) ;
#207781 = CARTESIAN_POINT ( 'NONE',  ( -10.81685113641997020, 3.157239479008171035, 6.648618798508739935 ) ) ;
#207782 = CARTESIAN_POINT ( 'NONE',  ( -1.402160292154681736E-14, 11.98437500034140335, 1.575800808251682339 ) ) ;
#207783 = CARTESIAN_POINT ( 'NONE',  ( 6.604189988765333474, -0.8127675640051763573, 1.729262449380222222 ) ) ;
#207784 = CARTESIAN_POINT ( 'NONE',  ( -9.169391961543940539, 9.592045464756413509, 1.040834085586084257E-14 ) ) ;
#207785 = CARTESIAN_POINT ( 'NONE',  ( 5.120175567455225618, 9.125288595339771547, -0.7998128361456281477 ) ) ;
#207786 = CARTESIAN_POINT ( 'NONE',  ( -11.92619526248524409, 11.02744613914173932, -1.328859120100604585 ) ) ;
#207787 = CARTESIAN_POINT ( 'NONE',  ( 3.999292125906905859, 5.688926785023260102, 1.443375672974062551 ) ) ;
#207788 =( NAMED_UNIT ( * ) SI_UNIT ( $, .STERADIAN. ) SOLID_ANGLE_UNIT ( ) );
#207789 = CARTESIAN_POINT ( 'NONE',  ( 2.984766373302843778, 6.633977868828633717, -0.7998128361456291469 ) ) ;
#207790 = ORIENTED_EDGE ( 'NONE', *, *, #129145, .T. ) ;
#207791 = CARTESIAN_POINT ( 'NONE',  ( -5.478376588373717659, 8.549133898814758936, -1.199719254218452047 ) ) ;
#207793 = CARTESIAN_POINT ( 'NONE',  ( 7.367930134383754215, 7.560616343061329125, -0.7998128361456341429 ) ) ;
#207792 = CARTESIAN_POINT ( 'NONE',  ( 0.1981138333790652684, -9.280569609800584985, -9.498748750704418597 ) ) ;
#207794 = CARTESIAN_POINT ( 'NONE',  ( -2.679285714285713826, -0.4970443252110337551, -0.09999999999999592548 ) ) ;
#207795 = CARTESIAN_POINT ( 'NONE',  ( 0.1394461523057500818, 4.098109337479769465, -2.274588453029251500 ) ) ;
#207796 = CARTESIAN_POINT ( 'NONE',  ( -6.616015773788831211, 7.781401826584148473, 1.082531754730549967 ) ) ;
#207797 = CARTESIAN_POINT ( 'NONE',  ( 2.672928840188529609, 6.270167413528593414, 0.000000000000000000 ) ) ;
#207798 = CARTESIAN_POINT ( 'NONE',  ( 2.184365610098043309, 1.138103218778206971, -1.607087707149345901 ) ) ;
#207799 = CARTESIAN_POINT ( 'NONE',  ( 3.919546125582054508, -1.392558991000433011, -1.458545569310132350 ) ) ;
#207800 = CARTESIAN_POINT ( 'NONE',  ( -8.182509401047415309, 9.505014708432145909, 1.199719254218462483 ) ) ;
#207801 = CARTESIAN_POINT ( 'NONE',  ( 6.827182134110200806, 2.035520418778674845, 2.394189263408800450 ) ) ;
#207802 = CARTESIAN_POINT ( 'NONE',  ( 4.066501749483540706, -2.044453849244652233, -0.7895499924894524568 ) ) ;
#207803 = CARTESIAN_POINT ( 'NONE',  ( 1.403658749385964244, 1.209764585679671933, 1.481909061747192391 ) ) ;
#207804 = CARTESIAN_POINT ( 'NONE',  ( 1.940333228260374021, 1.905070304733847752, 0.2851023952017122665 ) ) ;
#207805 = CARTESIAN_POINT ( 'NONE',  ( -7.621654909176601045, 12.04368116068139472, 0.7998128361456481317 ) ) ;
#207806 = PRESENTATION_STYLE_ASSIGNMENT (( #43216 ) ) ;
#207807 = CARTESIAN_POINT ( 'NONE',  ( 0.2333540202161220045, 5.723122673495201873, -2.639760918834464398 ) ) ;
#207808 = CARTESIAN_POINT ( 'NONE',  ( 7.204675194429079505E-15, -1.487500000000000044, -3.475000000000000089 ) ) ;
#207810 = EDGE_CURVE ( 'NONE', #73904, #166401, #74039, .T. ) ;
#207809 = CARTESIAN_POINT ( 'NONE',  ( 6.259060471003163428, 10.45398764947904624, -0.7998128361456291469 ) ) ;
#207811 = CARTESIAN_POINT ( 'NONE',  ( 5.555090253297246150, 7.504024600312024340, 1.599625672291267398 ) ) ;
#207812 = CARTESIAN_POINT ( 'NONE',  ( -7.037870247915987143, -8.199999999999986855, 6.381095703207952496 ) ) ;
#207813 = CARTESIAN_POINT ( 'NONE',  ( 5.017926250833595780, 7.907978821730911712, -1.082531754730548412 ) ) ;
#207814 = ORIENTED_EDGE ( 'NONE', *, *, #7153, .F. ) ;
#207816 = CARTESIAN_POINT ( 'NONE',  ( 2.860023507607223792, 0.7224298503675909977, -1.879176508647899535 ) ) ;
#207815 = CARTESIAN_POINT ( 'NONE',  ( 5.741722636381445533, 1.839460222191912964, 0.08393339073512617876 ) ) ;
#207817 = CARTESIAN_POINT ( 'NONE',  ( 4.288600692895239597, -2.201063653074202708, 0.6618141117178658606 ) ) ;
#207819 = CARTESIAN_POINT ( 'NONE',  ( 3.344433574756133787, -1.832611177030788685, -0.3225857369167430821 ) ) ;
#207818 = CARTESIAN_POINT ( 'NONE',  ( -0.1288028175206725467, 2.854926803129751001, -2.761885894952537779 ) ) ;
#207820 = CARTESIAN_POINT ( 'NONE',  ( 7.526711554241970248, 8.810193563817646734, -1.199719254218452047 ) ) ;
#207821 = DIRECTION ( 'NONE',  ( 0.000000000000000000, -1.000000000000000000, -9.023263958591317418E-17 ) ) ;
#207822 = CARTESIAN_POINT ( 'NONE',  ( 6.416268857797894576, -1.911816439625917852, 0.05404522429636184067 ) ) ;
#207823 = CARTESIAN_POINT ( 'NONE',  ( -6.672584156219988571, 10.93643194889866521, -0.7998128361456291469 ) ) ;
#207824 = CARTESIAN_POINT ( 'NONE',  ( -4.665414256878287702, 8.457084043084382330, -0.7216878364870338292 ) ) ;
#207825 = CARTESIAN_POINT ( 'NONE',  ( 5.495677747024089399, -2.090933975967598446, 0.001106539467419370270 ) ) ;
#207826 = CARTESIAN_POINT ( 'NONE',  ( 5.314433026876846711, 9.143996264757578984, -0.7216878364870267237 ) ) ;
#207827 = ORIENTED_EDGE ( 'NONE', *, *, #185659, .F. ) ;
#207828 = CARTESIAN_POINT ( 'NONE',  ( 1.926045559616737846, 3.520657594693878956, 0.3999999999999681033 ) ) ;
#207829 = CARTESIAN_POINT ( 'NONE',  ( 0.4999999999999952260, 3.172938907704321743, -0.4000000000000062395 ) ) ;
#207830 = CARTESIAN_POINT ( 'NONE',  ( 6.164645834669005175, -1.214467819493704415, 1.225147371335724156 ) ) ;
#207831 = CARTESIAN_POINT ( 'NONE',  ( -5.436983294280064882, 6.301900917203534291, 1.199719254218450271 ) ) ;
#207832 = AXIS2_PLACEMENT_3D ( 'NONE', #77633, #209750, #28896 ) ;
#207833 = CARTESIAN_POINT ( 'NONE',  ( 1.793227186479518398, 1.284509341651525638, -1.165198513391290103 ) ) ;
#207834 = DIRECTION ( 'NONE',  ( 1.000000000000000000, 1.725633230170963762E-31, 8.638326563840814399E-31 ) ) ;
#207835 = FACE_OUTER_BOUND ( 'NONE', #209688, .T. ) ;
#207836 = AXIS2_PLACEMENT_3D ( 'NONE', #64893, #198088, #101666 ) ;
#207837 = DIRECTION ( 'NONE',  ( 0.000000000000000000, 0.000000000000000000, 1.000000000000000000 ) ) ;
#207838 = CARTESIAN_POINT ( 'NONE',  ( 5.313404054176891655, -1.830285002536722549, -1.167499077736388724 ) ) ;
#207839 = CARTESIAN_POINT ( 'NONE',  ( 4.055160972438559774, -1.518969423100406946, -1.012540670841777013 ) ) ;
#207840 = CARTESIAN_POINT ( 'NONE',  ( 2.184356868638567928, 1.133688150830698627, -1.600809071968431807 ) ) ;
#207841 = AXIS2_PLACEMENT_3D ( 'NONE', #113666, #198031, #65872 ) ;
#207842 = CARTESIAN_POINT ( 'NONE',  ( -11.48243876534946040, 9.799999999999998934, -3.200000000000001510 ) ) ;
#207843 = CARTESIAN_POINT ( 'NONE',  ( -8.618179199781044630, 13.20629283305325963, 0.7998128361456341429 ) ) ;
#207844 = CARTESIAN_POINT ( 'NONE',  ( 6.564118927310645724, 10.80988918183778225, -0.7998128361456291469 ) ) ;
#207845 = CARTESIAN_POINT ( 'NONE',  ( 3.053504691927158898, -1.869126254513186591, 1.001442229663196182 ) ) ;
#207846 = CARTESIAN_POINT ( 'NONE',  ( 6.827182134110224787, 2.015384445464900587, 2.492173930675382287 ) ) ;
#207847 = PRESENTATION_STYLE_ASSIGNMENT (( #172174 ) ) ;
#207848 = CARTESIAN_POINT ( 'NONE',  ( -5.526577223899823643, 6.240148858909590146, -0.9599604131041916677 ) ) ;
#207849 = CARTESIAN_POINT ( 'NONE',  ( 1.182579820358391931, 1.236233925375467058, -1.660450453320160058 ) ) ;
#207851 = CARTESIAN_POINT ( 'NONE',  ( -1.500000000000001110, 14.05208333401613530, 0.8660254037844419273 ) ) ;
#207850 = DIRECTION ( 'NONE',  ( 0.000000000000000000, 1.000000000000000000, 0.000000000000000000 ) ) ;
#207853 = ORIENTED_EDGE ( 'NONE', *, *, #180453, .T. ) ;
#207852 = CARTESIAN_POINT ( 'NONE',  ( 3.317226741293349157, 1.750174726733638497, -1.367746370967915626 ) ) ;
#207854 = CARTESIAN_POINT ( 'NONE',  ( 0.6164066528375180543, 0.1772060041554945342, 2.291936309153388862 ) ) ;
#207856 = CARTESIAN_POINT ( 'NONE',  ( 0.4265131056294459433, -1.285834093136655643, 1.481649512794058543 ) ) ;
#207855 = CARTESIAN_POINT ( 'NONE',  ( 2.523789150438203510, 6.096171108819874007, 0.7998128361456462443 ) ) ;
#207858 = CARTESIAN_POINT ( 'NONE',  ( 0.000000000000000000, -0.08749999999999961975, -4.012584370867899430 ) ) ;
#207857 = CARTESIAN_POINT ( 'NONE',  ( 5.391302360089590628, 6.318882837306503575, -1.199719254218452047 ) ) ;
#207859 = EDGE_CURVE ( 'NONE', #162762, #59123, #203680, .T. ) ;
#207860 = CARTESIAN_POINT ( 'NONE',  ( 1.474420525118734323E-15, 14.99987590242439595, 11.68000000000000327 ) ) ;
#207861 = DIRECTION ( 'NONE',  ( 1.000000000000000000, 2.090028284309406390E-15, 0.000000000000000000 ) ) ;
#207862 = CARTESIAN_POINT ( 'NONE',  ( -1.651133652709660948, -0.8391591008036085597, 1.022755049771800984 ) ) ;
#207863 = CARTESIAN_POINT ( 'NONE',  ( -0.2104748580754183807, 2.005809028216706924, -2.517884123765606663 ) ) ;
#207864 = CARTESIAN_POINT ( 'NONE',  ( 2.537784596217841138, 0.8154259780687975745, -1.519840121599738803 ) ) ;
#207865 = CARTESIAN_POINT ( 'NONE',  ( 0.9015777671340443611, -1.966303774932298021, 0.4465067697373495403 ) ) ;
#207866 = CARTESIAN_POINT ( 'NONE',  ( 2.831036414133382806, 0.8244386821347724492, -2.145926533794308533 ) ) ;
#207867 = CARTESIAN_POINT ( 'NONE',  ( 3.866728509311831985, -1.522874988181441180, 1.673262526929709670 ) ) ;
#207868 = CARTESIAN_POINT ( 'NONE',  ( 5.215496775961459441, -0.3099510095366068696, 2.083004237123146307 ) ) ;
#207869 = CARTESIAN_POINT ( 'NONE',  ( -5.966997003790221576, 9.015228033513643879, -1.082531754730549967 ) ) ;
#207870 = VERTEX_POINT ( 'NONE', #61042 ) ;
#207871 = CARTESIAN_POINT ( 'NONE',  ( 3.954177229731909549, 0.6350985098286399122, 1.652046152411037694 ) ) ;
#207872 = EDGE_CURVE ( 'NONE', #210693, #106547, #191021, .T. ) ;
#207874 = CARTESIAN_POINT ( 'NONE',  ( 6.614806897001766828, -0.1637801000826353548, 2.256214727502181994 ) ) ;
#207873 = CARTESIAN_POINT ( 'NONE',  ( 3.214691819771663628, 6.764574533126651801, -0.7216878364870338292 ) ) ;
#207875 = CARTESIAN_POINT ( 'NONE',  ( 5.912015133600425187, 1.233162958052456348, -1.367321061651972869 ) ) ;
#207876 = CARTESIAN_POINT ( 'NONE',  ( -3.764360206088648297, 7.543504007078730922, -0.7998128361456281477 ) ) ;
#207877 = CARTESIAN_POINT ( 'NONE',  ( 1.499999999999987121, 3.795833333333356929, -0.8660254037844262731 ) ) ;
#207878 = CARTESIAN_POINT ( 'NONE',  ( 4.962908505822442251, 0.2168217322565079985, -2.180687389885840322 ) ) ;
#207879 = CARTESIAN_POINT ( 'NONE',  ( -2.137381772448751605, 5.645362501165475777, -0.7998128361456281477 ) ) ;
#207880 = CARTESIAN_POINT ( 'NONE',  ( 0.000000000000000000, 6.062865449010541141, 0.000000000000000000 ) ) ;
#207881 = CARTESIAN_POINT ( 'NONE',  ( 6.092251258522619395, 1.023830597077223903, -1.799436568697235783 ) ) ;
#207882 = CARTESIAN_POINT ( 'NONE',  ( 0.5148617154710420918, 0.1531739628206352510, 2.010800830040265996 ) ) ;
#207883 = CARTESIAN_POINT ( 'NONE',  ( -1.001543065824772872E-14, 4.821875000341419693, 1.575800808251672791 ) ) ;
#207884 = CARTESIAN_POINT ( 'NONE',  ( 2.719263968888342653, -0.1887435353777958125, 1.917229668948018162 ) ) ;
#207885 = CARTESIAN_POINT ( 'NONE',  ( -0.6823417656250039265, 9.817708333674735499, -1.181850606188755259 ) ) ;
#207886 = CARTESIAN_POINT ( 'NONE',  ( -4.460269349215930212, 4.305995116947750390, 1.214306433183764966E-14 ) ) ;
#207887 = CARTESIAN_POINT ( 'NONE',  ( -0.01689291694152022724, -1.444339507245323118, 1.687895485215410885 ) ) ;
#207888 = ORIENTED_EDGE ( 'NONE', *, *, #118553, .F. ) ;
#207890 = DIRECTION ( 'NONE',  ( 1.000000000000000000, -0.000000000000000000, 1.224646799147353207E-16 ) ) ;
#207889 = CARTESIAN_POINT ( 'NONE',  ( -3.187575512988701565, 6.732938841879847480, 0.000000000000000000 ) ) ;
#207891 = CARTESIAN_POINT ( 'NONE',  ( 3.493197133815315603, 7.227147089426516402, -0.7998128361456291469 ) ) ;
#207892 = CARTESIAN_POINT ( 'NONE',  ( -15.75000000000000000, 12.69999999999999929, -1.400000000000001910 ) ) ;
#207893 = DIRECTION ( 'NONE',  ( -3.497202527569253358E-15, -0.000000000000000000, -1.000000000000000000 ) ) ;
#207894 = CARTESIAN_POINT ( 'NONE',  ( 10.19581844778559621, 10.80880345838189527, 6.242887950171588152 ) ) ;
#207895 = CARTESIAN_POINT ( 'NONE',  ( 9.693716643646590470, 12.33242205571964512, 1.443375672974076540 ) ) ;
#207896 = CARTESIAN_POINT ( 'NONE',  ( 0.7659737006216191801, -1.952758744216346765, 0.1886366088557633325 ) ) ;
#207897 = CARTESIAN_POINT ( 'NONE',  ( 1.364683531249988757, 1.696875000341414808, 0.000000000000000000 ) ) ;
#207898 = CARTESIAN_POINT ( 'NONE',  ( -15.75000000000000000, 11.29999999999998117, 3.199999999999997957 ) ) ;
#207899 = CARTESIAN_POINT ( 'NONE',  ( 5.353941776413853937, -0.7077614321437855072, 1.829919609802006741 ) ) ;
#207900 = CARTESIAN_POINT ( 'NONE',  ( -8.779068160048691283, 10.20099992726700933, -1.199719254218446718 ) ) ;
#207902 = ADVANCED_FACE ( 'NONE', ( #93566 ), #108795, .T. ) ;
#207901 = CIRCLE ( 'NONE', #187190, 0.09999999999999982514 ) ;
#207903 = CARTESIAN_POINT ( 'NONE',  ( -6.087247782411500552, 7.164505836643929371, 1.082531754730549967 ) ) ;
#207904 = CARTESIAN_POINT ( 'NONE',  ( 6.579002408576895000, -0.1006694238701970334, -2.159482418181729813 ) ) ;
#207906 = ORIENTED_EDGE ( 'NONE', *, *, #147938, .T. ) ;
#207905 = CARTESIAN_POINT ( 'NONE',  ( -0.08269815893113435790, -5.360092950639682385, -10.99976946526262900 ) ) ;
#207907 = CARTESIAN_POINT ( 'NONE',  ( -1.201851678989727383E-14, 5.696875000341416140, -1.575800808251660134 ) ) ;
#207908 = CARTESIAN_POINT ( 'NONE',  ( 6.837195077073701555, -1.761838062178729070, 0.8845485525767071699 ) ) ;
#207909 = CARTESIAN_POINT ( 'NONE',  ( 6.204387268089465834, -1.258339971413184433, -1.193046581750532464 ) ) ;
#207911 = CARTESIAN_POINT ( 'NONE',  ( 3.421585747727782678, -1.306972202059282218, -1.759028276249123168 ) ) ;
#207910 = CARTESIAN_POINT ( 'NONE',  ( 1.360316468749988683, 0.2656250003413990202, -1.387778780781445676E-14 ) ) ;
#207912 = CARTESIAN_POINT ( 'NONE',  ( 4.190657675959572614, -2.281913287836007331, -0.3425691479843806508 ) ) ;
#207913 = CARTESIAN_POINT ( 'NONE',  ( 5.782513925583750769, -2.009559558911724775, -0.4558285042701361589 ) ) ;
#207914 = CARTESIAN_POINT ( 'NONE',  ( 2.027192386733965179, -1.268372964689370663, -1.470586975900304516 ) ) ;
#207915 = CARTESIAN_POINT ( 'NONE',  ( -3.904385050611244079, 7.498940292447679568, 1.040834085586084257E-14 ) ) ;
#207916 = PRODUCT ( 'negative coil', 'negative coil', '', ( #105645 ) ) ;
#207917 =( LENGTH_UNIT ( ) NAMED_UNIT ( * ) SI_UNIT ( .MILLI., .METRE. ) );
#207918 = CARTESIAN_POINT ( 'NONE',  ( 4.834296457332984076, -1.136628438424293508, -1.790084250976264002 ) ) ;
#207919 = CARTESIAN_POINT ( 'NONE',  ( -1.355252715606880543E-15, 3.019799309333170978, 12.05075272264442177 ) ) ;
#207920 = CARTESIAN_POINT ( 'NONE',  ( 3.744767666119628746, 2.000857235306313875, -0.2496062519145719194 ) ) ;
#207921 = CARTESIAN_POINT ( 'NONE',  ( -6.046573321570485327, 6.156683084694754449, 0.000000000000000000 ) ) ;
#207922 = CARTESIAN_POINT ( 'NONE',  ( -5.772739544368596043, 9.956889578397179363, -0.7998128361456362523 ) ) ;
#207923 = CARTESIAN_POINT ( 'NONE',  ( 8.778014389843965759, 12.32843499053828928, 1.199719254218450271 ) ) ;
#207924 = CARTESIAN_POINT ( 'NONE',  ( 0.2404813148422607627, 0.3085585699703840556, 1.799268721412583316 ) ) ;
#207925 = CARTESIAN_POINT ( 'NONE',  ( -6.934069218746458318, 7.054445274817795486, -0.7998128361456362523 ) ) ;
#207926 = CARTESIAN_POINT ( 'NONE',  ( -5.599738924909661186, 5.745725798494749625, 0.2540040342395213369 ) ) ;
#207927 = CARTESIAN_POINT ( 'NONE',  ( 1.566031286093723995, 8.750666943143137644, -2.469538363634776079 ) ) ;
#207928 = ORIENTED_EDGE ( 'NONE', *, *, #87277, .F. ) ;
#207929 = CARTESIAN_POINT ( 'NONE',  ( 5.629779042149522184, -1.305697561153400965, -1.594503516446880154 ) ) ;
#207930 = CARTESIAN_POINT ( 'NONE',  ( -5.899206235277530297, 9.896508017883515862, 0.7216878364870267237 ) ) ;
#207931 = CARTESIAN_POINT ( 'NONE',  ( 6.000769315822030740E-16, -4.000000000000005329, 4.899999999999999467 ) ) ;
#207932 = CARTESIAN_POINT ( 'NONE',  ( -4.952806187693842510, 4.672695395264567786, 0.7998128361456341429 ) ) ;
#207933 = DIRECTION ( 'NONE',  ( 0.000000000000000000, 0.000000000000000000, 1.000000000000000000 ) ) ;
#207934 = CARTESIAN_POINT ( 'NONE',  ( 4.793620647492384812, 1.883690600511141566, -0.7290150168693364519 ) ) ;
#207936 = ORIENTED_EDGE ( 'NONE', *, *, #108550, .F. ) ;
#207935 = CARTESIAN_POINT ( 'NONE',  ( 1.499999999999989120, 0.7750000000000187850, 0.000000000000000000 ) ) ;
#207938 = CARTESIAN_POINT ( 'NONE',  ( 9.083599731475983319, 11.62061899152058686, 1.443375672974076540 ) ) ;
#207937 = CARTESIAN_POINT ( 'NONE',  ( -5.679940009482361774, 5.591294530676332641, 0.7998128361456281477 ) ) ;
#207939 = CARTESIAN_POINT ( 'NONE',  ( 4.794779880727245036, 8.745660294157122649, -0.7998128361456281477 ) ) ;
#207940 = MECHANICAL_DESIGN_GEOMETRIC_PRESENTATION_REPRESENTATION (  '', ( #200954 ), #45308 ) ;
#207941 = CARTESIAN_POINT ( 'NONE',  ( 4.733308493599470701, -1.885100903509504544, 0.8332785242166717010 ) ) ;
#207942 = CARTESIAN_POINT ( 'NONE',  ( 2.777970385693105726, 1.728001979019553103, -1.038993764437286416 ) ) ;
#207943 = VERTEX_POINT ( 'NONE', #56775 ) ;
#207944 = LINE ( 'NONE', #13997, #97317 ) ;
#207945 = CARTESIAN_POINT ( 'NONE',  ( 3.506755287428983792, 7.242964935309132990, 1.040834085586084257E-14 ) ) ;
#207947 = ORIENTED_EDGE ( 'NONE', *, *, #1373, .T. ) ;
#207946 = CARTESIAN_POINT ( 'NONE',  ( -11.43209210103587559, 9.944039240160824633, 3.649125173352122609 ) ) ;
#207948 = CARTESIAN_POINT ( 'NONE',  ( 5.819104682239041537, 7.212836251160942957, -1.171789181936284896 ) ) ;
#207949 = CARTESIAN_POINT ( 'NONE',  ( 3.286482353612128815, -1.943773746517188039, 0.5350062169211177165 ) ) ;
#207950 = CARTESIAN_POINT ( 'NONE',  ( 2.501689010688646242, -0.7045654096689784041, -1.701190496055771550 ) ) ;
#207951 = CARTESIAN_POINT ( 'NONE',  ( 0.9092882892361430214, 1.744143012382966207, -1.511207573902007884 ) ) ;
#207952 = CARTESIAN_POINT ( 'NONE',  ( 4.037295881819344956, 7.932205305423046582, -0.7998128361456362523 ) ) ;
#207953 = CARTESIAN_POINT ( 'NONE',  ( 3.901784996602038813, -0.6316019492740264640, 2.067237329103743804 ) ) ;
#207954 = CARTESIAN_POINT ( 'NONE',  ( -5.228640796364566690, 9.251831362400652736, -0.7998128361456231517 ) ) ;
#207955 = EDGE_LOOP ( 'NONE', ( #189553, #15245, #61614, #142652 ) ) ;
#207956 = CARTESIAN_POINT ( 'NONE',  ( 0.3282377607281112275, 2.323664549684620440, 1.224999999999963229 ) ) ;
#207957 = CARTESIAN_POINT ( 'NONE',  ( 1.533845512228737551, 0.9248708299973290581, -1.625957014461040906 ) ) ;
#207958 = CARTESIAN_POINT ( 'NONE',  ( 5.629747345311447937, -1.250075164085572954, -1.524477324586423377 ) ) ;
#207960 = CARTESIAN_POINT ( 'NONE',  ( 8.636180661780656465, 11.09863007687603087, -1.443375672974052559 ) ) ;
#207959 = CARTESIAN_POINT ( 'NONE',  ( -0.6823417656250212460, 5.301041667008086655, 1.181850606188767472 ) ) ;
#207962 = CARTESIAN_POINT ( 'NONE',  ( 0.9091299924109221831, 1.668792687453458878, -1.444214864661397035 ) ) ;
#207961 = CARTESIAN_POINT ( 'NONE',  ( -5.656776405399756236, 7.622658444431597680, -1.599625672291256295 ) ) ;
#207963 = DIRECTION ( 'NONE',  ( 1.039099362110107450E-15, 1.000000000000000000, -4.583713267641621330E-32 ) ) ;
#207964 = CARTESIAN_POINT ( 'NONE',  ( 5.678167406024951624, 5.518950149984223508, 0.7998128361456341429 ) ) ;
#207965 = CARTESIAN_POINT ( 'NONE',  ( -4.629219384062206011, 7.488174150459498968, -1.199719254218452047 ) ) ;
#207966 = CARTESIAN_POINT ( 'NONE',  ( 6.539320575229278454, 0.5749733277502915296, 2.156147827957733742 ) ) ;
#207967 = CARTESIAN_POINT ( 'NONE',  ( 5.295764336479223289, -0.7102129355434207980, 1.839261741220117097 ) ) ;
#207968 = CARTESIAN_POINT ( 'NONE',  ( 5.549573066657292664, -1.816037693736268333, -1.423817124750816232 ) ) ;
#207969 = CARTESIAN_POINT ( 'NONE',  ( 6.232830220009587308, -1.767433141015135822, -0.5829711297899267120 ) ) ;
#207970 = CARTESIAN_POINT ( 'NONE',  ( 3.608308625203029862, 2.062741128266020851, 0.004805803398660184710 ) ) ;
#207971 = CARTESIAN_POINT ( 'NONE',  ( 6.643132081016124069, 7.813037518349371879, 1.082531754730558626 ) ) ;
#207972 = CARTESIAN_POINT ( 'NONE',  ( 3.854260808034858155, 7.718664386007802136, -0.7998128361456362523 ) ) ;
#207973 = CARTESIAN_POINT ( 'NONE',  ( 6.749980374757213575, 8.968339418673846097, 1.599625672291268286 ) ) ;
#207974 = CARTESIAN_POINT ( 'NONE',  ( 1.364683531249988535, 1.426041667008083991, 0.7879004041258500513 ) ) ;
#207975 = CARTESIAN_POINT ( 'NONE',  ( -4.304609288505035103, 14.53049063336417746, 11.21048893683339642 ) ) ;
#207976 = CARTESIAN_POINT ( 'NONE',  ( 4.650083499362856365, 8.368921815991249957, 0.7216878364870438212 ) ) ;
#207977 = CARTESIAN_POINT ( 'NONE',  ( 5.811019572999191141, -1.715256576162796032, 1.331060940585542030 ) ) ;
#207978 = DIRECTION ( 'NONE',  ( -1.000000000000000000, -1.725633230170963762E-31, -8.638326563840814399E-31 ) ) ;
#207980 = CARTESIAN_POINT ( 'NONE',  ( 4.212339636135824961, 1.685202893791247769, 0.7422218904534692019 ) ) ;
#207979 = CARTESIAN_POINT ( 'NONE',  ( -4.039966587192274083, 5.736380323189513852, 1.443375672974064550 ) ) ;
#207982 = DIRECTION ( 'NONE',  ( -0.6507913734559641616, -0.7592566023653004592, 0.000000000000000000 ) ) ;
#207981 = CARTESIAN_POINT ( 'NONE',  ( -10.02012520139310681, 1.794419290072776896, -6.231960695612073664 ) ) ;
#207983 = CARTESIAN_POINT ( 'NONE',  ( 6.286699343557897279, 1.907799665397521105, -1.078441415684105120 ) ) ;
#207984 = DIRECTION ( 'NONE',  ( 0.000000000000000000, 0.000000000000000000, -1.000000000000000000 ) ) ;
#207985 = CARTESIAN_POINT ( 'NONE',  ( 0.2107632190684857465, -0.9678151086435597961, -2.042474306115627414 ) ) ;
#207986 = CARTESIAN_POINT ( 'NONE',  ( -3.978769281187482854, 7.845005453061479450, 0.1301786893823601021 ) ) ;
#207987 = DIRECTION ( 'NONE',  ( 1.000000000000000000, 0.000000000000000000, -5.421010862427519212E-16 ) ) ;
#207988 = CARTESIAN_POINT ( 'NONE',  ( 6.296370465541430761, 6.973533528358998979, 0.9269300130883666444 ) ) ;
#207989 = CARTESIAN_POINT ( 'NONE',  ( -5.763624699140894592, 5.896852701852039580, -0.7216878364870338292 ) ) ;
#207990 = CARTESIAN_POINT ( 'NONE',  ( 2.929970594329034395, 6.432399770110250437, -0.7216878364870338292 ) ) ;
#207991 =( BOUNDED_SURFACE ( )  B_SPLINE_SURFACE ( 1, 2, ( 
 ( #30316, #96401, #12972, #128956, #76909, #147266, #145164, #213298, #144108, #130024, #143035, #63869, #209030, #127909, #177639, #161389, #64925, #162451, #131074, #113762, #112691, #176563, #28172, #197062, #11912, #14027, #212236, #193861, #126828, #31382, #196015, #15099, #60665, #79048, #47651, #210102, #77985, #94268, #179766, #192785, #111626, #29247, #48700, #97458, #62794, #93203, #194935, #163513, #81188, #114814, #149385, #16154, #199169, #198119, #182941, #67032, #132111, #136349, #148330, #85444, #49750, #35619, #99571, #967, #50815, #17223, #115877, #65962, #3098, #151529, #133169, #32439, #164569, #200242, #19364, #69168, #54019, #116941, #181862, #86514, #2029, #202370, #83300, #52942, #68098, #34557, #84381, #100628, #201302, #134233, #36685, #185060, #98507, #120158, #119079, #102772, #33498, #166704, #82239, #70236, #51892, #18295, #150468, #135288, #118015, #184004, #165635, #101697, #214330, #167767, #168827, #20431, #152579, #4166, #170961, #22561, #141716, #88666, #9532, #104920, #207726, #8455, #75605, #91884, #154726, #59349, #72383, #108173, #87588, #103841, #190402, #71303, #122316, #206656, #186134, #173122, #174199, #6309, #138482, #37769, #189348, #187208, #40988, #169890, #137416, #203435, #42060, #74543, #25772, #38837, #204504, #56154, #188273, #39914, #55089, #24703, #121238, #90805, #89745, #106023, #21479, #156869, #157939, #153660, #5229, #172044, #23637, #155794, #73457, #140643, #7378, #139559, #205586, #57223, #58288, #123383, #107099, #124445, #194674, #63617, #47392, #31133, #13783, #211977, #144909, #126572, #111372, #79858, #129772, #78787, #28990, #125504, #193612, #209844, #192532, #60411, #162196, #26842, #113505, #208781, #179513, #195755, #44186, #96145, #160053, #177376, #45254, #145967, #80932, #191467, #147023, #97208, #163260, #76661, #95076, #175256, #14842, #161125, #127648, #12711, #112434, #176314, #27918, #142775, #94014, #109248, #110306, #11657, #77730, #210916, #143852, #61483, #62543, #213046, #128705, #43132, #46318, #92945, #158990, #10586, #178447 ),
 ( #30055, #117765, #164315, #67839, #131857, #181612, #16967, #49496, #148076, #98258, #35365, #183756, #165374, #64675, #196812, #18037, #51641, #101440, #86260, #99324, #214082, #118819, #34302, #167514, #15906, #36435, #184806, #83048, #66769, #19111, #33241, #85189, #149123, #100375, #20173, #130821, #81988, #1782, #132910, #182681, #84124, #115617, #114568, #705, #65709, #198915, #201047, #180560, #133985, #48455, #168573, #32182, #50561, #199992, #197864, #116682, #166445, #150210, #151272, #2845, #152331, #68914, #135034, #52690, #102511, #103585, #124190, #4969, #185873, #53766, #89485, #155540, #138230, #39644, #202106, #58026, #55895, #190153, #54833, #40729, #119899, #189096, #136089, #186951, #88405, #72122, #41808, #7119, #25519, #106835, #107921, #173946, #120983, #91627, #104660, #140382, #37509, #169643, #8202, #21227, #154473, #24437, #3908, #205327, #206401, #38583, #203187, #69978, #73192, #71047, #139298, #87331, #153398, #137163, #74287, #172866, #170707, #22292, #6051, #204243, #122052, #188016, #105752, #56965, #171779, #123138, #23375, #90548, #156612, #62296, #129519, #30879, #113252, #179257, #76402, #159790, #45000, #128455, #142511, #11393, #157679, #9277, #46064, #75348, #158733, #194423, #12461, #95891, #79606, #63363, #112185, #29805, #177114, #10328, #143590, #178189, #161944, #111110, #61228, #141463, #77471, #27656, #208520, #92687, #13536, #59089, #145725, #26586, #211725, #195499, #60155, #47135, #192271, #209582, #127383, #207470, #125249, #191210, #126311, #42873, #193356, #43932, #28731, #110047, #108981, #94816, #175000, #176060, #93752, #160867, #78536, #144653, #210668, #165123, #146776, #134785, #66516, #99070, #16714, #83861, #147823, #213841, #114317, #65460, #80685, #164074, #15654, #180315, #82799, #98019, #81741, #131611, #52443, #197610, #200792, #49254, #148875, #198663, #67585, #115375, #448, #184555, #163006, #199737, #118569, #181369, #133730, #166184, #35105, #18850, #2592, #51383, #183496, #116429, #32993, #132659, #117504, #101176, #50311, #182422, #96958 ) ),
 .UNSPECIFIED., .F., .F., .T. ) 
 B_SPLINE_SURFACE_WITH_KNOTS ( ( 2, 2 ),
 ( 3, 2, 2, 2, 2, 2, 2, 2, 2, 2, 2, 2, 2, 2, 2, 2, 2, 2, 2, 2, 2, 2, 2, 2, 2, 2, 2, 2, 2, 2, 2, 2, 2, 2, 2, 2, 2, 2, 2, 2, 2, 2, 2, 2, 2, 2, 2, 2, 2, 2, 2, 2, 2, 2, 2, 2, 2, 2, 2, 2, 2, 2, 2, 2, 2, 2, 2, 2, 2, 2, 2, 2, 2, 2, 2, 2, 2, 2, 2, 2, 2, 2, 2, 2, 2, 2, 2, 2, 2, 2, 2, 2, 2, 2, 2, 2, 2, 2, 2, 2, 2, 2, 2, 2, 2, 2, 2, 2, 2, 2, 2, 2, 2, 2, 2, 2, 2, 2, 2, 2, 3 ),
 ( 0.000000000000000000, 1.000000000000000000 ),
 ( 0.000000000000000000, 0.008333333333333333218, 0.01666666666666666644, 0.02500000000000000139, 0.03333333333333333287, 0.04166666666666666435, 0.05000000000000000278, 0.05833333333333333426, 0.06666666666666666574, 0.07499999999999999722, 0.08333333333333332871, 0.09166666666666666019, 0.1000000000000000056, 0.1083333333333333370, 0.1166666666666666685, 0.1250000000000000000, 0.1333333333333333315, 0.1416666666666666630, 0.1499999999999999944, 0.1583333333333333259, 0.1666666666666666574, 0.1749999999999999889, 0.1833333333333333204, 0.1916666666666666796, 0.2000000000000000111, 0.2083333333333333426, 0.2166666666666666741, 0.2250000000000000056, 0.2333333333333333370, 0.2416666666666666685, 0.2500000000000000000, 0.2583333333333333592, 0.2666666666666666630, 0.2750000000000000222, 0.2833333333333333259, 0.2916666666666666852, 0.2999999999999999889, 0.3083333333333333481, 0.3166666666666666519, 0.3250000000000000111, 0.3333333333333333148, 0.3416666666666666741, 0.3499999999999999778, 0.3583333333333333370, 0.3666666666666666408, 0.3750000000000000000, 0.3833333333333333592, 0.3916666666666666630, 0.4000000000000000222, 0.4083333333333333259, 0.4166666666666666852, 0.4249999999999999889, 0.4333333333333333481, 0.4416666666666666519, 0.4500000000000000111, 0.4583333333333333148, 0.4666666666666666741, 0.4749999999999999778, 0.4833333333333333370, 0.4916666666666666408, 0.5000000000000000000, 0.5083333333333333037, 0.5166666666666667185, 0.5250000000000000222, 0.5333333333333333259, 0.5416666666666666297, 0.5500000000000000444, 0.5583333333333333481, 0.5666666666666666519, 0.5749999999999999556, 0.5833333333333333703, 0.5916666666666666741, 0.5999999999999999778, 0.6083333333333332815, 0.6166666666666666963, 0.6250000000000000000, 0.6333333333333333037, 0.6416666666666667185, 0.6500000000000000222, 0.6583333333333333259, 0.6666666666666666297, 0.6750000000000000444, 0.6833333333333333481, 0.6916666666666666519, 0.6999999999999999556, 0.7083333333333333703, 0.7166666666666666741, 0.7249999999999999778, 0.7333333333333332815, 0.7416666666666666963, 0.7500000000000000000, 0.7583333333333333037, 0.7666666666666667185, 0.7750000000000000222, 0.7833333333333333259, 0.7916666666666666297, 0.8000000000000000444, 0.8083333333333333481, 0.8166666666666666519, 0.8249999999999999556, 0.8333333333333333703, 0.8416666666666666741, 0.8499999999999999778, 0.8583333333333332815, 0.8666666666666666963, 0.8750000000000000000, 0.8833333333333333037, 0.8916666666666667185, 0.9000000000000000222, 0.9083333333333333259, 0.9166666666666666297, 0.9250000000000000444, 0.9333333333333333481, 0.9416666666666666519, 0.9499999999999999556, 0.9583333333333333703, 0.9666666666666666741, 0.9749999999999999778, 0.9833333333333332815, 0.9916666666666666963, 1.000000000000000000 ),
 .UNSPECIFIED. ) 
 GEOMETRIC_REPRESENTATION_ITEM ( )  RATIONAL_B_SPLINE_SURFACE ( (
 ( 1.000000000000000000, 0.8660254037844387076, 1.000000000000000000, 0.8660254037844387076, 1.000000000000000000, 0.8660254037844387076, 1.000000000000000000, 0.8660254037844387076, 1.000000000000000000, 0.8660254037844387076, 1.000000000000000000, 0.8660254037844387076, 1.000000000000000000, 0.8660254037844387076, 1.000000000000000000, 0.8660254037844387076, 1.000000000000000000, 0.8660254037844387076, 1.000000000000000000, 0.8660254037844387076, 1.000000000000000000, 0.8660254037844387076, 1.000000000000000000, 0.8660254037844387076, 1.000000000000000000, 0.8660254037844387076, 1.000000000000000000, 0.8660254037844387076, 1.000000000000000000, 0.8660254037844387076, 1.000000000000000000, 0.8660254037844387076, 1.000000000000000000, 0.8660254037844387076, 1.000000000000000000, 0.8660254037844387076, 1.000000000000000000, 0.8660254037844387076, 1.000000000000000000, 0.8660254037844387076, 1.000000000000000000, 0.8660254037844387076, 1.000000000000000000, 0.8660254037844387076, 1.000000000000000000, 0.8660254037844387076, 1.000000000000000000, 0.8660254037844387076, 1.000000000000000000, 0.8660254037844387076, 1.000000000000000000, 0.8660254037844387076, 1.000000000000000000, 0.8660254037844387076, 1.000000000000000000, 0.8660254037844387076, 1.000000000000000000, 0.8660254037844387076, 1.000000000000000000, 0.8660254037844387076, 1.000000000000000000, 0.8660254037844387076, 1.000000000000000000, 0.8660254037844387076, 1.000000000000000000, 0.8660254037844387076, 1.000000000000000000, 0.8660254037844387076, 1.000000000000000000, 0.8660254037844387076, 1.000000000000000000, 0.8660254037844387076, 1.000000000000000000, 0.8660254037844387076, 1.000000000000000000, 0.8660254037844387076, 1.000000000000000000, 0.8660254037844387076, 1.000000000000000000, 0.8660254037844387076, 1.000000000000000000, 0.8660254037844387076, 1.000000000000000000, 0.8660254037844387076, 1.000000000000000000, 0.8660254037844387076, 1.000000000000000000, 0.8660254037844387076, 1.000000000000000000, 0.8660254037844387076, 1.000000000000000000, 0.8660254037844387076, 1.000000000000000000, 0.8660254037844387076, 1.000000000000000000, 0.8660254037844387076, 1.000000000000000000, 0.8660254037844387076, 1.000000000000000000, 0.8660254037844387076, 1.000000000000000000, 0.8660254037844387076, 1.000000000000000000, 0.8660254037844387076, 1.000000000000000000, 0.8660254037844387076, 1.000000000000000000, 0.8660254037844387076, 1.000000000000000000, 0.8660254037844387076, 1.000000000000000000, 0.8660254037844387076, 1.000000000000000000, 0.8660254037844387076, 1.000000000000000000, 0.8660254037844387076, 1.000000000000000000, 0.8660254037844387076, 1.000000000000000000, 0.8660254037844387076, 1.000000000000000000, 0.8660254037844387076, 1.000000000000000000, 0.8660254037844387076, 1.000000000000000000, 0.8660254037844387076, 1.000000000000000000, 0.8660254037844387076, 1.000000000000000000, 0.8660254037844387076, 1.000000000000000000, 0.8660254037844387076, 1.000000000000000000, 0.8660254037844387076, 1.000000000000000000, 0.8660254037844387076, 1.000000000000000000, 0.8660254037844387076, 1.000000000000000000, 0.8660254037844387076, 1.000000000000000000, 0.8660254037844387076, 1.000000000000000000, 0.8660254037844387076, 1.000000000000000000, 0.8660254037844387076, 1.000000000000000000, 0.8660254037844387076, 1.000000000000000000, 0.8660254037844387076, 1.000000000000000000, 0.8660254037844387076, 1.000000000000000000, 0.8660254037844387076, 1.000000000000000000, 0.8660254037844387076, 1.000000000000000000, 0.8660254037844387076, 1.000000000000000000, 0.8660254037844387076, 1.000000000000000000, 0.8660254037844387076, 1.000000000000000000, 0.8660254037844387076, 1.000000000000000000, 0.8660254037844387076, 1.000000000000000000, 0.8660254037844387076, 1.000000000000000000, 0.8660254037844387076, 1.000000000000000000, 0.8660254037844387076, 1.000000000000000000, 0.8660254037844387076, 1.000000000000000000, 0.8660254037844387076, 1.000000000000000000, 0.8660254037844387076, 1.000000000000000000, 0.8660254037844387076, 1.000000000000000000, 0.8660254037844387076, 1.000000000000000000, 0.8660254037844387076, 1.000000000000000000, 0.8660254037844387076, 1.000000000000000000, 0.8660254037844387076, 1.000000000000000000, 0.8660254037844387076, 1.000000000000000000, 0.8660254037844387076, 1.000000000000000000, 0.8660254037844387076, 1.000000000000000000, 0.8660254037844387076, 1.000000000000000000, 0.8660254037844387076, 1.000000000000000000, 0.8660254037844387076, 1.000000000000000000, 0.8660254037844387076, 1.000000000000000000, 0.8660254037844387076, 1.000000000000000000, 0.8660254037844387076, 1.000000000000000000, 0.8660254037844387076, 1.000000000000000000, 0.8660254037844387076, 1.000000000000000000, 0.8660254037844387076, 1.000000000000000000, 0.8660254037844387076, 1.000000000000000000, 0.8660254037844387076, 1.000000000000000000, 0.8660254037844387076, 1.000000000000000000, 0.8660254037844387076, 1.000000000000000000, 0.8660254037844387076, 1.000000000000000000, 0.8660254037844387076, 1.000000000000000000, 0.8660254037844387076, 1.000000000000000000, 0.8660254037844387076, 1.000000000000000000, 0.8660254037844387076, 1.000000000000000000, 0.8660254037844387076, 1.000000000000000000, 0.8660254037844387076, 1.000000000000000000, 0.8660254037844387076, 1.000000000000000000, 0.8660254037844387076, 1.000000000000000000, 0.8660254037844387076, 1.000000000000000000),
 ( 1.000000000000000000, 0.8660254037844387076, 1.000000000000000000, 0.8660254037844387076, 1.000000000000000000, 0.8660254037844387076, 1.000000000000000000, 0.8660254037844387076, 1.000000000000000000, 0.8660254037844387076, 1.000000000000000000, 0.8660254037844387076, 1.000000000000000000, 0.8660254037844387076, 1.000000000000000000, 0.8660254037844387076, 1.000000000000000000, 0.8660254037844387076, 1.000000000000000000, 0.8660254037844387076, 1.000000000000000000, 0.8660254037844387076, 1.000000000000000000, 0.8660254037844387076, 1.000000000000000000, 0.8660254037844387076, 1.000000000000000000, 0.8660254037844387076, 1.000000000000000000, 0.8660254037844387076, 1.000000000000000000, 0.8660254037844387076, 1.000000000000000000, 0.8660254037844387076, 1.000000000000000000, 0.8660254037844387076, 1.000000000000000000, 0.8660254037844387076, 1.000000000000000000, 0.8660254037844387076, 1.000000000000000000, 0.8660254037844387076, 1.000000000000000000, 0.8660254037844387076, 1.000000000000000000, 0.8660254037844387076, 1.000000000000000000, 0.8660254037844387076, 1.000000000000000000, 0.8660254037844387076, 1.000000000000000000, 0.8660254037844387076, 1.000000000000000000, 0.8660254037844387076, 1.000000000000000000, 0.8660254037844387076, 1.000000000000000000, 0.8660254037844387076, 1.000000000000000000, 0.8660254037844387076, 1.000000000000000000, 0.8660254037844387076, 1.000000000000000000, 0.8660254037844387076, 1.000000000000000000, 0.8660254037844387076, 1.000000000000000000, 0.8660254037844387076, 1.000000000000000000, 0.8660254037844387076, 1.000000000000000000, 0.8660254037844387076, 1.000000000000000000, 0.8660254037844387076, 1.000000000000000000, 0.8660254037844387076, 1.000000000000000000, 0.8660254037844387076, 1.000000000000000000, 0.8660254037844387076, 1.000000000000000000, 0.8660254037844387076, 1.000000000000000000, 0.8660254037844387076, 1.000000000000000000, 0.8660254037844387076, 1.000000000000000000, 0.8660254037844387076, 1.000000000000000000, 0.8660254037844387076, 1.000000000000000000, 0.8660254037844387076, 1.000000000000000000, 0.8660254037844387076, 1.000000000000000000, 0.8660254037844387076, 1.000000000000000000, 0.8660254037844387076, 1.000000000000000000, 0.8660254037844387076, 1.000000000000000000, 0.8660254037844387076, 1.000000000000000000, 0.8660254037844387076, 1.000000000000000000, 0.8660254037844387076, 1.000000000000000000, 0.8660254037844387076, 1.000000000000000000, 0.8660254037844387076, 1.000000000000000000, 0.8660254037844387076, 1.000000000000000000, 0.8660254037844387076, 1.000000000000000000, 0.8660254037844387076, 1.000000000000000000, 0.8660254037844387076, 1.000000000000000000, 0.8660254037844387076, 1.000000000000000000, 0.8660254037844387076, 1.000000000000000000, 0.8660254037844387076, 1.000000000000000000, 0.8660254037844387076, 1.000000000000000000, 0.8660254037844387076, 1.000000000000000000, 0.8660254037844387076, 1.000000000000000000, 0.8660254037844387076, 1.000000000000000000, 0.8660254037844387076, 1.000000000000000000, 0.8660254037844387076, 1.000000000000000000, 0.8660254037844387076, 1.000000000000000000, 0.8660254037844387076, 1.000000000000000000, 0.8660254037844387076, 1.000000000000000000, 0.8660254037844387076, 1.000000000000000000, 0.8660254037844387076, 1.000000000000000000, 0.8660254037844387076, 1.000000000000000000, 0.8660254037844387076, 1.000000000000000000, 0.8660254037844387076, 1.000000000000000000, 0.8660254037844387076, 1.000000000000000000, 0.8660254037844387076, 1.000000000000000000, 0.8660254037844387076, 1.000000000000000000, 0.8660254037844387076, 1.000000000000000000, 0.8660254037844387076, 1.000000000000000000, 0.8660254037844387076, 1.000000000000000000, 0.8660254037844387076, 1.000000000000000000, 0.8660254037844387076, 1.000000000000000000, 0.8660254037844387076, 1.000000000000000000, 0.8660254037844387076, 1.000000000000000000, 0.8660254037844387076, 1.000000000000000000, 0.8660254037844387076, 1.000000000000000000, 0.8660254037844387076, 1.000000000000000000, 0.8660254037844387076, 1.000000000000000000, 0.8660254037844387076, 1.000000000000000000, 0.8660254037844387076, 1.000000000000000000, 0.8660254037844387076, 1.000000000000000000, 0.8660254037844387076, 1.000000000000000000, 0.8660254037844387076, 1.000000000000000000, 0.8660254037844387076, 1.000000000000000000, 0.8660254037844387076, 1.000000000000000000, 0.8660254037844387076, 1.000000000000000000, 0.8660254037844387076, 1.000000000000000000, 0.8660254037844387076, 1.000000000000000000, 0.8660254037844387076, 1.000000000000000000, 0.8660254037844387076, 1.000000000000000000, 0.8660254037844387076, 1.000000000000000000, 0.8660254037844387076, 1.000000000000000000, 0.8660254037844387076, 1.000000000000000000, 0.8660254037844387076, 1.000000000000000000, 0.8660254037844387076, 1.000000000000000000, 0.8660254037844387076, 1.000000000000000000, 0.8660254037844387076, 1.000000000000000000, 0.8660254037844387076, 1.000000000000000000, 0.8660254037844387076, 1.000000000000000000, 0.8660254037844387076, 1.000000000000000000, 0.8660254037844387076, 1.000000000000000000, 0.8660254037844387076, 1.000000000000000000, 0.8660254037844387076, 1.000000000000000000, 0.8660254037844387076, 1.000000000000000000, 0.8660254037844387076, 1.000000000000000000, 0.8660254037844387076, 1.000000000000000000, 0.8660254037844387076, 1.000000000000000000, 0.8660254037844387076, 1.000000000000000000) ) ) 
 REPRESENTATION_ITEM ( '' )  SURFACE ( )  );
#207992 = AXIS2_PLACEMENT_3D ( 'NONE', #178356, #47298, #143755 ) ;
#207993 = CARTESIAN_POINT ( 'NONE',  ( 1.023854850961497309, 1.058662087540670704, -1.418139054142423472 ) ) ;
#207994 = CARTESIAN_POINT ( 'NONE',  ( 5.549481842319204716, -1.818904971374595503, 0.8629315129762565872 ) ) ;
#207995 = CARTESIAN_POINT ( 'NONE',  ( 7.169564303528210836, 7.258913197071374945, -0.7998128361456281477 ) ) ;
#207996 = CARTESIAN_POINT ( 'NONE',  ( 4.120224405726905736, -1.080582774747363306, -1.807441255628852828 ) ) ;
#207997 = CARTESIAN_POINT ( 'NONE',  ( 3.022943291168778579, -1.688106736905025995, 0.9054777632113325536 ) ) ;
#207998 = AXIS2_PLACEMENT_3D ( 'NONE', #208309, #126094, #187796 ) ;
#207999 = CARTESIAN_POINT ( 'NONE',  ( 4.650814871655007288, -0.4294639348428323511, -1.921992245654633447 ) ) ;
#208000 = CARTESIAN_POINT ( 'NONE',  ( 5.484630696634174463, -1.278254659592213516, 1.563874148425943078 ) ) ;
#208001 = CARTESIAN_POINT ( 'NONE',  ( 2.166681600665042229, -1.709288833360942617, -0.7604731621856930524 ) ) ;
#208004 = ORIENTED_EDGE ( 'NONE', *, *, #119318, .T. ) ;
#208003 = CARTESIAN_POINT ( 'NONE',  ( 1.441514601552947417, -1.799640695080907182, 0.6472408003148700795 ) ) ;
#208002 = CARTESIAN_POINT ( 'NONE',  ( 4.986778444009251743, -0.2158907008250054438, -1.711239743519934242 ) ) ;
#208006 = CARTESIAN_POINT ( 'NONE',  ( 4.365362273920250225, 5.155639410070820716, 1.082531754730560403 ) ) ;
#208005 = CARTESIAN_POINT ( 'NONE',  ( 2.526237079854487089, -1.271617311931704686, -1.803507373242494438 ) ) ;
#208007 = EDGE_CURVE ( 'NONE', #180121, #143111, #94636, .T. ) ;
#208008 = CARTESIAN_POINT ( 'NONE',  ( -0.6823417656250003738, 2.280208333674753174, -1.181850606188749264 ) ) ;
#208009 = CARTESIAN_POINT ( 'NONE',  ( 6.760214184729610665, -1.961454122871961747, 0.04698431645466792650 ) ) ;
#208010 = CARTESIAN_POINT ( 'NONE',  ( 8.450809820019639318, 8.753699632978056755, -0.7998128361456291469 ) ) ;
#208011 = CARTESIAN_POINT ( 'NONE',  ( -8.319899820280397762, 12.85830022363583147, -0.7998128361456281477 ) ) ;
#208012 = DIRECTION ( 'NONE',  ( 0.000000000000000000, 0.000000000000000000, 1.000000000000000000 ) ) ;
#208013 = DIRECTION ( 'NONE',  ( 0.000000000000000000, 0.000000000000000000, -1.000000000000000000 ) ) ;
#208014 = DIRECTION ( 'NONE',  ( 0.000000000000000000, 0.000000000000000000, 1.000000000000000000 ) ) ;
#208015 = CARTESIAN_POINT ( 'NONE',  ( 1.820844063133007396, -1.465591517063179028, 1.462601037713284535 ) ) ;
#208016 = CARTESIAN_POINT ( 'NONE',  ( -0.7499999999999972244, 3.608333333333359150, -1.299038105676652011 ) ) ;
#208017 = CARTESIAN_POINT ( 'NONE',  ( 6.311484202361478779, 7.322151976631905868, -1.199719254218446718 ) ) ;
#208018 = CARTESIAN_POINT ( 'NONE',  ( -7.039708073993679704, 9.236078724457858158, 1.599625672291283607 ) ) ;
#208019 = CARTESIAN_POINT ( 'NONE',  ( 3.528865121306874464, 7.339036084825155015, -0.7998128361456362523 ) ) ;
#208020 = CARTESIAN_POINT ( 'NONE',  ( 0.2936253167127310659, 1.883648094304795961, -0.7291253699766816476 ) ) ;
#208021 = CARTESIAN_POINT ( 'NONE',  ( 1.500000000000001332, 10.40625000068279249, 0.000000000000000000 ) ) ;
#208022 = CARTESIAN_POINT ( 'NONE',  ( -1.364683531250000748, 2.009375000341421913, 1.214306433183764966E-14 ) ) ;
#208024 = CARTESIAN_POINT ( 'NONE',  ( 2.900554798319789906, 5.471398800426671372, 1.199719254218452047 ) ) ;
#208023 = DIRECTION ( 'NONE',  ( 0.000000000000000000, 1.000000000000000000, 0.000000000000000000 ) ) ;
#208025 = CARTESIAN_POINT ( 'NONE',  ( 5.009138659175729202, 2.010518709310470609, 0.1511151588593287465 ) ) ;
#208026 = CARTESIAN_POINT ( 'NONE',  ( 4.575340585108073732, 1.423666108326137048, 1.282088096497513652 ) ) ;
#208027 = CARTESIAN_POINT ( 'NONE',  ( 2.876726420669137863, -0.1638259704515396820, -2.185508879517850112 ) ) ;
#208028 = CARTESIAN_POINT ( 'NONE',  ( -1.734723475976807094E-15, 4.446955548196619645, -11.95586206894145676 ) ) ;
#208029 = CARTESIAN_POINT ( 'NONE',  ( 1.499999999999987121, 0.07708333401615156955, -0.8660254037844323793 ) ) ;
#208030 = CARTESIAN_POINT ( 'NONE',  ( 5.642843092333371224, 1.941422931094261450, 0.5326616679640855390 ) ) ;
#208031 = CARTESIAN_POINT ( 'NONE',  ( 1.423922367354793606, -1.897583212610975734, 0.2371896777705190806 ) ) ;
#208032 = CARTESIAN_POINT ( 'NONE',  ( -6.175902666224832416, 7.163973517805802160, -1.199719254218446718 ) ) ;
#208034 = CARTESIAN_POINT ( 'NONE',  ( 6.609000000000050612, -6.653734691735092887E-05, 2.100160721423645960 ) ) ;
#208033 = CARTESIAN_POINT ( 'NONE',  ( -2.819732761962335577, 5.273143408055916304, -1.082531754730543971 ) ) ;
#208035 = CARTESIAN_POINT ( 'NONE',  ( -0.6823417656250039265, 9.880208333674728394, -1.181850606188755259 ) ) ;
#208037 = CARTESIAN_POINT ( 'NONE',  ( -6.981522756394290319, 7.109807735406931783, 0.7998128361456341429 ) ) ;
#208036 = CARTESIAN_POINT ( 'NONE',  ( 3.737900851971903915, 2.080878125540788215, 0.2026709130291924343 ) ) ;
#208039 = ORIENTED_EDGE ( 'NONE', *, *, #48666, .T. ) ;
#208038 = CARTESIAN_POINT ( 'NONE',  ( 1.781837903662389477, -0.9264376740152606704, 1.454631767934653208 ) ) ;
#208040 = CARTESIAN_POINT ( 'NONE',  ( 5.503720292143644777, 8.508425209887878538, 1.199719254218462483 ) ) ;
#208041 = CARTESIAN_POINT ( 'NONE',  ( -0.4486483537597074078, 13.27801534917682780, 1.409698628028286382 ) ) ;
#208042 = CARTESIAN_POINT ( 'NONE',  ( 0.3792546940144908563, -0.1001052471676349837, 1.959448305358338693 ) ) ;
#208043 = FACE_OUTER_BOUND ( 'NONE', #200466, .T. ) ;
#208044 = CARTESIAN_POINT ( 'NONE',  ( 4.710568305744190276, 7.583081225755162968, 1.199719254218462483 ) ) ;
#208045 = ORIENTED_EDGE ( 'NONE', *, *, #34501, .T. ) ;
#208046 = CARTESIAN_POINT ( 'NONE',  ( 1.264911064067342217, 3.850000000000006306, -0.4999999999999987232 ) ) ;
#208047 = B_SPLINE_CURVE_WITH_KNOTS ( 'NONE', 3,
 ( #159356, #8835, #155100, #75976 ),
 .UNSPECIFIED., .F., .F.,
 ( 4, 4 ),
 ( 0.001673025196799804177, 0.002270020235895683393 ),
 .UNSPECIFIED. ) ;
#208048 = CARTESIAN_POINT ( 'NONE',  ( 3.000440247697288676, -1.785030861869114638, -0.3072999389705335926 ) ) ;
#208049 = ORIENTED_EDGE ( 'NONE', *, *, #102848, .F. ) ;
#208050 = CARTESIAN_POINT ( 'NONE',  ( 3.297657676621871925, 4.870353260857385180, 1.599625672291267398 ) ) ;
#208051 = CARTESIAN_POINT ( 'NONE',  ( 5.585032934186686226, 5.480569609498057382, 0.000000000000000000 ) ) ;
#208052 = CARTESIAN_POINT ( 'NONE',  ( 3.369578772036628145, 0.4373610723380080834, -1.757749666579068171 ) ) ;
#208053 = CARTESIAN_POINT ( 'NONE',  ( 0.5997958527293488773, 3.416913062369157483, -0.2585301179639583613 ) ) ;
#208054 = CARTESIAN_POINT ( 'NONE',  ( -10.98194350564911481, -7.666862915010147717, 0.6300133639306313427 ) ) ;
#208055 = CARTESIAN_POINT ( 'NONE',  ( 5.891837173953166307, 5.977390820968681240, -0.04595957878574669087 ) ) ;
#208056 = CARTESIAN_POINT ( 'NONE',  ( 4.387043322907993925, 0.09000376980121749249, 1.858987348747977331 ) ) ;
#208057 = CARTESIAN_POINT ( 'NONE',  ( 1.739701290322914540, 1.910364143156467298, -0.1427236045144583687 ) ) ;
#208058 = CARTESIAN_POINT ( 'NONE',  ( 0.4986989427119004059, 1.520756344202650601, -1.009667857431728599 ) ) ;
#208059 = CARTESIAN_POINT ( 'NONE',  ( 6.471393748265519719, 5.229711127717882491, -2.419999999999995932 ) ) ;
#208060 = CARTESIAN_POINT ( 'NONE',  ( -4.136646265500965924, 7.840188053144151681, -0.7216878364870512597 ) ) ;
#208061 = VECTOR ( 'NONE', #65679, 1000.000000000000000 ) ;
#208062 = CARTESIAN_POINT ( 'NONE',  ( 4.798147134389644464, 8.131168186839138556, 0.8272934513729796047 ) ) ;
#208063 = CARTESIAN_POINT ( 'NONE',  ( 9.633311866038676285, 13.62946609490282235, 8.224406077922058245 ) ) ;
#208064 = CARTESIAN_POINT ( 'NONE',  ( -1.499999999999997780, 5.181250000682820378, 1.214306433183764966E-14 ) ) ;
#208065 = CARTESIAN_POINT ( 'NONE',  ( 1.464175926609780964E-14, -2.493749999044085452, -3.475000000000000533 ) ) ;
#208066 = CARTESIAN_POINT ( 'NONE',  ( 8.324343129110697959, 9.774450407793066731, -1.082531754730543083 ) ) ;
#208067 = CARTESIAN_POINT ( 'NONE',  ( 6.016450702237627901, 0.7947307017554460229, 1.802146183335861629 ) ) ;
#208068 = CARTESIAN_POINT ( 'NONE',  ( -4.446184310277715213, 7.274633231044262516, -1.199719254218452047 ) ) ;
#208069 = DIRECTION ( 'NONE',  ( -7.387867266669436732E-31, -1.000000000000000000, 8.546850786086437571E-32 ) ) ;
#208070 = CARTESIAN_POINT ( 'NONE',  ( 0.4981332788140432899, -0.7063641614380437028, -1.967824727186429978 ) ) ;
#208071 = CARTESIAN_POINT ( 'NONE',  ( 7.771848369131631351, 10.09024240211882351, -1.599625672291262513 ) ) ;
#208072 = CARTESIAN_POINT ( 'NONE',  ( 4.981433139801599630, 1.797578344525651906, -0.6930591852608753989 ) ) ;
#208073 = CARTESIAN_POINT ( 'NONE',  ( -6.905180308061733996, 6.950465202360470052, 0.7998128361456341429 ) ) ;
#208074 = CARTESIAN_POINT ( 'NONE',  ( 1.465546361252961782, 1.799214786004127209, -0.3081908958329632742 ) ) ;
#208075 = CARTESIAN_POINT ( 'NONE',  ( 2.561379550486083012, -1.920685204893451292, -1.086737900330703166 ) ) ;
#208076 = CARTESIAN_POINT ( 'NONE',  ( 0.7500000000000006661, 9.864583334016129967, 1.299038105676657340 ) ) ;
#208077 = CARTESIAN_POINT ( 'NONE',  ( 0.7735182334044669039, 0.3705173918269571431, -1.875978362188877036 ) ) ;
#208078 = ORIENTED_EDGE ( 'NONE', *, *, #150919, .T. ) ;
#208079 = CARTESIAN_POINT ( 'NONE',  ( 0.5023235590321275534, 1.964037083787707028, 0.1483792944171925254 ) ) ;
#208080 = CARTESIAN_POINT ( 'NONE',  ( 2.419391519165543070, -1.120004824200554916, -1.586377984052749879 ) ) ;
#208081 = ORIENTED_EDGE ( 'NONE', *, *, #180932, .T. ) ;
#208082 = CARTESIAN_POINT ( 'NONE',  ( 1.300157425512000087, -1.823841169980220167, 0.8594962466553013325 ) ) ;
#208084 = CARTESIAN_POINT ( 'NONE',  ( 6.121894333209238148, 1.833584433263518942, -0.3168336897404684382 ) ) ;
#208083 = CARTESIAN_POINT ( 'NONE',  ( -4.847922445338252118, 7.813604065273374921, -1.199719254218453823 ) ) ;
#208085 = CARTESIAN_POINT ( 'NONE',  ( 4.923546060418115822, 5.773167154356443120, -1.199719254218452047 ) ) ;
#208086 = CARTESIAN_POINT ( 'NONE',  ( -11.55950211276791428, 13.80000000000000071, -3.221476510067116550 ) ) ;
#208087 = CARTESIAN_POINT ( 'NONE',  ( 8.778014389843965759, 12.32843499053828928, 1.199719254218450271 ) ) ;
#208088 = CARTESIAN_POINT ( 'NONE',  ( -5.752737250900127997, 5.605948302338584099, 0.000000000000000000 ) ) ;
#208089 = CARTESIAN_POINT ( 'NONE',  ( -6.608673532018475960, 6.674816973635147477, -0.7998128361456362523 ) ) ;
#208090 = CARTESIAN_POINT ( 'NONE',  ( 2.208753784402537335, 1.959192758111829136, 0.9821998110004714899 ) ) ;
#208091 = CARTESIAN_POINT ( 'NONE',  ( 3.172244755917638770, 5.684407401003788607, -1.082531754730543083 ) ) ;
#208092 = AXIS2_PLACEMENT_3D ( 'NONE', #19956, #52475, #87105 ) ;
#208093 = CARTESIAN_POINT ( 'NONE',  ( 5.688757509019037428, 5.629766575900002401, 2.500000000000000000 ) ) ;
#208094 = CARTESIAN_POINT ( 'NONE',  ( 0.4999999999999900080, 3.950000000000009059, -0.5000000000000160982 ) ) ;
#208095 = CARTESIAN_POINT ( 'NONE',  ( 2.473051018021198200, 0.08991741065280876855, -1.823594477012622228 ) ) ;
#208096 = DIRECTION ( 'NONE',  ( 0.000000000000000000, 0.000000000000000000, -1.000000000000000000 ) ) ;
#208097 = CARTESIAN_POINT ( 'NONE',  ( -3.079673448598517549, 6.744702790006905424, 1.040834085586084257E-14 ) ) ;
#208098 = CARTESIAN_POINT ( 'NONE',  ( -4.953783236630994402, 8.080086878320878796, -1.094444140625696837 ) ) ;
#208099 = DIRECTION ( 'NONE',  ( 0.000000000000000000, 1.000000000000000000, 0.000000000000000000 ) ) ;
#208100 = CARTESIAN_POINT ( 'NONE',  ( 8.565000355531088516, 11.01558638625153286, -1.599625672291257406 ) ) ;
#208101 = CARTESIAN_POINT ( 'NONE',  ( 0.5219392174641559468, -1.029590632097213687, -1.628125521969860712 ) ) ;
#208102 = CARTESIAN_POINT ( 'NONE',  ( 6.086763564210844635, 1.889667650816441391, 0.5265613530214610094 ) ) ;
#208103 = AXIS2_PLACEMENT_3D ( 'NONE', #162605, #81342, #29404 ) ;
#208104 = CARTESIAN_POINT ( 'NONE',  ( -1.402160292154681736E-14, 15.06250000000000000, 1.732050807568881190 ) ) ;
#208105 = CARTESIAN_POINT ( 'NONE',  ( -7.335124800193271177, 8.516399340768996851, -1.199719254218452935 ) ) ;
#208106 = CARTESIAN_POINT ( 'NONE',  ( 5.834086172582112262, 5.700855377634248100, 1.040834085586084257E-14 ) ) ;
#208107 = CARTESIAN_POINT ( 'NONE',  ( 5.513277522340928272, -2.138352208816508782, 0.4792397250529822905 ) ) ;
#208109 = ADVANCED_FACE ( 'NONE', ( #206209 ), #160680, .F. ) ;
#208108 = CARTESIAN_POINT ( 'NONE',  ( 3.625891163443736520, 2.020865133175090644, -0.4488579359705275329 ) ) ;
#208111 = CARTESIAN_POINT ( 'NONE',  ( -1.201851678989727383E-14, 2.759375000341417916, -1.575800808251660134 ) ) ;
#208110 = CARTESIAN_POINT ( 'NONE',  ( 8.371655185961106582, 14.07500887114600197, 8.535501002982430307 ) ) ;
#208112 = ORIENTED_EDGE ( 'NONE', *, *, #122569, .F. ) ;
#208113 = CARTESIAN_POINT ( 'NONE',  ( 4.606216143772843274, -0.1140155944862955434, 2.295953707746749117 ) ) ;
#208114 = CARTESIAN_POINT ( 'NONE',  ( 7.293923454472087897, 8.572294120714675003, 1.082531754730558626 ) ) ;
#208116 = CARTESIAN_POINT ( 'NONE',  ( 5.398914348987510436, 6.259949555863199677, -2.420000000000000373 ) ) ;
#208115 = CARTESIAN_POINT ( 'NONE',  ( 3.757017964762656703, 7.397288368949487491, -1.734723475976807094E-15 ) ) ;
#208117 = CARTESIAN_POINT ( 'NONE',  ( 0.2876181914312899157, 1.702867465475272901, 1.534690983289775712 ) ) ;
#208118 = CARTESIAN_POINT ( 'NONE',  ( 6.620655732516611103, 3.701195159515461075, 2.440764268381501179 ) ) ;
#208119 = CARTESIAN_POINT ( 'NONE',  ( -7.937372586157736443, 8.224965870130965584, 0.7998128361456341429 ) ) ;
#208120 = CARTESIAN_POINT ( 'NONE',  ( 5.173749199105643903, -1.077276334994947460, 1.615559063095718839 ) ) ;
#208121 = CARTESIAN_POINT ( 'NONE',  ( 9.124274191872634887, 11.66807252865000244, -1.443375672974058777 ) ) ;
#208122 = ORIENTED_EDGE ( 'NONE', *, *, #207059, .F. ) ;
#208123 = CARTESIAN_POINT ( 'NONE',  ( 5.519756697582541172, -0.4584384640409416289, 1.856529252577573619 ) ) ;
#208124 = CARTESIAN_POINT ( 'NONE',  ( 6.053657651994457822, 0.4959367165196375549, -1.651908409946404976 ) ) ;
#208125 = CARTESIAN_POINT ( 'NONE',  ( 5.225796113160614986, 0.8128206588041907432, -1.845625551132886288 ) ) ;
#208127 = CARTESIAN_POINT ( 'NONE',  ( -2.875737979874388284, 6.369128386579808954, -0.7216878364870458196 ) ) ;
#208126 = CARTESIAN_POINT ( 'NONE',  ( -8.533967624797991647, 12.04371376465130439, -1.199719254218446718 ) ) ;
#208128 = CARTESIAN_POINT ( 'NONE',  ( -1.642778471874998480, -1.188541666188709600, 2.845375778867863303 ) ) ;
#208130 = CARTESIAN_POINT ( 'NONE',  ( 6.714108650864204719, -0.8368934294483711955, -1.559304158387794015 ) ) ;
#208129 = CARTESIAN_POINT ( 'NONE',  ( 1.957086829145736173, 0.3561595965777020756, -2.059905414565963433 ) ) ;
#208131 = CARTESIAN_POINT ( 'NONE',  ( 5.625625018759272677, 0.3960990390993284205, 1.976956468877195894 ) ) ;
#208132 = EDGE_CURVE ( 'NONE', #175615, #93441, #27280, .T. ) ;
#208134 = CARTESIAN_POINT ( 'NONE',  ( 2.713130565535960770, -0.2235823006870632790, 2.281328536464954038 ) ) ;
#208133 = CARTESIAN_POINT ( 'NONE',  ( 4.899292406491845497, 6.809203455697518947, -1.599625672291273171 ) ) ;
#208135 = CARTESIAN_POINT ( 'NONE',  ( 1.745671189342316687, 0.5440799701325367277, 1.653152385070497887 ) ) ;
#208136 = CARTESIAN_POINT ( 'NONE',  ( 11.91826848330681976, 11.00729645956991654, -1.400000080589506979 ) ) ;
#208137 = CARTESIAN_POINT ( 'NONE',  ( 1.932526292592825046, 0.8863411937694037901, 1.489983018702551787 ) ) ;
#208138 = CARTESIAN_POINT ( 'NONE',  ( -1.752700365193352367E-14, 1.609375000341425777, -1.570758158831794260 ) ) ;
#208139 = CARTESIAN_POINT ( 'NONE',  ( 1.556854020514925496, 1.524047875013130104, -1.067797667942985917 ) ) ;
#208140 = CARTESIAN_POINT ( 'NONE',  ( 2.963510081828163223, 1.832883945819727689, 1.163594247970006990 ) ) ;
#208141 = CARTESIAN_POINT ( 'NONE',  ( 3.081267818761534549, 1.592661989535900657, 1.236799713577160231 ) ) ;
#208142 = CARTESIAN_POINT ( 'NONE',  ( 4.906250000000003553, 1.895863743163974213, -0.7852924748302423374 ) ) ;
#208143 = PRESENTATION_LAYER_ASSIGNMENT (  '', '', ( #121815 ) ) ;
#208144 = CARTESIAN_POINT ( 'NONE',  ( 0.7499999999999885647, 0.8479166673494853423, -1.299038105676652899 ) ) ;
#208145 = CARTESIAN_POINT ( 'NONE',  ( 6.568979851886898480, -1.762530817088540758, -0.7781539781668064260 ) ) ;
#208146 = CARTESIAN_POINT ( 'NONE',  ( -1.364683531250000748, 14.85937500034140157, 0.000000000000000000 ) ) ;
#208147 = CARTESIAN_POINT ( 'NONE',  ( 2.988771237642441569, -1.320003323290209751, 1.786578734224959497 ) ) ;
#208148 = ORIENTED_EDGE ( 'NONE', *, *, #19773, .F. ) ;
#208150 = CIRCLE ( 'NONE', #114834, 0.07999999999999933553 ) ;
#208149 = CARTESIAN_POINT ( 'NONE',  ( -0.2110808730067144090, 0.7535804146166940054, -1.881771259391984197 ) ) ;
#208151 = CARTESIAN_POINT ( 'NONE',  ( -1.500000000000015099, 0.3791666666666850261, -0.8660254037844383745 ) ) ;
#208152 = CARTESIAN_POINT ( 'NONE',  ( 7.391166297744269365, 11.77477778067701664, 1.040834085586084257E-14 ) ) ;
#208153 = CARTESIAN_POINT ( 'NONE',  ( -1.364683531250000748, 0.009375000341420303140, 0.000000000000000000 ) ) ;
#208154 = CARTESIAN_POINT ( 'NONE',  ( 6.240512348869785342, 1.279970183950808860, -1.815422973897186543 ) ) ;
#208155 = CARTESIAN_POINT ( 'NONE',  ( 4.299235682465595509, -1.708000122724560477, 0.9650500775852040025 ) ) ;
#208157 = CARTESIAN_POINT ( 'NONE',  ( -4.772106882330223954, 8.511282429453158827, -0.7216878364870267237 ) ) ;
#208156 = CARTESIAN_POINT ( 'NONE',  ( 3.521367211247359741, 5.131347717920458962, -1.599625672291262513 ) ) ;
#208158 = LINE ( 'NONE', #90179, #118339 ) ;
#208159 = CARTESIAN_POINT ( 'NONE',  ( 5.571622904855764169, 2.182566619097675797, -0.5956038432519733528 ) ) ;
#208160 = CARTESIAN_POINT ( 'NONE',  ( 2.664570663672768180, -0.7871131050594852852, -1.906781320289064885 ) ) ;
#208161 = CARTESIAN_POINT ( 'NONE',  ( -5.181187258716735577, 9.196468901811520880, 0.7998128361456481317 ) ) ;
#208162 = EDGE_CURVE ( 'NONE', #105939, #35911, #51574, .T. ) ;
#208163 = EDGE_LOOP ( 'NONE', ( #182821, #88041 ) ) ;
#208164 = CARTESIAN_POINT ( 'NONE',  ( -0.7500000000000215383, 2.722916667349486897, 1.299038105676671107 ) ) ;
#208165 = CARTESIAN_POINT ( 'NONE',  ( 3.936663633328242096, 0.2718032920513112627, 1.850550731861917653 ) ) ;
#208166 = CARTESIAN_POINT ( 'NONE',  ( 2.302961303058923992, 1.131868135402936737, -1.313931383173136513 ) ) ;
#208167 = CARTESIAN_POINT ( 'NONE',  ( 5.935146830689759234, -1.586316731616247200, -1.512381816529739353 ) ) ;
#208168 = CARTESIAN_POINT ( 'NONE',  ( 1.167327668269029228, -1.995579438226593894, -0.9423882379527288577 ) ) ;
#208169 = CARTESIAN_POINT ( 'NONE',  ( 5.226486033959851341, 0.1448775283907685063, 1.936603901228886926 ) ) ;
#208170 = DIRECTION ( 'NONE',  ( 0.6507913734559651608, -0.7592566023652994600, 0.000000000000000000 ) ) ;
#208171 = CARTESIAN_POINT ( 'NONE',  ( 0.000000000000000000, 0.000000000000000000, -1.999999999999999556 ) ) ;
#208172 = CARTESIAN_POINT ( 'NONE',  ( 1.002577532868035526, -1.966644254196001196, 0.4445047019146358691 ) ) ;
#208173 = CARTESIAN_POINT ( 'NONE',  ( -0.2104748580754166598, -0.006608320950483163522, -2.103482951484026753 ) ) ;
#208174 = CARTESIAN_POINT ( 'NONE',  ( -1.138412281109779656E-15, -8.526088927970992160, 10.80093815994596262 ) ) ;
#208175 = CARTESIAN_POINT ( 'NONE',  ( 6.416638760586134360, -1.319225726833603840, -1.525046029381103452 ) ) ;
#208176 = CARTESIAN_POINT ( 'NONE',  ( -9.854078719034067291, 10.39084668182823634, 0.7998128361456462443 ) ) ;
#208177 =( BOUNDED_CURVE ( )  B_SPLINE_CURVE ( 2, ( #74607, #125570, #61544, #140711, #173192, #60474, #43195, #109308, #123454, #108240, #127711, #175318, #90875, #110371, #189416, #206726, #11718, #26904, #76722, #24773, #93009, #193671, #10646, #142838, #41060, #208844, #58354, #77793, #190468, #94077, #174264, #45314, #160116, #143913, #214144, #149193, #128764, #179572, #83112, #65770, #768, #129832, #148142, #12773, #31191, #98316, #47452, #210973, #113567, #66834, #97264, #30115, #49554, #34367, #79917, #165438, #48510, #15965, #178505, #213104, #147082, #163319, #14900, #194738, #164381, #162255, #17035, #13841, #82049, #96205, #132977, #181674, #131918, #197928, #198979, #46375, #80994, #50624, #115680, #116750, #64736, #33301, #63678, #182749, #180622, #112494, #195815, #130879, #161187, #196873, #99386, #146027, #78847, #144967, #114630, #62601, #212036, #32245, #87407, #150277, #54901, #55970, #100441, #68985, #137236, #204313, #118893, #135103, #200060, #188087, #122123, #1847, #166512, #52759, #138298, #3980, #67906, #51712, #101510, #18104, #153471, #201117, #121054, #154540, #103661, #22369, #184878, #19180, #84190, #71120, #20244, #169710, #36503, #117831, #85255, #102582, #2912, #134052, #167581, #168642, #183822, #21300, #35434 ),
 .UNSPECIFIED., .F., .T. ) 
 B_SPLINE_CURVE_WITH_KNOTS ( ( 3, 2, 2, 2, 2, 2, 2, 2, 2, 2, 2, 2, 2, 2, 2, 2, 2, 2, 2, 2, 2, 2, 2, 2, 2, 2, 2, 2, 2, 2, 2, 2, 2, 2, 2, 2, 2, 2, 2, 2, 2, 2, 2, 2, 2, 2, 2, 2, 2, 2, 2, 2, 2, 2, 2, 2, 2, 2, 2, 2, 2, 2, 2, 2, 2, 2, 2, 2, 2, 2, 2, 3 ),
 ( 0.000000000000000000, 0.01041666666666666609, 0.02083333333333333218, 0.03125000000000000000, 0.04166666666666666435, 0.05208333333333333565, 0.06250000000000000000, 0.07291666666666667129, 0.08333333333333332871, 0.09375000000000000000, 0.1041666666666666713, 0.1145833333333333287, 0.1250000000000000000, 0.1354166666666666574, 0.1458333333333333426, 0.1562500000000000000, 0.1666666666666666574, 0.1770833333333333426, 0.1875000000000000000, 0.1979166666666666574, 0.2083333333333333426, 0.2187500000000000000, 0.2291666666666666574, 0.2395833333333333426, 0.2500000000000000000, 0.2604166666666666852, 0.2708333333333333148, 0.2812500000000000000, 0.2916666666666666852, 0.3020833333333333148, 0.3125000000000000000, 0.3229166666666666852, 0.3333333333333333148, 0.3437500000000000000, 0.3541666666666666852, 0.3645833333333333148, 0.3750000000000000000, 0.3854166666666666852, 0.3958333333333333148, 0.4062500000000000000, 0.4166666666666666852, 0.4270833333333333148, 0.4375000000000000000, 0.4479166666666666852, 0.4583333333333333148, 0.4687500000000000000, 0.4791666666666666852, 0.4895833333333333148, 0.5000000000000000000, 0.5104166666666666297, 0.5208333333333333703, 0.5312500000000000000, 0.5416666666666666297, 0.5520833333333333703, 0.5625000000000000000, 0.5729166666666666297, 0.5833333333333333703, 0.5937500000000000000, 0.6041666666666666297, 0.6145833333333333703, 0.6250000000000000000, 0.6354166666666666297, 0.6458333333333333703, 0.6562500000000000000, 0.6666666666666666297, 0.6770833333333333703, 0.6875000000000000000, 0.6979166666666666297, 0.7083333333333333703, 0.7187500000000000000, 0.7291666666666666297, 0.7305924012910729459 ),
 .UNSPECIFIED. ) 
 CURVE ( )  GEOMETRIC_REPRESENTATION_ITEM ( )  RATIONAL_B_SPLINE_CURVE ( ( 1.000000000000000000, 0.8660254037844387076, 1.000000000000000000, 0.8660254037844387076, 1.000000000000000000, 0.8660254037844387076, 1.000000000000000000, 0.8660254037844387076, 1.000000000000000000, 0.8660254037844387076, 1.000000000000000000, 0.8660254037844387076, 1.000000000000000000, 0.8660254037844387076, 1.000000000000000000, 0.8660254037844387076, 1.000000000000000000, 0.8660254037844387076, 1.000000000000000000, 0.8660254037844387076, 1.000000000000000000, 0.8660254037844387076, 1.000000000000000000, 0.8660254037844387076, 1.000000000000000000, 0.8660254037844387076, 1.000000000000000000, 0.8660254037844387076, 1.000000000000000000, 0.8660254037844387076, 1.000000000000000000, 0.8660254037844387076, 1.000000000000000000, 0.8660254037844387076, 1.000000000000000000, 0.8660254037844387076, 1.000000000000000000, 0.8660254037844387076, 1.000000000000000000, 0.8660254037844387076, 1.000000000000000000, 0.8660254037844387076, 1.000000000000000000, 0.8660254037844387076, 1.000000000000000000, 0.8660254037844387076, 1.000000000000000000, 0.8660254037844387076, 1.000000000000000000, 0.8660254037844387076, 1.000000000000000000, 0.8660254037844387076, 1.000000000000000000, 0.8660254037844387076, 1.000000000000000000, 0.8660254037844387076, 1.000000000000000000, 0.8660254037844387076, 1.000000000000000000, 0.8660254037844387076, 1.000000000000000000, 0.8660254037844387076, 1.000000000000000000, 0.8660254037844387076, 1.000000000000000000, 0.8660254037844387076, 1.000000000000000000, 0.8660254037844387076, 1.000000000000000000, 0.8660254037844387076, 1.000000000000000000, 0.8660254037844387076, 1.000000000000000000, 0.8660254037844387076, 1.000000000000000000, 0.8660254037844387076, 1.000000000000000000, 0.8660254037844387076, 1.000000000000000000, 0.8660254037844387076, 1.000000000000000000, 0.8660254037844387076, 1.000000000000000000, 0.8660254037844387076, 1.000000000000000000, 0.8660254037844387076, 1.000000000000000000, 0.8660254037844387076, 1.000000000000000000, 0.8660254037844387076, 1.000000000000000000, 0.8660254037844387076, 1.000000000000000000, 0.8660254037844387076, 1.000000000000000000, 0.8660254037844387076, 1.000000000000000000, 0.8660254037844387076, 1.000000000000000000, 0.8660254037844387076, 1.000000000000000000, 0.8660254037844387076, 1.000000000000000000, 0.8660254037844387076, 1.000000000000000000, 0.8660254037844387076, 1.000000000000000000, 0.8660254037844387076, 1.000000000000000000, 0.8660254037844387076, 1.000000000000000000, 0.8660254037844387076, 1.000000000000000000, 0.8660254037844387076, 1.000000000000000000, 0.8660254037844387076, 1.000000000000000000, 0.8660254037844387076, 1.000000000000000000, 0.8660254037844387076, 1.000000000000000000, 0.8660254037844387076, 1.000000000000000000, 0.8660254037844387076, 1.000000000000000000, 0.8660254037844387076, 1.000000000000000000, 0.8660254037844387076, 1.000000000000000000, 0.8660254037844387076, 1.000000000000000000, 0.8660254037844387076, 1.000000000000000000, 0.8660254037844387076, 1.000000000000000000, 0.8660254037844387076, 1.000000000000000000, 0.8660254037844387076, 1.000000000000000000, 0.8660254037844387076, 1.000000000000000000, 0.9816628268209235397, 0.9683452906431546658 ) ) 
 REPRESENTATION_ITEM ( '' )  );
#208178 = CARTESIAN_POINT ( 'NONE',  ( 7.121056995675668411, 9.330985799753529264, -1.599625672291262513 ) ) ;
#208179 = CARTESIAN_POINT ( 'NONE',  ( 5.076602173674213070, 4.887400388900169368, 0.000000000000000000 ) ) ;
#208180 = CARTESIAN_POINT ( 'NONE',  ( 4.652862234063231739, -1.464609733205827879, 1.089778014065109657 ) ) ;
#208181 = CARTESIAN_POINT ( 'NONE',  ( 2.151677955860908487, -1.772288797910109404, -1.314638326115322053 ) ) ;
#208182 = VERTEX_POINT ( 'NONE', #109864 ) ;
#208183 = CARTESIAN_POINT ( 'NONE',  ( -7.795011973214244883, 8.058878488363559356, 0.7998128361456341429 ) ) ;
#208184 = CARTESIAN_POINT ( 'NONE',  ( 1.642778471875000035, -1.713541666188707291, -2.845375778867859751 ) ) ;
#208185 = CARTESIAN_POINT ( 'NONE',  ( -9.020252271793614440, 9.418049160047695878, 0.7998128361456462443 ) ) ;
#208186 = CARTESIAN_POINT ( 'NONE',  ( 0.9846354891296082990, -1.278160710921724341, 1.563951078967614094 ) ) ;
#208187 = CARTESIAN_POINT ( 'NONE',  ( -1.266901613973837604, 3.917879858053340048, 0.4965463943947248104 ) ) ;
#208188 = ORIENTED_EDGE ( 'NONE', *, *, #83083, .T. ) ;
#208189 = CARTESIAN_POINT ( 'NONE',  ( -5.472651281771599763, 6.413789912602166687, 1.199719254218452935 ) ) ;
#208190 = CARTESIAN_POINT ( 'NONE',  ( 3.027998222813840901, 0.9912708380838133326, 1.574746995948882455 ) ) ;
#208191 = CARTESIAN_POINT ( 'NONE',  ( 9.028840231696797503, 12.62106513936658203, -1.199719254218446718 ) ) ;
#208192 = CARTESIAN_POINT ( 'NONE',  ( 6.486953984781112403, -2.015912550161761629, 0.05229459904129707404 ) ) ;
#208193 = EDGE_LOOP ( 'NONE', ( #79000, #173592 ) ) ;
#208194 = ORIENTED_EDGE ( 'NONE', *, *, #2302, .F. ) ;
#208195 = CARTESIAN_POINT ( 'NONE',  ( -8.025536864285518490, 11.45054454405341282, -1.199719254218446718 ) ) ;
#208196 = CARTESIAN_POINT ( 'NONE',  ( 4.230939532379584200, 0.09184734775685021724, 1.823503176236190626 ) ) ;
#208198 = CARTESIAN_POINT ( 'NONE',  ( -5.012244793233714191, 6.784968962630095746, -1.449178643049347848 ) ) ;
#208197 = CARTESIAN_POINT ( 'NONE',  ( -3.806807270387036368, 7.663301925418665839, 0.000000000000000000 ) ) ;
#208199 = CARTESIAN_POINT ( 'NONE',  ( 5.612152705277200226, 7.484198595525810127, -1.333638438132278559 ) ) ;
#208200 = CARTESIAN_POINT ( 'NONE',  ( 6.468125021464292246, 1.674632898861495134, 1.122323893169609565 ) ) ;
#208201 = CARTESIAN_POINT ( 'NONE',  ( 5.437399513225577685, 0.7426265630364609072, -1.684910612069365321 ) ) ;
#208202 = CARTESIAN_POINT ( 'NONE',  ( 4.424672798056923817, 1.421823072290354872, -1.817590327873227052 ) ) ;
#208204 = CARTESIAN_POINT ( 'NONE',  ( 3.932747076415766596, 6.745899468197171345, 1.199719254218451159 ) ) ;
#208203 = B_SPLINE_CURVE_WITH_KNOTS ( 'NONE', 3,
 ( #176649, #125847, #28261, #42406, #91153, #93289, #109588, #26115 ),
 .UNSPECIFIED., .F., .F.,
 ( 4, 2, 2, 4 ),
 ( -5.999999999723453794E-08, 0.001495742970897297663, 0.002243644456345944907, 0.002991545941794591934 ),
 .UNSPECIFIED. ) ;
#208205 = CARTESIAN_POINT ( 'NONE',  ( 0.7903930413690943846, -2.044920356511644499, -0.2547782948326294816 ) ) ;
#208206 = CARTESIAN_POINT ( 'NONE',  ( 5.621827251160867789, 9.710548892996357040, 1.040834085586084257E-14 ) ) ;
#208207 = CARTESIAN_POINT ( 'NONE',  ( 1.962350597898457671, -1.776395552165145997, -0.7852436748517297449 ) ) ;
#208208 = CARTESIAN_POINT ( 'NONE',  ( 6.186922437512073714, -1.269050685324083050, -1.916131536371464383 ) ) ;
#208209 = DIRECTION ( 'NONE',  ( 0.6507913734559640506, -0.7592566023653004592, 0.000000000000000000 ) ) ;
#208210 = CARTESIAN_POINT ( 'NONE',  ( -8.072954122294394352, 8.383144328957069291, -0.7998128361456362523 ) ) ;
#208211 = AXIS2_PLACEMENT_3D ( 'NONE', #182977, #168862, #115910 ) ;
#208212 = CARTESIAN_POINT ( 'NONE',  ( 4.205816867194319464, -1.865656749788859647, 0.1373567816406878750 ) ) ;
#208213 = ORIENTED_EDGE ( 'NONE', *, *, #75497, .F. ) ;
#208215 = CARTESIAN_POINT ( 'NONE',  ( -3.949167883330528372, 7.829389307186077396, 1.214306433183764966E-14 ) ) ;
#208214 = CARTESIAN_POINT ( 'NONE',  ( 2.408343312057196872, -1.907530749141531423, -0.1368029246449145864 ) ) ;
#208216 = CARTESIAN_POINT ( 'NONE',  ( 4.213639274598267370, -0.3785452818781535611, 2.174016619501429215 ) ) ;
#208217 = CARTESIAN_POINT ( 'NONE',  ( -1.225000000000046052, 0.04166666734950023182, -0.7072540797573217963 ) ) ;
#208218 = CARTESIAN_POINT ( 'NONE',  ( -10.24975248460684440, 3.776839368175542777, 6.158671921171848140 ) ) ;
#208219 = CARTESIAN_POINT ( 'NONE',  ( 6.522881301506172846, 6.782652071278222117, -0.7216878364870458196 ) ) ;
#208220 = CARTESIAN_POINT ( 'NONE',  ( -5.872089928050201024, 8.904503111816948646, 1.082531754730550855 ) ) ;
#208221 = CARTESIAN_POINT ( 'NONE',  ( 2.143765197515819843, 0.7580581125649475949, -1.819971111534921970 ) ) ;
#208222 = CARTESIAN_POINT ( 'NONE',  ( 2.503307172793560298, 1.853534942699623045, -1.374368423928104876 ) ) ;
#208223 = CARTESIAN_POINT ( 'NONE',  ( 2.506241959165692812, 1.961374882610424919, 0.05109738790698423877 ) ) ;
#208224 = CARTESIAN_POINT ( 'NONE',  ( -5.285699784481336927, 7.260012063351913625, 1.599625672291263401 ) ) ;
#208225 = CARTESIAN_POINT ( 'NONE',  ( 6.754736851877535031, -0.5442653458712517489, -1.989433905422931748 ) ) ;
#208226 = CARTESIAN_POINT ( 'NONE',  ( 4.378920427533921078, 4.211088041652093494, 1.214306433183764966E-14 ) ) ;
#208227 = CARTESIAN_POINT ( 'NONE',  ( 4.030482632556767975, 0.5424685788828055300, 1.942097399793737633 ) ) ;
#208228 = CARTESIAN_POINT ( 'NONE',  ( 3.203469434578891661, 6.959407783642502565, -0.7998128361456362523 ) ) ;
#208229 = VERTEX_POINT ( 'NONE', #107728 ) ;
#208230 = CARTESIAN_POINT ( 'NONE',  ( 4.751185534883737738, 0.1928377863454934504, -2.007255887737584121 ) ) ;
#208231 = CARTESIAN_POINT ( 'NONE',  ( 0.7500000000000006661, 10.08333333333333215, 1.299038105676657340 ) ) ;
#208232 = CARTESIAN_POINT ( 'NONE',  ( 11.78331023100045627, 13.79999999999998295, 1.799999999999999600 ) ) ;
#208233 = CARTESIAN_POINT ( 'NONE',  ( -0.4500000000000163869, 3.950000000000009059, -1.561251128379126385E-14 ) ) ;
#208234 = CARTESIAN_POINT ( 'NONE',  ( 9.856941372335116469, 11.45851867493453291, 1.199719254218450271 ) ) ;
#208235 = CARTESIAN_POINT ( 'NONE',  ( 1.938562956190786002, -1.164097522067691903, 1.832441342696682574 ) ) ;
#208236 = CARTESIAN_POINT ( 'NONE',  ( 4.193214648376505593, 8.114110533073061404, 0.000000000000000000 ) ) ;
#208237 = CARTESIAN_POINT ( 'NONE',  ( -8.770850689852672133, 14.55305235829676391, -8.174590314132164082 ) ) ;
#208238 = CARTESIAN_POINT ( 'NONE',  ( 2.969827553264007047, 0.9974664638083343693, 1.582205488144486250 ) ) ;
#208239 = CARTESIAN_POINT ( 'NONE',  ( 6.362596528949501895, -1.533591692085239266, 1.523617273982772247 ) ) ;
#208240 = AXIS2_PLACEMENT_3D ( 'NONE', #56164, #122328, #185072 ) ;
#208242 = CARTESIAN_POINT ( 'NONE',  ( 6.827182134110203471, 1.269052739965634391, 2.024653661457261222 ) ) ;
#208241 = CARTESIAN_POINT ( 'NONE',  ( 0.000000000000000000, 6.999999999999999112, 0.000000000000000000 ) ) ;
#208243 = CARTESIAN_POINT ( 'NONE',  ( 0.6823417656249899377, 0.5927083336747518416, 1.181850606188755259 ) ) ;
#208244 = CARTESIAN_POINT ( 'NONE',  ( 3.633378786761193968, -0.1378984027537045187, 1.907353237798288470 ) ) ;
#208245 = CARTESIAN_POINT ( 'NONE',  ( 4.188192146485575584, -1.750654529572701179, -0.2590412592250490587 ) ) ;
#208246 = CARTESIAN_POINT ( 'NONE',  ( 2.156764536687346467, 0.4205103164258168769, 1.865301821287323136 ) ) ;
#208247 = CARTESIAN_POINT ( 'NONE',  ( -4.578903193113314174, 6.365139696764064325, 1.599625672291267398 ) ) ;
#208249 = CARTESIAN_POINT ( 'NONE',  ( 6.556256410252866651, -1.173993033552203968, 1.514159254448317782 ) ) ;
#208248 = DIRECTION ( 'NONE',  ( 1.000000000000000000, 0.000000000000000000, 0.000000000000000000 ) ) ;
#208250 = CARTESIAN_POINT ( 'NONE',  ( 1.499999999999987566, -0.4749999999999823808, 0.000000000000000000 ) ) ;
#208251 = CARTESIAN_POINT ( 'NONE',  ( 1.311079954825690619, -1.633285661836245906, 1.272233187909928454 ) ) ;
#208252 = CARTESIAN_POINT ( 'NONE',  ( -0.6823417656250003738, -0.9697916663252494907, -1.181850606188749264 ) ) ;
#208253 = CARTESIAN_POINT ( 'NONE',  ( 6.526239545637954720, 1.075124705556152138, -1.530631868311462362 ) ) ;
#208254 = CARTESIAN_POINT ( 'NONE',  ( 1.629252094361890890, -1.719607636260962025, 0.6136192449261099746 ) ) ;
#208256 = CARTESIAN_POINT ( 'NONE',  ( 4.614363445337835934, 8.349151705029461468, -0.2795175495247017583 ) ) ;
#208255 = CARTESIAN_POINT ( 'NONE',  ( 5.496761087669068679, -0.5331231007881258588, -2.141394884921154151 ) ) ;
#208257 = EDGE_CURVE ( 'NONE', #182623, #192862, #79240, .T. ) ;
#208258 = CARTESIAN_POINT ( 'NONE',  ( -1.001543065824772872E-14, 5.634375000341415252, 1.575800808251672791 ) ) ;
#208259 = CARTESIAN_POINT ( 'NONE',  ( 3.139185485588998237, -0.1492200975972737820, -2.057319831125117737 ) ) ;
#208260 = CARTESIAN_POINT ( 'NONE',  ( -7.121056995675673740, 9.330985799753529264, -1.599625672291263179 ) ) ;
#208261 = CARTESIAN_POINT ( 'NONE',  ( 8.483651433849084711, 10.92067931095586886, 1.599625672291281386 ) ) ;
#208262 = CARTESIAN_POINT ( 'NONE',  ( 1.354873262373950116, 3.776319345677265460, -0.6436764175676652489 ) ) ;
#208263 = CARTESIAN_POINT ( 'NONE',  ( -0.02191186323001123593, -9.962467934940974601, -10.91967397018793129 ) ) ;
#208264 = CARTESIAN_POINT ( 'NONE',  ( 6.587282531393223728, 8.778525268082516320, 1.599625672291268286 ) ) ;
#208265 = EDGE_LOOP ( 'NONE', ( #19796, #200127, #103529, #207928, #95206 ) ) ;
#208266 = CARTESIAN_POINT ( 'NONE',  ( 4.861816338261779613, -0.5554421346023461492, 1.994381909410049669 ) ) ;
#208267 = CARTESIAN_POINT ( 'NONE',  ( -0.6823417656250003738, 0.2802083336747515641, -1.181850606188749264 ) ) ;
#208268 = CARTESIAN_POINT ( 'NONE',  ( 3.005316911853897821, 1.824354345256746557, 1.159134172154026032 ) ) ;
#208269 = CARTESIAN_POINT ( 'NONE',  ( -4.651028767811522080, 8.324525799487361155, 0.4279074293446327171 ) ) ;
#208270 = CARTESIAN_POINT ( 'NONE',  ( 2.754561962923445684, 2.004688795240500365, 0.2448751400806712664 ) ) ;
#208271 = CARTESIAN_POINT ( 'NONE',  ( 6.620655732516647518, 3.684600858287550906, 2.687722323901103660 ) ) ;
#208272 = EDGE_CURVE ( 'NONE', #41470, #75032, #134624, .T. ) ;
#208274 = CARTESIAN_POINT ( 'NONE',  ( 6.968527767744104651, 8.192665819532020777, 1.082531754730558626 ) ) ;
#208273 = CARTESIAN_POINT ( 'NONE',  ( 3.475000000000000533, -1.254166666666665098, 2.006292185433948827 ) ) ;
#208275 = CARTESIAN_POINT ( 'NONE',  ( -5.921879234118920365, 10.13088588310589699, 0.000000000000000000 ) ) ;
#208276 = CARTESIAN_POINT ( 'NONE',  ( 1.147673126774436225, 1.985868168208399842, -0.3494872464938902357 ) ) ;
#208278 = CARTESIAN_POINT ( 'NONE',  ( 5.689076433642084041, 1.658752129386225516, 1.432425853890168188 ) ) ;
#208277 = CARTESIAN_POINT ( 'NONE',  ( -4.229253852459088137, 7.021547696922494808, 1.199719254218464037 ) ) ;
#208279 = CARTESIAN_POINT ( 'NONE',  ( -3.730655187671924722, 7.355891203230078723, 0.6115009643793259952 ) ) ;
#208280 = CARTESIAN_POINT ( 'NONE',  ( 4.886922752366290368, -1.802716094696995786, -0.6387714794457154399 ) ) ;
#208281 = CARTESIAN_POINT ( 'NONE',  ( -4.464712657601869417, 4.103252943490596216, 0.7998128361456341429 ) ) ;
#208282 = CARTESIAN_POINT ( 'NONE',  ( 5.544921637864819175, 7.492161215640853023, -1.443375672974057666 ) ) ;
#208284 = CARTESIAN_POINT ( 'NONE',  ( 3.708611378246814638, 1.915606880664010747, 0.6298579873919087913 ) ) ;
#208283 = CARTESIAN_POINT ( 'NONE',  ( -9.286972035236626510, 11.85788667924133399, -1.443375672974058777 ) ) ;
#208285 = CARTESIAN_POINT ( 'NONE',  ( 0.6823417656249969321, 13.58854166700806942, -1.181850606188757036 ) ) ;
#208286 = CARTESIAN_POINT ( 'NONE',  ( 5.842733193948632220, 0.3409603658401075821, 1.690541223788865510 ) ) ;
#208287 = CARTESIAN_POINT ( 'NONE',  ( 6.444921918449731280, 8.612437886315108315, 1.599625672291268286 ) ) ;
#208288 = CARTESIAN_POINT ( 'NONE',  ( 8.405692050792682224, 12.75046512599275772, -0.7216878364870328300 ) ) ;
#208289 = CARTESIAN_POINT ( 'NONE',  ( -11.52888687719611660, 11.29423125105035730, -3.331331986263548650 ) ) ;
#208290 = CARTESIAN_POINT ( 'NONE',  ( 4.305816765424046011, -1.865681898550693107, 0.1353468896250972775 ) ) ;
#208291 = DIRECTION ( 'NONE',  ( -1.207943261119674327E-30, -2.168404344971008079E-15, 1.000000000000000000 ) ) ;
#208293 = CIRCLE ( 'NONE', #146185, 2.000000000000006661 ) ;
#208292 = CARTESIAN_POINT ( 'NONE',  ( 1.217730340897508645, 0.4076058164220326407, -2.029561569317724690 ) ) ;
#208294 = CARTESIAN_POINT ( 'NONE',  ( -2.580963302752292243, -0.4788041664876945269, 0.000000000000000000 ) ) ;
#208295 = ORIENTED_EDGE ( 'NONE', *, *, #202413, .T. ) ;
#208296 = CARTESIAN_POINT ( 'NONE',  ( 6.375650462676996533, 0.3020505593925585375, -1.785944618546008833 ) ) ;
#208298 = CARTESIAN_POINT ( 'NONE',  ( 5.578253857379852576, 5.472660686556754861, -0.7998128361456481317 ) ) ;
#208297 = AXIS2_PLACEMENT_3D ( 'NONE', #173440, #188592, #189656 ) ;
#208300 = ADVANCED_FACE ( 'NONE', ( #142329 ), #208341, .T. ) ;
#208299 = CARTESIAN_POINT ( 'NONE',  ( -0.07068620461728526705, -1.560437159073333468, -1.276799021846956705 ) ) ;
#208301 = CARTESIAN_POINT ( 'NONE',  ( 0.5096461351858303512, -0.6515609501748579335, 1.690550641884549954 ) ) ;
#208302 = CARTESIAN_POINT ( 'NONE',  ( 5.356880090730863131, 7.343055753976412525, 1.443375672974064550 ) ) ;
#208303 = CARTESIAN_POINT ( 'NONE',  ( 9.502044606515637426, 13.11535572295773555, 7.329770145308074802 ) ) ;
#208304 = ORIENTED_EDGE ( 'NONE', *, *, #107978, .T. ) ;
#208305 = CARTESIAN_POINT ( 'NONE',  ( 8.012505595552012139, 11.33137838057728786, -1.082531754730543083 ) ) ;
#208307 = CARTESIAN_POINT ( 'NONE',  ( 8.613507663383630941, 8.943513783569379427, -0.7998128361456221525 ) ) ;
#208306 = CARTESIAN_POINT ( 'NONE',  ( 0.2562055958934654210, -1.961350414083770977, -0.05204156388862594962 ) ) ;
#208308 = CARTESIAN_POINT ( 'NONE',  ( 5.044510182127093678, -1.384340171167136369, 1.324308159167127075 ) ) ;
#208309 = CARTESIAN_POINT ( 'NONE',  ( 0.000000000000000000, 13.49999999999999822, 0.000000000000000000 ) ) ;
#208310 = CARTESIAN_POINT ( 'NONE',  ( -6.232040409365024125, 6.934648621905299848, 0.8351839086257698552 ) ) ;
#208311 = ADVANCED_FACE ( 'NONE', ( #145544, #81555 ), #181185, .F. ) ;
#208312 = PRESENTATION_STYLE_ASSIGNMENT (( #106615 ) ) ;
#208314 = EDGE_LOOP ( 'NONE', ( #193825, #76935, #212404, #133129 ) ) ;
#208313 = CARTESIAN_POINT ( 'NONE',  ( 5.233084105194869551, 6.167981546557892436, -1.082531754730548412 ) ) ;
#208315 = CARTESIAN_POINT ( 'NONE',  ( -8.270110514656041190, 10.67154823856396817, 1.443375672974090751 ) ) ;
#208316 = CARTESIAN_POINT ( 'NONE',  ( 2.342841879718413622, 0.4729757327756217156, 2.109170662781891359 ) ) ;
#208317 = CARTESIAN_POINT ( 'NONE',  ( -3.797165540279144214, 6.587721009371067638, 1.199719254218452935 ) ) ;
#208318 = CARTESIAN_POINT ( 'NONE',  ( 5.533136088152891929, 9.469426179571447832, -0.7216878364870458196 ) ) ;
#208319 = CARTESIAN_POINT ( 'NONE',  ( 0.1938080739139167730, 1.976361990896974508, -0.7691651810952588875 ) ) ;
#208320 = CARTESIAN_POINT ( 'NONE',  ( 4.366094929315432083, 0.8608494910617261464, 1.609850404305966265 ) ) ;
#208321 = CARTESIAN_POINT ( 'NONE',  ( 9.053633104220391914, 12.24030617166337898, -7.400564859916917371 ) ) ;
#208322 = CARTESIAN_POINT ( 'NONE',  ( 1.335163258876404857, -1.783904897583366012, 0.8392522581757311251 ) ) ;
#208323 = CARTESIAN_POINT ( 'NONE',  ( 3.304848191199673213, -0.3775801424153284458, -1.874573493127674961 ) ) ;
#208324 = ORIENTED_EDGE ( 'NONE', *, *, #68527, .F. ) ;
#208325 = CARTESIAN_POINT ( 'NONE',  ( 0.2999999999999807265, 4.000000000000008882, 1.007084189318371514 ) ) ;
#208326 = CARTESIAN_POINT ( 'NONE',  ( 4.299236425489592506, -1.714783525531939690, 0.9686585690476202659 ) ) ;
#208327 = EDGE_LOOP ( 'NONE', ( #99905, #36391, #112621, #22231, #89137, #15955 ) ) ;
#208328 = CARTESIAN_POINT ( 'NONE',  ( 5.583525073002030048, -0.8696438758921558598, 1.736526053206193243 ) ) ;
#208329 = ORIENTED_EDGE ( 'NONE', *, *, #139632, .T. ) ;
#208330 = CARTESIAN_POINT ( 'NONE',  ( -6.448838341955544173, 7.552674816150118708, 1.199719254218452047 ) ) ;
#208332 = CARTESIAN_POINT ( 'NONE',  ( 6.416280414004661203, -2.120105685773795212, 0.05337830808049835035 ) ) ;
#208331 = CARTESIAN_POINT ( 'NONE',  ( -5.635349125135588721, 6.603604063193491136, 1.199719254218452935 ) ) ;
#208333 = CARTESIAN_POINT ( 'NONE',  ( 6.739811759324814133, 8.956476034002680109, -1.443375672974078761 ) ) ;
#208335 = ORIENTED_EDGE ( 'NONE', *, *, #161090, .T. ) ;
#208334 = CARTESIAN_POINT ( 'NONE',  ( 4.160738352132353768, 0.5130957772990808463, 1.842076966104645663 ) ) ;
#208336 = CARTESIAN_POINT ( 'NONE',  ( -9.499700864329909678, -7.154544010627095219, -0.07538891330675204228 ) ) ;
#208337 = CARTESIAN_POINT ( 'NONE',  ( 0.000000000000000000, 0.5000000000000004441, -3.475000000000000089 ) ) ;
#208338 = STYLED_ITEM ( 'NONE', ( #132995 ), #30072 ) ;
#208339 = CARTESIAN_POINT ( 'NONE',  ( 9.518950567327413737, 3.582805947358006282, -7.307358422849591584 ) ) ;
#208340 = CARTESIAN_POINT ( 'NONE',  ( 5.479157358542966705, -1.820838119324312165, -0.8587918944957111389 ) ) ;
#208341 = CYLINDRICAL_SURFACE ( 'NONE', #117016, 1.224999999999996980 ) ;
#208342 = CARTESIAN_POINT ( 'NONE',  ( 6.674438497507635404, -1.118711561685633349, 1.443368817030561635 ) ) ;
#208343 = CARTESIAN_POINT ( 'NONE',  ( 2.242711981562468093, -2.029969483702593003, -0.4061203719310027549 ) ) ;
#208344 = CARTESIAN_POINT ( 'NONE',  ( -7.700668062882072284, 10.00719871149432549, -1.443375672974059665 ) ) ;
#208345 = CARTESIAN_POINT ( 'NONE',  ( -5.826481282663010575, 7.222486169913409526, -1.172043233395845485 ) ) ;
#208346 = DIRECTION ( 'NONE',  ( -1.000000000000000000, 0.000000000000000000, 0.000000000000000000 ) ) ;
#208347 = CARTESIAN_POINT ( 'NONE',  ( 6.772336237553374438, -1.148929780121176414, 1.476827877338216854 ) ) ;
#208348 = CARTESIAN_POINT ( 'NONE',  ( 6.043183783389218355, 8.073467052085995022, 1.599625672291267398 ) ) ;
#208349 = SURFACE_STYLE_FILL_AREA ( #9097 ) ;
#208350 = CARTESIAN_POINT ( 'NONE',  ( 5.560252395380222090, 5.659585014131299552, 0.7216878364870328300 ) ) ;
#208351 = CARTESIAN_POINT ( 'NONE',  ( 2.703961570921634028, 5.242040035128820108, -1.199719254218446718 ) ) ;
#208352 = CARTESIAN_POINT ( 'NONE',  ( -1.364683531250000748, 12.17187500034139980, 0.000000000000000000 ) ) ;
#208353 = CARTESIAN_POINT ( 'NONE',  ( -5.922214171070950606, 5.803671375871217286, -0.7998128361456291469 ) ) ;
#208354 = CARTESIAN_POINT ( 'NONE',  ( -6.038177310039794854, 8.137902509836795417, -1.599625672291271394 ) ) ;
#208355 = CARTESIAN_POINT ( 'NONE',  ( 4.430095426116970714, -1.344173880920132458, -1.095666204706043700 ) ) ;
#208356 = CIRCLE ( 'NONE', #31972, 0.08000000000000020983 ) ;
#208357 = CARTESIAN_POINT ( 'NONE',  ( -4.904298879841297421, 6.744767997946721216, 1.599625672291267398 ) ) ;
#208358 = AXIS2_PLACEMENT_3D ( 'NONE', #73835, #144222, #210216 ) ;
#208359 = CARTESIAN_POINT ( 'NONE',  ( 2.325130699016836555, -1.891071737562114219, -0.8429460452448679364 ) ) ;
#208360 = CARTESIAN_POINT ( 'NONE',  ( 3.743865479105834559, 2.100983596406953424, -0.2614307623071217557 ) ) ;
#208361 = CARTESIAN_POINT ( 'NONE',  ( 7.507464373665139412, 9.781794407407920389, 1.599625672291281386 ) ) ;
#208362 = CARTESIAN_POINT ( 'NONE',  ( 0.09005296632881229502, -9.916958724994124452, 10.99963137851698924 ) ) ;
#208363 = CARTESIAN_POINT ( 'NONE',  ( 2.237097273892864724, -0.09148514208244534762, -1.967424487969974711 ) ) ;
#208364 = CARTESIAN_POINT ( 'NONE',  ( 5.946581215072361815, 6.122072269273588496, 0.7275674859277461159 ) ) ;
#208365 = CARTESIAN_POINT ( 'NONE',  ( 4.378920427533921078, 4.211088041652093494, 1.214306433183764966E-14 ) ) ;
#208367 = CARTESIAN_POINT ( 'NONE',  ( 10.91962425643199985, -9.999999999999994671, -0.09058751758333170867 ) ) ;
#208366 = CARTESIAN_POINT ( 'NONE',  ( -1.737500000000000266, -2.508333333333334636, -3.009438278150923907 ) ) ;
#208368 = CARTESIAN_POINT ( 'NONE',  ( 3.539304732165698741, -1.735471681261467669, -1.497634786905965187 ) ) ;
#208369 = CARTESIAN_POINT ( 'NONE',  ( 0.3986991128735201673, 1.519733473351183362, -1.011397189243423700 ) ) ;
#208370 = CARTESIAN_POINT ( 'NONE',  ( 7.015418140428412386, 7.149352350113456822, 0.7998128361456331437 ) ) ;
#208371 = CARTESIAN_POINT ( 'NONE',  ( 5.612712405933139692, 9.491988873656591608, 1.040834085586084257E-14 ) ) ;
#208372 = CARTESIAN_POINT ( 'NONE',  ( -9.182950115157607840, 9.607863310639020327, 0.7998128361456462443 ) ) ;
#208373 = CARTESIAN_POINT ( 'NONE',  ( 1.564699064445768784, 0.6353654490140858702, 1.910354371721780797 ) ) ;
#208374 = CARTESIAN_POINT ( 'NONE',  ( 2.395295693335119935, -1.754585731169123752, 0.8775363634117984146 ) ) ;
#208375 = CARTESIAN_POINT ( 'NONE',  ( -8.616370316684697883, 10.01118577667568132, -1.199719254218446718 ) ) ;
#208376 = CARTESIAN_POINT ( 'NONE',  ( -5.876569516519495551, 8.943415971659659292, 1.199719254218452047 ) ) ;
#208377 = DIRECTION ( 'NONE',  ( 0.7592566023653005702, -0.6507913734559640506, 0.000000000000000000 ) ) ;
#208379 = CARTESIAN_POINT ( 'NONE',  ( 3.643183530381717716, -1.339777920602200467, -1.156514101391445948 ) ) ;
#208378 = CARTESIAN_POINT ( 'NONE',  ( 4.874988757033254849, 1.950858131582337007, -0.7520741601412093136 ) ) ;
#208380 = CARTESIAN_POINT ( 'NONE',  ( -4.415768667553307481E-15, 0.1250000006828069499, 1.224999999999963229 ) ) ;
#208381 = EDGE_CURVE ( 'NONE', #156, #78199, #102407, .T. ) ;
#208382 = CARTESIAN_POINT ( 'NONE',  ( 6.298803545911215274, 1.902247386433516541, 1.278772944020603930 ) ) ;
#208383 = CARTESIAN_POINT ( 'NONE',  ( 5.244012475127576955, 0.5104456934865635453, 1.663790013937071599 ) ) ;
#208384 = CARTESIAN_POINT ( 'NONE',  ( 8.586391356156291010, 8.911878091804165791, 0.7998128361456481317 ) ) ;
#208385 = CARTESIAN_POINT ( 'NONE',  ( 6.486976479784771321, -2.298278054978039275, 0.05155775693151467415 ) ) ;
#208386 = CARTESIAN_POINT ( 'NONE',  ( 5.009033543107539899, 1.729337909971711662, 0.1259922892337256017 ) ) ;
#208387 = CARTESIAN_POINT ( 'NONE',  ( 5.389208567375425751, 0.1545246996936377182, 2.165725388718000133 ) ) ;
#208388 = DIRECTION ( 'NONE',  ( 0.000000000000000000, -1.000000000000000000, 0.000000000000000000 ) ) ;
#208389 = CARTESIAN_POINT ( 'NONE',  ( 6.456263137377813877, -1.236968576560824040, 1.593241027169020052 ) ) ;
#208390 = CARTESIAN_POINT ( 'NONE',  ( 4.906250000000003553, 1.895863743163974213, -0.7852924748302423374 ) ) ;
#208391 = CARTESIAN_POINT ( 'NONE',  ( -3.386512176934025842, 6.359426010807541552, 0.9097930222844696768 ) ) ;
#208392 = CARTESIAN_POINT ( 'NONE',  ( 4.665017848976360071, -1.720483299173672043, -0.8667214970639931515 ) ) ;
#208393 = CARTESIAN_POINT ( 'NONE',  ( 1.499999999999993117, 11.13541666734946567, 0.8660254037844409281 ) ) ;
#208394 = CARTESIAN_POINT ( 'NONE',  ( 0.4521970297205242240, -1.575145348204033180, -1.566492488853583387 ) ) ;
#208395 = EDGE_LOOP ( 'NONE', ( #55923, #39345 ) ) ;
#208396 = CARTESIAN_POINT ( 'NONE',  ( 0.7499999999999920064, 4.233333333333352932, 1.299038105676669330 ) ) ;
#208397 = CARTESIAN_POINT ( 'NONE',  ( 5.671388329218120639, 5.511041227042920099, 1.040834085586084257E-14 ) ) ;
#208398 = CARTESIAN_POINT ( 'NONE',  ( 7.806797523370503811, 8.002351953554066810, 1.040834085586084257E-14 ) ) ;
#208399 = CARTESIAN_POINT ( 'NONE',  ( 2.104415045828517350, -0.9466870704337572162, 2.009588771043930411 ) ) ;
#208400 = FILL_AREA_STYLE_COLOUR ( '', #208755 ) ;
#208401 = CARTESIAN_POINT ( 'NONE',  ( 7.782016984564065432, 8.181367358187307204, 0.7216878364870458196 ) ) ;
#208402 = CARTESIAN_POINT ( 'NONE',  ( -8.310784975052669665, 12.63974020429606249, -0.7216878364870267237 ) ) ;
#208403 = CARTESIAN_POINT ( 'NONE',  ( 6.536439455564164724, 7.758839131980592718, 1.082531754730549967 ) ) ;
#208404 = CARTESIAN_POINT ( 'NONE',  ( 0.8267963299631932994, 0.8146243292815741333, -1.844710905833810255 ) ) ;
#208406 = CARTESIAN_POINT ( 'NONE',  ( 5.951645758832087907, 1.559603009536973284, 1.349993227703372156 ) ) ;
#208405 = CARTESIAN_POINT ( 'NONE',  ( 9.738834413317897898, 10.25639499182604730, 0.000000000000000000 ) ) ;
#208407 = CARTESIAN_POINT ( 'NONE',  ( 0.7499999999999902300, 5.316666666666685082, -1.299038105676658228 ) ) ;
#208408 = CARTESIAN_POINT ( 'NONE',  ( -3.277320446201389181, 4.846626492033466072, 1.599625672291267398 ) ) ;
#208409 = CARTESIAN_POINT ( 'NONE',  ( -2.308604159940524703, 5.474475169625423909, -0.7811085970239580734 ) ) ;
#208410 = CARTESIAN_POINT ( 'NONE',  ( 1.364683531249988757, 0.8843750003414210248, 0.000000000000000000 ) ) ;
#208411 = CARTESIAN_POINT ( 'NONE',  ( 0.7019891895669374549, -0.5885738721268447549, -1.669159149975569578 ) ) ;
#208412 = CARTESIAN_POINT ( 'NONE',  ( 6.100242454504600786, -0.2022020391262440986, 1.722246827497366795 ) ) ;
#208413 = CARTESIAN_POINT ( 'NONE',  ( 5.864775363713938816, 0.1190308195875185160, -1.736441914165016476 ) ) ;
#208414 = CARTESIAN_POINT ( 'NONE',  ( 3.210744404368763405, 2.073164229931067304, 0.9784878017504093917 ) ) ;
#208415 = CARTESIAN_POINT ( 'NONE',  ( -1.402160292154681736E-14, 0.1968750003414221628, -1.575800808251665908 ) ) ;
#208416 = CARTESIAN_POINT ( 'NONE',  ( 2.624749632297512569, -1.717891791495285592, 0.6627527109525217508 ) ) ;
#208417 = CARTESIAN_POINT ( 'NONE',  ( 8.886479618753304166, 12.45497775759917758, -1.199719254218446718 ) ) ;
#208418 = SHAPE_REPRESENTATION_RELATIONSHIP ( 'NONE' , 'NONE' ,  #135824, #24096 ) ;
#208419 = CARTESIAN_POINT ( 'NONE',  ( 2.590611583786633254, -0.3098195481324728107, -1.798931244660670448 ) ) ;
#208420 = CARTESIAN_POINT ( 'NONE',  ( 3.305314717767214638, 1.277042846462652204, -1.560500556308255238 ) ) ;
#208421 = CARTESIAN_POINT ( 'NONE',  ( -2.779058300676974014, 6.186059084191009916, -0.7216878364870257245 ) ) ;
#208422 = CARTESIAN_POINT ( 'NONE',  ( -15.75000000000000000, 11.29999999999999893, -1.800000000000001155 ) ) ;
#208423 = CARTESIAN_POINT ( 'NONE',  ( 5.192451847192011805, -2.089709803398311028, -0.2606072588380181076 ) ) ;
#208424 = CARTESIAN_POINT ( 'NONE',  ( -6.358937740009323214, 7.377514437221045718, -1.199719254218446718 ) ) ;
#208425 = CARTESIAN_POINT ( 'NONE',  ( 7.457833306149189490, 16.00157973104908393, 10.25342808721416077 ) ) ;
#208426 = CARTESIAN_POINT ( 'NONE',  ( 2.119664376568120012, 0.3561266789769075292, -2.039353370234835872 ) ) ;
#208427 = CARTESIAN_POINT ( 'NONE',  ( 4.325214697959421706, 5.004837554829479451, 1.199719254218462483 ) ) ;
#208428 = CARTESIAN_POINT ( 'NONE',  ( -1.360316468750021768, 0.1718750003414371008, -3.295974604355933479E-14 ) ) ;
#208429 = CARTESIAN_POINT ( 'NONE',  ( 4.863993733624056404, 0.6645719631460760279, -2.013739200842738608 ) ) ;
#208430 = CARTESIAN_POINT ( 'NONE',  ( 0.3988885142760539293, 1.602443225120395720, -1.069099046168849876 ) ) ;
#208431 = ORIENTED_EDGE ( 'NONE', *, *, #158613, .T. ) ;
#208432 = CARTESIAN_POINT ( 'NONE',  ( -3.156015896931072540, 6.904045323053366268, 0.000000000000000000 ) ) ;
#208433 = CARTESIAN_POINT ( 'NONE',  ( 8.666686507633574621, 11.13422023037111330, 1.599625672291281386 ) ) ;
#208434 = CARTESIAN_POINT ( 'NONE',  ( 5.031484404002879884, 6.963427452793765404, 1.443375672974065660 ) ) ;
#208435 = CARTESIAN_POINT ( 'NONE',  ( 1.001543065824772753E-15, -1.268749999044083587, 4.012584370867899430 ) ) ;
#208436 = CARTESIAN_POINT ( 'NONE',  ( -6.013204822860843457, 6.974159367214481264, -1.199719254218446718 ) ) ;
#208437 = CARTESIAN_POINT ( 'NONE',  ( 6.381110825713084189, -1.939362502171553482, -0.8581636585355473246 ) ) ;
#208438 = CARTESIAN_POINT ( 'NONE',  ( 2.063634109657853433, 0.3607628843028657939, -2.074664996798830874 ) ) ;
#208439 = CARTESIAN_POINT ( 'NONE',  ( -5.061990249855848667, 6.999017606288844284, -1.599625672291271394 ) ) ;
#208440 = CARTESIAN_POINT ( 'NONE',  ( 9.074484886248265880, 9.481320543578137361, 0.7998128361456462443 ) ) ;
#208441 = CARTESIAN_POINT ( 'NONE',  ( 6.051566885458855793, 1.408179756913958913, 1.216655509429155124 ) ) ;
#208442 = CARTESIAN_POINT ( 'NONE',  ( 7.721532178182734185, 8.967207948423393304, 1.199719254218462483 ) ) ;
#208443 = CARTESIAN_POINT ( 'NONE',  ( -4.981695098378565945, 4.776675467721892332, -0.7998128361456362523 ) ) ;
#208444 = CARTESIAN_POINT ( 'NONE',  ( -8.649738815838677652, 13.03518635187974262, 0.7216878364870357165 ) ) ;
#208445 = CIRCLE ( 'NONE', #66492, 9.616019636405020776 ) ;
#208446 = CARTESIAN_POINT ( 'NONE',  ( 0.2992908618118708675, -0.2657624787030036240, -2.103842954668332599 ) ) ;
#208447 = PLANE ( 'NONE',  #5529 ) ;
#208449 = CARTESIAN_POINT ( 'NONE',  ( 2.699599903323801620, -1.451799986561516764, -1.319707477925702310 ) ) ;
#208448 = CARTESIAN_POINT ( 'NONE',  ( -0.6125000000000105915, -0.9583333333333110549, 1.060881119635910252 ) ) ;
#208450 = CARTESIAN_POINT ( 'NONE',  ( 1.288190726105652217, -0.9714702286227733241, 1.931199087792371261 ) ) ;
#208451 = CIRCLE ( 'NONE', #14715, 2.011244508837062295 ) ;
#208453 = CARTESIAN_POINT ( 'NONE',  ( -6.123385318682658784, 6.005027156464323390, -0.2239653954101868127 ) ) ;
#208452 = CARTESIAN_POINT ( 'NONE',  ( -3.786470039966538970, 7.639575156594750283, 0.000000000000000000 ) ) ;
#208454 = CARTESIAN_POINT ( 'NONE',  ( -1.364683531250012516, 1.530208333674756505, 0.7879004041258379498 ) ) ;
#208455 = CARTESIAN_POINT ( 'NONE',  ( 2.589492015636893907, -1.735658606974595619, -0.1281804514613407997 ) ) ;
#208456 = CARTESIAN_POINT ( 'NONE',  ( 6.860062538834778678, 8.066123052471139587, -1.082531754730543083 ) ) ;
#208457 = CARTESIAN_POINT ( 'NONE',  ( -11.03376256896084584, 6.348997720274319079, -6.086949085616508270 ) ) ;
#208458 = EDGE_CURVE ( 'NONE', #131174, #124865, #194238, .T. ) ;
#208459 = CARTESIAN_POINT ( 'NONE',  ( 2.302111043707856020, -1.802142186715177674, 0.9039695891032775155 ) ) ;
#208460 = FACE_OUTER_BOUND ( 'NONE', #87979, .T. ) ;
#208461 = CARTESIAN_POINT ( 'NONE',  ( -3.623772196602547346, 7.449761006003425834, 0.000000000000000000 ) ) ;
#208462 = CARTESIAN_POINT ( 'NONE',  ( 2.377750047251852017, 1.211369778508808448, 1.555330764497768303 ) ) ;
#208464 = CARTESIAN_POINT ( 'NONE',  ( -7.119440060951841787, 7.478637290631501067, 0.000000000000000000 ) ) ;
#208463 = CARTESIAN_POINT ( 'NONE',  ( 6.064708884584704585, 0.6063723501847050334, 1.813766235492550560 ) ) ;
#208465 = CARTESIAN_POINT ( 'NONE',  ( -5.844973620822877969, 7.912498205750389424, 1.443375672974058777 ) ) ;
#208466 = CARTESIAN_POINT ( 'NONE',  ( 5.037736595929563244, 8.035053907629919223, -1.199719254218452047 ) ) ;
#208467 = CARTESIAN_POINT ( 'NONE',  ( -7.391130018105325661, 8.652015104991543026, -1.199719254218452047 ) ) ;
#208468 = CARTESIAN_POINT ( 'NONE',  ( 1.225266875139136458, 1.782313340379863442, 0.9499306202595361182 ) ) ;
#208469 = CARTESIAN_POINT ( 'NONE',  ( 4.243338890952890630, 5.973648010910253880, -1.443375672974051449 ) ) ;
#208470 = CARTESIAN_POINT ( 'NONE',  ( 6.264718444480717352, -1.637942392629457178, 1.625721277839597745 ) ) ;
#208471 = CARTESIAN_POINT ( 'NONE',  ( 6.391066755906244623, 0.1909826923555627554, 1.952524381009380861 ) ) ;
#208472 = CARTESIAN_POINT ( 'NONE',  ( 2.992962298452767289, 0.2353761085502041883, 1.947492218917420637 ) ) ;
#208473 = CARTESIAN_POINT ( 'NONE',  ( 9.097684769969825780, 10.57271930550834860, -1.199719254218446718 ) ) ;
#208474 = CARTESIAN_POINT ( 'NONE',  ( 0.7213275451133926985, 1.987047012402185731, 0.3419330716275259530 ) ) ;
#208475 = ORIENTED_EDGE ( 'NONE', *, *, #141556, .F. ) ;
#208476 = CARTESIAN_POINT ( 'NONE',  ( 1.534521455381025801, 0.6695800964386169341, 2.008721144947374526 ) ) ;
#208478 = CARTESIAN_POINT ( 'NONE',  ( -5.533699252672048985, 9.607732894759390518, -0.7998128361456231517 ) ) ;
#208477 = CARTESIAN_POINT ( 'NONE',  ( -2.923754682041362241, 6.562797562356882608, 0.7998128361456341429 ) ) ;
#208479 = CARTESIAN_POINT ( 'NONE',  ( 1.622747808203903963, -1.734053015003593101, 0.6191010992530541213 ) ) ;
#208480 = VERTEX_POINT ( 'NONE', #161760 ) ;
#208481 = CARTESIAN_POINT ( 'NONE',  ( 10.87086078464171202, 9.638125288626520515, -5.094357749550133541 ) ) ;
#208482 = CARTESIAN_POINT ( 'NONE',  ( 2.654661980655496301, 2.105093816413053709, 0.2552270188876659129 ) ) ;
#208483 = CARTESIAN_POINT ( 'NONE',  ( -0.7499999999999972244, 4.389583334016150751, -1.299038105676652899 ) ) ;
#208484 = CARTESIAN_POINT ( 'NONE',  ( 8.274553823041976841, 8.548067636504127265, 1.040834085586084257E-14 ) ) ;
#208485 = CARTESIAN_POINT ( 'NONE',  ( 6.502017186205484300, 9.743381262951846367, -1.199719254218452047 ) ) ;
#208486 = CARTESIAN_POINT ( 'NONE',  ( 2.688805810584052658, -0.3489404079633807165, -2.030846992095108217 ) ) ;
#208488 = CARTESIAN_POINT ( 'NONE',  ( 1.259045258496578557, 1.813921241667546758, -0.3151448728593714277 ) ) ;
#208487 = CARTESIAN_POINT ( 'NONE',  ( -8.850775351622791831, 9.220326086515070685, -0.7998128361456291469 ) ) ;
#208489 = CARTESIAN_POINT ( 'NONE',  ( 0.6823417656249899377, 4.676041667008086655, -1.181850606188754593 ) ) ;
#208490 = DIRECTION ( 'NONE',  ( 0.000000000000000000, 0.000000000000000000, 1.000000000000000000 ) ) ;
#208491 = CARTESIAN_POINT ( 'NONE',  ( 1.286813488861813459, 4.047007041464545374, -0.4595522011843575783 ) ) ;
#208492 = CARTESIAN_POINT ( 'NONE',  ( -11.94105721237523099, 10.90000000000000036, 1.187919463087248273 ) ) ;
#208493 = CARTESIAN_POINT ( 'NONE',  ( 1.383733252933561086, 2.037972573443189717, -0.8472329510355591786 ) ) ;
#208494 = CARTESIAN_POINT ( 'NONE',  ( 2.882378335548450465, -1.165601267607863978, 1.938926327226223822 ) ) ;
#208495 = CARTESIAN_POINT ( 'NONE',  ( -7.537970219518066450, 11.73812298950569044, -0.7216878364870267237 ) ) ;
#208496 = CARTESIAN_POINT ( 'NONE',  ( 2.794932832814459811, -0.1373201097526421111, -1.806460840857474937 ) ) ;
#208497 = EDGE_CURVE ( 'NONE', #153422, #103797, #98886, .T. ) ;
#208498 = CARTESIAN_POINT ( 'NONE',  ( 3.432743858578292784, -1.563009043653120322, 1.107381117132580250 ) ) ;
#208499 = CARTESIAN_POINT ( 'NONE',  ( 4.545415791725802457, 1.850806902094417783, -0.9279678557222792445 ) ) ;
#208500 = CARTESIAN_POINT ( 'NONE',  ( 1.364683531249988535, 2.426041667008088432, 0.7879004041258500513 ) ) ;
#208501 = CARTESIAN_POINT ( 'NONE',  ( 2.219545571343143120, -1.912749475042923475, 0.4771270530836198565 ) ) ;
#208502 = CARTESIAN_POINT ( 'NONE',  ( 0.1824732010112985747, -1.867734037610004449, -0.4713708115406111676 ) ) ;
#208503 = CARTESIAN_POINT ( 'NONE',  ( 2.869827659178546764, 0.9992216309704025079, 1.581230272166146644 ) ) ;
#208505 = CARTESIAN_POINT ( 'NONE',  ( 4.601164721245145195, 8.482418317249249995, 0.1585857521721554253 ) ) ;
#208504 = CARTESIAN_POINT ( 'NONE',  ( 1.823324434984688214, 2.154351390505971686, 0.8276274939288345012 ) ) ;
#208506 = CARTESIAN_POINT ( 'NONE',  ( 4.105780043149899861, 0.6285678624660723246, -1.751810336424673542 ) ) ;
#208507 = CARTESIAN_POINT ( 'NONE',  ( 0.6823417656249899377, 3.676041667008085767, -1.181850606188754593 ) ) ;
#208508 = CIRCLE ( 'NONE', #184241, 3.000000000000010214 ) ;
#208510 = CARTESIAN_POINT ( 'NONE',  ( -5.057354993097396445, 5.859001232490445688, -1.199719254218446718 ) ) ;
#208509 = AXIS2_PLACEMENT_3D ( 'NONE', #196788, #113480, #101414 ) ;
#208511 = CARTESIAN_POINT ( 'NONE',  ( 6.962275575817444384, 8.081408578997208991, -1.199719254218446718 ) ) ;
#208512 = CARTESIAN_POINT ( 'NONE',  ( -1.297698954646265834, 3.601166593375767278, 0.4386024987755252624 ) ) ;
#208513 = CARTESIAN_POINT ( 'NONE',  ( 0.9265589629697315033, 1.253077620556674932, -1.692570004448453957 ) ) ;
#208514 = CARTESIAN_POINT ( 'NONE',  ( -1.364683531250010295, 4.592708333674755394, 0.7879004041258379498 ) ) ;
#208515 = CARTESIAN_POINT ( 'NONE',  ( 5.975883356200851537, 1.282301362320131588, 1.740048508431484953 ) ) ;
#208516 = CARTESIAN_POINT ( 'NONE',  ( 0.0002682147194760230472, -0.9481790448457677600, 1.783359508359374512 ) ) ;
#208517 = CARTESIAN_POINT ( 'NONE',  ( 1.364683531249988757, -0.8656249996585805295, 0.000000000000000000 ) ) ;
#208518 = CARTESIAN_POINT ( 'NONE',  ( -3.958617665510272943, 6.601842462195195438, -1.082531754730549967 ) ) ;
#208519 = EDGE_CURVE ( 'NONE', #213687, #109299, #14549, .T. ) ;
#208522 = CARTESIAN_POINT ( 'NONE',  ( 3.036663219780971978, 6.486598156479028709, -0.7216878364870267237 ) ) ;
#208521 = CARTESIAN_POINT ( 'NONE',  ( 6.925078400183582339, 2.988348447159621113, 2.209593971251204714 ) ) ;
#208520 = CARTESIAN_POINT ( 'NONE',  ( 5.027041095616958444, 9.086908054853605421, 0.000000000000000000 ) ) ;
#208523 = CARTESIAN_POINT ( 'NONE',  ( -4.950662367645459305, 5.804802846121667415, -1.199719254218453823 ) ) ;
#208524 = CARTESIAN_POINT ( 'NONE',  ( 4.399625206644591557, -1.976670321813909892, 0.3981083777728141038 ) ) ;
#208526 = CARTESIAN_POINT ( 'NONE',  ( -5.587368702163209910, 9.532697562583475559, 0.000000000000000000 ) ) ;
#208525 = CARTESIAN_POINT ( 'NONE',  ( -9.707274797704657843, 11.38787068781932987, 1.082531754730558626 ) ) ;
#208527 = FACE_OUTER_BOUND ( 'NONE', #165079, .T. ) ;
#208529 = CARTESIAN_POINT ( 'NONE',  ( -1.364683531250014514, 10.08854166700806410, -0.7879004041258335089 ) ) ;
#208528 = CARTESIAN_POINT ( 'NONE',  ( 5.735289742212391850, -1.956171686333206816, 0.9202595734885756773 ) ) ;
#208530 = CARTESIAN_POINT ( 'NONE',  ( -9.592557376868645846, 11.15007068022363157, -1.199719254218441611 ) ) ;
#208532 = CARTESIAN_POINT ( 'NONE',  ( 6.116814581292481456, 0.2004514801264325186, 2.006445662566976651 ) ) ;
#208531 = CARTESIAN_POINT ( 'NONE',  ( -5.870317324592812191, 7.871789516823500144, -1.443375672974051449 ) ) ;
#208533 = CARTESIAN_POINT ( 'NONE',  ( -1.364683531250012516, 0.5927083336747520637, 0.7879004041258379498 ) ) ;
#208534 = CARTESIAN_POINT ( 'NONE',  ( 0.3617173305617603640, -5.199791778942882026, 10.99431798667029803 ) ) ;
#208535 = CARTESIAN_POINT ( 'NONE',  ( 1.436838838544731267, 7.449283400311756509, 4.203727439823562229 ) ) ;
#208536 = CARTESIAN_POINT ( 'NONE',  ( 1.277515311556869593, 1.024738337535425758, 1.387312573235904845 ) ) ;
#208537 = CARTESIAN_POINT ( 'NONE',  ( 5.671053392266061977, 9.838255734277600695, 0.7998128361456331437 ) ) ;
#208538 = CARTESIAN_POINT ( 'NONE',  ( 4.854701522145073334, 7.821512988214679218, -1.199719254218450271 ) ) ;
#208539 = CARTESIAN_POINT ( 'NONE',  ( -1.364683531250014514, -0.4489583329919089039, -0.7879004041258359514 ) ) ;
#208540 = CARTESIAN_POINT ( 'NONE',  ( 0.6140562859980386312, 1.226574898224697119, -1.275979240986246710 ) ) ;
#208541 = B_SPLINE_CURVE_WITH_KNOTS ( 'NONE', 3,
 ( #169977, #38922, #204589, #151622, #101790, #185151, #85532, #3188 ),
 .UNSPECIFIED., .F., .F.,
 ( 4, 2, 2, 4 ),
 ( 2.602085213965248775E-18, 0.0002461874215021552068, 0.0004923748430043078115, 0.0009847496860086130208 ),
 .UNSPECIFIED. ) ;
#208542 = CARTESIAN_POINT ( 'NONE',  ( 1.910792991191323065, -0.5388759818002909485, -1.939549710442307839 ) ) ;
#208543 = CARTESIAN_POINT ( 'NONE',  ( 3.909358855915114006, 1.891329263188616938, 1.136761501516952766 ) ) ;
#208544 = CARTESIAN_POINT ( 'NONE',  ( 5.260662464746663325, -0.7247129924745611129, -2.046699161452083526 ) ) ;
#208545 = EDGE_LOOP ( 'NONE', ( #28964, #171022 ) ) ;
#208546 = CARTESIAN_POINT ( 'NONE',  ( -1.402160292154681736E-14, -0.2874999999999741096, 1.732050807568877637 ) ) ;
#208547 = CARTESIAN_POINT ( 'NONE',  ( 7.904040366642689719, 10.24446639921506552, 1.443375672974076540 ) ) ;
#208549 = CARTESIAN_POINT ( 'NONE',  ( 3.093375225471244772, -0.3905761854139707667, 1.978056131710544063 ) ) ;
#208548 = CARTESIAN_POINT ( 'NONE',  ( 3.229257539231108698, 1.917844101178723504, 0.9048822562475050679 ) ) ;
#208551 = EDGE_LOOP ( 'NONE', ( #25996, #155865, #79879, #108574, #74059, #7740, #41357, #58205 ) ) ;
#208550 = CARTESIAN_POINT ( 'NONE',  ( 3.832113882524991411, -0.9361971883012323303, -1.550792431135393334 ) ) ;
#208552 = CARTESIAN_POINT ( 'NONE',  ( 6.119526231721748033, 8.232809585132461194, 1.599625672291269396 ) ) ;
#208553 = ORIENTED_EDGE ( 'NONE', *, *, #118098, .F. ) ;
#208554 = CARTESIAN_POINT ( 'NONE',  ( -9.579665964935227151, -7.246166700194470067, 0.000000000000000000 ) ) ;
#208555 = CARTESIAN_POINT ( 'NONE',  ( 6.322862864304120478, 1.705426906915354035, 0.6521430802832667295 ) ) ;
#208557 = CARTESIAN_POINT ( 'NONE',  ( 1.815515222670351259, -1.254507992466627808, -1.447865379607627512 ) ) ;
#208556 = DIRECTION ( 'NONE',  ( 0.000000000000000000, 1.000000000000000000, 1.496258514059622730E-16 ) ) ;
#208558 = CARTESIAN_POINT ( 'NONE',  ( 1.230728480726486884, 3.226239941806479106, 0.7750000000000152323 ) ) ;
#208559 = EDGE_CURVE ( 'NONE', #77381, #152468, #197909, .T. ) ;
#208560 = CARTESIAN_POINT ( 'NONE',  ( 1.364683531249988757, 2.196875000341415252, 1.214306433183764966E-14 ) ) ;
#208561 = LINE ( 'NONE', #25558, #101898 ) ;
#208562 = CARTESIAN_POINT ( 'NONE',  ( 5.436455051933180016, 2.129025116502227810, 0.3735886874452337691 ) ) ;
#208563 = EDGE_CURVE ( 'NONE', #144257, #132208, #267, .T. ) ;
#208564 = CARTESIAN_POINT ( 'NONE',  ( -5.207740401424942434, 6.208690235484773723, 1.082531754730549078 ) ) ;
#208565 = CARTESIAN_POINT ( 'NONE',  ( -7.761116589180078407, 8.019333873657032541, 0.000000000000000000 ) ) ;
#208566 = CARTESIAN_POINT ( 'NONE',  ( 3.129257641292593650, 1.918792544363761454, 0.9031103230835100248 ) ) ;
#208568 = CARTESIAN_POINT ( 'NONE',  ( -12.36958382383909871, 9.653479897959526213, -1.396270995789667513 ) ) ;
#208567 = CARTESIAN_POINT ( 'NONE',  ( -4.842962054798890748, 4.879744820279569240, 0.4763033239258877560 ) ) ;
#208569 = CARTESIAN_POINT ( 'NONE',  ( 4.622318808457460015, 1.215050846432633946, -1.552280729921464708 ) ) ;
#208570 =( BOUNDED_CURVE ( )  B_SPLINE_CURVE ( 2, ( #202489, #105040, #4284, #134359, #70355 ),
 .UNSPECIFIED., .F., .T. ) 
 B_SPLINE_CURVE_WITH_KNOTS ( ( 3, 2, 3 ),
 ( 0.02164518822461731357, 0.02500000000000000139, 0.02792328123870144521 ),
 .UNSPECIFIED. ) 
 CURVE ( )  GEOMETRIC_REPRESENTATION_ITEM ( )  RATIONAL_B_SPLINE_CURVE ( ( 0.9355558506697161381, 0.9460648536416673693, 1.000000000000000000, 0.9530025491704537943, 0.9389779222473411124 ) ) 
 REPRESENTATION_ITEM ( '' )  );
#208571 = CARTESIAN_POINT ( 'NONE',  ( 6.328373294368253354, -0.9077179077918960948, -1.683272687665722467 ) ) ;
#208572 = ORIENTED_EDGE ( 'NONE', *, *, #176386, .T. ) ;
#208573 = CARTESIAN_POINT ( 'NONE',  ( 5.946512563314596100, -1.495626773323457170, 1.498989405617740189 ) ) ;
#208574 = FACE_OUTER_BOUND ( 'NONE', #164871, .T. ) ;
#208575 = CARTESIAN_POINT ( 'NONE',  ( 1.188034388246852480, -1.312013912954514971, -1.601590607232979524 ) ) ;
#208576 = CARTESIAN_POINT ( 'NONE',  ( 2.431497994139957264, 0.9153433635570235039, -1.712687122320022626 ) ) ;
#208577 = ORIENTED_EDGE ( 'NONE', *, *, #29742, .T. ) ;
#208578 = CARTESIAN_POINT ( 'NONE',  ( 6.527324610336440180, 6.579909898339485252, 0.7998128361456331437 ) ) ;
#208579 = CARTESIAN_POINT ( 'NONE',  ( 6.713222337422018349, 7.861122810861019161, -1.199719254218452047 ) ) ;
#208581 = CARTESIAN_POINT ( 'NONE',  ( 7.156006149914539982, 7.243095351188763686, 1.040834085586084257E-14 ) ) ;
#208580 = CARTESIAN_POINT ( 'NONE',  ( 3.451197694293614671, 0.5077425806990677470, -2.027912974856157291 ) ) ;
#208582 = CARTESIAN_POINT ( 'NONE',  ( 8.011942431032855083, 8.311964022485323511, 0.7998128361456291469 ) ) ;
#208584 = ORIENTED_EDGE ( 'NONE', *, *, #200627, .T. ) ;
#208583 = CARTESIAN_POINT ( 'NONE',  ( 0.5569035977302905227, -1.554463864252687122, 0.9298500530290281230 ) ) ;
#208585 = CARTESIAN_POINT ( 'NONE',  ( 5.092482806099829062, -2.189899077852827780, -0.2726905915074183673 ) ) ;
#208586 = CARTESIAN_POINT ( 'NONE',  ( -0.07917133907641019097, -6.459673408256690230, -11.00057242252814760 ) ) ;
#208587 = CARTESIAN_POINT ( 'NONE',  ( 2.731697238759897672, -2.059418846490802313, 0.7933392487004320426 ) ) ;
#208588 = CARTESIAN_POINT ( 'NONE',  ( 6.760712154708803823, 11.03924794713562818, 1.040834085586084257E-14 ) ) ;
#208590 =( BOUNDED_SURFACE ( )  B_SPLINE_SURFACE ( 3, 2, ( 
 ( #38342, #170466, #57793 ),
 ( #26348, #5803, #7957 ),
 ( #122897, #125016, #91386 ),
 ( #24201, #106597, #137989 ) ),
 .UNSPECIFIED., .F., .F., .T. ) 
 B_SPLINE_SURFACE_WITH_KNOTS ( ( 4, 4 ),
 ( 3, 3 ),
 ( 0.000000000000000000, 3.124373798653399658E-05 ),
 ( 0.000000000000000000, 1.000000000000000000 ),
 .UNSPECIFIED. ) 
 GEOMETRIC_REPRESENTATION_ITEM ( )  RATIONAL_B_SPLINE_SURFACE ( (
 ( 1.000000000000000000, 0.7071067811870779263, 1.000000000000000000),
 ( 1.000000000000000000, 0.7053575014263694376, 1.000000000000000000),
 ( 1.000000000000000000, 0.7044883013754974499, 1.000000000000000000),
 ( 1.000000000000000000, 0.7045118851642885316, 1.000000000000000000) ) ) 
 REPRESENTATION_ITEM ( '' )  SURFACE ( )  );
#208589 = CARTESIAN_POINT ( 'NONE',  ( 0.000000000000000000, 4.000000000000003553, -11.99999999999999112 ) ) ;
#208591 = CARTESIAN_POINT ( 'NONE',  ( 2.068876254944008508, -1.477226179422253871, 1.214308343151893510 ) ) ;
#208592 = CIRCLE ( 'NONE', #97941, 10.99999999999999112 ) ;
#208593 = CARTESIAN_POINT ( 'NONE',  ( 9.745613490124728884, 10.26430391476735338, 0.7998128361456462443 ) ) ;
#208594 = CARTESIAN_POINT ( 'NONE',  ( 4.791501694037465953, -1.894250426384594066, 0.8359921707915064504 ) ) ;
#208596 = CARTESIAN_POINT ( 'NONE',  ( 3.045950098598048328, 0.7793912989166664751, -2.016482303682599841 ) ) ;
#208595 = CARTESIAN_POINT ( 'NONE',  ( 1.500511526392835693, 8.643217832945683909, -2.569261818345971893 ) ) ;
#208597 = CARTESIAN_POINT ( 'NONE',  ( 5.091441847573507928, -0.7891374179831472935, 2.044738775321436997 ) ) ;
#208598 = EDGE_LOOP ( 'NONE', ( #124365, #161905, #189157 ) ) ;
#208599 = CARTESIAN_POINT ( 'NONE',  ( 11.48243876534946217, 12.21999999999998288, 3.199999999999997957 ) ) ;
#208600 = B_SPLINE_CURVE_WITH_KNOTS ( 'NONE', 3,
 ( #1627, #67686, #133832, #52538, #69825, #51485 ),
 .UNSPECIFIED., .F., .F.,
 ( 4, 2, 4 ),
 ( 0.001525776914076238918, 0.001915068532333861259, 0.002304360150591483816 ),
 .UNSPECIFIED. ) ;
#208601 = CARTESIAN_POINT ( 'NONE',  ( 0.4465194593917913846, 3.080450244942120719, -0.4155024747329958412 ) ) ;
#208602 = CARTESIAN_POINT ( 'NONE',  ( -0.2652791711382684881, 7.171141847836421057, 2.094821536884128310 ) ) ;
#208603 = CARTESIAN_POINT ( 'NONE',  ( 4.248501033035879004, 6.049946853332221153, -1.599625672291273171 ) ) ;
#208604 = CARTESIAN_POINT ( 'NONE',  ( -1.364683531250010295, 15.19270833367472839, 0.7879004041258445001 ) ) ;
#208605 = CARTESIAN_POINT ( 'NONE',  ( -2.830620210203090181, 6.524417021870718258, 0.000000000000000000 ) ) ;
#208606 = CARTESIAN_POINT ( 'NONE',  ( -8.758204044748012507, 11.24099069033793974, 1.443375672974064550 ) ) ;
#208607 = CARTESIAN_POINT ( 'NONE',  ( 3.874598038455354665, 7.742391154831717692, -0.7998128361456362523 ) ) ;
#208608 = CARTESIAN_POINT ( 'NONE',  ( 5.612195314557796522, 2.068136773602911038, -0.09592777784667855245 ) ) ;
#208609 = CARTESIAN_POINT ( 'NONE',  ( 3.879452639046445661, 1.813680402594812557, -0.6499425845708036720 ) ) ;
#208610 = CARTESIAN_POINT ( 'NONE',  ( 0.01720424586787797083, -1.842442205116225695, 0.8197940039925479816 ) ) ;
#208611 = CARTESIAN_POINT ( 'NONE',  ( -9.541187415715041809, 12.15447128979948310, -1.599625672291263179 ) ) ;
#208612 = CARTESIAN_POINT ( 'NONE',  ( 3.811813743736467419, 7.598866467667865443, 1.040834085586084257E-14 ) ) ;
#208613 = LINE ( 'NONE', #74376, #56372 ) ;
#208614 = CARTESIAN_POINT ( 'NONE',  ( 4.891434682365626507, -1.802310843600445800, 0.7943598514809721012 ) ) ;
#208615 = CARTESIAN_POINT ( 'NONE',  ( 0.1995291103054769866, -0.5802879427523646161, 2.113158525371459096 ) ) ;
#208616 = CARTESIAN_POINT ( 'NONE',  ( 4.178209475066913647, -1.049361115903378883, 1.493786327181771068 ) ) ;
#208617 = CARTESIAN_POINT ( 'NONE',  ( 5.885648082108177803, 9.880690172519326353, 0.7216878364870317197 ) ) ;
#208618 = CARTESIAN_POINT ( 'NONE',  ( 3.023105065722954787, 5.510411095776657220, 1.082531754730546636 ) ) ;
#208619 = CARTESIAN_POINT ( 'NONE',  ( -5.433785704026946384, 9.561443431331920095, 0.000000000000000000 ) ) ;
#208620 = CARTESIAN_POINT ( 'NONE',  ( 3.705121118284530279, 7.544668081299086282, -1.734723475976807094E-15 ) ) ;
#208621 = EDGE_LOOP ( 'NONE', ( #171556, #123568, #15707, #146147 ) ) ;
#208623 = CARTESIAN_POINT ( 'NONE',  ( 6.258070432960613161, 0.7665029349510013024, -1.861766797742714585 ) ) ;
#208622 = CARTESIAN_POINT ( 'NONE',  ( 3.069684041021227827, -1.094477399149307306, 1.480508570315848482 ) ) ;
#208624 = CARTESIAN_POINT ( 'NONE',  ( 1.406082690172899108, 0.4493768194517386849, 2.253890741632145200 ) ) ;
#208625 = CARTESIAN_POINT ( 'NONE',  ( 5.489096970993415425, 0.1405823987245969631, 1.956747174436481274 ) ) ;
#208626 = CARTESIAN_POINT ( 'NONE',  ( -4.367698041896780126, 8.247398148854895084, 0.7998128361456481317 ) ) ;
#208627 = CARTESIAN_POINT ( 'NONE',  ( 0.4170821662628897974, 3.033599471985628959, -0.4170821662629418114 ) ) ;
#208628 = EDGE_CURVE ( 'NONE', #88097, #188712, #158964, .T. ) ;
#208629 = CARTESIAN_POINT ( 'NONE',  ( -4.620631424159025613, 4.285158171140619032, -0.7998128361456221525 ) ) ;
#208630 = CARTESIAN_POINT ( 'NONE',  ( 0.4673438449808891004, 1.800595422158430825, 1.021790579661909781 ) ) ;
#208631 = CARTESIAN_POINT ( 'NONE',  ( -5.808742468812186033, 5.741564066561132940, 0.000000000000000000 ) ) ;
#208633 = CARTESIAN_POINT ( 'NONE',  ( 6.526229032160782317, 1.014938005144504274, -1.449696215517197961 ) ) ;
#208632 = CARTESIAN_POINT ( 'NONE',  ( 1.716468666696397971, 1.951974251796151583, 0.7495149520271927601 ) ) ;
#208634 = CARTESIAN_POINT ( 'NONE',  ( -0.7500000000000215383, 2.941666666666689522, 1.299038105676671107 ) ) ;
#208635 = ORIENTED_EDGE ( 'NONE', *, *, #32909, .F. ) ;
#208636 = CARTESIAN_POINT ( 'NONE',  ( 1.364683531249988535, 3.426041667008085323, 0.7879004041258499402 ) ) ;
#208637 = CARTESIAN_POINT ( 'NONE',  ( 1.891783327304029205, -0.4647161096258972668, -1.677148923195219243 ) ) ;
#208638 = CIRCLE ( 'NONE', #77074, 0.1599999999999999756 ) ;
#208639 = CARTESIAN_POINT ( 'NONE',  ( 4.150767584078112193, 7.994312614733129152, 0.7998128361456321445 ) ) ;
#208641 = CYLINDRICAL_SURFACE ( 'NONE', #120458, 0.09999999999999999167 ) ;
#208640 = FILL_AREA_STYLE_COLOUR ( '', #200258 ) ;
#208642 = CARTESIAN_POINT ( 'NONE',  ( 2.279564191164831666, 1.060311948399524695, 1.360390198354200386 ) ) ;
#208643 = CARTESIAN_POINT ( 'NONE',  ( 2.947022816757136621, -1.793111998972513277, -1.259777465452505796 ) ) ;
#208644 = CARTESIAN_POINT ( 'NONE',  ( 5.549527019956425278, -1.737703232767298545, -1.360318885177333570 ) ) ;
#208645 = CARTESIAN_POINT ( 'NONE',  ( -11.05174500248992331, 4.511067306307721125, -6.216760965876352962 ) ) ;
#208646 =( BOUNDED_SURFACE ( )  B_SPLINE_SURFACE ( 3, 2, ( 
 ( #84894, #66479, #31902 ),
 ( #166145, #53462, #67546 ),
 ( #81702, #182379, #115337 ),
 ( #198625, #50272, #34009 ),
 ( #150982, #68621, #17731 ),
 ( #133690, #199694, #183457 ),
 ( #35063, #101134, #36133 ),
 ( #167222, #147784, #131572 ),
 ( #200753, #52402, #168284 ),
 ( #152041, #19882, #85966 ) ),
 .UNSPECIFIED., .F., .F., .T. ) 
 B_SPLINE_SURFACE_WITH_KNOTS ( ( 4, 2, 2, 2, 4 ),
 ( 3, 3 ),
 ( 0.000000000000000000, 0.0003762414628101696688, 0.0007524829256203393376, 0.001128724388430508898, 0.001504965851240678675 ),
 ( 0.000000000000000000, 1.000000000000000000 ),
 .UNSPECIFIED. ) 
 GEOMETRIC_REPRESENTATION_ITEM ( )  RATIONAL_B_SPLINE_SURFACE ( (
 ( 1.000000000000000000, 0.7796368470575135712, 1.000000000000000000),
 ( 1.000000000000000000, 0.7902951223000224124, 1.000000000000000000),
 ( 1.000000000000000000, 0.7826420995578321493, 1.000000000000000000),
 ( 1.000000000000000000, 0.7484677895294554739, 1.000000000000000000),
 ( 1.000000000000000000, 0.7229395345770123216, 1.000000000000000000),
 ( 1.000000000000000000, 0.7019560918380093328, 1.000000000000000000),
 ( 1.000000000000000000, 0.7093811322644433259, 1.000000000000000000),
 ( 1.000000000000000000, 0.7456665127358711453, 1.000000000000000000),
 ( 1.000000000000000000, 0.7703623356575411973, 1.000000000000000000),
 ( 1.000000000000000000, 0.7796377409682134774, 1.000000000000000000) ) ) 
 REPRESENTATION_ITEM ( '' )  SURFACE ( )  );
#208647 = CARTESIAN_POINT ( 'NONE',  ( 2.835037514343414777, -2.076374246603398532, -0.6340929010987955694 ) ) ;
#208648 = CARTESIAN_POINT ( 'NONE',  ( 0.6975366375942676500, -0.6598540886826111951, 1.702458561391326342 ) ) ;
#208649 = CARTESIAN_POINT ( 'NONE',  ( 3.134099051248913970, 2.117513410275436936, -0.004568276605129357668 ) ) ;
#208650 = CARTESIAN_POINT ( 'NONE',  ( 6.539320575229255361, 3.697401852651286180, 2.511149361313206096 ) ) ;
#208651 = ORIENTED_EDGE ( 'NONE', *, *, #189189, .T. ) ;
#208653 = CARTESIAN_POINT ( 'NONE',  ( 0.6823417656249882723, 1.238541667008083547, -1.181850606188749264 ) ) ;
#208652 = CARTESIAN_POINT ( 'NONE',  ( 4.089605575727714104, -0.8772585143675699637, 2.118060962191004037 ) ) ;
#208654 = LINE ( 'NONE', #24575, #22639 ) ;
#208655 = CARTESIAN_POINT ( 'NONE',  ( 3.704402285031850539, 5.344888637335695414, -1.599625672291262513 ) ) ;
#208656 = CARTESIAN_POINT ( 'NONE',  ( 6.428415558115947448, -1.044286553621230240, -1.960546399981792476 ) ) ;
#208657 = CARTESIAN_POINT ( 'NONE',  ( -5.409340102172518705, 9.254721185935849803, 0.000000000000000000 ) ) ;
#208658 = CARTESIAN_POINT ( 'NONE',  ( 4.555176424511575561, 4.416720038126027426, -0.7216878364870188411 ) ) ;
#208659 = CIRCLE ( 'NONE', #98006, 0.07999999999999940492 ) ;
#208660 = CARTESIAN_POINT ( 'NONE',  ( -6.846504384776774366, 7.089935991768773427, -0.7216878364870267237 ) ) ;
#208661 = CARTESIAN_POINT ( 'NONE',  ( 6.825078400183572036, 4.699117039843025090, 2.418333817060664082 ) ) ;
#208662 = ORIENTED_EDGE ( 'NONE', *, *, #152831, .F. ) ;
#208663 = CARTESIAN_POINT ( 'NONE',  ( 4.641250102003463773, 0.7743139518727223392, 1.862017545363145565 ) ) ;
#208665 = CARTESIAN_POINT ( 'NONE',  ( 2.131754086930433001, 1.975065156136386335, -0.5945119761870448771 ) ) ;
#208664 = CARTESIAN_POINT ( 'NONE',  ( 5.178324605415663306, 8.128796908705222535, 1.199719254218462483 ) ) ;
#208666 = CARTESIAN_POINT ( 'NONE',  ( 7.343676480457483002, 8.596652644402405841, -1.199719254218452047 ) ) ;
#208667 = CARTESIAN_POINT ( 'NONE',  ( 4.760321331729593375, 5.686701320840210627, -1.082531754730548412 ) ) ;
#208668 = CARTESIAN_POINT ( 'NONE',  ( 3.285556943750000070, -2.734374999522042771, 0.000000000000000000 ) ) ;
#208669 = CARTESIAN_POINT ( 'NONE',  ( -1.364683531250010295, 4.780208333674755394, 0.7879004041258379498 ) ) ;
#208670 = CARTESIAN_POINT ( 'NONE',  ( 5.613277516225614328, -2.138688192980051639, 0.4772630486022874652 ) ) ;
#208671 = CARTESIAN_POINT ( 'NONE',  ( 3.727185537919291747, 2.006959858346604619, 0.1948421285040344286 ) ) ;
#208672 = CARTESIAN_POINT ( 'NONE',  ( 2.032514702046281485, -1.644074058028240692, 0.8291662819630771786 ) ) ;
#208673 = CARTESIAN_POINT ( 'NONE',  ( 7.630541526392844887, 7.796719957080126662, 0.7998128361456341429 ) ) ;
#208674 =( NAMED_UNIT ( * ) SI_UNIT ( $, .STERADIAN. ) SOLID_ANGLE_UNIT ( ) );
#208675 = CARTESIAN_POINT ( 'NONE',  ( 0.08252656676070461994, -0.1270158569062987686, -1.696106202995291357 ) ) ;
#208676 = AXIS2_PLACEMENT_3D ( 'NONE', #80063, #30259, #176506 ) ;
#208677 = CARTESIAN_POINT ( 'NONE',  ( -8.037286134802835491, 8.271255333558444889, -0.7998128361456291469 ) ) ;
#208679 = CARTESIAN_POINT ( 'NONE',  ( -4.308458954092677651, 8.248562223075252220, -0.7998128361456362523 ) ) ;
#208678 = CARTESIAN_POINT ( 'NONE',  ( 5.717715967963762580, -2.208827357630326560, 0.4893477075747532101 ) ) ;
#208680 = CARTESIAN_POINT ( 'NONE',  ( 2.438226732591573409, 0.9919046538873840246, -1.857854779501419307 ) ) ;
#208681 = CARTESIAN_POINT ( 'NONE',  ( -5.855142236255304944, 7.924361590421551860, -1.599625672291271394 ) ) ;
#208682 = CARTESIAN_POINT ( 'NONE',  ( 7.781490099239519509, 11.16582331816642260, 1.199719254218460707 ) ) ;
#208683 = CARTESIAN_POINT ( 'NONE',  ( 7.824464048418096951, 8.301165276008827476, -0.7216878364870317197 ) ) ;
#208684 = CARTESIAN_POINT ( 'NONE',  ( -6.958359152311683893, 9.141171649162195934, -1.599625672291263179 ) ) ;
#208685 = B_SPLINE_CURVE_WITH_KNOTS ( 'NONE', 3,
 ( #98236, #164291, #15879, #148049, #65685, #131832, #99299, #16942, #83021, #66743 ),
 .UNSPECIFIED., .F., .F.,
 ( 4, 2, 2, 2, 4 ),
 ( 0.000000000000000000, 0.0002334048330869045729, 0.0004668096661738091457, 0.0007002144992607138270, 0.0009336193323476185083 ),
 .UNSPECIFIED. ) ;
#208686 = CARTESIAN_POINT ( 'NONE',  ( -1.115562610750309283E-14, 9.593750000682799595, 1.500000000000001554 ) ) ;
#208687 = CARTESIAN_POINT ( 'NONE',  ( 6.548225005276093746, 9.623051025255367819, -1.082531754730537976 ) ) ;
#208688 = CARTESIAN_POINT ( 'NONE',  ( 4.100400566228236343, 7.694619998084524681, 0.6794913885044724378 ) ) ;
#208689 = CIRCLE ( 'NONE', #149812, 0.08000000000000037637 ) ;
#208690 = CARTESIAN_POINT ( 'NONE',  ( -8.676855123066012254, 12.10645282934361866, -1.082531754730543971 ) ) ;
#208692 = CARTESIAN_POINT ( 'NONE',  ( 2.883289241188752072, -2.054055030226094480, -0.8463503915563088675 ) ) ;
#208691 = CARTESIAN_POINT ( 'NONE',  ( 1.564851893998190135, 0.6701894319398638000, 2.011955567234039677 ) ) ;
#208693 = CARTESIAN_POINT ( 'NONE',  ( 0.04788047853313340263, -1.708876078042343316, -1.396090968258607790 ) ) ;
#208694 = CARTESIAN_POINT ( 'NONE',  ( -4.423703259808839938, 8.383013913077441259, 0.7998128361456352531 ) ) ;
#208695 = CARTESIAN_POINT ( 'NONE',  ( 4.462605117192430804, 8.358123070033169455, 1.040834085586084257E-14 ) ) ;
#208696 = CARTESIAN_POINT ( 'NONE',  ( 4.123457186961496213, 0.2424046295769199388, -1.946780420294342617 ) ) ;
#208697 = CARTESIAN_POINT ( 'NONE',  ( 9.887974103068218668, 10.43039129653476493, 0.7998128361456462443 ) ) ;
#208698 = CARTESIAN_POINT ( 'NONE',  ( -4.552667031389123764, 6.999162803142576550, 1.172958579310765970 ) ) ;
#208699 = CARTESIAN_POINT ( 'NONE',  ( 2.184835310096557404, 5.700724961754617404, 1.040834085586084257E-14 ) ) ;
#208700 = CARTESIAN_POINT ( 'NONE',  ( 1.364683531249988757, 1.134375000341421247, 0.000000000000000000 ) ) ;
#208701 = CARTESIAN_POINT ( 'NONE',  ( -5.980555157403903976, 6.149938236492225485, 0.000000000000000000 ) ) ;
#208703 = ORIENTED_EDGE ( 'NONE', *, *, #106933, .F. ) ;
#208702 = CARTESIAN_POINT ( 'NONE',  ( -5.043269954603569083, 7.867270132804026872, 1.082531754730560403 ) ) ;
#208704 = CARTESIAN_POINT ( 'NONE',  ( 3.146849984228027974, 2.069795010335002239, 0.4607391970517027979 ) ) ;
#208705 = CARTESIAN_POINT ( 'NONE',  ( -4.450819567036169211, 8.414649604842665553, -0.7998128361456362523 ) ) ;
#208706 = CARTESIAN_POINT ( 'NONE',  ( 4.083022661009271914, -0.2092679848491978134, -2.151539631373246220 ) ) ;
#208707 = CARTESIAN_POINT ( 'NONE',  ( 3.526749072549471453, -1.699942963128863838, 0.7078653300200201670 ) ) ;
#208708 = CARTESIAN_POINT ( 'NONE',  ( -4.344470927813957495, 7.211826089590096522, 1.015455228366731966 ) ) ;
#208709 = CARTESIAN_POINT ( 'NONE',  ( 1.364683531249986537, 0.6760416670080884316, 0.7879004041258500513 ) ) ;
#208710 = CARTESIAN_POINT ( 'NONE',  ( 5.683501733545419654, -0.7767583057271000291, 1.557453612149447775 ) ) ;
#208712 = EDGE_CURVE ( 'NONE', #62106, #14287, #29911, .T. ) ;
#208711 = CARTESIAN_POINT ( 'NONE',  ( 6.727182134110202050, 0.5964276595885747989, 1.864301751488647962 ) ) ;
#208713 = CARTESIAN_POINT ( 'NONE',  ( 4.528060117284244512, 4.385084346360807572, 0.7216878364870317197 ) ) ;
#208714 = CARTESIAN_POINT ( 'NONE',  ( 4.663288057535367237, 8.288536188413402783, 0.5084364831346009916 ) ) ;
#208715 = CARTESIAN_POINT ( 'NONE',  ( 3.045950098598048328, 0.7793912989166664751, -2.016482303682599841 ) ) ;
#208716 = EDGE_CURVE ( 'NONE', #16492, #206986, #33917, .T. ) ;
#208717 = CARTESIAN_POINT ( 'NONE',  ( 5.641953822799152363, -0.04667112846407085042, -2.015725140939367943 ) ) ;
#208718 = CARTESIAN_POINT ( 'NONE',  ( -8.798878505144658746, 10.32807501316600884, -1.082531754730543083 ) ) ;
#208719 = CARTESIAN_POINT ( 'NONE',  ( 2.940462584922590938, 2.145230175562794717, 0.2658940370997217584 ) ) ;
#208720 = CARTESIAN_POINT ( 'NONE',  ( 4.130118527232538028, 1.057347662480428108, -1.663647784685320818 ) ) ;
#208721 = CARTESIAN_POINT ( 'NONE',  ( 0.06437606466144081552, -1.426665095847098330, 1.663708609037084951 ) ) ;
#208722 = CARTESIAN_POINT ( 'NONE',  ( 0.8510977523443744586, 0.6731378975963157041, 2.207243034677327298 ) ) ;
#208723 = CARTESIAN_POINT ( 'NONE',  ( 4.019036194231017767, -1.857530068489420705, 0.5666795103562488611 ) ) ;
#208726 = EDGE_LOOP ( 'NONE', ( #171243, #162596, #18098, #14171, #159818 ) ) ;
#208725 = DIRECTION ( 'NONE',  ( 0.000000000000000000, -1.000000000000000000, 0.000000000000000000 ) ) ;
#208724 = CARTESIAN_POINT ( 'NONE',  ( -8.473482818416670170, 10.90881592628469932, -1.443375672974058777 ) ) ;
#208727 = CARTESIAN_POINT ( 'NONE',  ( -6.038177310039794854, 8.137902509836795417, -1.599625672291271394 ) ) ;
#208728 = CARTESIAN_POINT ( 'NONE',  ( 6.890000000000050306, -0.002781820520068867264, 1.999840353888074240 ) ) ;
#208730 = ORIENTED_EDGE ( 'NONE', *, *, #108052, .F. ) ;
#208729 = CARTESIAN_POINT ( 'NONE',  ( -4.132202957115018727, 8.042930226601317401, 0.000000000000000000 ) ) ;
#208731 = CARTESIAN_POINT ( 'NONE',  ( -9.124274191872645545, 9.747334100047323702, -0.7216878364870267237 ) ) ;
#208732 = CARTESIAN_POINT ( 'NONE',  ( 1.870444250305805856, 1.134645063044220858, 1.892580404734986121 ) ) ;
#208733 = CARTESIAN_POINT ( 'NONE',  ( 3.285556943750000514, -1.013541666188710888, 1.896917185911906500 ) ) ;
#208734 = CARTESIAN_POINT ( 'NONE',  ( 6.877797714452785982, -1.903667959252927533, 0.4735691183095217527 ) ) ;
#208735 = CARTESIAN_POINT ( 'NONE',  ( -0.6823417656250212460, 5.113541667008086655, 1.181850606188767472 ) ) ;
#208736 = CARTESIAN_POINT ( 'NONE',  ( -1.201851678989727383E-14, 3.868750000682817713, -1.732050807568863648 ) ) ;
#208737 = CARTESIAN_POINT ( 'NONE',  ( 6.029390871727402512, 6.069343164222702924, -0.5281050654588164139 ) ) ;
#208739 = CARTESIAN_POINT ( 'NONE',  ( 6.720655732516647163, 0.005566325962592238996, 1.826293863978686982 ) ) ;
#208738 = DIRECTION ( 'NONE',  ( 0.000000000000000000, 1.000000000000000000, 0.000000000000000000 ) ) ;
#208740 = CARTESIAN_POINT ( 'NONE',  ( 5.894452933195246658, 1.502573388107550034, -1.063714819228026132 ) ) ;
#208741 = ORIENTED_EDGE ( 'NONE', *, *, #45569, .F. ) ;
#208742 = CARTESIAN_POINT ( 'NONE',  ( 1.360316468749964480, -0.2343749996585806072, -5.204170427930421283E-15 ) ) ;
#208743 = CARTESIAN_POINT ( 'NONE',  ( -8.206763054973658100, 8.468978407091068306, 0.7998128361456602331 ) ) ;
#208744 = FACE_OUTER_BOUND ( 'NONE', #21780, .T. ) ;
#208745 = CARTESIAN_POINT ( 'NONE',  ( 6.504144398916748671, -0.9053081408615070158, 1.915699539216948688 ) ) ;
#208746 = CARTESIAN_POINT ( 'NONE',  ( -2.335486742378066527, -0.1025264918674536757, -0.4876558207452462712 ) ) ;
#208747 = CARTESIAN_POINT ( 'NONE',  ( 4.690231075323689325, 7.559354456931247412, 1.199719254218462483 ) ) ;
#208748 = CARTESIAN_POINT ( 'NONE',  ( 0.2861016050247901510, -0.9718399577113141508, 1.817365962020002890 ) ) ;
#208749 = EDGE_CURVE ( 'NONE', #178392, #72859, #186513, .T. ) ;
#208752 = CARTESIAN_POINT ( 'NONE',  ( 5.284640796330934087, 1.621094592300664328, -0.8731043043393662550 ) ) ;
#208751 = CARTESIAN_POINT ( 'NONE',  ( 1.908444903620472477, 0.5799682436128813512, 1.768463464005122443 ) ) ;
#208750 = LINE ( 'NONE', #128676, #317 ) ;
#208753 = CARTESIAN_POINT ( 'NONE',  ( 5.798083248138522272, 9.916180889470295412, 0.7998128361456462443 ) ) ;
#208754 = CARTESIAN_POINT ( 'NONE',  ( -4.911974738770095605, 4.719687011848955116, 0.4085689905262423482 ) ) ;
#208755 = COLOUR_RGB ( '', 0.31764706, 0.68627451, 0.89019608) ;
#208756 = CARTESIAN_POINT ( 'NONE',  ( -6.038177310039794854, 8.137902509836795417, -1.599625672291271394 ) ) ;
#208758 = EDGE_LOOP ( 'NONE', ( #131005, #122194, #160923, #151074, #59293 ) ) ;
#208757 = CARTESIAN_POINT ( 'NONE',  ( -6.776587425048114177, -7.030236945366979739, -6.796206128891399523 ) ) ;
#208759 = CARTESIAN_POINT ( 'NONE',  ( 4.336686996305870068, 2.164023489887345164, 0.4319772483800735086 ) ) ;
#208760 = CARTESIAN_POINT ( 'NONE',  ( 6.098944901167723032, 1.854799121126067485, -1.295245758874500996 ) ) ;
#208761 = CARTESIAN_POINT ( 'NONE',  ( -4.907688418466881863, 8.669460888279271416, 0.7216878364870458196 ) ) ;
#208762 = CARTESIAN_POINT ( 'NONE',  ( 5.326340473083292615, -0.8217345736999382977, -1.614601580891014354 ) ) ;
#208763 = CARTESIAN_POINT ( 'NONE',  ( 6.016788071399586713, 0.1949370894720331426, 1.905806522959735627 ) ) ;
#208764 = CARTESIAN_POINT ( 'NONE',  ( -5.342823980928589123, 4.390142039796948836, -2.499999999999994671 ) ) ;
#208765 = CARTESIAN_POINT ( 'NONE',  ( 5.215449470722859360, 1.565665547294055715, 1.097690013397538022 ) ) ;
#208766 = CARTESIAN_POINT ( 'NONE',  ( 0.2154177506630133854, -1.835460468737951878, 0.3602540799089171131 ) ) ;
#208767 = CARTESIAN_POINT ( 'NONE',  ( 2.905482715143858030, -1.942096844255640109, 0.5424705965835219246 ) ) ;
#208769 = CARTESIAN_POINT ( 'NONE',  ( 3.615936863914733124, -2.074906038012876763, 0.3600020511305370707 ) ) ;
#208768 = CARTESIAN_POINT ( 'NONE',  ( -8.967828540435322182, 12.54988483289483980, 1.199719254218462483 ) ) ;
#208770 = CARTESIAN_POINT ( 'NONE',  ( 8.097244055859613709, 10.46987070330147063, -1.599625672291262513 ) ) ;
#208772 = CARTESIAN_POINT ( 'NONE',  ( -8.701635661872465732, 9.046329781806354831, 1.040834085586084257E-14 ) ) ;
#208771 = CARTESIAN_POINT ( 'NONE',  ( 1.499999999999987121, 0.004166666666691258049, 0.8660254037844524744 ) ) ;
#208773 = DIRECTION ( 'NONE',  ( 1.000000000000000000, -0.000000000000000000, -0.000000000000000000 ) ) ;
#208774 = CARTESIAN_POINT ( 'NONE',  ( 3.463153198524880239, -1.648742896667846125, 1.166392943622736267 ) ) ;
#208775 = CARTESIAN_POINT ( 'NONE',  ( 0.6823417656249899377, 3.176041667008085323, -1.181850606188754593 ) ) ;
#208776 = CARTESIAN_POINT ( 'NONE',  ( 2.333974999846879061, 5.874721266463329705, -0.7998128361456291469 ) ) ;
#208777 = ADVANCED_FACE ( 'NONE', ( #154031 ), #154997, .F. ) ;
#208778 = CARTESIAN_POINT ( 'NONE',  ( 4.411504763889100289, -0.3743020017868466387, 2.128795073437335095 ) ) ;
#208779 = CARTESIAN_POINT ( 'NONE',  ( -3.475000000000000533, -1.706249999044083587, 0.000000000000000000 ) ) ;
#208780 = CARTESIAN_POINT ( 'NONE',  ( 1.499999999999989120, 5.004166666666691299, 0.8660254037844524744 ) ) ;
#208782 = CARTESIAN_POINT ( 'NONE',  ( 9.568546172724150978, -8.233137084989836652, -0.4683205530892405877 ) ) ;
#208781 = CARTESIAN_POINT ( 'NONE',  ( 5.508355548902068577, 9.648441583686274470, 0.7998128361456331437 ) ) ;
#208783 = CARTESIAN_POINT ( 'NONE',  ( 8.893785580440313865, 9.478430720042945623, 1.040834085586084257E-14 ) ) ;
#208785 = CARTESIAN_POINT ( 'NONE',  ( 9.356044174147720938, 13.88059531916365508, -7.514793805895062739 ) ) ;
#208784 = CARTESIAN_POINT ( 'NONE',  ( 2.225261637991797325, -1.984409513266917502, -0.8813929409505830703 ) ) ;
#208787 = CARTESIAN_POINT ( 'NONE',  ( 0.4504185290156897947, -1.555054577268409899, -0.9855837367087336709 ) ) ;
#208786 = CARTESIAN_POINT ( 'NONE',  ( -5.422898255786193111, 8.310169817517122581, -1.082531754730544860 ) ) ;
#208788 = CARTESIAN_POINT ( 'NONE',  ( 0.6823417656249899377, 2.342708333674753618, 1.181850606188767472 ) ) ;
#208790 = B_SPLINE_CURVE_WITH_KNOTS ( 'NONE', 3,
 ( #189559, #201517, #70449, #136564 ),
 .UNSPECIFIED., .F., .F.,
 ( 4, 4 ),
 ( 0.000000000000000000, 0.0001618775200852311160 ),
 .UNSPECIFIED. ) ;
#208789 = CARTESIAN_POINT ( 'NONE',  ( 2.296645709751913955, 1.758124065145909798, -1.308193547052277861 ) ) ;
#208791 = CARTESIAN_POINT ( 'NONE',  ( 6.883263157960362477, 2.445608615952394871, 2.336423753955836791 ) ) ;
#208792 = CARTESIAN_POINT ( 'NONE',  ( 2.132027182898531326, -1.478040878648724465, -1.713098503734461708 ) ) ;
#208793 = CARTESIAN_POINT ( 'NONE',  ( -5.533699252672048985, 9.607732894759390518, -0.7998128361456231517 ) ) ;
#208794 = CARTESIAN_POINT ( 'NONE',  ( 0.6823417656249899377, 4.238541667008085767, -1.181850606188754593 ) ) ;
#208795 = CARTESIAN_POINT ( 'NONE',  ( 5.279289985772466665, 7.652873027719338417, 1.222721368963412214 ) ) ;
#208796 = CARTESIAN_POINT ( 'NONE',  ( -0.7500000000000179856, 12.29166666666666607, 1.299038105676658228 ) ) ;
#208797 = CARTESIAN_POINT ( 'NONE',  ( 5.221298555038576872, 9.105615724271411082, 0.000000000000000000 ) ) ;
#208798 = EDGE_CURVE ( 'NONE', #116176, #27161, #38144, .T. ) ;
#208799 = CARTESIAN_POINT ( 'NONE',  ( 4.094789254117153554, 1.496004596371943496, -0.9451293409883186891 ) ) ;
#208800 = CARTESIAN_POINT ( 'NONE',  ( 9.610031953988080744, 10.10612545594124967, -0.7998128361456281477 ) ) ;
#208801 = CARTESIAN_POINT ( 'NONE',  ( 1.096861832941862236, -0.5116358106188825250, -2.042740603722263515 ) ) ;
#208803 = CARTESIAN_POINT ( 'NONE',  ( -0.7500000000000006661, 1.108333333333356929, -1.299038105676652011 ) ) ;
#208802 = CARTESIAN_POINT ( 'NONE',  ( 0.6823417656249934904, 10.44270833367473550, 1.181850606188764807 ) ) ;
#208804 = CARTESIAN_POINT ( 'NONE',  ( -3.935609729716867289, 7.813571461303467913, 0.7998128361456352531 ) ) ;
#208805 = CARTESIAN_POINT ( 'NONE',  ( 6.573846656420020196, -0.8593871168269312522, 1.822298249534954673 ) ) ;
#208806 = ORIENTED_EDGE ( 'NONE', *, *, #95154, .T. ) ;
#208807 = CARTESIAN_POINT ( 'NONE',  ( 4.030043484472041193, 1.001115284758803625, -1.580040089582811280 ) ) ;
#208808 = CARTESIAN_POINT ( 'NONE',  ( 4.750872686184268723, -0.4484009487188305720, -2.020967519627144604 ) ) ;
#208809 = CARTESIAN_POINT ( 'NONE',  ( -7.255021596644144921, 7.636815748939187465, 0.7216878364870317197 ) ) ;
#208810 = CARTESIAN_POINT ( 'NONE',  ( -2.493461049780994365, 3.507114751586604129, 11.73081193161140590 ) ) ;
#208811 = CARTESIAN_POINT ( 'NONE',  ( 8.076906825439115423, 10.44614393447756129, -1.599625672291262513 ) ) ;
#208812 = CARTESIAN_POINT ( 'NONE',  ( -1.513761821635718485, 8.683429030108589686, 2.534756493980089509 ) ) ;
#208813 = CARTESIAN_POINT ( 'NONE',  ( 6.481679955784983349, 9.719654494127929922, -1.199719254218452047 ) ) ;
#208814 = AXIS2_PLACEMENT_3D ( 'NONE', #205856, #201573, #53219 ) ;
#208815 = CARTESIAN_POINT ( 'NONE',  ( 4.868390568588833567, 4.879779592243221664, -0.3669954890176479467 ) ) ;
#208816 = ADVANCED_FACE ( 'NONE', ( #5597 ), #203811, .T. ) ;
#208817 = CARTESIAN_POINT ( 'NONE',  ( 1.364683531249988757, -0.8656249996585805295, 0.000000000000000000 ) ) ;
#208818 = CARTESIAN_POINT ( 'NONE',  ( 3.719154087244529894, -1.729071306366702698, -0.9269775827704658244 ) ) ;
#208819 = EDGE_CURVE ( 'NONE', #156687, #158767, #166008, .T. ) ;
#208820 = CARTESIAN_POINT ( 'NONE',  ( 0.8079699768257715409, -1.730602710733687877, 1.034004433739174500 ) ) ;
#208821 = CARTESIAN_POINT ( 'NONE',  ( -4.390861645979385663, 6.216034235099629157, -1.599625672291271394 ) ) ;
#208823 = CARTESIAN_POINT ( 'NONE',  ( 6.639320575229255894, 7.053084031878349869, 2.494893166485531388 ) ) ;
#208822 = CARTESIAN_POINT ( 'NONE',  ( 7.910292558569346433, 11.31609285405122556, -1.199719254218446718 ) ) ;
#208824 = CARTESIAN_POINT ( 'NONE',  ( 1.370139650511486007, -1.190941340819328564, 1.442406204513801971 ) ) ;
#208825 = CARTESIAN_POINT ( 'NONE',  ( 1.364683531249988535, 4.113541667008088432, 0.7879004041258500513 ) ) ;
#208826 = CARTESIAN_POINT ( 'NONE',  ( 3.041273912350466624, 0.05370876457178561797, 2.012661466405294863 ) ) ;
#208828 = CARTESIAN_POINT ( 'NONE',  ( 3.111064062886280013, 0.05467929133608259024, 2.116691892344662929 ) ) ;
#208827 = CARTESIAN_POINT ( 'NONE',  ( -5.409340102172518705, 9.254721185935849803, 0.000000000000000000 ) ) ;
#208829 = CARTESIAN_POINT ( 'NONE',  ( 1.499999999999990896, 5.056250000682820378, 1.214306433183764966E-14 ) ) ;
#208830 = CARTESIAN_POINT ( 'NONE',  ( 5.336411075974297979, -1.153114810915600641, 1.719314882265559286 ) ) ;
#208831 = CARTESIAN_POINT ( 'NONE',  ( 4.947799714344386146, 4.737130853015369958, -0.7998128361456481317 ) ) ;
#208833 = CARTESIAN_POINT ( 'NONE',  ( 4.054051625686104998, 4.688480637177271149, -1.199719254218446718 ) ) ;
#208832 = CARTESIAN_POINT ( 'NONE',  ( -0.05888619351396630341, -1.618772603580875158, -1.322922665863958125 ) ) ;
#208835 = ORIENTED_EDGE ( 'NONE', *, *, #210828, .F. ) ;
#208834 = CARTESIAN_POINT ( 'NONE',  ( 4.875911338656576888, 1.051942333337583468, 1.491839654383666947 ) ) ;
#208836 = CARTESIAN_POINT ( 'NONE',  ( 8.938903350111612411, 9.323142084752035430, -0.7998128361456221525 ) ) ;
#208837 = CARTESIAN_POINT ( 'NONE',  ( 1.608462485350598881, 8.735270501766754236, -2.463594439587636131 ) ) ;
#208838 = CARTESIAN_POINT ( 'NONE',  ( 12.43309052428753070, 7.572468744233063376, 1.895192891247173606 ) ) ;
#208839 = CARTESIAN_POINT ( 'NONE',  ( 9.606148981167590861, -6.583980363595129504, -0.4355862708379804604 ) ) ;
#208840 = CARTESIAN_POINT ( 'NONE',  ( -1.364683531250014514, 12.65104166700806232, -0.7879004041258335089 ) ) ;
#208841 = CARTESIAN_POINT ( 'NONE',  ( 5.215449470722859360, 1.565665547294055715, 1.097690013397538022 ) ) ;
#208842 = CARTESIAN_POINT ( 'NONE',  ( -7.147119532698295252, 11.49005655479003174, 0.000000000000000000 ) ) ;
#208843 = CARTESIAN_POINT ( 'NONE',  ( 6.144869935491714230, 8.192100896205568361, -1.599625672291262513 ) ) ;
#208844 = CARTESIAN_POINT ( 'NONE',  ( -1.360316468750018659, 2.401041667008069425, -0.7853790794159061228 ) ) ;
#208845 = CARTESIAN_POINT ( 'NONE',  ( 5.684946482831785275, 5.526859072925533134, -0.7998128361456231517 ) ) ;
#208846 = ORIENTED_EDGE ( 'NONE', *, *, #159504, .T. ) ;
#208847 = CARTESIAN_POINT ( 'NONE',  ( -6.947627372360122955, 7.070263120700404968, 0.000000000000000000 ) ) ;
#208848 = CARTESIAN_POINT ( 'NONE',  ( -11.07123604129543182, 13.79999999999999538, 0.8055550039003244178 ) ) ;
#208850 = CARTESIAN_POINT ( 'NONE',  ( 5.318541398310776103, 9.426991741329731056, -0.7998128361456481317 ) ) ;
#208849 = CARTESIAN_POINT ( 'NONE',  ( -5.000000000000013323, 8.499999999999996447, 0.7750000000000004663 ) ) ;
#208851 = CARTESIAN_POINT ( 'NONE',  ( 3.069588487047325309E-15, 0.7598076211376200151, 10.89999999999921343 ) ) ;
#208852 = CARTESIAN_POINT ( 'NONE',  ( -6.500216601102190239, 6.758717457939978246, 0.07576745652920421903 ) ) ;
#208853 = CARTESIAN_POINT ( 'NONE',  ( -5.233084105194862445, 9.049089189461916760, 0.7216878364870458196 ) ) ;
#208854 = CARTESIAN_POINT ( 'NONE',  ( 2.835626683552519012, 6.459981564119914310, 0.000000000000000000 ) ) ;
#208855 = CARTESIAN_POINT ( 'NONE',  ( 1.832793114640043131, -1.868399652882225981, -0.6228533014895777375 ) ) ;
#208856 = CARTESIAN_POINT ( 'NONE',  ( 3.866814677988283044, -0.2004539179165897023, -2.006445418776988010 ) ) ;
#208857 = CARTESIAN_POINT ( 'NONE',  ( -6.659026002606323047, 10.92061410301605662, 0.000000000000000000 ) ) ;
#208858 = CARTESIAN_POINT ( 'NONE',  ( 5.554000203453580475, 6.508696987897830688, -1.199719254218452047 ) ) ;
#208859 = CARTESIAN_POINT ( 'NONE',  ( 6.727182134110193168, 3.677753830905213128, 2.802861976130672783 ) ) ;
#208860 = CARTESIAN_POINT ( 'NONE',  ( 3.416156609664961152, 1.390242785425911620, -1.694013327489252152 ) ) ;
#208861 = CARTESIAN_POINT ( 'NONE',  ( 9.475937867762608491, 4.398642301159960688, -7.290291149262039916 ) ) ;
#208862 = CARTESIAN_POINT ( 'NONE',  ( 1.887598533328225692, 1.326653652590740418, 1.397000115363009609 ) ) ;
#208863 = CARTESIAN_POINT ( 'NONE',  ( -9.332089804907933939, 9.781859615347734405, 1.040834085586084257E-14 ) ) ;
#208864 = CARTESIAN_POINT ( 'NONE',  ( -0.1296875068448125334, 4.095146142119266308, -2.381513845672214913 ) ) ;
#208865 = CARTESIAN_POINT ( 'NONE',  ( 0.1329588055935213564, 1.397696041676167678, -2.105440929937075989 ) ) ;
#208866 = CARTESIAN_POINT ( 'NONE',  ( 4.475600106286968582, 5.354526557823810151, -1.082531754730548412 ) ) ;
#208867 = CARTESIAN_POINT ( 'NONE',  ( 6.662942426112080874, 9.860851032851066122, 1.199719254218460707 ) ) ;
#208868 = CARTESIAN_POINT ( 'NONE',  ( 5.311043488251262268, 7.219303374425030562, -1.599625672291256295 ) ) ;
#208869 = CARTESIAN_POINT ( 'NONE',  ( -5.738979324002792204, 5.917037536912586049, -2.440165351838337049 ) ) ;
#208870 = CARTESIAN_POINT ( 'NONE',  ( 5.180624094197585627, 8.097792972322238825, -1.082531754730548412 ) ) ;
#208871 = ORIENTED_EDGE ( 'NONE', *, *, #89214, .T. ) ;
#208873 = CARTESIAN_POINT ( 'NONE',  ( 3.106110754726201240, -0.8138748988139458129, 1.841402425526596387 ) ) ;
#208872 = CARTESIAN_POINT ( 'NONE',  ( 6.233933901472759942, 1.822226914158030286, 0.2631550708301691466 ) ) ;
#208874 = CARTESIAN_POINT ( 'NONE',  ( 4.798391170199634459, -2.103835099937763964, 0.9258070857356412997 ) ) ;
#208876 = CARTESIAN_POINT ( 'NONE',  ( 1.867776877072557129, -1.847639373886921677, 0.2213648055933575276 ) ) ;
#208875 = CARTESIAN_POINT ( 'NONE',  ( -0.02880301295726198432, 1.985184585160368664, -2.687100061827327302 ) ) ;
#208877 = CARTESIAN_POINT ( 'NONE',  ( -6.328041841479842056, 6.870487382198048998, 0.6860574420480938240 ) ) ;
#208878 = DIRECTION ( 'NONE',  ( 0.000000000000000000, -1.000000000000000000, 0.000000000000000000 ) ) ;
#208879 = DIRECTION ( 'NONE',  ( -0.6260462619842731558, 0.7797859179643593652, 0.000000000000000000 ) ) ;
#208880 = CARTESIAN_POINT ( 'NONE',  ( -8.857554428429624593, 9.228235009456373206, 0.7998128361456462443 ) ) ;
#208881 = CARTESIAN_POINT ( 'NONE',  ( -4.814553946628611136, 8.631080347793099961, 0.000000000000000000 ) ) ;
#208883 = CARTESIAN_POINT ( 'NONE',  ( 3.924554409752772699, 1.776107677202539925, 0.5873546117282567591 ) ) ;
#208882 = CARTESIAN_POINT ( 'NONE',  ( 4.546477914129923192, -1.678139501482888152, 1.246787890680167710 ) ) ;
#208884 = CARTESIAN_POINT ( 'NONE',  ( 6.968527767744104651, 8.192665819532020777, 1.082531754730558626 ) ) ;
#208885 = ORIENTED_EDGE ( 'NONE', *, *, #139883, .F. ) ;
#208886 = CARTESIAN_POINT ( 'NONE',  ( 2.972444473424885381, 6.543659789869906263, -0.5046856791834258837 ) ) ;
#208887 = CARTESIAN_POINT ( 'NONE',  ( -3.768803514918907194, 7.340761834140026032, 0.7216878364870037421 ) ) ;
#208888 = CARTESIAN_POINT ( 'NONE',  ( 6.533849689656099358, -1.133137674240388248, -1.300586445545851344 ) ) ;
#208889 = CARTESIAN_POINT ( 'NONE',  ( -4.713430959045263435, 8.650753218861462202, 0.7998128361456481317 ) ) ;
#208890 = CARTESIAN_POINT ( 'NONE',  ( 1.635018144205732771, 0.5444147220468772419, 1.646514679669469849 ) ) ;
#208891 = CARTESIAN_POINT ( 'NONE',  ( -9.333041836230020039, 14.55305236562984383, 7.472413793098202639 ) ) ;
#208892 = FACE_OUTER_BOUND ( 'NONE', #125356, .T. ) ;
#208893 = FACE_OUTER_BOUND ( 'NONE', #5322, .T. ) ;
#208894 = CARTESIAN_POINT ( 'NONE',  ( 5.981339239477990510, -0.06126731230964890806, 2.170386710549534470 ) ) ;
#208895 = CARTESIAN_POINT ( 'NONE',  ( 4.230939532379584200, 0.09184734775685021724, 1.823503176236190626 ) ) ;
#208896 = CARTESIAN_POINT ( 'NONE',  ( 1.692165188054130187, 0.9715730843921737137, -1.704227633833883759 ) ) ;
#208897 = CARTESIAN_POINT ( 'NONE',  ( 6.473823543489908516, -0.9023987703748233002, 1.913193491996653783 ) ) ;
#208898 = DIRECTION ( 'NONE',  ( 0.000000000000000000, 0.000000000000000000, 1.000000000000000000 ) ) ;
#208899 = CARTESIAN_POINT ( 'NONE',  ( 1.499999999999990896, 5.525000000000022560, 1.214306433183764966E-14 ) ) ;
#208900 = CARTESIAN_POINT ( 'NONE',  ( 8.586391356156291010, 8.911878091804165791, 0.7998128361456481317 ) ) ;
#208901 = CARTESIAN_POINT ( 'NONE',  ( 2.543736517606724146, -1.977637755382474438, 0.7655657148115800892 ) ) ;
#208902 = DIRECTION ( 'NONE',  ( 0.000000000000000000, -1.000000000000000000, -1.804652791718263484E-16 ) ) ;
#208903 = CARTESIAN_POINT ( 'NONE',  ( -5.239262321155076840, 6.291427928779091516, 1.253643227873025179 ) ) ;
#208904 = CARTESIAN_POINT ( 'NONE',  ( -4.729598638066518035, 6.837371794175130191, -1.235194855336968045 ) ) ;
#208905 = CARTESIAN_POINT ( 'NONE',  ( 0.2685318824256071601, -0.8817220219094963340, -1.871193708407721035 ) ) ;
#208907 = CARTESIAN_POINT ( 'NONE',  ( 1.499999999999993117, 14.13541666734946389, 0.8660254037844409281 ) ) ;
#208906 = CARTESIAN_POINT ( 'NONE',  ( -10.79323474359244805, 4.699907862511227385, 5.141973737680021195 ) ) ;
#208909 = ORIENTED_EDGE ( 'NONE', *, *, #213110, .F. ) ;
#208908 = CARTESIAN_POINT ( 'NONE',  ( 3.123905467589927820, -0.4314640245299468657, 2.178836924841739631 ) ) ;
#208910 = CARTESIAN_POINT ( 'NONE',  ( 0.6690544563107813092, 1.549219078230345215, 1.698357357312555660 ) ) ;
#208912 = CARTESIAN_POINT ( 'NONE',  ( 6.438341905586414171, -1.108352981827376738, 1.739313939070710857 ) ) ;
#208911 = CARTESIAN_POINT ( 'NONE',  ( 4.359110081993588182, 5.044382169536003602, -1.199719254218452047 ) ) ;
#208914 = CARTESIAN_POINT ( 'NONE',  ( -3.475000000000000533, -1.429166666666668251, -2.006292185433948827 ) ) ;
#208913 = CARTESIAN_POINT ( 'NONE',  ( 3.203469434578891661, 6.959407783642502565, -0.7998128361456362523 ) ) ;
#208915 = CARTESIAN_POINT ( 'NONE',  ( 0.1333542156527478262, 0.001576319744088505292, -2.046049510433409768 ) ) ;
#208916 = CARTESIAN_POINT ( 'NONE',  ( 5.759284750224211713, 1.812880138157666465, -0.3211251414683007899 ) ) ;
#208917 = DIRECTION ( 'NONE',  ( 0.7592566023653005702, -0.6507913734559639396, 0.000000000000000000 ) ) ;
#208918 = CARTESIAN_POINT ( 'NONE',  ( -0.2102771530458459603, 1.310786636098780544, -2.452585248267840967 ) ) ;
#208919 = CARTESIAN_POINT ( 'NONE',  ( 2.643205280608558194, -1.276243157467608302, -1.160367288944160968 ) ) ;
#208920 = CARTESIAN_POINT ( 'NONE',  ( 1.481658059775035952, -0.6748446255696785023, 1.900416712880992343 ) ) ;
#208921 = CARTESIAN_POINT ( 'NONE',  ( 3.129784643070336436, 0.5604733119842463251, 2.229205935122404725 ) ) ;
#208922 = CARTESIAN_POINT ( 'NONE',  ( 2.425404053729601550, -0.002036344795489434568, 2.262578821637390547 ) ) ;
#208923 = CARTESIAN_POINT ( 'NONE',  ( 5.672525241255916839, -1.337268198843853506, 1.627036470456619810 ) ) ;
#208924 = CARTESIAN_POINT ( 'NONE',  ( -6.211043768836215229, 8.339580045099285854, 1.443375672974064550 ) ) ;
#208925 = CARTESIAN_POINT ( 'NONE',  ( 4.094789254117153554, 1.496004596371943496, -0.9451293409883186891 ) ) ;
#208927 = CARTESIAN_POINT ( 'NONE',  ( 0.006404353242023088852, -0.9848532314915852126, -2.067437341614616120 ) ) ;
#208926 = CARTESIAN_POINT ( 'NONE',  ( 3.404505970362959655, 6.986024375483197879, 0.7216878364870257245 ) ) ;
#208928 = CARTESIAN_POINT ( 'NONE',  ( 4.189278935350455590, -0.7026162016144417155, 1.701997885059022497 ) ) ;
#208929 = CARTESIAN_POINT ( 'NONE',  ( -5.599681137644054729, 6.491715067794862293, 1.199719254218450271 ) ) ;
#208930 = CARTESIAN_POINT ( 'NONE',  ( 5.788968402910812827, 6.816513227226497662, 1.082531754730558626 ) ) ;
#208931 = CARTESIAN_POINT ( 'NONE',  ( -0.7500000000000215383, 3.691666666666690411, 1.299038105676671107 ) ) ;
#208932 = EDGE_CURVE ( 'NONE', #104308, #142643, #71930, .T. ) ;
#208933 = CARTESIAN_POINT ( 'NONE',  ( 5.068408068084750084, -2.062719301109996461, -0.7404068969242216802 ) ) ;
#208934 = CARTESIAN_POINT ( 'NONE',  ( -4.959585264500673496, 4.680604318205876524, 1.214306433183764966E-14 ) ) ;
#208935 = CARTESIAN_POINT ( 'NONE',  ( 0.5511734105799784844, 7.507429961897218895, -1.922562588595817301 ) ) ;
#208936 = CARTESIAN_POINT ( 'NONE',  ( 5.125469573878929097, 0.2063957376101481500, -2.060066405364005426 ) ) ;
#208937 = CARTESIAN_POINT ( 'NONE',  ( 0.2511858651975951151, 0.1928294586405615574, -2.007256720055437871 ) ) ;
#208938 = CARTESIAN_POINT ( 'NONE',  ( 1.364683531249990311, 4.634375000341417916, 1.214306433183764966E-14 ) ) ;
#208939 = CARTESIAN_POINT ( 'NONE',  ( 3.334515964829305457, 1.879714267205140565, 0.4213298384171912381 ) ) ;
#208940 = CARTESIAN_POINT ( 'NONE',  ( -0.6823417656250039265, 9.567708333674735499, -1.181850606188755259 ) ) ;
#208941 = CARTESIAN_POINT ( 'NONE',  ( -4.297571505851936813, 4.116180966356429494, 1.214306433183764966E-14 ) ) ;
#208942 = CARTESIAN_POINT ( 'NONE',  ( 0.2643399247034176613, 0.6888887472211238094, -2.111998681152967183 ) ) ;
#208943 = ORIENTED_EDGE ( 'NONE', *, *, #77981, .F. ) ;
#208945 = DIRECTION ( 'NONE',  ( 0.000000000000000000, 1.000000000000000000, 0.000000000000000000 ) ) ;
#208944 = DIRECTION ( 'NONE',  ( 0.000000000000000000, 1.000000000000000000, 0.000000000000000000 ) ) ;
#208946 = CARTESIAN_POINT ( 'NONE',  ( 4.168242161197552420, 6.950367390450747251, -1.199719254218452047 ) ) ;
#208947 = CARTESIAN_POINT ( 'NONE',  ( 4.542476715900265916, 4.951051008190067826, -0.8264431066547142102 ) ) ;
#208948 = CARTESIAN_POINT ( 'NONE',  ( 1.499999999999996891, 11.17708333401612819, -0.8660254037844378194 ) ) ;
#208949 = CARTESIAN_POINT ( 'NONE',  ( 11.55950211276791251, 13.87999999999998302, 3.221476510067114329 ) ) ;
#208950 = CARTESIAN_POINT ( 'NONE',  ( -6.098824340890369733, 6.672706474115194908, -0.7681833417966426047 ) ) ;
#208952 = EDGE_CURVE ( 'NONE', #86738, #30509, #170264, .T. ) ;
#208951 = CARTESIAN_POINT ( 'NONE',  ( 1.117545225965112188, 0.3861695934333775337, -1.923310697798483293 ) ) ;
#208953 = CARTESIAN_POINT ( 'NONE',  ( 0.6823417656249899377, 1.655208333674752730, 1.181850606188755259 ) ) ;
#208954 = CARTESIAN_POINT ( 'NONE',  ( 6.754756207809571755, -1.674487575904315406, 1.366813541845832924 ) ) ;
#208955 = ADVANCED_FACE ( 'NONE', ( #83676 ), #58049, .T. ) ;
#208956 = AXIS2_PLACEMENT_3D ( 'NONE', #183117, #34724, #84551 ) ;
#208957 = CARTESIAN_POINT ( 'NONE',  ( 5.019951445752288244, 1.940773837913706057, -0.2859759768028962146 ) ) ;
#208958 = CARTESIAN_POINT ( 'NONE',  ( -8.459397779922852578, 11.95671561229694824, 1.199719254218453823 ) ) ;
#208959 = CARTESIAN_POINT ( 'NONE',  ( -5.219525951136850139, 7.112532914458205013, -1.443375672974051449 ) ) ;
#208960 = CARTESIAN_POINT ( 'NONE',  ( 6.121977807712331909, -1.196819783530624015, -1.799967629666970881 ) ) ;
#208962 = ORIENTED_EDGE ( 'NONE', *, *, #78852, .T. ) ;
#208961 = FACE_OUTER_BOUND ( 'NONE', #198411, .T. ) ;
#208963 = CARTESIAN_POINT ( 'NONE',  ( -1.201851678989727383E-14, 4.071875000341425022, 1.575800808251672791 ) ) ;
#208964 = CARTESIAN_POINT ( 'NONE',  ( 6.784453690597813669, -1.932871751835860241, -0.3867854297147227394 ) ) ;
#208965 = CARTESIAN_POINT ( 'NONE',  ( 6.257189190585941141, -1.725921076436988111, -0.1656679613657590366 ) ) ;
#208966 = VECTOR ( 'NONE', #31140, 1000.000000000000000 ) ;
#208968 = CARTESIAN_POINT ( 'NONE',  ( 2.560326853991791829, -1.509077608345666066, 1.589458984681046516 ) ) ;
#208967 = CARTESIAN_POINT ( 'NONE',  ( 0.6801582343749917881, 0.7239583336747443809, 1.178068619123793015 ) ) ;
#208969 = CARTESIAN_POINT ( 'NONE',  ( 4.735574959254028826, -2.111847384580630038, 0.9304801611131856554 ) ) ;
#208970 = CARTESIAN_POINT ( 'NONE',  ( 5.413377607122367152, -0.3064755606005803434, 2.037752308911133348 ) ) ;
#208971 = CARTESIAN_POINT ( 'NONE',  ( 0.8670093773819181893, 1.871751486835357747, -0.5171616756182734198 ) ) ;
#208972 = CARTESIAN_POINT ( 'NONE',  ( -7.199016378732087773, 7.501199984716642177, 0.7216878364870317197 ) ) ;
#208973 = CARTESIAN_POINT ( 'NONE',  ( 4.640951271726033056, 2.030106984047326701, 0.6129599860185754867 ) ) ;
#208974 = CARTESIAN_POINT ( 'NONE',  ( 2.373672848961404735, -0.3474683332905931232, -1.986100487175908258 ) ) ;
#208975 = CARTESIAN_POINT ( 'NONE',  ( -4.406036734316898240, 6.163462161501577441, -1.443375672974051449 ) ) ;
#208976 = CARTESIAN_POINT ( 'NONE',  ( 6.088949818052607377, -0.3178892970779038096, -2.183640257897196513 ) ) ;
#208977 = CARTESIAN_POINT ( 'NONE',  ( -3.422965436091124136, -3.085995815972477629, -0.3132428434422417918 ) ) ;
#208978 = CARTESIAN_POINT ( 'NONE',  ( 0.1350027811974127134, -1.670744041527939094, 0.7364786222084362954 ) ) ;
#208979 = CARTESIAN_POINT ( 'NONE',  ( -4.586401103172829785, 8.572828063668767484, 0.7998128361456281477 ) ) ;
#208981 = CARTESIAN_POINT ( 'NONE',  ( -6.466312919074983512, 6.508729591867735031, -0.7998128361456361413 ) ) ;
#208980 = CARTESIAN_POINT ( 'NONE',  ( -4.733024909954385073, 8.320217716143888609, 0.7565452571775049817 ) ) ;
#208982 = FACE_OUTER_BOUND ( 'NONE', #170400, .T. ) ;
#208983 = ORIENTED_EDGE ( 'NONE', *, *, #64571, .T. ) ;
#208984 = CARTESIAN_POINT ( 'NONE',  ( 5.875869988399868404, 1.225711027941748466, 1.656622483273604729 ) ) ;
#208985 = CARTESIAN_POINT ( 'NONE',  ( 1.360316468750000896, 2.515625000341401130, -3.469446951953614189E-15 ) ) ;
#208986 = CARTESIAN_POINT ( 'NONE',  ( -0.2108831679770959699, 2.036692374882024037, -2.313561348563981657 ) ) ;
#208987 = CARTESIAN_POINT ( 'NONE',  ( -2.605138072120212200, 6.191078184115536232, -0.7998128361456281477 ) ) ;
#208988 = CARTESIAN_POINT ( 'NONE',  ( -4.462568837553487100, 5.235360394347691404, -1.199719254218453823 ) ) ;
#208989 = CARTESIAN_POINT ( 'NONE',  ( 4.916668454303085412, -0.6825918349771132876, -1.900952964002266210 ) ) ;
#208990 = CARTESIAN_POINT ( 'NONE',  ( -0.7500000000000215383, 0.1916666666666871910, 1.299038105676659116 ) ) ;
#208992 = CARTESIAN_POINT ( 'NONE',  ( 8.758204044747998296, 11.24099069033793974, 1.443375672974076540 ) ) ;
#208991 = CARTESIAN_POINT ( 'NONE',  ( -4.980641328173854632, 6.904110530993182948, 1.599625672291263179 ) ) ;
#208993 = CARTESIAN_POINT ( 'NONE',  ( 7.793239369756836510, 7.986534107671458216, 0.7998128361456341429 ) ) ;
#208994 = CARTESIAN_POINT ( 'NONE',  ( 3.766525121192493941, -1.385455288492474235, 1.525868174829993373 ) ) ;
#208995 = CARTESIAN_POINT ( 'NONE',  ( 3.287732575140738245, 1.587837554856496469, -1.242726844152844956 ) ) ;
#208996 = ORIENTED_EDGE ( 'NONE', *, *, #90038, .T. ) ;
#208997 = CARTESIAN_POINT ( 'NONE',  ( 6.727182134110194056, 3.682851444631680238, 2.702965647100653790 ) ) ;
#208998 = CARTESIAN_POINT ( 'NONE',  ( 3.181359600701000989, 6.863336634126477875, 0.000000000000000000 ) ) ;
#209000 = ORIENTED_EDGE ( 'NONE', *, *, #18978, .F. ) ;
#208999 = CARTESIAN_POINT ( 'NONE',  ( -3.062251564868939457, 6.240124004417943127, -0.7724295644362719759 ) ) ;
#209001 = CARTESIAN_POINT ( 'NONE',  ( 3.233749808020690342, -1.861731463674856979, -0.7741979076196570109 ) ) ;
#209002 = CARTESIAN_POINT ( 'NONE',  ( 2.378628397106247849, 1.683441843134887428, -0.7459445200509451368 ) ) ;
#209003 = CARTESIAN_POINT ( 'NONE',  ( 1.137850649969934347, -2.084210194689451789, 0.9910022104400189047 ) ) ;
#209004 = CARTESIAN_POINT ( 'NONE',  ( 4.655245641445829641, 6.524482229810530498, 1.599625672291269396 ) ) ;
#209005 = CARTESIAN_POINT ( 'NONE',  ( 2.442841770826277958, 0.4709965094221583159, 2.109507199432036018 ) ) ;
#209006 = CARTESIAN_POINT ( 'NONE',  ( -5.225778143063529946, 8.184159369294361497, 1.199719254218452047 ) ) ;
#209007 = ORIENTED_EDGE ( 'NONE', *, *, #158430, .F. ) ;
#209008 = CARTESIAN_POINT ( 'NONE',  ( 0.000000000000000000, 0.5000000000000000000, 0.000000000000000000 ) ) ;
#209009 = CARTESIAN_POINT ( 'NONE',  ( 0.9888773766892227091, 1.651582696977689890, -0.8784067438419729257 ) ) ;
#209010 = CARTESIAN_POINT ( 'NONE',  ( 5.840691970153715218, 0.3840316513750040572, 1.933538979438324867 ) ) ;
#209011 = CIRCLE ( 'NONE', #105313, 0.08000000000000041800 ) ;
#209013 = CARTESIAN_POINT ( 'NONE',  ( 9.531018800282609504, 10.22186947652563305, 0.7216878364870458196 ) ) ;
#209012 = CARTESIAN_POINT ( 'NONE',  ( -0.6823417656250212460, 3.301041667008085323, 1.181850606188767472 ) ) ;
#209015 = CARTESIAN_POINT ( 'NONE',  ( 0.4521680116954321371, 0.6883007682146925488, -2.096869779678663281 ) ) ;
#209014 = CARTESIAN_POINT ( 'NONE',  ( -7.226659571283968297, 8.389856573708110332, 1.199719254218450271 ) ) ;
#209016 = CARTESIAN_POINT ( 'NONE',  ( 6.848098043024292814, -0.8888149443028300345, 1.868052569137634400 ) ) ;
#209017 = CARTESIAN_POINT ( 'NONE',  ( 5.301401758143367893, 6.143722458377430584, 1.199719254218462483 ) ) ;
#209018 = CARTESIAN_POINT ( 'NONE',  ( -4.954615070790188369, 7.867802451642154082, -1.199719254218452047 ) ) ;
#209019 = CARTESIAN_POINT ( 'NONE',  ( 6.539320575229280230, 7.629137130509070275, 2.703262396134015866 ) ) ;
#209020 = CARTESIAN_POINT ( 'NONE',  ( 5.067239680553584869, 0.1942248685237786265, -1.961885565008324006 ) ) ;
#209021 = CARTESIAN_POINT ( 'NONE',  ( 0.08834397731360790762, 1.226219587655341448, 1.729930300845914815 ) ) ;
#209022 = CARTESIAN_POINT ( 'NONE',  ( 4.846439200125199243, 2.301219453760998679, 0.1735292846544200795 ) ) ;
#209023 = CIRCLE ( 'NONE', #195297, 0.08000000000000020983 ) ;
#209024 = CARTESIAN_POINT ( 'NONE',  ( 3.309489505334945569, -1.683523595015530505, -1.191345380358753925 ) ) ;
#209025 = CARTESIAN_POINT ( 'NONE',  ( 6.317736394288122170, 10.31451686007074997, 0.7216878364870438212 ) ) ;
#209026 = EDGE_CURVE ( 'NONE', #169163, #211199, #150841, .T. ) ;
#209027 = CARTESIAN_POINT ( 'NONE',  ( 4.960304097753311936, 6.880383762169266504, 1.599625672291268286 ) ) ;
#209028 = CARTESIAN_POINT ( 'NONE',  ( 4.980641328173811999, 6.904110530993182948, 1.599625672291269396 ) ) ;
#209029 = CARTESIAN_POINT ( 'NONE',  ( 1.364683531249990311, 2.696875000341415696, 1.214306433183764966E-14 ) ) ;
#209030 = CARTESIAN_POINT ( 'NONE',  ( 5.076602173674213070, 4.887400388900169368, 0.000000000000000000 ) ) ;
#209031 = CARTESIAN_POINT ( 'NONE',  ( 4.324687812634874895, 7.989293514808604613, 0.7216878364870317197 ) ) ;
#209032 = CARTESIAN_POINT ( 'NONE',  ( 5.547405112160277874, 1.917339678720403118, -1.018715297254897401 ) ) ;
#209034 = CARTESIAN_POINT ( 'NONE',  ( 3.948646536499214932, -1.533023199436277961, -1.019512891124202403 ) ) ;
#209033 = CARTESIAN_POINT ( 'NONE',  ( -4.284013352238265959, 5.060732334775157604, -1.082531754730544860 ) ) ;
#209036 = CARTESIAN_POINT ( 'NONE',  ( 6.620655732516673275, 1.290356161719278028, 1.942653802560645460 ) ) ;
#209035 = CARTESIAN_POINT ( 'NONE',  ( -11.81911962874431055, 11.25710573484113830, 1.591749704452489533 ) ) ;
#209037 = CARTESIAN_POINT ( 'NONE',  ( 5.899973326018037589, -0.7874313895239596350, -2.045375389432432467 ) ) ;
#209038 = CARTESIAN_POINT ( 'NONE',  ( -4.123088111887291518, 7.824370207261548416, 0.000000000000000000 ) ) ;
#209039 = CARTESIAN_POINT ( 'NONE',  ( 0.1813603024932753938, -0.1560989159599696641, -2.227174003853182871 ) ) ;
#209040 = CARTESIAN_POINT ( 'NONE',  ( -4.377891688998395203, 7.365737962781053305, -1.202262209786943759 ) ) ;
#209041 =( LENGTH_UNIT ( ) NAMED_UNIT ( * ) SI_UNIT ( .MILLI., .METRE. ) );
#209042 = CARTESIAN_POINT ( 'NONE',  ( 4.774898309648160755, 8.276035162536045320, 0.8191430224755236189 ) ) ;
#209043 = CARTESIAN_POINT ( 'NONE',  ( -5.112833325684920993, 6.097965313788082931, -1.082531754730549967 ) ) ;
#209044 = CARTESIAN_POINT ( 'NONE',  ( 4.475600106286968582, 5.354526557823810151, -1.082531754730548412 ) ) ;
#209045 = CARTESIAN_POINT ( 'NONE',  ( 1.006321374186702311, 1.343689884961623227, -1.152001066587736267 ) ) ;
#209046 = CARTESIAN_POINT ( 'NONE',  ( 5.145186220991746495, 0.1505098195577254938, 2.007535063509538809 ) ) ;
#209047 = CARTESIAN_POINT ( 'NONE',  ( 6.226218857173709154, 8.287007971501239467, 1.599625672291281386 ) ) ;
#209048 = CARTESIAN_POINT ( 'NONE',  ( 3.645630060059632083, -1.593344849414342290, -1.377153647973597073 ) ) ;
#209049 = CARTESIAN_POINT ( 'NONE',  ( 2.724132717865447084, 1.901453608201342238, 0.2316716071539808575 ) ) ;
#209050 = CARTESIAN_POINT ( 'NONE',  ( 0.000000000000000000, 0.2000000000000057288, -11.50000000000000000 ) ) ;
#209051 = CARTESIAN_POINT ( 'NONE',  ( 4.738697576358215535, -1.909850223682897807, -0.4806687167441258679 ) ) ;
#209052 = CARTESIAN_POINT ( 'NONE',  ( 6.029558467290160984, -0.2429869472727399504, 2.005020512606956018 ) ) ;
#209053 = CARTESIAN_POINT ( 'NONE',  ( 1.375632740723360836, 1.111493989511678881, 1.504490780774490499 ) ) ;
#209056 = VERTEX_POINT ( 'NONE', #200612 ) ;
#209055 = CARTESIAN_POINT ( 'NONE',  ( 1.125099709691119276, 1.687896996356451629, 0.8989547360247207575 ) ) ;
#209054 = CARTESIAN_POINT ( 'NONE',  ( 5.039546052477672511, -1.223360384887246743, -1.216254805912063919 ) ) ;
#209058 = CARTESIAN_POINT ( 'NONE',  ( 3.524756749872944628, 7.056040608253000279, -0.7216878364870267237 ) ) ;
#209057 = CARTESIAN_POINT ( 'NONE',  ( 1.506762622594171930, -0.7967928049063888185, -2.058199171410409978 ) ) ;
#209059 = CARTESIAN_POINT ( 'NONE',  ( -1.402160292154681736E-14, 2.009375000341422801, -1.575800808251660134 ) ) ;
#209060 = CARTESIAN_POINT ( 'NONE',  ( 6.591235234537977661, 10.84152487360300299, 0.7998128361456462443 ) ) ;
#209061 = CARTESIAN_POINT ( 'NONE',  ( 6.631728656526095556, -1.223761959379562114, -1.414937998750566361 ) ) ;
#209062 = CARTESIAN_POINT ( 'NONE',  ( 0.5451294715435256455, 6.857673057455659915, -3.776897409940819017 ) ) ;
#209063 = CARTESIAN_POINT ( 'NONE',  ( -4.660252114795309097, 6.460046772059735432, -1.599625672291256517 ) ) ;
#209064 = CARTESIAN_POINT ( 'NONE',  ( 6.726765607527583235, -8.198316282514454656, 6.726765607527558366 ) ) ;
#209065 = ORIENTED_EDGE ( 'NONE', *, *, #177202, .T. ) ;
#209066 = CARTESIAN_POINT ( 'NONE',  ( 1.609917502266303480, 0.6029389078928657497, -1.980602105166151095 ) ) ;
#209067 = CARTESIAN_POINT ( 'NONE',  ( -0.7500000000000006661, 2.858333333333358706, -1.299038105676652011 ) ) ;
#209068 = CARTESIAN_POINT ( 'NONE',  ( 4.937140493670735708, 8.911747675924535983, -0.7998128361456281477 ) ) ;
#209069 = CARTESIAN_POINT ( 'NONE',  ( -8.362681821530818738, 8.650883634741092010, -0.7998128361456291469 ) ) ;
#209070 = CARTESIAN_POINT ( 'NONE',  ( 5.090160327287878594, 4.903218234782778850, -0.7998128361456481317 ) ) ;
#209071 = CARTESIAN_POINT ( 'NONE',  ( 0.1002680356884171620, -0.9499045104094726577, 1.782327323349098602 ) ) ;
#209072 = CARTESIAN_POINT ( 'NONE',  ( 1.499999999999996891, 10.42708333401613352, -0.8660254037844378194 ) ) ;
#209073 = EDGE_CURVE ( 'NONE', #73414, #52005, #3475, .T. ) ;
#209074 = CARTESIAN_POINT ( 'NONE',  ( 1.364683531249988535, 2.905208333674754506, -0.7879004041258239610 ) ) ;
#209076 = CARTESIAN_POINT ( 'NONE',  ( 8.568389894156670294, 12.94027927658408217, -0.7216878364870257245 ) ) ;
#209075 = CARTESIAN_POINT ( 'NONE',  ( 11.33772463945036790, 10.90000000000000036, -3.680000000000002824 ) ) ;
#209077 = CARTESIAN_POINT ( 'NONE',  ( 5.026720154644213068, 1.994564127574052437, -0.2930270067487000252 ) ) ;
#209078 = CARTESIAN_POINT ( 'NONE',  ( 5.190618481123168593, 1.446159319891277661, -1.256491027437984354 ) ) ;
#209079 = DIRECTION ( 'NONE',  ( 0.6507913734559641616, -0.7592566023653004592, 0.000000000000000000 ) ) ;
#209080 = CARTESIAN_POINT ( 'NONE',  ( 2.560326853991791829, -1.509077608345666066, 1.589458984681046516 ) ) ;
#209081 = CARTESIAN_POINT ( 'NONE',  ( 0.1335669894368864408, 5.721243636067999461, -2.747585559332069494 ) ) ;
#209082 = CARTESIAN_POINT ( 'NONE',  ( 0.7499999999999885647, 0.5145833340161540814, 1.299038105676657340 ) ) ;
#209083 = CARTESIAN_POINT ( 'NONE',  ( 5.818613517226002507, -0.7285450932710479943, -1.876915101588324974 ) ) ;
#209084 = CARTESIAN_POINT ( 'NONE',  ( 1.459083999156213229, -1.613880964290699938, 1.025699646091532857 ) ) ;
#209085 = CARTESIAN_POINT ( 'NONE',  ( -5.682838942422375084, 9.781729199468104596, 0.000000000000000000 ) ) ;
#209086 = EDGE_CURVE ( 'NONE', #201094, #45840, #99640, .T. ) ;
#209088 = CARTESIAN_POINT ( 'NONE',  ( 6.450787963126683344, -1.935726721829626351, -0.8580517621625349811 ) ) ;
#209087 = CARTESIAN_POINT ( 'NONE',  ( -4.622967192579922724, 4.495809267539077503, 1.214306433183764966E-14 ) ) ;
#209089 = CARTESIAN_POINT ( 'NONE',  ( 0.6823417656249934904, 9.505208333674728394, 1.181850606188764807 ) ) ;
#209091 = CARTESIAN_POINT ( 'NONE',  ( -7.014364370223741929, 9.276787413384745662, -1.599625672291271394 ) ) ;
#209090 = CARTESIAN_POINT ( 'NONE',  ( 3.860945534362031140, 0.2537485593089708336, -2.075202752206976697 ) ) ;
#209093 = EDGE_LOOP ( 'NONE', ( #67204, #74318, #151234, #143374 ) ) ;
#209092 = CARTESIAN_POINT ( 'NONE',  ( 1.799380453634431998, -0.5854278125525367305, 1.622511832645438190 ) ) ;
#209094 = CARTESIAN_POINT ( 'NONE',  ( 6.416280414004661203, -2.120105685773795212, 0.05337830808049835035 ) ) ;
#209095 = CARTESIAN_POINT ( 'NONE',  ( 5.178324605415663306, 8.128796908705222535, 1.199719254218462483 ) ) ;
#209096 = CARTESIAN_POINT ( 'NONE',  ( 11.00592642091246454, 12.48979727563561504, 1.444015479094872934 ) ) ;
#209097 = CARTESIAN_POINT ( 'NONE',  ( 7.586009164902111301, -6.657020681837064302, 7.796438949605565938 ) ) ;
#209098 = DIRECTION ( 'NONE',  ( 0.7592566023653005702, -0.6507913734559639396, 0.000000000000000000 ) ) ;
#209099 = CARTESIAN_POINT ( 'NONE',  ( 6.494519276145969577, 7.535692896047149425, -1.199719254218446718 ) ) ;
#209100 = ORIENTED_EDGE ( 'NONE', *, *, #213856, .F. ) ;
#209101 = CARTESIAN_POINT ( 'NONE',  ( 2.701584635150193314, 1.282363399140455273, 1.279706459777726346 ) ) ;
#209102 = CARTESIAN_POINT ( 'NONE',  ( -5.096975683733680818, 8.033889833409558534, -1.199719254218452047 ) ) ;
#209103 = ORIENTED_EDGE ( 'NONE', *, *, #199193, .T. ) ;
#209104 = CARTESIAN_POINT ( 'NONE',  ( 3.948449050077836642, 5.629609863222681199, 1.599625672291267398 ) ) ;
#209105 = ORIENTED_EDGE ( 'NONE', *, *, #78185, .F. ) ;
#209106 = CARTESIAN_POINT ( 'NONE',  ( 4.736594563127852098, 6.619389305106191834, -1.599625672291273171 ) ) ;
#209107 = CARTESIAN_POINT ( 'NONE',  ( 4.107922266221023300, -0.6895048676278795474, 1.675321109400946806 ) ) ;
#209108 = FACE_OUTER_BOUND ( 'NONE', #166860, .T. ) ;
#209109 = DIRECTION ( 'NONE',  ( -0.6507913734559642727, 0.7592566023653003482, 2.775557561562893816E-17 ) ) ;
#209110 = CARTESIAN_POINT ( 'NONE',  ( 4.525353972290461435, 6.990290696447242880, 1.167197606177571734 ) ) ;
#209111 = ORIENTED_EDGE ( 'NONE', *, *, #19714, .F. ) ;
#209112 = CARTESIAN_POINT ( 'NONE',  ( 3.666312420855986520, -0.7522870471967492145, -1.702408540065254883 ) ) ;
#209113 = CARTESIAN_POINT ( 'NONE',  ( 1.247507242870619981, 1.886983585358002813, -0.3289482045247971165 ) ) ;
#209114 = CARTESIAN_POINT ( 'NONE',  ( 0.6569167496461197908, -1.539450689919025450, -0.9809549629347169564 ) ) ;
#209115 = VECTOR ( 'NONE', #52012, 1000.000000000000000 ) ;
#209116 = DIRECTION ( 'NONE',  ( 0.000000000000000000, 1.000000000000000000, 0.000000000000000000 ) ) ;
#209117 = FACE_OUTER_BOUND ( 'NONE', #74862, .T. ) ;
#209118 = ADVANCED_FACE ( 'NONE', ( #67404 ), #55470, .T. ) ;
#209119 = CARTESIAN_POINT ( 'NONE',  ( 6.003728048595398548, 7.077753126805482076, 1.059392881431284961 ) ) ;
#209120 = FACE_OUTER_BOUND ( 'NONE', #67171, .T. ) ;
#209121 = CARTESIAN_POINT ( 'NONE',  ( -4.151086725614978157, 2.978102892632842558, 0.7750000000000117906 ) ) ;
#209122 = CARTESIAN_POINT ( 'NONE',  ( -3.551873057100300990, 5.166937871415542283, 1.443375672974064550 ) ) ;
#209123 = CIRCLE ( 'NONE', #12001, 4.022469383779238683 ) ;
#209124 = CARTESIAN_POINT ( 'NONE',  ( 8.595506201384020883, 9.130438111143927671, 0.7216878364870438212 ) ) ;
#209125 = CARTESIAN_POINT ( 'NONE',  ( 5.471530992243406999, -0.2926990004611991214, 1.947462276923512370 ) ) ;
#209126 = CARTESIAN_POINT ( 'NONE',  ( -4.497554271431319250, 6.270232621468402989, -1.599625672291256295 ) ) ;
#209127 = DIRECTION ( 'NONE',  ( 1.000000000000000000, 0.000000000000000000, 0.000000000000000000 ) ) ;
#209128 = CARTESIAN_POINT ( 'NONE',  ( 0.7090669197488512765, -0.3047467688393705187, 2.068175119304823451 ) ) ;
#209129 = CARTESIAN_POINT ( 'NONE',  ( 7.446452682403650769, 9.710614100936176385, -1.599625672291262513 ) ) ;
#209130 = CARTESIAN_POINT ( 'NONE',  ( 5.034167752753979208, 0.9906028322895725768, -1.652054708979720399 ) ) ;
#209131 = CARTESIAN_POINT ( 'NONE',  ( -6.389970470742427189, 6.349387058821269747, -0.7998128361456291469 ) ) ;
#209132 = CARTESIAN_POINT ( 'NONE',  ( 0.9908991873810431006, 1.612194894691898250, -0.8564790819722142290 ) ) ;
#209133 = CARTESIAN_POINT ( 'NONE',  ( 2.315298440750997777, 1.971968782506158924, 0.9909306302095726160 ) ) ;
#209134 = FACE_OUTER_BOUND ( 'NONE', #23966, .T. ) ;
#209135 = CARTESIAN_POINT ( 'NONE',  ( 0.8086807686161383568, -0.4671638426185490967, -1.854305266343849734 ) ) ;
#209136 = AXIS2_PLACEMENT_3D ( 'NONE', #3216, #86629, #153768 ) ;
#209137 = CARTESIAN_POINT ( 'NONE',  ( 1.012081461190861065, 1.967466754592902989, -0.09309286250217158054 ) ) ;
#209138 = CARTESIAN_POINT ( 'NONE',  ( 2.454547613406708351, -1.690768538996465509, -0.9553028803331271579 ) ) ;
#209139 = ORIENTED_EDGE ( 'NONE', *, *, #21930, .T. ) ;
#209140 = CARTESIAN_POINT ( 'NONE',  ( 1.018907413236518789, 2.013924516646655949, -0.09611688112247382398 ) ) ;
#209142 = CARTESIAN_POINT ( 'NONE',  ( 5.330833089851809703, -1.751472900985746373, -0.6291486930528921162 ) ) ;
#209141 = CARTESIAN_POINT ( 'NONE',  ( -6.967964602780620353, 7.093989889524320525, 0.000000000000000000 ) ) ;
#209143 = CARTESIAN_POINT ( 'NONE',  ( 3.953084306836263995, 6.769626237021087789, 1.199719254218452047 ) ) ;
#209144 = CARTESIAN_POINT ( 'NONE',  ( -0.1909996267163149852, 7.629137130509101361, -2.600377616606447617 ) ) ;
#209145 = CARTESIAN_POINT ( 'NONE',  ( 10.55910270694468345, 11.21337466772398095, 0.7998128361456462443 ) ) ;
#209146 = CARTESIAN_POINT ( 'NONE',  ( -4.578903193113314174, 6.365139696764064325, 1.599625672291267398 ) ) ;
#209147 = CARTESIAN_POINT ( 'NONE',  ( -7.208094944320834863, 8.438474185576302133, -1.199719254218452047 ) ) ;
#209148 = CARTESIAN_POINT ( 'NONE',  ( 1.646283778714407342, 0.6915601415973006150, 2.079641132013386517 ) ) ;
#209149 = CARTESIAN_POINT ( 'NONE',  ( 4.419594888374914099, 5.218910793601261311, -1.082531754730548412 ) ) ;
#209150 = CARTESIAN_POINT ( 'NONE',  ( 8.188198428010544205, 8.517596018959260107, 0.000000000000000000 ) ) ;
#209151 = PLANE ( 'NONE',  #54640 ) ;
#209152 = CARTESIAN_POINT ( 'NONE',  ( 3.070728972534173096, -1.687097908962056803, -0.6982200720766564839 ) ) ;
#209153 = CARTESIAN_POINT ( 'NONE',  ( -11.92619526913699879, 10.19999999999999929, -1.328859060402686199 ) ) ;
#209154 = CARTESIAN_POINT ( 'NONE',  ( -4.600294193738529103, 4.261431402316699035, -0.7998128361456221525 ) ) ;
#209155 = CARTESIAN_POINT ( 'NONE',  ( -4.762026763822442277, 8.287006692039220468, -0.8189809589772244491 ) ) ;
#209156 = CARTESIAN_POINT ( 'NONE',  ( 4.000000000000012434, 4.999999999999997335, -0.7500000000000006661 ) ) ;
#209157 = CIRCLE ( 'NONE', #108910, 0.5000000000000004441 ) ;
#209158 = CARTESIAN_POINT ( 'NONE',  ( 9.240045382913317340, 10.73880668727576015, -1.199719254218446718 ) ) ;
#209159 = CARTESIAN_POINT ( 'NONE',  ( 0.6977243349758615043, -0.6943943954660827256, 1.797178231592330588 ) ) ;
#209160 = CARTESIAN_POINT ( 'NONE',  ( 5.155110299917927463, 1.633153276354940342, -1.086568599608192409 ) ) ;
#209161 = CARTESIAN_POINT ( 'NONE',  ( -1.500000000000015099, 14.97916666666666252, -0.8660254037844309360 ) ) ;
#209162 = CARTESIAN_POINT ( 'NONE',  ( -7.121056995675673740, 9.330985799753529264, -1.599625672291263179 ) ) ;
#209163 = CARTESIAN_POINT ( 'NONE',  ( 6.322179702674084467, 6.270297829408224111, 1.040834085586084257E-14 ) ) ;
#209164 = CARTESIAN_POINT ( 'NONE',  ( 5.372676843235411503, -0.05303982195071360595, -2.191091664329389399 ) ) ;
#209165 = FACE_OUTER_BOUND ( 'NONE', #118317, .T. ) ;
#209166 = CARTESIAN_POINT ( 'NONE',  ( 4.452052287080165982, -0.7971045336818067817, 1.910850710330507907 ) ) ;
#209168 = CARTESIAN_POINT ( 'NONE',  ( 0.6823417656249899377, 0.9052083336747520637, 1.181850606188755259 ) ) ;
#209167 = FILL_AREA_STYLE_COLOUR ( '', #210351 ) ;
#209169 = ORIENTED_EDGE ( 'NONE', *, *, #83250, .T. ) ;
#209170 = CARTESIAN_POINT ( 'NONE',  ( 3.534061846033216714, -1.878541635090751560, 1.324563465849286859 ) ) ;
#209172 = ORIENTED_EDGE ( 'NONE', *, *, #149834, .T. ) ;
#209171 = CARTESIAN_POINT ( 'NONE',  ( 7.131225611108085616, 10.30321839872603462, 1.082531754730558626 ) ) ;
#209173 = CARTESIAN_POINT ( 'NONE',  ( 4.665414256878284149, 6.536345614481700927, -1.443375672974068769 ) ) ;
#209174 = CARTESIAN_POINT ( 'NONE',  ( -7.772296586883777003, -5.601927612791864242, -7.784592198500460469 ) ) ;
#209175 = CARTESIAN_POINT ( 'NONE',  ( -7.587723245503481095, 8.881373870289390737, 1.199719254218452047 ) ) ;
#209176 = CARTESIAN_POINT ( 'NONE',  ( 4.171774378167571129, -1.117019396711134371, 1.588354668226848565 ) ) ;
#209177 = ORIENTED_EDGE ( 'NONE', *, *, #98691, .T. ) ;
#209178 = CARTESIAN_POINT ( 'NONE',  ( 7.714226216051361718, 11.94375498546120795, -0.7216878364870267237 ) ) ;
#209179 = ORIENTED_EDGE ( 'NONE', *, *, #31271, .T. ) ;
#209180 = CARTESIAN_POINT ( 'NONE',  ( 5.625241921295836889, 1.689600096388569561, 0.8957793909229803120 ) ) ;
#209181 = CARTESIAN_POINT ( 'NONE',  ( 5.895441327320324554, 1.309037806329484521, 1.123130245766153612 ) ) ;
#209182 = CARTESIAN_POINT ( 'NONE',  ( 4.803922858132807505, -1.082837210388952309, -1.700963621564715700 ) ) ;
#209183 = CARTESIAN_POINT ( 'NONE',  ( 7.752014238602739730E-16, 3.079999999999999183, 6.329999999999995630 ) ) ;
#209184 = CARTESIAN_POINT ( 'NONE',  ( 1.454063653991678473, 0.6380318336138122159, -2.112638918738508398 ) ) ;
#209186 = CARTESIAN_POINT ( 'NONE',  ( -4.841670253855968831, 4.821239182352949904, 0.000000000000000000 ) ) ;
#209185 = CARTESIAN_POINT ( 'NONE',  ( -3.838578530388868426, 7.492387228696840040, -0.009810069892855370621 ) ) ;
#209188 = CARTESIAN_POINT ( 'NONE',  ( 6.538360807962172672, 1.750891970090788119, 0.2567797125347607845 ) ) ;
#209187 = CARTESIAN_POINT ( 'NONE',  ( 1.623107816722869412, -1.968041427791475728, 0.7057566781872460782 ) ) ;
#209189 = CARTESIAN_POINT ( 'NONE',  ( 5.731092321990707283, 2.014232586630093191, 0.09613807139101374077 ) ) ;
#209191 = CARTESIAN_POINT ( 'NONE',  ( 3.539304732165698741, -1.735471681261467669, -1.497634786905965187 ) ) ;
#209190 = CARTESIAN_POINT ( 'NONE',  ( 3.874598038455354665, 7.742391154831717692, -0.7998128361456362523 ) ) ;
#209192 = CARTESIAN_POINT ( 'NONE',  ( 1.147962396684144792, -1.373903031218721926, 1.068100470705938276 ) ) ;
#209193 = CARTESIAN_POINT ( 'NONE',  ( 2.654661980655496301, 2.105093816413053709, 0.2552270188876659129 ) ) ;
#209194 = DIRECTION ( 'NONE',  ( 0.7592566023653005702, 0.6507913734559639396, 0.000000000000000000 ) ) ;
#209195 = CARTESIAN_POINT ( 'NONE',  ( 1.352469423652577607, -0.7852941029048329247, 1.545897522503926647 ) ) ;
#209196 = CARTESIAN_POINT ( 'NONE',  ( 1.360316468749951602, 2.526041667008117830, 0.7853790794158560518 ) ) ;
#209197 = CARTESIAN_POINT ( 'NONE',  ( 1.152544200391303786, -0.4473333697519957242, -1.806370492606963474 ) ) ;
#209198 = CARTESIAN_POINT ( 'NONE',  ( 1.153041021216383299, -0.5271860560512993121, -2.106100485105724562 ) ) ;
#209199 = CARTESIAN_POINT ( 'NONE',  ( 3.028530041973789722, 0.4946322284519070189, 1.954779462066410733 ) ) ;
#209200 = CARTESIAN_POINT ( 'NONE',  ( 4.875000000000002665, 2.052068128417942727, -2.776269294175867294E-13 ) ) ;
#209201 = CARTESIAN_POINT ( 'NONE',  ( -1.201851678989727383E-14, 1.243750000682821044, 1.732050807568877637 ) ) ;
#209202 = CARTESIAN_POINT ( 'NONE',  ( 6.656866507323381477, -1.487278495449697147, 1.224136630395280534 ) ) ;
#209203 = CARTESIAN_POINT ( 'NONE',  ( -0.6823417656250003738, 13.40104166700806232, 1.181850606188754593 ) ) ;
#209204 = CARTESIAN_POINT ( 'NONE',  ( 3.428187820690358656, -2.188011084934568196, 0.3830038565930964367 ) ) ;
#209205 = ORIENTED_EDGE ( 'NONE', *, *, #75095, .T. ) ;
#209206 = CARTESIAN_POINT ( 'NONE',  ( 1.836970198721030181E-16, 13.49999999999999822, 1.500000000000000222 ) ) ;
#209207 = CARTESIAN_POINT ( 'NONE',  ( 6.740374924288304648, 11.01552117831172062, 1.040834085586084257E-14 ) ) ;
#209208 = CARTESIAN_POINT ( 'NONE',  ( -0.6823417656250003738, -1.032291666325242607, -1.181850606188749264 ) ) ;
#209210 = EDGE_CURVE ( 'NONE', #204176, #157195, #127409, .T. ) ;
#209209 = CARTESIAN_POINT ( 'NONE',  ( 4.211346380768822506, -1.629847038978438079, -1.091715234301626314 ) ) ;
#209212 = CARTESIAN_POINT ( 'NONE',  ( -5.409340102172518705, 9.254721185935849803, 0.000000000000000000 ) ) ;
#209211 = CARTESIAN_POINT ( 'NONE',  ( 2.822068529938852155, 6.444163718237301275, -0.7998128361456291469 ) ) ;
#209213 = CARTESIAN_POINT ( 'NONE',  ( -1.378881877344206197, 4.087185210396952151, 0.5904953584336783967 ) ) ;
#209214 = CARTESIAN_POINT ( 'NONE',  ( 5.272873185648853323, -2.127775705341850898, -0.7691360568998426572 ) ) ;
#209215 = CARTESIAN_POINT ( 'NONE',  ( 2.049356628244120682, 1.795697342706262578, -1.014786283375568976 ) ) ;
#209216 = CARTESIAN_POINT ( 'NONE',  ( -5.371001409308059138, 9.417918744168066070, -0.7998128361456231517 ) ) ;
#209217 = ORIENTED_EDGE ( 'NONE', *, *, #179732, .F. ) ;
#209218 = CARTESIAN_POINT ( 'NONE',  ( -1.500000000000013101, 1.910416667349488451, -0.8660254037844313801 ) ) ;
#209219 = CARTESIAN_POINT ( 'NONE',  ( 3.321420150926617687, -1.803644938814071175, 0.4956094624995326381 ) ) ;
#209220 = CARTESIAN_POINT ( 'NONE',  ( 2.285452750267936484, 1.391693986029099772, -1.034342955966370603 ) ) ;
#209221 = CARTESIAN_POINT ( 'NONE',  ( 6.321842903100939104, 1.263506803105146847, -1.790488031206059372 ) ) ;
#209222 = CARTESIAN_POINT ( 'NONE',  ( 0.8334014933106950185, 0.1641056870149599223, 2.200712145998296343 ) ) ;
#209223 = CARTESIAN_POINT ( 'NONE',  ( 3.889662759143839299, 1.564074849111227516, 1.492423382767386730 ) ) ;
#209224 = CARTESIAN_POINT ( 'NONE',  ( 5.208904604407663008, -0.2832176519766657630, 1.921071368630644649 ) ) ;
#209225 = CARTESIAN_POINT ( 'NONE',  ( 0.3124999997796079620, 1.451031294483781764, 1.451031289061110341 ) ) ;
#209226 = CARTESIAN_POINT ( 'NONE',  ( 1.250000000000033973, 8.500000000000000000, 9.921567416492207414 ) ) ;
#209227 = SURFACE_STYLE_USAGE ( .BOTH. , #174654 ) ;
#209228 = CARTESIAN_POINT ( 'NONE',  ( -1.360316468749997565, 2.890625000341401574, 1.734723475976807094E-15 ) ) ;
#209229 = CARTESIAN_POINT ( 'NONE',  ( 5.344375030997434273, 0.3906003880304632636, -1.978050218768567792 ) ) ;
#209230 = CARTESIAN_POINT ( 'NONE',  ( -8.154339323615371171, 11.60081407993821045, 1.199719254218453823 ) ) ;
#209231 = CARTESIAN_POINT ( 'NONE',  ( 7.633404179693907388, 8.864391950186421454, -1.199719254218441611 ) ) ;
#209232 = CARTESIAN_POINT ( 'NONE',  ( 1.387358672531703974, 7.315968950352358391, 4.254625267140708544 ) ) ;
#209233 = CARTESIAN_POINT ( 'NONE',  ( 3.369579884941567016, 1.780956498284639533, -0.4009276245297774266 ) ) ;
#209234 = CARTESIAN_POINT ( 'NONE',  ( 2.046200460737709559, 0.8445575735530999051, -2.038961412367201298 ) ) ;
#209235 = ORIENTED_EDGE ( 'NONE', *, *, #135294, .F. ) ;
#209236 = CARTESIAN_POINT ( 'NONE',  ( -4.624739795592943459, 6.488892076315448065, -1.443375672974066548 ) ) ;
#209237 = UNCERTAINTY_MEASURE_WITH_UNIT (LENGTH_MEASURE( 1.000000000000000082E-05 ), #94356, 'distance_accuracy_value', 'NONE');
#209238 = CARTESIAN_POINT ( 'NONE',  ( 3.285556943749998737, -1.742708332855374076, -1.896917185911906500 ) ) ;
#209239 = CARTESIAN_POINT ( 'NONE',  ( -8.290974629956718189, 9.631557475493025322, -1.199719254218446718 ) ) ;
#209240 = CARTESIAN_POINT ( 'NONE',  ( 0.7209703750307445702, 1.526537956607315172, -1.322641891180293516 ) ) ;
#209241 = CARTESIAN_POINT ( 'NONE',  ( 1.453939175038564624, -1.538220317728825393, -1.459821603020584613 ) ) ;
#209242 = CARTESIAN_POINT ( 'NONE',  ( 0.9999999999999833467, 8.600000000000013856, -0.3999999999999832023 ) ) ;
#209243 = CARTESIAN_POINT ( 'NONE',  ( -5.098748287191073203, 8.106234214101666780, 1.199719254218452935 ) ) ;
#209244 = CARTESIAN_POINT ( 'NONE',  ( 1.867776877072557129, -1.847639373886921677, 0.2213648055933575276 ) ) ;
#209245 = CARTESIAN_POINT ( 'NONE',  ( 4.355193658487811703, 6.104145239700998538, -1.599625672291255185 ) ) ;
#209246 = CARTESIAN_POINT ( 'NONE',  ( 1.323354039402934390, -0.05256100377049736927, 2.161234000603563299 ) ) ;
#209247 = CARTESIAN_POINT ( 'NONE',  ( 6.100232455412330168, -0.2440331339308223768, 2.001510902166554473 ) ) ;
#209248 = ORIENTED_EDGE ( 'NONE', *, *, #80635, .F. ) ;
#209249 = ORIENTED_EDGE ( 'NONE', *, *, #73875, .F. ) ;
#209250 =( BOUNDED_CURVE ( )  B_SPLINE_CURVE ( 2, ( #63818, #214284, #201259, #82191, #185016, #200196, #52899 ),
 .UNSPECIFIED., .F., .T. ) 
 B_SPLINE_CURVE_WITH_KNOTS ( ( 3, 2, 2, 3 ),
 ( 0.1071428571428572341, 0.1130952380952381098, 0.1190476190476189855, 0.1249999999999998612 ),
 .UNSPECIFIED. ) 
 CURVE ( )  GEOMETRIC_REPRESENTATION_ITEM ( )  RATIONAL_B_SPLINE_CURVE ( ( 0.9999999999999977796, 0.8660254037844409281, 1.000000000000000000, 0.8660254037844387076, 1.000000000000000000, 0.8660254037844418162, 0.9999999999999968914 ) ) 
 REPRESENTATION_ITEM ( '' )  );
#209251 = CARTESIAN_POINT ( 'NONE',  ( -10.13488352141530768, 11.78278451552804817, 1.199719254218462483 ) ) ;
#209252 = CARTESIAN_POINT ( 'NONE',  ( 3.809063337113669068, 1.566667275063510445, 0.9371452329686791316 ) ) ;
#209254 = CARTESIAN_POINT ( 'NONE',  ( -5.989290089449875509, 6.089315518664643712, -0.6934025848366349720 ) ) ;
#209253 = CARTESIAN_POINT ( 'NONE',  ( -4.281342646865346602, 8.216926531310035031, 0.7998128361456352531 ) ) ;
#209255 = CARTESIAN_POINT ( 'NONE',  ( 6.562153376633583335, 6.794832157118596783, -0.3727171428496069971 ) ) ;
#209256 = CARTESIAN_POINT ( 'NONE',  ( 6.098982473628085543, 0.9961464269193781584, -1.752763620266280187 ) ) ;
#209257 = CARTESIAN_POINT ( 'NONE',  ( 5.929618730664214077, 0.9035273275350870215, -1.604119651413847603 ) ) ;
#209258 = CARTESIAN_POINT ( 'NONE',  ( -10.99970480893081692, -5.740513804456437441, -0.08058608058607553970 ) ) ;
#209259 = CARTESIAN_POINT ( 'NONE',  ( 4.266487514486948740, 1.085833288323118095, 2.036285375418740884 ) ) ;
#209260 = CARTESIAN_POINT ( 'NONE',  ( 6.690022453700429139, 6.769724048930809701, 0.7998128361456331437 ) ) ;
#209261 = CARTESIAN_POINT ( 'NONE',  ( 6.432923066502826082, 0.2047513753351773436, 2.151863363619124225 ) ) ;
#209262 = CARTESIAN_POINT ( 'NONE',  ( 2.718228044968384882, 1.829540209339441503, 0.6518440813585175686 ) ) ;
#209263 = CARTESIAN_POINT ( 'NONE',  ( 4.798391170199634459, -2.103835099937763964, 0.9258070857356412997 ) ) ;
#209264 = DIRECTION ( 'NONE',  ( 0.8660254037844385966, 0.5000000000000001110, 0.000000000000000000 ) ) ;
#209266 = CIRCLE ( 'NONE', #143626, 0.08000000000000025147 ) ;
#209265 = CARTESIAN_POINT ( 'NONE',  ( -7.923814432544069142, 8.209148024248356990, 0.000000000000000000 ) ) ;
#209267 = CARTESIAN_POINT ( 'NONE',  ( 4.504681594071535677, 1.446009304718363087, -1.186774495104812699 ) ) ;
#209268 = ORIENTED_EDGE ( 'NONE', *, *, #77102, .F. ) ;
#209269 = AXIS2_PLACEMENT_3D ( 'NONE', #151333, #152391, #23436 ) ;
#209272 = CARTESIAN_POINT ( 'NONE',  ( -5.418418667316934112, 6.350518529071726981, -1.199719254218453823 ) ) ;
#209271 = CARTESIAN_POINT ( 'NONE',  ( -0.7500000000000215383, 0.4729166673494850093, 1.299038105676659116 ) ) ;
#209270 = CARTESIAN_POINT ( 'NONE',  ( 2.865378420500460876, -1.565876230000915692, -1.097592462808501645 ) ) ;
#209273 = CARTESIAN_POINT ( 'NONE',  ( 3.879664727460280904, 2.078262106501146622, -0.7427522710690689367 ) ) ;
#209274 = CARTESIAN_POINT ( 'NONE',  ( 6.983263157960363010, 3.696136926403908340, 2.460428995873820579 ) ) ;
#209275 = CARTESIAN_POINT ( 'NONE',  ( 5.872089928050205465, 6.023395468912922546, -0.7216878364870458196 ) ) ;
#209276 = CARTESIAN_POINT ( 'NONE',  ( -5.600926855776888758, 7.627776979863398310, -1.443375672974066548 ) ) ;
#209277 = CARTESIAN_POINT ( 'NONE',  ( 1.581257511629934775, 1.823016439315219062, -0.7507060404894276839 ) ) ;
#209278 = CARTESIAN_POINT ( 'NONE',  ( 1.747554699363640607, -1.948627443588932806, 1.235768562340158194 ) ) ;
#209279 = CARTESIAN_POINT ( 'NONE',  ( 2.471086628630547288, 1.751123931924388089, 0.8847596551376719631 ) ) ;
#209280 = FACE_OUTER_BOUND ( 'NONE', #104319, .T. ) ;
#209281 = CARTESIAN_POINT ( 'NONE',  ( 5.946154108440814490, -0.9325515945646453142, 1.839819606017919718 ) ) ;
#209282 = CARTESIAN_POINT ( 'NONE',  ( 2.724825686666657809, 6.122787701178987518, 0.000000000000000000 ) ) ;
#209283 = CARTESIAN_POINT ( 'NONE',  ( 4.100796195634116792, 1.845626398921360822, 0.8128187495666516771 ) ) ;
#209284 = CARTESIAN_POINT ( 'NONE',  ( 4.960304097753311936, 6.880383762169266504, 1.599625672291268286 ) ) ;
#209285 = ORIENTED_EDGE ( 'NONE', *, *, #125435, .F. ) ;
#209286 = CARTESIAN_POINT ( 'NONE',  ( -8.839026081105473054, 12.39961529701003684, -1.199719254218446718 ) ) ;
#209287 = CARTESIAN_POINT ( 'NONE',  ( -11.14389002924298566, 7.220603907090449525, 3.549113525960188031 ) ) ;
#209288 = CARTESIAN_POINT ( 'NONE',  ( 10.42352117080803708, 11.05519620889787724, -0.7998128361456281477 ) ) ;
#209289 = CARTESIAN_POINT ( 'NONE',  ( 2.377987901236592982, -2.106814941015792808, 0.5239127008311114109 ) ) ;
#209290 = CARTESIAN_POINT ( 'NONE',  ( -0.7158994178059416846, 2.800000000000024691, 1.161830092591057184 ) ) ;
#209291 = CARTESIAN_POINT ( 'NONE',  ( -3.099846755496448392, 14.55179011166401892, -11.55524956803910008 ) ) ;
#209292 = LINE ( 'NONE', #145440, #15075 ) ;
#209293 = CARTESIAN_POINT ( 'NONE',  ( 2.987410616422137455, 1.320145714686842497, 1.325460448179466066 ) ) ;
#209294 = CARTESIAN_POINT ( 'NONE',  ( 6.837200347746461127, -1.934230338078479772, 0.9651617863762137484 ) ) ;
#209296 = CARTESIAN_POINT ( 'NONE',  ( 6.727182134110198497, 4.703735537933666500, 2.273690654489219032 ) ) ;
#209295 = DIRECTION ( 'NONE',  ( -1.000000000000000000, 0.000000000000000000, 0.000000000000000000 ) ) ;
#209297 = CARTESIAN_POINT ( 'NONE',  ( -0.6823417656249969321, 5.780208333674756283, -1.181850606188749264 ) ) ;
#209298 = CARTESIAN_POINT ( 'NONE',  ( -1.408835580989212355, 3.462626791720190944, 0.5203893312692456918 ) ) ;
#209299 = CARTESIAN_POINT ( 'NONE',  ( 1.699719973799845185, 1.319605273547658220, 1.384218846220357291 ) ) ;
#209300 = CARTESIAN_POINT ( 'NONE',  ( 3.819032205515503708, -0.1302183858614604506, 1.765120429581680916 ) ) ;
#209301 = VECTOR ( 'NONE', #59127, 1000.000000000000114 ) ;
#209302 = CARTESIAN_POINT ( 'NONE',  ( 1.330556988563241561, 1.283596529665396169, -1.417643162000304935 ) ) ;
#209303 = CARTESIAN_POINT ( 'NONE',  ( -5.687809136132860210, 6.594531066031826150, -1.199719254218446718 ) ) ;
#209305 = CARTESIAN_POINT ( 'NONE',  ( 6.380494711820015930, -0.5163536399260219012, -1.844617532318414632 ) ) ;
#209304 =( NAMED_UNIT ( * ) SI_UNIT ( $, .STERADIAN. ) SOLID_ANGLE_UNIT ( ) );
#209306 = CARTESIAN_POINT ( 'NONE',  ( -1.500000000000015099, -0.5791666666666476226, 0.8660254037844403729 ) ) ;
#209307 = CARTESIAN_POINT ( 'NONE',  ( 0.7310241076574041097, -1.948878508384953356, -0.6990896207654460071 ) ) ;
#209308 = CARTESIAN_POINT ( 'NONE',  ( -1.500000000000011324, 5.879166666666686858, -0.8660254037844313801 ) ) ;
#209309 = CARTESIAN_POINT ( 'NONE',  ( 3.855102659575539548, 8.506872032340217160, -2.500000000000707878 ) ) ;
#209310 = CARTESIAN_POINT ( 'NONE',  ( 5.084763247618332649, -0.2297073032716222263, -1.856415652357709778 ) ) ;
#209311 = CARTESIAN_POINT ( 'NONE',  ( 1.576486190600217663, -1.733098801405801304, -0.5742540608338757568 ) ) ;
#209313 = CARTESIAN_POINT ( 'NONE',  ( 5.067666882003905471, 7.850148838107081417, 1.122879199148843377 ) ) ;
#209312 = CARTESIAN_POINT ( 'NONE',  ( 5.268293329372571776, 1.085216321637239023, 1.921556908365213312 ) ) ;
#209314 = CARTESIAN_POINT ( 'NONE',  ( 0.6823417656249899377, 5.738541667008087543, -1.181850606188754593 ) ) ;
#209315 = CARTESIAN_POINT ( 'NONE',  ( 2.594246270321644676, 0.9746516854327008650, -1.817902028900773459 ) ) ;
#209316 = CARTESIAN_POINT ( 'NONE',  ( -7.934546212495630968, 10.28005655271014795, -1.599625672291263179 ) ) ;
#209317 = CARTESIAN_POINT ( 'NONE',  ( 8.540746701604824409, 12.05162268759261224, -1.199719254218446718 ) ) ;
#209318 = CARTESIAN_POINT ( 'NONE',  ( 1.390311220213875876, 3.551797531149446296, -0.5641062960582096109 ) ) ;
#209319 = TOROIDAL_SURFACE ( 'NONE', #46709, 0.8299999999999999600, 0.08000000000000000167 ) ;
#209320 = CARTESIAN_POINT ( 'NONE',  ( 5.020262018810099924, 9.078999131912302900, 0.7998128361456331437 ) ) ;
#209321 = ORIENTED_EDGE ( 'NONE', *, *, #91462, .F. ) ;
#209322 = CARTESIAN_POINT ( 'NONE',  ( 5.582505937350194181, 1.236201877336528643, -1.660625051266072960 ) ) ;
#209323 = CARTESIAN_POINT ( 'NONE',  ( -1.364683531250014514, -0.4489583329919089039, -0.7879004041258359514 ) ) ;
#209324 = CARTESIAN_POINT ( 'NONE',  ( 2.337400524717429207, -1.931973293601353392, 0.9696072025056484689 ) ) ;
#209325 = CARTESIAN_POINT ( 'NONE',  ( -4.613315975161869531, 8.372148359400446438, -0.1986654441144524719 ) ) ;
#209326 = CARTESIAN_POINT ( 'NONE',  ( 2.772133559515827184, 2.009754670806723098, -0.2000300323863890006 ) ) ;
#209327 = CARTESIAN_POINT ( 'NONE',  ( 7.725699985795420055, -5.832912386296867702, 7.725699985795402291 ) ) ;
#209328 = VERTEX_POINT ( 'NONE', #27214 ) ;
#209331 = CARTESIAN_POINT ( 'NONE',  ( 6.466876084038451822, 10.48851316477946582, 1.040834085586084257E-14 ) ) ;
#209330 = CARTESIAN_POINT ( 'NONE',  ( 1.737500000000001155, -1.283333333333334325, 3.009438278150922130 ) ) ;
#209329 = CARTESIAN_POINT ( 'NONE',  ( 1.499999999999989120, 3.785416667349481123, 0.8660254037844522523 ) ) ;
#209332 = CARTESIAN_POINT ( 'NONE',  ( -8.093291352714894415, 8.406871097780989288, -0.7998128361456362523 ) ) ;
#209333 = CARTESIAN_POINT ( 'NONE',  ( 1.833220611596135363, -1.622487599052296670, -1.197302888167578683 ) ) ;
#209335 = CARTESIAN_POINT ( 'NONE',  ( 6.480031355044912900, -2.148842909532014289, -0.4297212958329286736 ) ) ;
#209334 = CARTESIAN_POINT ( 'NONE',  ( -6.078132937628113908, 5.985576603521232109, 1.040834085586084257E-14 ) ) ;
#209336 = CARTESIAN_POINT ( 'NONE',  ( 1.499999999999989120, 5.327083334016152527, -0.8660254037844323793 ) ) ;
#209337 = CARTESIAN_POINT ( 'NONE',  ( 4.394721148579957770, -1.856311205515799090, -0.4593126252911488572 ) ) ;
#209338 = CARTESIAN_POINT ( 'NONE',  ( -4.223528545856940042, 4.886203710709899006, -1.199719254218446718 ) ) ;
#209339 = EDGE_CURVE ( 'NONE', #195013, #127020, #57596, .T. ) ;
#209340 = CARTESIAN_POINT ( 'NONE',  ( 5.463572716182812705, 9.317992568947877530, 0.7216878364870438212 ) ) ;
#209342 = CARTESIAN_POINT ( 'NONE',  ( 3.480092364642515701, -2.014234743589532695, -0.09611699103692641910 ) ) ;
#209341 = CARTESIAN_POINT ( 'NONE',  ( -7.646435447983039424, 11.86466575604815787, 0.000000000000000000 ) ) ;
#209343 = CARTESIAN_POINT ( 'NONE',  ( 1.364683531249996529, 13.77604166700806765, 0.7879004041258405033 ) ) ;
#209344 = CARTESIAN_POINT ( 'NONE',  ( -7.075376061485238566, 9.347967719856493218, 1.599625672291269396 ) ) ;
#209345 = CARTESIAN_POINT ( 'NONE',  ( 4.787984082328099689, -0.8109719804370466578, 1.522229471167990233 ) ) ;
#209346 = CARTESIAN_POINT ( 'NONE',  ( 7.537407054554579489, 7.758339416593960536, 0.000000000000000000 ) ) ;
#209347 = CARTESIAN_POINT ( 'NONE',  ( 10.41229878561526512, 11.25002945941372623, -0.7216878364870257245 ) ) ;
#209348 = CARTESIAN_POINT ( 'NONE',  ( -1.001543065824772872E-14, 4.712500000000018119, 1.732050807568877637 ) ) ;
#209349 = CARTESIAN_POINT ( 'NONE',  ( 3.989402248074361612, 1.353031944225962624, 1.291829963354161892 ) ) ;
#209350 = CARTESIAN_POINT ( 'NONE',  ( 2.535011536075336913, 5.133042487381361596, 0.9999999999999991118 ) ) ;
#209351 = CARTESIAN_POINT ( 'NONE',  ( 1.569279613544020568, 1.823957739939351619, 0.9794188589333228112 ) ) ;
#209352 = CARTESIAN_POINT ( 'NONE',  ( -6.392587740394328755, -6.532648833121157850, -6.999862025036979851 ) ) ;
#209353 = ORIENTED_EDGE ( 'NONE', *, *, #59450, .T. ) ;
#209355 = B_SPLINE_CURVE_WITH_KNOTS ( 'NONE', 3,
 ( #8388, #122245, #39841, #75535, #109175, #10518 ),
 .UNSPECIFIED., .F., .F.,
 ( 4, 2, 4 ),
 ( 0.000000000000000000, 0.0003168911866439334617, 0.0006337823732878669234 ),
 .UNSPECIFIED. ) ;
#209354 = CARTESIAN_POINT ( 'NONE',  ( 6.287769681992382509, 1.731225344711059266, -0.5331814487182000573 ) ) ;
#209356 = CARTESIAN_POINT ( 'NONE',  ( 4.634908411025333130, 6.500755460986618495, 1.599625672291268286 ) ) ;
#209357 = CARTESIAN_POINT ( 'NONE',  ( -4.559605246071192219, 3.300000000000025135, -0.7749999999999935829 ) ) ;
#209358 = CARTESIAN_POINT ( 'NONE',  ( -0.1056357528139931640, -1.757099710744941312, -0.4406103525058014392 ) ) ;
#209359 = CARTESIAN_POINT ( 'NONE',  ( 4.367134876933267407, 8.109091433148536865, 0.000000000000000000 ) ) ;
#209360 = CARTESIAN_POINT ( 'NONE',  ( 9.605809254248283580, 12.70095519382022964, -7.195141037656365590 ) ) ;
#209361 = CARTESIAN_POINT ( 'NONE',  ( 2.625153213768507854, -2.044362554934661791, 0.7897752707372793779 ) ) ;
#209362 = ORIENTED_EDGE ( 'NONE', *, *, #98529, .T. ) ;
#209364 = CARTESIAN_POINT ( 'NONE',  ( 10.07778825365955733, 10.65184113889131012, -0.7998128361456281477 ) ) ;
#209363 = CARTESIAN_POINT ( 'NONE',  ( 0.4847190467827041105, 1.876267867961832980, 0.5731238010058882226 ) ) ;
#209365 =( GEOMETRIC_REPRESENTATION_CONTEXT ( 3 ) GLOBAL_UNCERTAINTY_ASSIGNED_CONTEXT ( ( #146936 ) ) GLOBAL_UNIT_ASSIGNED_CONTEXT ( ( #179971, #150677, #97668 ) ) REPRESENTATION_CONTEXT ( 'NONE', 'WORKASPACE' ) );
#209366 = CARTESIAN_POINT ( 'NONE',  ( 5.413669558995096054, -1.219043080348445329, -1.477637860945772763 ) ) ;
#209367 = DIRECTION ( 'NONE',  ( 5.578564026256490882E-16, 1.000000000000000000, 9.066213480720158442E-32 ) ) ;
#209368 = CARTESIAN_POINT ( 'NONE',  ( -5.394899524673852476, 7.567224757263017132, 1.245178244268474010 ) ) ;
#209369 = EDGE_CURVE ( 'NONE', #152913, #149077, #143157, .T. ) ;
#209370 = PLANE ( 'NONE',  #188103 ) ;
#209371 = CARTESIAN_POINT ( 'NONE',  ( -1.402160292154681736E-14, 0.3218750003414227456, 1.575800808251672791 ) ) ;
#209373 = ORIENTED_EDGE ( 'NONE', *, *, #111378, .T. ) ;
#209372 = CARTESIAN_POINT ( 'NONE',  ( 6.480434237652135998, 6.662854153456708950, 0.7216878364870317197 ) ) ;
#209374 = CARTESIAN_POINT ( 'NONE',  ( -7.849807752632384172, 12.10193344480572897, 0.000000000000000000 ) ) ;
#209375 = CARTESIAN_POINT ( 'NONE',  ( 1.393688021309073433, 1.637156065531343740, 1.411701162175371893 ) ) ;
#209376 = CARTESIAN_POINT ( 'NONE',  ( -4.014095998097799267, 6.840806543492835345, -1.199719254218450271 ) ) ;
#209377 = CARTESIAN_POINT ( 'NONE',  ( 7.404161286838808920, 8.771181268467660885, -1.082531754730548412 ) ) ;
#209378 = CARTESIAN_POINT ( 'NONE',  ( -3.358669367883384105, 4.941533567329135401, -1.599625672291262513 ) ) ;
#209379 = CARTESIAN_POINT ( 'NONE',  ( 4.717693524642503355, -1.790169364231732674, 0.3569235582787863570 ) ) ;
#209380 = CARTESIAN_POINT ( 'NONE',  ( 11.84405005182567727, 6.745048178605705935, -3.657409634699734458 ) ) ;
#209381 = CARTESIAN_POINT ( 'NONE',  ( 1.001173315506132422, 1.609201512179364135, 1.138472824994830379 ) ) ;
#209382 = CARTESIAN_POINT ( 'NONE',  ( 3.129067941553372645, 1.730785544086024696, 0.8136490247460312908 ) ) ;
#209383 = EDGE_LOOP ( 'NONE', ( #3363, #81426, #120328, #38864 ) ) ;
#209384 = CARTESIAN_POINT ( 'NONE',  ( 3.807052887859848855, -1.611515334864065840, 1.132039114057415308 ) ) ;
#209385 = VERTEX_POINT ( 'NONE', #105297 ) ;
#209386 = CARTESIAN_POINT ( 'NONE',  ( 5.899939537456503125, -0.7029524595547633758, -1.810543181819963321 ) ) ;
#209387 = EDGE_LOOP ( 'NONE', ( #104656, #170175, #148991, #84994, #196223 ) ) ;
#209388 = CARTESIAN_POINT ( 'NONE',  ( -6.017840079619296567, 8.114175741012878973, -1.599625672291271394 ) ) ;
#209390 = CARTESIAN_POINT ( 'NONE',  ( -1.510657702057710340E-15, 1.375000000682792267, 1.224999999999963229 ) ) ;
#209389 = CARTESIAN_POINT ( 'NONE',  ( -6.134138155540168391, 6.121192367743780949, 0.000000000000000000 ) ) ;
#209391 = CARTESIAN_POINT ( 'NONE',  ( 6.170369307550816806, 9.252495721234380355, 1.082531754730549967 ) ) ;
#209392 = CARTESIAN_POINT ( 'NONE',  ( 4.301352856729808494, 1.706663192164651122, -0.8627939227693476321 ) ) ;
#209393 = CARTESIAN_POINT ( 'NONE',  ( 5.018332763094478288, 6.785885375482345161, -1.424093192218821136 ) ) ;
#209394 = CARTESIAN_POINT ( 'NONE',  ( -9.488025208946957889, -6.683951901172175525, 0.1062647697984211714 ) ) ;
#209395 = CARTESIAN_POINT ( 'NONE',  ( 0.4999999999999674705, 3.999999999999989786, 0.4499999999999625966 ) ) ;
#209396 = CARTESIAN_POINT ( 'NONE',  ( 5.215494488825547670, 1.647103507230001096, 1.157162265453457239 ) ) ;
#209397 = CARTESIAN_POINT ( 'NONE',  ( 0.5475226324602644468, 7.495867147881389414, 1.923617955668152302 ) ) ;
#209399 = CARTESIAN_POINT ( 'NONE',  ( 5.647672796105281279, 1.985869605424210649, -0.3494789899042491932 ) ) ;
#209398 = CARTESIAN_POINT ( 'NONE',  ( 6.217409598193539999, -0.2183660865492654257, 1.812524795094340835 ) ) ;
#209400 = CARTESIAN_POINT ( 'NONE',  ( 2.014207461368537455, 2.064961549741591185, -0.1501100615294431728 ) ) ;
#209401 = CARTESIAN_POINT ( 'NONE',  ( -7.158341918335454857, 10.33485409049125003, 1.082531754730549967 ) ) ;
#209402 = CARTESIAN_POINT ( 'NONE',  ( -5.479780979625591186, 7.495630219063617261, -1.250153324542001343 ) ) ;
#209403 = CARTESIAN_POINT ( 'NONE',  ( 9.427850895902817996, 13.54474674066948481, 7.423989997610750180 ) ) ;
#209404 = CARTESIAN_POINT ( 'NONE',  ( -15.75000000000000000, 13.79999999999998295, 1.799999999999999600 ) ) ;
#209405 = CARTESIAN_POINT ( 'NONE',  ( 7.233438648090761980, 8.397765496649418182, 1.199719254218462483 ) ) ;
#209406 = CARTESIAN_POINT ( 'NONE',  ( 3.891353782322113375, 4.498666486585943147, -1.199719254218446718 ) ) ;
#209407 = CARTESIAN_POINT ( 'NONE',  ( -0.6823417656250003738, 12.21354166700806765, 1.181850606188754593 ) ) ;
#209408 = CARTESIAN_POINT ( 'NONE',  ( -5.434120640978981065, 5.234228924097238611, -0.7998128361456221525 ) ) ;
#209410 = CARTESIAN_POINT ( 'NONE',  ( -7.228432174741334038, 8.462200954400218578, -1.199719254218452047 ) ) ;
#209409 = CARTESIAN_POINT ( 'NONE',  ( -11.94650005372637835, 11.15102700337638097, -1.135399707157295435 ) ) ;
#209412 = CARTESIAN_POINT ( 'NONE',  ( 3.902719751800659775, -0.8955246652143248332, -1.484863070527132622 ) ) ;
#209411 = VECTOR ( 'NONE', #126987, 1000.000000000000000 ) ;
#209413 = CARTESIAN_POINT ( 'NONE',  ( -4.253507506385335368, 5.985511395581417204, 1.599625672291267398 ) ) ;
#209414 = CARTESIAN_POINT ( 'NONE',  ( 1.393514648303464165, -1.873246724434135313, 0.8816542684770898308 ) ) ;
#209415 = CARTESIAN_POINT ( 'NONE',  ( 2.952857568058687043, -1.957288919824872186, -0.8077276291160383481 ) ) ;
#209416 = CARTESIAN_POINT ( 'NONE',  ( 4.222474775652216294, 7.013638773981186958, 1.199719254218462483 ) ) ;
#209417 = AXIS2_PLACEMENT_3D ( 'NONE', #114650, #29072, #11736 ) ;
#209418 = CARTESIAN_POINT ( 'NONE',  ( 9.101601193475611140, 9.512956235343358102, -0.7998128361456221525 ) ) ;
#209419 = CARTESIAN_POINT ( 'NONE',  ( 0.1007326007325878847, -9.919999999999998153, 10.99953876047308476 ) ) ;
#209420 = CARTESIAN_POINT ( 'NONE',  ( 0.6902129346560643697, 1.017158767820530940, -1.686321398027894825 ) ) ;
#209421 = CARTESIAN_POINT ( 'NONE',  ( 4.100400566228236343, 7.694619998084524681, 0.6794913885044724378 ) ) ;
#209422 = CARTESIAN_POINT ( 'NONE',  ( 3.362058906508953449, 6.866226457661676719, -0.7216878364870267237 ) ) ;
#209424 = DIRECTION ( 'NONE',  ( 1.276756478318932585E-15, -1.000000000000000000, 1.665334536937738262E-16 ) ) ;
#209423 = CARTESIAN_POINT ( 'NONE',  ( 1.737499999999999378, -2.216666666666665453, -3.009438278150925683 ) ) ;
#209425 = CARTESIAN_POINT ( 'NONE',  ( 3.258078344973667662, 1.030780755083884115, 2.047500790377681845 ) ) ;
#209426 = CARTESIAN_POINT ( 'NONE',  ( 0.1526014871912773629, -1.468541917219987836, 1.084465738218153064 ) ) ;
#209427 = CARTESIAN_POINT ( 'NONE',  ( 3.568532368641282648, 0.6928216322696268969, 1.782650395559831180 ) ) ;
#209428 = CARTESIAN_POINT ( 'NONE',  ( 5.505492895601038938, 8.580769590579979678, -1.199719254218452047 ) ) ;
#209429 = CARTESIAN_POINT ( 'NONE',  ( 5.626270559546804328, 9.507806719539201978, 0.7216878364870438212 ) ) ;
#209430 = CARTESIAN_POINT ( 'NONE',  ( -9.657485491635913633, 10.16148791653038330, 1.040834085586084257E-14 ) ) ;
#209431 =( BOUNDED_CURVE ( )  B_SPLINE_CURVE ( 2, ( #64994, #180890, #131148, #195020, #163595, #149462, #30400, #147344, #150542 ),
 .UNSPECIFIED., .F., .T. ) 
 B_SPLINE_CURVE_WITH_KNOTS ( ( 3, 2, 2, 2, 3 ),
 ( 0.9017857142857143016, 0.9047619047619047672, 0.9107142857142856984, 0.9166666666666666297, 0.9196428571428570953 ),
 .UNSPECIFIED. ) 
 CURVE ( )  GEOMETRIC_REPRESENTATION_ITEM ( )  RATIONAL_B_SPLINE_CURVE ( ( 0.9330127018922194093, 0.9330127018922194093, 1.000000000000000000, 0.8660254037844387076, 1.000000000000000000, 0.8660254037844387076, 1.000000000000000000, 0.9330127018922206306, 0.9330127018922194093 ) ) 
 REPRESENTATION_ITEM ( '' )  );
#209432 = CARTESIAN_POINT ( 'NONE',  ( 1.793228464370033581, -0.1031022715946017104, -2.010704963445380411 ) ) ;
#209433 = CARTESIAN_POINT ( 'NONE',  ( 1.797631089865757259, -1.417250949620936895, -1.356651810197152086 ) ) ;
#209434 = CARTESIAN_POINT ( 'NONE',  ( -8.809047120577080392, 11.30030761213851953, 1.599625672291269396 ) ) ;
#209435 = CARTESIAN_POINT ( 'NONE',  ( -5.540478329478883524, 9.615641817700700145, 0.000000000000000000 ) ) ;
#209436 = CARTESIAN_POINT ( 'NONE',  ( -5.721177634842498527, 5.777054783512106440, 0.000000000000000000 ) ) ;
#209438 = CARTESIAN_POINT ( 'NONE',  ( 3.783871084116468886, -0.8724064270978303393, 1.539809854060821603 ) ) ;
#209437 = CARTESIAN_POINT ( 'NONE',  ( 5.419903170966573924, 1.246048553727102659, -1.678571210107776324 ) ) ;
#209439 = CARTESIAN_POINT ( 'NONE',  ( 0.7124089920922619390, 15.00000000000000355, 12.66466791154580207 ) ) ;
#209441 = CARTESIAN_POINT ( 'NONE',  ( 6.017577161850602430, -1.268579900078286471, -1.909058160655076053 ) ) ;
#209440 = DIRECTION ( 'NONE',  ( 0.000000000000000000, 0.000000000000000000, -1.000000000000000000 ) ) ;
#209442 = CARTESIAN_POINT ( 'NONE',  ( 5.437372246358883388, 0.6999822053482355200, -1.593550356025658976 ) ) ;
#209443 = CARTESIAN_POINT ( 'NONE',  ( 8.263858322729371153, 9.599921783727809910, -1.199719254218446718 ) ) ;
#209444 = CARTESIAN_POINT ( 'NONE',  ( 10.50000000000000178, 12.69999999999998153, 3.599999999999999201 ) ) ;
#209445 = CARTESIAN_POINT ( 'NONE',  ( 4.340949964944015527, -0.9985633389030469376, 1.417159075928013046 ) ) ;
#209446 = CARTESIAN_POINT ( 'NONE',  ( 6.039545795398320926, 2.008403840061912859, -0.8252953610491889913 ) ) ;
#209447 = FACE_OUTER_BOUND ( 'NONE', #83192, .T. ) ;
#209448 = CARTESIAN_POINT ( 'NONE',  ( 0.4271636869729276698, -1.812546591343185298, 1.094284096637233583 ) ) ;
#209450 = MECHANICAL_DESIGN_GEOMETRIC_PRESENTATION_REPRESENTATION (  '', ( #29523 ), #192139 ) ;
#209449 = CARTESIAN_POINT ( 'NONE',  ( 5.687500000000004441, -1.451031289060884077, 1.451031289061342378 ) ) ;
#209451 = CARTESIAN_POINT ( 'NONE',  ( 11.04536101718726293, 10.19999999999999929, -1.100000000000000311 ) ) ;
#209452 = CARTESIAN_POINT ( 'NONE',  ( 2.995051018759773420, 1.652986441767102743, -0.9890191681132395329 ) ) ;
#209453 = CARTESIAN_POINT ( 'NONE',  ( -1.500000000000001110, 10.80208333401613352, 0.8660254037844419273 ) ) ;
#209454 = CARTESIAN_POINT ( 'NONE',  ( 0.2413015266095243083, 2.127564327900688390, 0.6385326005407893080 ) ) ;
#209455 = ORIENTED_EDGE ( 'NONE', *, *, #176534, .T. ) ;
#209456 = CARTESIAN_POINT ( 'NONE',  ( -0.1409997244346122836, 0.7174646053854060179, -2.082770303449644977 ) ) ;
#209457 = CARTESIAN_POINT ( 'NONE',  ( 0.7499999999999885647, 2.566666666666689522, -1.299038105676658228 ) ) ;
#209458 = CARTESIAN_POINT ( 'NONE',  ( 5.961834861707224320, 7.978559976790334574, -1.599625672291262513 ) ) ;
#209459 = CARTESIAN_POINT ( 'NONE',  ( 3.035994277891720827, -2.140246456218936721, 0.5942984311890684435 ) ) ;
#209460 = EDGE_CURVE ( 'NONE', #158934, #45871, #123268, .T. ) ;
#209461 = CARTESIAN_POINT ( 'NONE',  ( 7.131225611108088280, 9.342849184424693476, 1.443375672974076540 ) ) ;
#209462 = CARTESIAN_POINT ( 'NONE',  ( -9.124274191872631334, 12.62844174295135069, -1.082531754730543083 ) ) ;
#209463 = CARTESIAN_POINT ( 'NONE',  ( 4.309512724297349884, 6.121127159803966933, 1.599625672291261402 ) ) ;
#209464 = AXIS2_PLACEMENT_3D ( 'NONE', #71385, #55168, #187287 ) ;
#209465 = CARTESIAN_POINT ( 'NONE',  ( 0.7740648250077889481, 1.777010169924503558, -0.9530137779002674225 ) ) ;
#209467 = CARTESIAN_POINT ( 'NONE',  ( 5.389153705970353592, 0.1484172631736270231, 2.057380146747369576 ) ) ;
#209466 = CARTESIAN_POINT ( 'NONE',  ( 10.07778825365955733, 10.65184113889131012, -0.7998128361456281477 ) ) ;
#209468 = DIRECTION ( 'NONE',  ( -0.05872483221476459958, -0.000000000000000000, -0.9982742078614211811 ) ) ;
#209469 = LINE ( 'NONE', #93636, #51206 ) ;
#209470 = FILL_AREA_STYLE ('',( #6993 ) ) ;
#209471 = CARTESIAN_POINT ( 'NONE',  ( 1.364683531249986537, 0.6135416670080880985, 0.7879004041258500513 ) ) ;
#209472 = CARTESIAN_POINT ( 'NONE',  ( 0.5789240690485557561, 1.654349777479852346, -0.6291145533634836529 ) ) ;
#209473 = CARTESIAN_POINT ( 'NONE',  ( 6.258463337875916466, 1.656396116010181219, -0.5134576769376431038 ) ) ;
#209474 = CARTESIAN_POINT ( 'NONE',  ( 5.724081574600810463, 1.679587015112851578, 0.4559996917168698261 ) ) ;
#209475 = CARTESIAN_POINT ( 'NONE',  ( 3.333774467322860868, 1.029290431845871989, -2.048349661755991313 ) ) ;
#209476 = CARTESIAN_POINT ( 'NONE',  ( -0.6823417656250246877, -0.9489583329919115684, 1.181850606188755259 ) ) ;
#209477 = CARTESIAN_POINT ( 'NONE',  ( 1.851249556194194179, 1.836288347861175785, -0.1344999175661651392 ) ) ;
#209478 = AXIS2_PLACEMENT_3D ( 'NONE', #163932, #198522, #84793 ) ;
#209479 = CARTESIAN_POINT ( 'NONE',  ( 8.561083932025322696, 12.07534945641652158, -1.199719254218446718 ) ) ;
#209480 = DIRECTION ( 'NONE',  ( -0.000000000000000000, 1.000000000000000000, 1.804652791718263484E-16 ) ) ;
#209481 = CARTESIAN_POINT ( 'NONE',  ( 1.852308540880560850, 0.5694407911355814367, 1.734573797025913189 ) ) ;
#209482 = CARTESIAN_POINT ( 'NONE',  ( 3.164685561777963230, 1.281361203394768111, 1.556908733426412450 ) ) ;
#209483 = CARTESIAN_POINT ( 'NONE',  ( -2.751941993449643409, 6.154423392425789174, 0.7216878364870317197 ) ) ;
#209484 = CARTESIAN_POINT ( 'NONE',  ( -4.038971567461725698, 3.986455684509185193, -0.5169845646830102392 ) ) ;
#209485 = CARTESIAN_POINT ( 'NONE',  ( 4.489357033980984291, 1.882333632172785487, -0.9445240646021864084 ) ) ;
#209486 = CARTESIAN_POINT ( 'NONE',  ( -5.228640796364566690, 9.251831362400652736, -0.7998128361456231517 ) ) ;
#209487 = CARTESIAN_POINT ( 'NONE',  ( 7.207828345953949167, 14.97151529443900486, 9.191422221725781938 ) ) ;
#209488 = CARTESIAN_POINT ( 'NONE',  ( 2.506376218629560171, 2.069854378281150709, 0.05321039126485183068 ) ) ;
#209489 = CARTESIAN_POINT ( 'NONE',  ( 3.032219910950674890, 6.689340329417765574, 0.7998128361456321445 ) ) ;
#209490 = CARTESIAN_POINT ( 'NONE',  ( -0.6801582343750438575, 0.7135416670080579893, 1.178068619123810334 ) ) ;
#209491 = CARTESIAN_POINT ( 'NONE',  ( 4.512424090126602394, -2.120028616272570332, -0.05109941365945279423 ) ) ;
#209492 = CARTESIAN_POINT ( 'NONE',  ( 6.639283661800273961, -1.628176093627232479, 0.8261057939347238310 ) ) ;
#209493 = VERTEX_POINT ( 'NONE', #106394 ) ;
#209494 = CARTESIAN_POINT ( 'NONE',  ( -3.494969737272722643, 7.299491470118629088, -0.7998128361456481317 ) ) ;
#209495 = B_SPLINE_CURVE_WITH_KNOTS ( 'NONE', 3,
 ( #58492, #75806, #89948, #144057, #107305, #155998, #57425, #123587, #189551, #41198, #91013, #141914, #33452 ),
 .UNSPECIFIED., .F., .F.,
 ( 4, 3, 3, 3, 4 ),
 ( -1.794875635996206868E-06, 0.000000000000000000, 4.049120399957791379E-05, 8.114731789401420019E-05, 0.0001124919062838589578 ),
 .UNSPECIFIED. ) ;
#209496 = CARTESIAN_POINT ( 'NONE',  ( 10.24726517383036928, 10.84956421242393887, 0.000000000000000000 ) ) ;
#209497 = CARTESIAN_POINT ( 'NONE',  ( 4.380693030546905398, 8.124909279031149012, 0.7216878364870247253 ) ) ;
#209498 = CARTESIAN_POINT ( 'NONE',  ( 1.737499999999999378, -1.472916665710751527, -3.009438278150925683 ) ) ;
#209499 = CARTESIAN_POINT ( 'NONE',  ( -4.232116505760120440, 8.089219690028791376, -0.7998128361456281477 ) ) ;
#209500 = CARTESIAN_POINT ( 'NONE',  ( 6.310795917644286490, -0.5669512758468171487, -2.043305014803979525 ) ) ;
#209501 = CARTESIAN_POINT ( 'NONE',  ( 1.395691461817370804, 1.594359505120213960, 1.375974583626845993 ) ) ;
#209502 = CARTESIAN_POINT ( 'NONE',  ( -4.118644803501354978, 8.027112380718707030, 0.7998128361456352531 ) ) ;
#209503 = CARTESIAN_POINT ( 'NONE',  ( 9.915090410295563927, 10.46202698829998567, -0.7998128361456281477 ) ) ;
#209504 = CARTESIAN_POINT ( 'NONE',  ( 5.946130789595732935, -0.8379359121385165921, 1.661726607698276181 ) ) ;
#209505 = CARTESIAN_POINT ( 'NONE',  ( 6.564118927310645724, 10.80988918183778225, -0.7998128361456291469 ) ) ;
#209506 = LINE ( 'NONE', #95810, #98900 ) ;
#209507 = CARTESIAN_POINT ( 'NONE',  ( -7.946487431385463651, 8.443525889470736345, 0.7216878364870317197 ) ) ;
#209508 = CARTESIAN_POINT ( 'NONE',  ( -10.31739171031960822, 11.13930453823545186, 1.040834085586084257E-14 ) ) ;
#209509 = CARTESIAN_POINT ( 'NONE',  ( 5.398914348987485567, 6.259949555863199677, 2.499999999999999556 ) ) ;
#209510 = CARTESIAN_POINT ( 'NONE',  ( 0.9657642407454472000, -4.140281660848636136, 0.3272472668956626918 ) ) ;
#209512 = CARTESIAN_POINT ( 'NONE',  ( 2.629291921057617554, 0.09916324773191761976, -1.959495597191794225 ) ) ;
#209511 = CARTESIAN_POINT ( 'NONE',  ( -7.867809214632013770, 8.073532260025807261, 1.040834085586084257E-14 ) ) ;
#209513 = CARTESIAN_POINT ( 'NONE',  ( 1.340939272977889951, 0.4221563536682856332, 2.119910705745978508 ) ) ;
#209515 = CARTESIAN_POINT ( 'NONE',  ( -6.137326611691442224, 5.996379759157309586, -0.05818935505210766357 ) ) ;
#209514 = CARTESIAN_POINT ( 'NONE',  ( -4.664887371553763096, 7.600063145858131364, -1.199719254218453823 ) ) ;
#209517 = EDGE_CURVE ( 'NONE', #64456, #76056, #130794, .T. ) ;
#209516 = CARTESIAN_POINT ( 'NONE',  ( 0.6823417656249899377, 1.342708333674752508, 1.181850606188755259 ) ) ;
#209518 = CARTESIAN_POINT ( 'NONE',  ( 2.758840240711700531, -1.728971274941538017, -0.1308756186972348801 ) ) ;
#209519 = CARTESIAN_POINT ( 'NONE',  ( 1.939017046771335240, 0.6676067653633214194, -1.607389671016548949 ) ) ;
#209520 = CARTESIAN_POINT ( 'NONE',  ( 7.456621297836078632, 8.762108271306003004, 1.082531754730558626 ) ) ;
#209521 = CARTESIAN_POINT ( 'NONE',  ( -10.50660484223216606, 5.359830900411396648, 5.105327592218940502 ) ) ;
#209522 = CARTESIAN_POINT ( 'NONE',  ( 2.442732317853496760, 1.238130588059358717, 1.591075322344523535 ) ) ;
#209523 = CARTESIAN_POINT ( 'NONE',  ( 6.925078400183557470, 1.239878965558613322, 2.257517960274835200 ) ) ;
#209524 = CARTESIAN_POINT ( 'NONE',  ( -4.659162064951642535, 5.464719159645540003, 1.199719254218452935 ) ) ;
#209525 = CARTESIAN_POINT ( 'NONE',  ( 1.200003858469798956, -1.971640592295399896, -0.002163809803111190443 ) ) ;
#209526 = EDGE_CURVE ( 'NONE', #183272, #12932, #208047, .T. ) ;
#209528 = CARTESIAN_POINT ( 'NONE',  ( -6.183927461608886844, 7.347575139032721303, 1.082531754730548412 ) ) ;
#209527 = CARTESIAN_POINT ( 'NONE',  ( 5.502191098127390489, -0.8541586074963626318, 1.711093258865265643 ) ) ;
#209529 = CARTESIAN_POINT ( 'NONE',  ( -6.427974226210522168, 6.671927150099951298, 0.000000000000000000 ) ) ;
#209530 = CARTESIAN_POINT ( 'NONE',  ( 6.886615681098613884, 6.999082814228660077, 0.000000000000000000 ) ) ;
#209531 = CARTESIAN_POINT ( 'NONE',  ( -7.456058132872594335, 7.663432341298296535, 0.000000000000000000 ) ) ;
#209532 = CARTESIAN_POINT ( 'NONE',  ( 1.031905740238812097, -1.969920897724128483, 0.4447463068311637846 ) ) ;
#209533 = CARTESIAN_POINT ( 'NONE',  ( -1.734723475976807094E-15, 2.999999999999988898, -6.938893903907228378E-15 ) ) ;
#209534 = CARTESIAN_POINT ( 'NONE',  ( 5.825286519090714599, -0.06434016213947668650, 2.306860349555530654 ) ) ;
#209535 = CARTESIAN_POINT ( 'NONE',  ( 5.476992472119650124, 1.812042599547862176, 0.7524171098330989516 ) ) ;
#209536 = CARTESIAN_POINT ( 'NONE',  ( 3.520314338623427020, 0.8779579967637550775, 1.754372790864023646 ) ) ;
#209537 = CARTESIAN_POINT ( 'NONE',  ( 8.585337585951586803, 11.03931315507545108, -1.599625672291255185 ) ) ;
#209538 = CARTESIAN_POINT ( 'NONE',  ( -9.333041836230021815, 14.55305236562984383, 7.472413793098204415 ) ) ;
#209539 = ORIENTED_EDGE ( 'NONE', *, *, #102049, .T. ) ;
#209540 = CARTESIAN_POINT ( 'NONE',  ( 0.6907973960054912821, 1.599150545848356364, -1.387813827701115610 ) ) ;
#209542 = CARTESIAN_POINT ( 'NONE',  ( -7.212047647465563038, 10.50147379109678880, -1.199719254218446718 ) ) ;
#209541 = CARTESIAN_POINT ( 'NONE',  ( -3.113568832632681360, 6.784247404713427798, -0.7998128361456281477 ) ) ;
#209543 = CARTESIAN_POINT ( 'NONE',  ( 1.517261703430743625, -1.021610662766696764, -1.531488883528262290 ) ) ;
#209544 = ORIENTED_EDGE ( 'NONE', *, *, #148219, .F. ) ;
#209545 = CARTESIAN_POINT ( 'NONE',  ( 10.80604400872368132, 9.580061684330026139, -5.115041846163436823 ) ) ;
#209546 = CARTESIAN_POINT ( 'NONE',  ( 3.234745892528373634, 1.342314639517484087, -1.641720766639111817 ) ) ;
#209547 = CARTESIAN_POINT ( 'NONE',  ( -1.500000000000011324, 4.202083334016156080, 0.8660254037844403729 ) ) ;
#209548 = CARTESIAN_POINT ( 'NONE',  ( 8.263858322729371153, 9.599921783727809910, -1.199719254218446718 ) ) ;
#209549 = CARTESIAN_POINT ( 'NONE',  ( -0.3282377607281335985, 2.613835450998162280, 1.224999999999989431 ) ) ;
#209550 = CARTESIAN_POINT ( 'NONE',  ( 3.497389175668437211, 1.622225323665491326, 1.270757995044344391 ) ) ;
#209552 = CARTESIAN_POINT ( 'NONE',  ( 0.7844012160764175512, 1.623964078452419857, -0.8677550623670119423 ) ) ;
#209551 = CARTESIAN_POINT ( 'NONE',  ( -6.906989191158078079, 10.14557225873805812, -1.199719254218440723 ) ) ;
#209553 = CARTESIAN_POINT ( 'NONE',  ( -1.201851678989727383E-14, 4.071875000341425022, 1.575800808251672791 ) ) ;
#209554 = CARTESIAN_POINT ( 'NONE',  ( -0.02244404828160087226, 6.946777552644228138, -2.784171975256703124 ) ) ;
#209555 = CARTESIAN_POINT ( 'NONE',  ( 1.422919657202426968, 3.901887307304316987, 0.5004438751493111015 ) ) ;
#209556 = CARTESIAN_POINT ( 'NONE',  ( 0.3642759247451561322, 2.182245240920151375, -0.3280614795862640820 ) ) ;
#209557 = CARTESIAN_POINT ( 'NONE',  ( 2.987861924072153563, 1.597690390425403173, 1.602079265715735223 ) ) ;
#209558 = CARTESIAN_POINT ( 'NONE',  ( -9.246297574839990929, 11.81043314211192019, 1.443375672974076540 ) ) ;
#209559 = CARTESIAN_POINT ( 'NONE',  ( 2.408236768384981019, -1.806978867004911171, -0.1295660047265032311 ) ) ;
#209560 = CARTESIAN_POINT ( 'NONE',  ( 3.063600739116902449, 1.219304168433880564, 1.477546071989847665 ) ) ;
#209561 = CARTESIAN_POINT ( 'NONE',  ( 4.281733463571851139, -1.982135700070002615, 0.5980053909793592304 ) ) ;
#209562 = CARTESIAN_POINT ( 'NONE',  ( -1.364683531250012516, 3.092708333674755838, 0.7879004041258379498 ) ) ;
#209563 = CARTESIAN_POINT ( 'NONE',  ( 1.657037912627358001, -1.689797944177928279, -1.015304737199155483 ) ) ;
#209564 = CARTESIAN_POINT ( 'NONE',  ( 0.3758376374219556393, 1.106279473776916378, 1.576890456013874120 ) ) ;
#209565 = CARTESIAN_POINT ( 'NONE',  ( 3.291731440620565330, -0.7593194595177065187, 1.709801165022284408 ) ) ;
#209567 = CARTESIAN_POINT ( 'NONE',  ( 4.666526410304530970, 8.402211131567142388, 0.5382107299411863499 ) ) ;
#209566 = CARTESIAN_POINT ( 'NONE',  ( 2.842713172187049331, 2.290369893530233902, 0.2817356681584815004 ) ) ;
#209568 = CARTESIAN_POINT ( 'NONE',  ( 2.558860573628952473, 1.496680913221506870, -1.105902276818030217 ) ) ;
#209569 = CARTESIAN_POINT ( 'NONE',  ( -1.201851678989727383E-14, 2.321875000341416584, 1.575800808251672791 ) ) ;
#209570 = VECTOR ( 'NONE', #142435, 1000.000000000000000 ) ;
#209571 = CARTESIAN_POINT ( 'NONE',  ( 0.2392226684038156193, -0.1392734953599965297, -2.030321344557210139 ) ) ;
#209572 = CARTESIAN_POINT ( 'NONE',  ( -3.737243898861318137, 7.511868315313511069, 0.7998128361456341429 ) ) ;
#209573 = CARTESIAN_POINT ( 'NONE',  ( 5.126954644262057492, 9.133197518281081173, 0.7998128361456462443 ) ) ;
#209574 = CARTESIAN_POINT ( 'NONE',  ( -1.494964465105841578, 3.364977991896605847, -0.1399972980471414497 ) ) ;
#209575 = CARTESIAN_POINT ( 'NONE',  ( 6.264693295067493395, -1.491911088229242788, 1.486630704232002609 ) ) ;
#209576 = CIRCLE ( 'NONE', #206034, 3.432849766368862632 ) ;
#209577 = CARTESIAN_POINT ( 'NONE',  ( -1.364683531249997417, 3.571875000341423245, 1.214306433183764966E-14 ) ) ;
#209578 = CARTESIAN_POINT ( 'NONE',  ( 5.589210384452774960, 1.909260796540311000, -1.013481389624170115 ) ) ;
#209579 = CARTESIAN_POINT ( 'NONE',  ( 6.633471379370169174, -0.1512203817595116073, 1.986116118494333227 ) ) ;
#209580 = CARTESIAN_POINT ( 'NONE',  ( -1.402160292154681736E-14, -0.8031249996585825279, -1.575800808251665908 ) ) ;
#209581 = CARTESIAN_POINT ( 'NONE',  ( -5.151735183512911043, 6.073074471262228435, 1.082531754730548412 ) ) ;
#209584 = CARTESIAN_POINT ( 'NONE',  ( 4.026408433578586354, 7.641300905909586660, 1.040834085586084257E-14 ) ) ;
#209583 = CARTESIAN_POINT ( 'NONE',  ( 6.825078400183553384, 4.701740280048592346, 2.318362489372997270 ) ) ;
#209582 = CARTESIAN_POINT ( 'NONE',  ( 5.176180785367283654, 9.260904359562321275, -0.7998128361456481317 ) ) ;
#209585 = CARTESIAN_POINT ( 'NONE',  ( -2.993318053567081360, 6.714231172462041819, 0.000000000000000000 ) ) ;
#209586 = CARTESIAN_POINT ( 'NONE',  ( 4.610564714392807240, 1.931124171932835809, 0.5807562064495259690 ) ) ;
#209587 = CARTESIAN_POINT ( 'NONE',  ( -6.665805079413154921, 10.92852302595736447, 0.7998128361456481317 ) ) ;
#209589 = CARTESIAN_POINT ( 'NONE',  ( -6.739811759324828344, 8.956476034002674780, -1.443375672974066548 ) ) ;
#209588 = CARTESIAN_POINT ( 'NONE',  ( -9.002250809794006159, 10.56534270192358704, -1.082531754730543971 ) ) ;
#209590 = CARTESIAN_POINT ( 'NONE',  ( -1.500000000000031530, 4.920833333333354709, 0.8660254037844287156 ) ) ;
#209592 = CARTESIAN_POINT ( 'NONE',  ( 1.364683531250000748, 9.255208333674733723, -0.7879004041258355073 ) ) ;
#209591 = CARTESIAN_POINT ( 'NONE',  ( 6.121977807712331909, -1.196819783530624015, -1.799967629666970881 ) ) ;
#209593 = CARTESIAN_POINT ( 'NONE',  ( -1.734723475976807094E-15, 2.999999999999988898, -6.938893903907228378E-15 ) ) ;
#209594 = CARTESIAN_POINT ( 'NONE',  ( -9.378489572351046633, 11.96465713920816043, -1.599625672291263179 ) ) ;
#209595 = EDGE_CURVE ( 'NONE', #155131, #108029, #23551, .T. ) ;
#209597 = CARTESIAN_POINT ( 'NONE',  ( 6.591432905763006111, -0.4393008961055907546, 1.975236973087670656 ) ) ;
#209596 = CARTESIAN_POINT ( 'NONE',  ( -6.900736999231456004, 8.113576589600553390, 1.082531754730549967 ) ) ;
#209598 = CARTESIAN_POINT ( 'NONE',  ( -0.6823417656250003738, 0.2802083336747515641, -1.181850606188749264 ) ) ;
#209599 = CARTESIAN_POINT ( 'NONE',  ( 6.589320575229281829, 7.629137130509070275, 2.703262396134015866 ) ) ;
#209600 = CARTESIAN_POINT ( 'NONE',  ( 1.892754278755165664, 1.501794282950255965, -0.8482797957840328973 ) ) ;
#209601 = CARTESIAN_POINT ( 'NONE',  ( 4.543917759235442944, 5.330267469643351852, 1.199719254218452935 ) ) ;
#209602 = CARTESIAN_POINT ( 'NONE',  ( 5.936491157937257235, 8.019268665717216749, 1.599625672291268286 ) ) ;
#209603 = CARTESIAN_POINT ( 'NONE',  ( -11.76006714841412837, 8.561852472810636883, -2.403998662577486733 ) ) ;
#209604 = CARTESIAN_POINT ( 'NONE',  ( 1.018396826474694761, 1.632260513341069252, 0.6844030214382245125 ) ) ;
#209605 = CARTESIAN_POINT ( 'NONE',  ( 1.541653539051958122, -1.894817064119158401, 0.6801782934461576557 ) ) ;
#209606 = CARTESIAN_POINT ( 'NONE',  ( -0.4041367621137820221, 3.038026290190013690, -0.4210133165200504179 ) ) ;
#209608 = AXIS2_PLACEMENT_3D ( 'NONE', #130806, #143834, #28974 ) ;
#209607 = CARTESIAN_POINT ( 'NONE',  ( 3.821466819111440927, -0.1649144712266135959, 2.200675313789305143 ) ) ;
#209609 = CARTESIAN_POINT ( 'NONE',  ( 5.278266929526361118, -1.155484533919543422, -1.837868763204909994 ) ) ;
#209610 = ORIENTED_EDGE ( 'NONE', *, *, #178698, .T. ) ;
#209611 = CARTESIAN_POINT ( 'NONE',  ( 0.7499999999999867883, -0.4333333333333133641, -1.299038105676652899 ) ) ;
#209612 = CARTESIAN_POINT ( 'NONE',  ( 7.239690839573049708, 11.39013037956983965, 1.040834085586084257E-14 ) ) ;
#209613 = B_SPLINE_CURVE_WITH_KNOTS ( 'NONE', 3,
 ( #54189, #186305, #185233, #104014, #53116, #2200, #200413, #152752, #120329, #18471 ),
 .UNSPECIFIED., .F., .F.,
 ( 4, 3, 3, 4 ),
 ( 0.000000000000000000, 8.893179197954797545E-05, 0.0001334007970840207931, 0.0001778705873658964021 ),
 .UNSPECIFIED. ) ;
#209615 = CARTESIAN_POINT ( 'NONE',  ( 3.321888824615967906, 0.9040932542298124597, -1.802426844439278142 ) ) ;
#209614 = CARTESIAN_POINT ( 'NONE',  ( 3.369896858953733698, 0.5134250039646214292, -2.057278921464212207 ) ) ;
#209617 = VERTEX_POINT ( 'NONE', #191839 ) ;
#209616 = CARTESIAN_POINT ( 'NONE',  ( 3.005918303229858424, -0.7299923727487073188, 1.658169170237313583 ) ) ;
#209618 = CARTESIAN_POINT ( 'NONE',  ( 6.062430963966053632, 7.101866208495718702, -1.199719254218452047 ) ) ;
#209619 = VERTEX_POINT ( 'NONE', #171333 ) ;
#209620 = CARTESIAN_POINT ( 'NONE',  ( -1.500000000000022204, 8.627523663848661428, 2.580000000000011173 ) ) ;
#209621 = CARTESIAN_POINT ( 'NONE',  ( 5.473741331615251227, 7.409117525016355010, -1.599625672291262513 ) ) ;
#209622 = VECTOR ( 'NONE', #156973, 1000.000000000000000 ) ;
#209623 = CARTESIAN_POINT ( 'NONE',  ( 6.445924739416000193, 0.6936395621829589686, -1.688995215704327313 ) ) ;
#209625 = CARTESIAN_POINT ( 'NONE',  ( 1.780357001937494799, -0.5149467098792412934, -1.845104466984174962 ) ) ;
#209624 = CARTESIAN_POINT ( 'NONE',  ( -4.765854690403601879, 5.518917546014321829, 1.199719254218462483 ) ) ;
#209626 = DIRECTION ( 'NONE',  ( -0.000000000000000000, -1.000000000000000000, 0.000000000000000000 ) ) ;
#209627 = CARTESIAN_POINT ( 'NONE',  ( -4.889337272013151825, 4.909234758358784312, -0.4031905389056227307 ) ) ;
#209628 = CARTESIAN_POINT ( 'NONE',  ( -0.6823417656250003738, 1.030208333674752286, -1.181850606188749264 ) ) ;
#209629 = CARTESIAN_POINT ( 'NONE',  ( 11.86145016429272836, 13.40000000000000036, -1.180000000000002158 ) ) ;
#209630 = CARTESIAN_POINT ( 'NONE',  ( -8.779068160048691283, 10.20099992726700933, -1.199719254218446718 ) ) ;
#209631 = VECTOR ( 'NONE', #47197, 1000.000000000000000 ) ;
#209632 = CARTESIAN_POINT ( 'NONE',  ( 5.084929678302337663, -0.2608814864752464491, -2.145832476913120068 ) ) ;
#209633 = CARTESIAN_POINT ( 'NONE',  ( -4.014622883422322985, 7.697827440719083647, -0.7216878364870458196 ) ) ;
#209634 = CARTESIAN_POINT ( 'NONE',  ( -6.720001414228860881, 7.869031733802326123, -1.199719254218452047 ) ) ;
#209635 = CARTESIAN_POINT ( 'NONE',  ( 2.918346969001627045, -2.117983955170518851, 0.1081942149789016649 ) ) ;
#209637 = CARTESIAN_POINT ( 'NONE',  ( -12.45759369916135029, 8.320971494343229580, 2.471636155840711169 ) ) ;
#209636 = CARTESIAN_POINT ( 'NONE',  ( -0.1298852118744256712, 0.2531197755418754247, -1.761387242530809250 ) ) ;
#209638 = CARTESIAN_POINT ( 'NONE',  ( 4.780523264075623224, -1.911459794658072697, -0.4817293046612564633 ) ) ;
#209639 = CARTESIAN_POINT ( 'NONE',  ( 6.310809538426106258, -0.5167911955388967415, -1.841158844219364044 ) ) ;
#209640 = ORIENTED_EDGE ( 'NONE', *, *, #50263, .T. ) ;
#209641 = CARTESIAN_POINT ( 'NONE',  ( 5.841034576552271318, -1.817201478619561383, -1.086431860386444681 ) ) ;
#209642 = CARTESIAN_POINT ( 'NONE',  ( 6.183927461164522299, 6.387205924212962849, 0.000000000000000000 ) ) ;
#209643 = CARTESIAN_POINT ( 'NONE',  ( 6.777801591175982132, -1.910752814866881089, 0.4773036857264860156 ) ) ;
#209644 = CARTESIAN_POINT ( 'NONE',  ( 2.519391418834667995, -1.118305101016278558, -1.587446049422422956 ) ) ;
#209645 = ORIENTED_EDGE ( 'NONE', *, *, #191183, .T. ) ;
#209646 = CARTESIAN_POINT ( 'NONE',  ( -3.902768115887413014, 5.646591783325653147, -1.599625672291283607 ) ) ;
#209647 = CARTESIAN_POINT ( 'NONE',  ( 5.501576472095266901, 9.640532660744973725, -0.7998128361456481317 ) ) ;
#209649 = CARTESIAN_POINT ( 'NONE',  ( 4.659198344590585350, 8.587481835331020719, 0.7998128361456462443 ) ) ;
#209648 = CARTESIAN_POINT ( 'NONE',  ( 3.134800171978794125, -1.843606372480216082, 0.9858348089602610997 ) ) ;
#209650 = CARTESIAN_POINT ( 'NONE',  ( 4.543390873910913896, 5.433615786718446472, 1.082531754730549078 ) ) ;
#209652 = VERTEX_POINT ( 'NONE', #43502 ) ;
#209651 = CARTESIAN_POINT ( 'NONE',  ( 0.08225775502835978858, -1.185065876811146834, 1.370160863432666076 ) ) ;
#209653 = CARTESIAN_POINT ( 'NONE',  ( 5.707716145626243964, -0.5396369327701348029, 2.139774205771049154 ) ) ;
#209654 = DIRECTION ( 'NONE',  ( -1.000000000000000000, 7.771561172376097755E-16, 4.440892098500627148E-16 ) ) ;
#209655 = CARTESIAN_POINT ( 'NONE',  ( 3.575398329460587554, 0.05639400328332971890, -2.206221599391814170 ) ) ;
#209656 = CARTESIAN_POINT ( 'NONE',  ( 7.099665995050449041, 11.43469409420089455, 0.7998128361456462443 ) ) ;
#209657 = DIRECTION ( 'NONE',  ( 0.000000000000000000, -1.000000000000000000, 0.000000000000000000 ) ) ;
#209658 = CARTESIAN_POINT ( 'NONE',  ( 1.875505643822904300, 0.3255412885708880433, -1.884197853084010443 ) ) ;
#209659 = CARTESIAN_POINT ( 'NONE',  ( 8.910733272679570049, 11.41894145625809820, -1.599625672291255185 ) ) ;
#209660 = CARTESIAN_POINT ( 'NONE',  ( 5.248515149483166553, -2.054309126314420642, -0.2569322651706855143 ) ) ;
#209662 = CARTESIAN_POINT ( 'NONE',  ( 3.415052781332720055, 1.953485055394106107, 0.9259690932504063277 ) ) ;
#209661 = CARTESIAN_POINT ( 'NONE',  ( 1.525408907393396740, 8.692885148323941991, -2.521481920632477447 ) ) ;
#209663 = CARTESIAN_POINT ( 'NONE',  ( 4.335597073515660149, 0.9364531651635084053, -1.981528385891350386 ) ) ;
#209664 = ORIENTED_EDGE ( 'NONE', *, *, #10396, .F. ) ;
#209665 = DIRECTION ( 'NONE',  ( 2.949029909160572061E-17, 1.000000000000000000, -8.673600428462503284E-15 ) ) ;
#209666 = CARTESIAN_POINT ( 'NONE',  ( -3.097867176628829133E-14, 3.975067388631681187, -1.872309607372827811 ) ) ;
#209667 = CARTESIAN_POINT ( 'NONE',  ( -0.1368715580176214641, 8.236096389523126504, 2.000481929432245121 ) ) ;
#209668 = CARTESIAN_POINT ( 'NONE',  ( 5.899733120602060232, 6.912052057904395141, -1.199719254218452047 ) ) ;
#209669 = CARTESIAN_POINT ( 'NONE',  ( 3.285556943750000070, -2.821874999522043570, 0.000000000000000000 ) ) ;
#209670 = DIRECTION ( 'NONE',  ( 0.000000000000000000, 0.000000000000000000, 1.000000000000000000 ) ) ;
#209671 = CARTESIAN_POINT ( 'NONE',  ( 0.6158615555539399544, 0.1511424999406512648, 2.010826230049263863 ) ) ;
#209672 = CARTESIAN_POINT ( 'NONE',  ( -8.026063749610047537, 11.34719622697832264, -1.082531754730543971 ) ) ;
#209673 = CARTESIAN_POINT ( 'NONE',  ( 5.845500506147374153, 6.848780674373954547, 1.199719254218453823 ) ) ;
#209674 = CARTESIAN_POINT ( 'NONE',  ( 4.135645376760338721, 1.951069878921590783, -0.6927527371542248069 ) ) ;
#209675 = CARTESIAN_POINT ( 'NONE',  ( 4.195867187722844172, -0.7361232629885716694, 1.780507395703424978 ) ) ;
#209676 = CARTESIAN_POINT ( 'NONE',  ( -0.0003749349099593791675, -1.976945657698804704, 0.3961262320883383592 ) ) ;
#209677 = CARTESIAN_POINT ( 'NONE',  ( -1.040834085586084257E-14, -7.242250812739412957, 9.811039896441885233 ) ) ;
#209678 = CARTESIAN_POINT ( 'NONE',  ( 5.229694566569264680, 7.124396299129368337, 1.599625672291267398 ) ) ;
#209679 = DIRECTION ( 'NONE',  ( 0.000000000000000000, 0.000000000000000000, -1.000000000000000000 ) ) ;
#209680 = CARTESIAN_POINT ( 'NONE',  ( 4.170725306337518923, 1.395817779951594950, -1.389658704579323611 ) ) ;
#209681 = CARTESIAN_POINT ( 'NONE',  ( 0.1467655724766807612, -1.757430454515636509, 1.308964887167405111 ) ) ;
#209682 = CARTESIAN_POINT ( 'NONE',  ( 3.562960707638890501, -1.610701098693729350, -0.8595150645765645692 ) ) ;
#209683 = PRODUCT_DEFINITION_SHAPE ( 'NONE', 'NONE',  #214422 ) ;
#209684 = CARTESIAN_POINT ( 'NONE',  ( 5.994113311017540191, 9.046863725278862844, -1.082531754730548412 ) ) ;
#209685 = CARTESIAN_POINT ( 'NONE',  ( 3.456965981360264895, 6.016582164020185530, -1.082531754730543971 ) ) ;
#209686 = CARTESIAN_POINT ( 'NONE',  ( -5.420227550413282636, 9.545625585449309725, 0.7998128361456291469 ) ) ;
#209687 = CARTESIAN_POINT ( 'NONE',  ( 4.634908411025333130, 6.500755460986618495, 1.599625672291268286 ) ) ;
#209688 = EDGE_LOOP ( 'NONE', ( #102227, #72173, #30328, #172142, #21807 ) ) ;
#209690 = CARTESIAN_POINT ( 'NONE',  ( 5.133069374350656133, 1.861756548879553996, 0.7665277172332859434 ) ) ;
#209689 = CARTESIAN_POINT ( 'NONE',  ( 1.399689850468607277, -0.6632477835330424787, -1.717811453623831808 ) ) ;
#209691 = CARTESIAN_POINT ( 'NONE',  ( 0.5448069426677571991, 2.143542105210020754, -0.8297726512136813781 ) ) ;
#209692 = CARTESIAN_POINT ( 'NONE',  ( 5.049637047142223167, 1.450995767963231264, 1.320413740667214508 ) ) ;
#209693 = CARTESIAN_POINT ( 'NONE',  ( -6.067437437315529536, 7.037430750744921859, 1.199719254218450271 ) ) ;
#209694 = CARTESIAN_POINT ( 'NONE',  ( 0.3999999999999889200, 0.000000000000000000, -5.204170427930421283E-15 ) ) ;
#209695 = AXIS2_PLACEMENT_3D ( 'NONE', #102804, #140404, #26608 ) ;
#209696 = CARTESIAN_POINT ( 'NONE',  ( -3.273404022695637572, 5.906389562198459231, 1.199719254218462483 ) ) ;
#209697 = CARTESIAN_POINT ( 'NONE',  ( -3.461074353238556167, 7.259946855412102273, 0.000000000000000000 ) ) ;
#209699 = CARTESIAN_POINT ( 'NONE',  ( 6.561408083364261401, 0.2975169865880605835, -1.744492507556465011 ) ) ;
#209698 = CARTESIAN_POINT ( 'NONE',  ( 1.452797965663179314, -1.794991982752047965, -1.071751678227941929 ) ) ;
#209700 = CARTESIAN_POINT ( 'NONE',  ( 0.08635228504285741291, 7.011029804986336877, -1.999717945518301399 ) ) ;
#209701 = CARTESIAN_POINT ( 'NONE',  ( -0.1102773484824119132, -0.006951161900758253548, -2.203378182130751206 ) ) ;
#209702 = CARTESIAN_POINT ( 'NONE',  ( 1.540153114873343609, -1.470452955542918660, 0.9307524122482965234 ) ) ;
#209703 = CARTESIAN_POINT ( 'NONE',  ( 5.636439174979242850, 7.598931675607687453, -1.599625672291262513 ) ) ;
#209705 = CARTESIAN_POINT ( 'NONE',  ( 1.567642296063686658, 8.684662666223690763, 2.500960217906281535 ) ) ;
#209704 = DIRECTION ( 'NONE',  ( -0.6929666359396602360, 0.000000000000000000, 0.7209696536432518288 ) ) ;
#209706 = CARTESIAN_POINT ( 'NONE',  ( 1.927930615940620873, 0.9947386370207593753, -1.408936266059911624 ) ) ;
#209707 = CARTESIAN_POINT ( 'NONE',  ( 2.191216702865448784, 1.696344223602393786, 1.387594652289561248 ) ) ;
#209708 = CARTESIAN_POINT ( 'NONE',  ( 4.371826309796801979, 2.140994599346605742, -0.5347268394074317088 ) ) ;
#209709 = CARTESIAN_POINT ( 'NONE',  ( -10.81809272050965376, 3.158133435639066899, -6.646723133134004868 ) ) ;
#209710 = CARTESIAN_POINT ( 'NONE',  ( 2.342849523213458962, -2.128499089237919417, -0.4270345827348878132 ) ) ;
#209711 = CARTESIAN_POINT ( 'NONE',  ( 1.541335573940459058, -1.321205422867760548, -1.260230113935792318 ) ) ;
#209712 = CARTESIAN_POINT ( 'NONE',  ( 3.854788253679425125, -1.977088355604763148, -0.7582873983895296321 ) ) ;
#209713 = CARTESIAN_POINT ( 'NONE',  ( 6.639320575229254118, 4.698690022235154196, 2.459427960261594492 ) ) ;
#209714 = EDGE_CURVE ( 'NONE', #31219, #214357, #37320, .T. ) ;
#209715 = ORIENTED_EDGE ( 'NONE', *, *, #51004, .F. ) ;
#209717 = CARTESIAN_POINT ( 'NONE',  ( -1.364683531250000748, 1.571875000341421691, 0.000000000000000000 ) ) ;
#209716 = CARTESIAN_POINT ( 'NONE',  ( 3.351411269679291038, 0.5553372447333758677, -2.223988721106509470 ) ) ;
#209718 = CARTESIAN_POINT ( 'NONE',  ( 2.198393463710220264, 5.716542807637226886, 0.7998128361456462443 ) ) ;
#209719 = CARTESIAN_POINT ( 'NONE',  ( 3.517450787741589036, 6.191110788085444128, -1.199719254218446718 ) ) ;
#209720 = CARTESIAN_POINT ( 'NONE',  ( 6.445936322256165418, -1.448296609194921647, -1.684281199878513657 ) ) ;
#209721 = CARTESIAN_POINT ( 'NONE',  ( -7.076992996653451939, 7.358839372291564374, 0.7216878364870317197 ) ) ;
#209722 = EDGE_CURVE ( 'NONE', #129981, #48908, #109622, .T. ) ;
#209723 = MECHANICAL_DESIGN_GEOMETRIC_PRESENTATION_REPRESENTATION (  '', ( #168158 ), #50793 ) ;
#209724 = CARTESIAN_POINT ( 'NONE',  ( 3.823036129373602154, 6.443664003369091731, -1.082531754730548412 ) ) ;
#209725 = CARTESIAN_POINT ( 'NONE',  ( -5.544921637864824504, 8.452530429942200385, -1.082531754730543971 ) ) ;
#209726 = CARTESIAN_POINT ( 'NONE',  ( 6.825078400183544503, 2.075476428726834577, 2.163873318353096931 ) ) ;
#209728 = VERTEX_POINT ( 'NONE', #90109 ) ;
#209727 = CIRCLE ( 'NONE', #123420, 0.08000000000000020983 ) ;
#209729 = CARTESIAN_POINT ( 'NONE',  ( 3.832657856672664565, 0.6767144645295587457, -1.899618369658891748 ) ) ;
#209731 = CARTESIAN_POINT ( 'NONE',  ( 2.571201674526869763, 1.840362857814400455, 0.9314759700368970829 ) ) ;
#209730 = CARTESIAN_POINT ( 'NONE',  ( 5.262536180398716290, 9.291375977107183104, -0.7998128361456291469 ) ) ;
#209732 = DIRECTION ( 'NONE',  ( -1.000000000000000000, 0.000000000000000000, 0.000000000000000000 ) ) ;
#209733 = CARTESIAN_POINT ( 'NONE',  ( 5.826972158823246595, 10.02016096192762085, -0.7998128361456481317 ) ) ;
#209734 = CARTESIAN_POINT ( 'NONE',  ( 1.642778471875000035, -3.726041666188707691, -2.845375778867859751 ) ) ;
#209735 = CARTESIAN_POINT ( 'NONE',  ( -1.364683531250012516, 4.488541667008090208, -0.7879004041258300672 ) ) ;
#209736 = CARTESIAN_POINT ( 'NONE',  ( 5.595707529797693702, -2.191629465999441084, -0.002916574791289594515 ) ) ;
#209737 = CARTESIAN_POINT ( 'NONE',  ( 2.391250195717840477, -0.7743161457766101208, -1.862016636315230844 ) ) ;
#209738 = CARTESIAN_POINT ( 'NONE',  ( 2.050122339901743196, -1.422379512129726908, 1.169167124061460949 ) ) ;
#209739 = ADVANCED_FACE ( 'NONE', ( #58659 ), #73842, .F. ) ;
#209740 = CARTESIAN_POINT ( 'NONE',  ( 7.644099680006512187, 7.812537802962739697, 1.040834085586084257E-14 ) ) ;
#209741 = CARTESIAN_POINT ( 'NONE',  ( 6.821331453475777629, -0.1281762050449504198, 1.796388512460028286 ) ) ;
#209742 = CARTESIAN_POINT ( 'NONE',  ( 0.01878015289935238558, -2.097885004189947278, 0.9400277066241318202 ) ) ;
#209743 = CARTESIAN_POINT ( 'NONE',  ( -7.015454420067433361, 10.27211502579893754, 1.199719254218453823 ) ) ;
#209745 = CARTESIAN_POINT ( 'NONE',  ( -4.145761110728687804, 8.058748072483927771, -0.7998128361456481317 ) ) ;
#209744 = CARTESIAN_POINT ( 'NONE',  ( 5.946200445400964263, 2.259567648220105252, 0.1180026366056959042 ) ) ;
#209746 = CARTESIAN_POINT ( 'NONE',  ( 1.365998295032941900, 2.074639164447332540, -0.3615360007043573187 ) ) ;
#209747 = CARTESIAN_POINT ( 'NONE',  ( -7.533490631048818109, 8.818102486758951031, -1.199719254218452047 ) ) ;
#209748 = CARTESIAN_POINT ( 'NONE',  ( 7.404724451357931336, 11.79059562655963056, 0.7998128361456462443 ) ) ;
#209749 = CARTESIAN_POINT ( 'NONE',  ( -9.578206935422265644, -9.900000000000005684, 0.1671882239536719994 ) ) ;
#209750 = DIRECTION ( 'NONE',  ( 0.000000000000000000, 0.000000000000000000, 1.000000000000000000 ) ) ;
#209751 = CARTESIAN_POINT ( 'NONE',  ( -8.701635661872465732, 9.046329781806354831, 1.040834085586084257E-14 ) ) ;
#209752 = CARTESIAN_POINT ( 'NONE',  ( 7.173763318589350568, -6.681223591463127498, 7.173763318589327476 ) ) ;
#209753 = CARTESIAN_POINT ( 'NONE',  ( 7.578644679914706472, 9.864838098032418401, 1.443375672974076540 ) ) ;
#209754 = CARTESIAN_POINT ( 'NONE',  ( 4.022946295931974170, 7.796337852756115794, -0.3444838504574644356 ) ) ;
#209755 = CARTESIAN_POINT ( 'NONE',  ( -9.490344339885977476, 11.13478515369756217, -1.082531754730539753 ) ) ;
#209756 = CARTESIAN_POINT ( 'NONE',  ( 2.479030958227887549, -1.528377378988081015, 1.612298682912993275 ) ) ;
#209757 = CARTESIAN_POINT ( 'NONE',  ( -2.428612866367529932E-14, 8.920000000000001705, 2.420000000000000373 ) ) ;
#209758 = CARTESIAN_POINT ( 'NONE',  ( -5.101610940492132151, 9.173906207207963348, -0.7998128361456362523 ) ) ;
#209759 = CARTESIAN_POINT ( 'NONE',  ( 3.825371897350130723, 7.614684313550482031, 0.7998128361456321445 ) ) ;
#209760 = CARTESIAN_POINT ( 'NONE',  ( 4.598074495912658044, 0.8407358649686399454, -1.772743347989129692 ) ) ;
#209761 = CARTESIAN_POINT ( 'NONE',  ( 10.21336978979620191, 10.81001959771741205, 0.7998128361456462443 ) ) ;
#209762 = CARTESIAN_POINT ( 'NONE',  ( -4.566676325625886435, 6.985790553628898003, 1.179912429979562249 ) ) ;
#209763 = CARTESIAN_POINT ( 'NONE',  ( 2.998324526916512411, 6.649795714711241423, 0.000000000000000000 ) ) ;
#209764 = CARTESIAN_POINT ( 'NONE',  ( 0.6823417656249882723, 0.1760416670080894308, -1.181850606188749264 ) ) ;
#209765 = CARTESIAN_POINT ( 'NONE',  ( -4.123088112331656951, 6.864000993478624579, 1.082531754730549967 ) ) ;
#209768 = ORIENTED_EDGE ( 'NONE', *, *, #120152, .F. ) ;
#209767 = CARTESIAN_POINT ( 'NONE',  ( -6.209271165378811297, 10.18797409300986878, 0.7216878364870458196 ) ) ;
#209766 = COLOUR_RGB ( '', 0.08235294, 0.09019608, 0.10196078) ;
#209769 = CARTESIAN_POINT ( 'NONE',  ( 3.234745892528373634, 1.342314639517484087, -1.641720766639111817 ) ) ;
#209770 = CARTESIAN_POINT ( 'NONE',  ( -4.176793841461789114, 7.030620694084159794, -1.199719254218455378 ) ) ;
#209771 = CARTESIAN_POINT ( 'NONE',  ( 4.610339536224768331, -0.9213992672730475508, -1.955631277330005968 ) ) ;
#209772 = CARTESIAN_POINT ( 'NONE',  ( 3.667381569930192597, 1.025862638139760419, 1.528780434079744843 ) ) ;
#209773 = CARTESIAN_POINT ( 'NONE',  ( -4.361599125657974696, 7.193191237876310318, 1.033186747995703758 ) ) ;
#209774 = CARTESIAN_POINT ( 'NONE',  ( -1.364683531250014514, -0.1989583329919157317, -0.7879004041258359514 ) ) ;
#209775 = CARTESIAN_POINT ( 'NONE',  ( 5.244012475127576955, 0.5104456934865635453, 1.663790013937071599 ) ) ;
#209776 = CARTESIAN_POINT ( 'NONE',  ( 10.91255906795568364, 3.426985321572577181, -3.952372590954820630 ) ) ;
#209777 = CARTESIAN_POINT ( 'NONE',  ( 2.887523530030648988, 6.312601851770308414, 0.000000000000000000 ) ) ;
#209778 = CARTESIAN_POINT ( 'NONE',  ( 0.7500000000000006661, 11.91666666666666607, -1.299038105676657340 ) ) ;
#209779 = CARTESIAN_POINT ( 'NONE',  ( 2.764712544972968811, -1.491509591961351910, 1.564943835847030229 ) ) ;
#209780 = CARTESIAN_POINT ( 'NONE',  ( 5.325545996062735377, -1.462220743079494012, 1.388274341532859335 ) ) ;
#209781 = CARTESIAN_POINT ( 'NONE',  ( -8.419250203962027612, 11.80591375705560608, 1.082531754730549967 ) ) ;
#209782 = CARTESIAN_POINT ( 'NONE',  ( 2.624079441566569582, -1.243859440641072123, -1.767801033134681843 ) ) ;
#209783 = CARTESIAN_POINT ( 'NONE',  ( 3.444560810740458390, 0.4755345817112103246, 1.913044316819292767 ) ) ;
#209784 = EDGE_CURVE ( 'NONE', #897, #145305, #96117, .T. ) ;
#209785 =( NAMED_UNIT ( * ) PLANE_ANGLE_UNIT ( ) SI_UNIT ( $, .RADIAN. ) );
#209786 = CARTESIAN_POINT ( 'NONE',  ( 4.282717048480193078, 1.733172068543160416, -0.8763712590400226654 ) ) ;
#209789 = ORIENTED_EDGE ( 'NONE', *, *, #84048, .F. ) ;
#209788 = DIRECTION ( 'NONE',  ( -5.578564026256490882E-16, -1.000000000000000000, -9.066213480720158442E-32 ) ) ;
#209787 = CARTESIAN_POINT ( 'NONE',  ( -7.334597914868722590, 11.50085530074811935, -0.7216878364870267237 ) ) ;
#209790 = CONICAL_SURFACE ( 'NONE', #36776, 4.000000000000000000, 0.8960553845713404852 ) ;
#209792 = ADVANCED_FACE ( 'NONE', ( #175627, #204875 ), #209151, .T. ) ;
#209791 = CARTESIAN_POINT ( 'NONE',  ( -6.526270840131767059, 8.707344961610770540, -1.599625672291271394 ) ) ;
#209793 = FACE_OUTER_BOUND ( 'NONE', #137214, .T. ) ;
#209795 = ORIENTED_EDGE ( 'NONE', *, *, #92162, .T. ) ;
#209794 = CARTESIAN_POINT ( 'NONE',  ( -5.167592825464113915, 6.057888380243431570, 1.199719254218452935 ) ) ;
#209796 = CARTESIAN_POINT ( 'NONE',  ( -8.365017589507372620, 9.821903944922480534, 1.082531754730558626 ) ) ;
#209797 = CARTESIAN_POINT ( 'NONE',  ( 1.852830919558448697, 0.6925466627333074499, 2.095365425716289032 ) ) ;
#209798 = CARTESIAN_POINT ( 'NONE',  ( -1.642778471874998480, -1.101041666188708801, 2.845375778867863303 ) ) ;
#209799 = CARTESIAN_POINT ( 'NONE',  ( 6.807479307002794577, -1.573682814073861902, -1.171087784426767753 ) ) ;
#209800 = CARTESIAN_POINT ( 'NONE',  ( -0.6823417656249969321, 5.530208333674756283, -1.181850606188749264 ) ) ;
#209801 = CARTESIAN_POINT ( 'NONE',  ( 1.499999999999987121, 4.077083334016147198, -0.8660254037844323793 ) ) ;
#209802 = CARTESIAN_POINT ( 'NONE',  ( 6.043473040404234276, 6.060458613201341826, -0.4842117992061110154 ) ) ;
#209804 = CARTESIAN_POINT ( 'NONE',  ( 6.111994396789379280, -2.190734547077430872, 0.2660306753756238041 ) ) ;
#209803 = DIRECTION ( 'NONE',  ( 5.578564026256490882E-16, 1.000000000000000000, 9.066213480720158442E-32 ) ) ;
#209805 = CARTESIAN_POINT ( 'NONE',  ( 5.437399513225577685, 0.7426265630364609072, -1.684910612069365321 ) ) ;
#209806 = ORIENTED_EDGE ( 'NONE', *, *, #161304, .F. ) ;
#209807 = CARTESIAN_POINT ( 'NONE',  ( -1.360316468750044860, -0.8385416663252739378, 0.7853790794158720390 ) ) ;
#209808 = CARTESIAN_POINT ( 'NONE',  ( -7.965578943228732278, 9.251929174310385307, -1.199719254218446718 ) ) ;
#209809 = LINE ( 'NONE', #80898, #196781 ) ;
#209810 = CARTESIAN_POINT ( 'NONE',  ( 6.117454236943913770, 1.763945953808215394, 1.176740244630887222 ) ) ;
#209811 = CARTESIAN_POINT ( 'NONE',  ( 8.790098660144264997, 13.29414747594432455, 8.101455065885630802 ) ) ;
#209812 = CARTESIAN_POINT ( 'NONE',  ( 6.322179702674084467, 6.270297829408224111, 1.040834085586084257E-14 ) ) ;
#209813 = CARTESIAN_POINT ( 'NONE',  ( 0.1279053400650804195, -1.267571945882491447, -1.625495855733450457 ) ) ;
#209816 = CARTESIAN_POINT ( 'NONE',  ( 3.966218424140379728, -1.719484690100345325, -0.6589542199007536460 ) ) ;
#209815 = CARTESIAN_POINT ( 'NONE',  ( 1.943593235818155351, 1.280450557881509299, 1.350794863662147627 ) ) ;
#209814 = CARTESIAN_POINT ( 'NONE',  ( -9.800782855757772083, 4.518459118458827639, 6.931930279218311064 ) ) ;
#209817 = CARTESIAN_POINT ( 'NONE',  ( 6.795661308947685164, 8.951357498570873261, -1.599625672291262513 ) ) ;
#209818 = CARTESIAN_POINT ( 'NONE',  ( -9.494457024495529751, 14.66554680615851325, -7.338830936511814507 ) ) ;
#209819 = CARTESIAN_POINT ( 'NONE',  ( -5.986807348886189040, 9.142303119412650503, -1.199719254218452047 ) ) ;
#209821 = ORIENTED_EDGE ( 'NONE', *, *, #140883, .T. ) ;
#209820 = CARTESIAN_POINT ( 'NONE',  ( 6.610000000000006537, 0.002781820520842553934, 2.000159646111852929 ) ) ;
#209822 = CARTESIAN_POINT ( 'NONE',  ( 3.457846583235091753, 0.5364296187198510646, -2.140574738106671759 ) ) ;
#209823 = CARTESIAN_POINT ( 'NONE',  ( 5.835331047353732536, -2.048883276207621229, 0.9597388403507837173 ) ) ;
#209824 = CARTESIAN_POINT ( 'NONE',  ( -6.073689629242176480, 6.188318776978391611, -0.7216878364870278340 ) ) ;
#209825 = CARTESIAN_POINT ( 'NONE',  ( 5.642768253578701376, 1.748184277621564808, 0.4749025624241067223 ) ) ;
#209826 = CARTESIAN_POINT ( 'NONE',  ( 0.1808755166769344669, 1.673851406602990366, -1.124249698880399162 ) ) ;
#209827 = CYLINDRICAL_SURFACE ( 'NONE', #206378, 1.250000000000000000 ) ;
#209828 = CARTESIAN_POINT ( 'NONE',  ( 6.631728656526095556, -1.223761959379562114, -1.414937998750566361 ) ) ;
#209829 = CARTESIAN_POINT ( 'NONE',  ( 6.129550632656369125, -0.2293275368827427663, 1.898405681093485953 ) ) ;
#209830 = DIRECTION ( 'NONE',  ( 0.000000000000000000, 1.000000000000000000, 0.000000000000000000 ) ) ;
#209831 = CARTESIAN_POINT ( 'NONE',  ( 0.7427767429722329506, -1.606530860214189893, 0.9580933318182258684 ) ) ;
#209832 = CARTESIAN_POINT ( 'NONE',  ( 0.7257964430846426396, 0.8128130212789463904, -1.845628942776005088 ) ) ;
#209834 = CARTESIAN_POINT ( 'NONE',  ( 4.037795408393930252, -1.452196710024173276, -1.525570609991099502 ) ) ;
#209833 = CARTESIAN_POINT ( 'NONE',  ( -8.748035429315585532, 11.22912730566677553, -1.599625672291263179 ) ) ;
#209835 = CARTESIAN_POINT ( 'NONE',  ( 7.397945374551106568, 11.78268670361832093, -0.7998128361456291469 ) ) ;
#209837 = CARTESIAN_POINT ( 'NONE',  ( -8.585337585951595685, 11.03931315507545108, -1.599625672291263179 ) ) ;
#209836 = CARTESIAN_POINT ( 'NONE',  ( -0.7500000000000006661, -0.3916666666666443475, -1.299038105676652011 ) ) ;
#209838 = CARTESIAN_POINT ( 'NONE',  ( 3.269790213696788683, 0.4867576797993823368, -1.960144559866239700 ) ) ;
#209839 = CARTESIAN_POINT ( 'NONE',  ( -1.201851678989727383E-14, 3.196875000341420137, -1.575800808251660134 ) ) ;
#209840 = CARTESIAN_POINT ( 'NONE',  ( 4.207107738942202246, 3.802713871720993399, 1.214306433183764966E-14 ) ) ;
#209841 = CARTESIAN_POINT ( 'NONE',  ( 2.741676502816026595, -1.599691942034554337, -1.453933697666408120 ) ) ;
#209842 = CARTESIAN_POINT ( 'NONE',  ( 6.016786309414542622, 10.24161080428416426, 0.7998128361456341429 ) ) ;
#209843 = CARTESIAN_POINT ( 'NONE',  ( -1.499999999999997780, 4.650000000000022560, 1.214306433183764966E-14 ) ) ;
#209845 = CARTESIAN_POINT ( 'NONE',  ( -9.623574082427422738, -9.090902906714937615, 0.4644248560400319747 ) ) ;
#209844 = CARTESIAN_POINT ( 'NONE',  ( 7.530627977747744062, 7.750430493652658015, -0.7998128361456341429 ) ) ;
#209846 = CARTESIAN_POINT ( 'NONE',  ( 7.727784369665023689, 11.95957283134381477, 1.040834085586084257E-14 ) ) ;
#209848 = CARTESIAN_POINT ( 'NONE',  ( 7.903398181601305694, 15.38462505118610757, -9.031418266963273211 ) ) ;
#209847 = CARTESIAN_POINT ( 'NONE',  ( 0.4148109920584437948, 0.8315006815404235585, 2.005833495578440928 ) ) ;
#209849 = CARTESIAN_POINT ( 'NONE',  ( -7.049876689426121779, 7.327203680526343632, -0.7216878364870278340 ) ) ;
#209850 = CIRCLE ( 'NONE', #78446, 2.000000000000000000 ) ;
#209851 = CARTESIAN_POINT ( 'NONE',  ( 0.6823417656249899377, 1.592708333674752730, 1.181850606188755259 ) ) ;
#209852 = CARTESIAN_POINT ( 'NONE',  ( 1.909981697816802049, -1.036543071415759298, -1.930953618257096993 ) ) ;
#209853 = CARTESIAN_POINT ( 'NONE',  ( 0.000000000000000000, -8.407420853759283830, 10.91970695577495931 ) ) ;
#209854 = CARTESIAN_POINT ( 'NONE',  ( 2.149658728627835469, -1.817393572686412107, -1.347411789871997057 ) ) ;
#209855 = CARTESIAN_POINT ( 'NONE',  ( -6.008234629150358330, 10.16135750065076060, 0.000000000000000000 ) ) ;
#209856 = CARTESIAN_POINT ( 'NONE',  ( 1.364683531249988535, 5.217708333674750065, -0.7879004041258300672 ) ) ;
#209857 = CARTESIAN_POINT ( 'NONE',  ( 5.309622429108474151, 7.625948988765205883, 1.230663689527239812 ) ) ;
#209858 = CARTESIAN_POINT ( 'NONE',  ( -1.402160292154681736E-14, 12.31250000000000355, 1.732050807568881190 ) ) ;
#209859 = CARTESIAN_POINT ( 'NONE',  ( 5.207740401424913124, 9.089797878388800711, -0.7216878364870458196 ) ) ;
#209860 =( BOUNDED_CURVE ( )  B_SPLINE_CURVE ( 2, ( #150996, #2563, #198639, #99044, #50287, #119612, #182396, #106286, #166159 ),
 .UNSPECIFIED., .F., .T. ) 
 B_SPLINE_CURVE_WITH_KNOTS ( ( 3, 2, 2, 2, 3 ),
 ( 0.8303571428571429047, 0.8333333333333333703, 0.8392857142857143016, 0.8452380952380952328, 0.8482142857142856984 ),
 .UNSPECIFIED. ) 
 CURVE ( )  GEOMETRIC_REPRESENTATION_ITEM ( )  RATIONAL_B_SPLINE_CURVE ( ( 0.9330127018922194093, 0.9330127018922206306, 1.000000000000000000, 0.8660254037844387076, 1.000000000000000000, 0.8660254037844387076, 1.000000000000000000, 0.9330127018922194093, 0.9330127018922194093 ) ) 
 REPRESENTATION_ITEM ( '' )  );
#209861 = CARTESIAN_POINT ( 'NONE',  ( 3.919032125857401905, -0.1322120426517567060, 1.764875357724977167 ) ) ;
#209862 = CARTESIAN_POINT ( 'NONE',  ( 8.341290820905593151, 10.75459192918846618, 1.599625672291281386 ) ) ;
#209863 = CARTESIAN_POINT ( 'NONE',  ( 0.4464868854077256866, 2.100361318156780399, 0.1544987475943972732 ) ) ;
#209865 = CARTESIAN_POINT ( 'NONE',  ( -0.7500000000000006661, 0.6083333333333564852, -1.299038105676652011 ) ) ;
#209864 = CARTESIAN_POINT ( 'NONE',  ( 1.364683531249996529, 8.713541667008067648, 0.7879004041258405033 ) ) ;
#209866 = CARTESIAN_POINT ( 'NONE',  ( -5.822300622425855110, 5.757381912443740646, 0.7998128361456281477 ) ) ;
#209867 = CARTESIAN_POINT ( 'NONE',  ( 6.415638736316127577, -1.319241173714128745, -1.525034172108488573 ) ) ;
#209868 = ORIENTED_EDGE ( 'NONE', *, *, #61478, .F. ) ;
#209869 = CARTESIAN_POINT ( 'NONE',  ( 10.24726517383036928, 10.84956421242393887, 0.000000000000000000 ) ) ;
#209871 = CARTESIAN_POINT ( 'NONE',  ( 3.537841792810627606, 0.8420186812403904764, -1.670516725672297031 ) ) ;
#209870 = AXIS2_PLACEMENT_3D ( 'NONE', #85959, #133681, #21986 ) ;
#209872 = CARTESIAN_POINT ( 'NONE',  ( 4.627825472248149552, 2.009385113269086087, -0.4979276649561757417 ) ) ;
#209873 = CARTESIAN_POINT ( 'NONE',  ( -6.577113915960841162, 7.806292669110006521, -1.082531754730549967 ) ) ;
#209874 = DIRECTION ( 'NONE',  ( -3.330669073875481947E-16, 4.742150360713068815E-16, 1.000000000000000000 ) ) ;
#209875 = CARTESIAN_POINT ( 'NONE',  ( 7.889955328148847258, 11.29236608522730911, -1.199719254218446718 ) ) ;
#209876 = CARTESIAN_POINT ( 'NONE',  ( -9.154780037725563702, 11.70366268214508487, 1.599625672291281386 ) ) ;
#209877 = CARTESIAN_POINT ( 'NONE',  ( -4.989511253089500720, 4.785794314884651790, -0.3387278650471270969 ) ) ;
#209878 = CARTESIAN_POINT ( 'NONE',  ( -5.426654608689173820, 6.244223002735716399, -0.9996599858201720146 ) ) ;
#209879 = CARTESIAN_POINT ( 'NONE',  ( -1.001543065824772872E-14, 5.134375000341421469, 1.575800808251672791 ) ) ;
#209880 = CARTESIAN_POINT ( 'NONE',  ( 3.525789274851616639, 1.914599547803575330, -0.4273510147508317591 ) ) ;
#209881 = EDGE_CURVE ( 'NONE', #174627, #156842, #59721, .T. ) ;
#209882 = CARTESIAN_POINT ( 'NONE',  ( 1.089219988750099732, 1.203171814842165288, -1.617568698395126292 ) ) ;
#209883 = CARTESIAN_POINT ( 'NONE',  ( -4.442231607132987925, 5.211633625523774960, -1.199719254218453823 ) ) ;
#209885 = LINE ( 'NONE', #7424, #22543 ) ;
#209884 = CARTESIAN_POINT ( 'NONE',  ( 7.639129486296027061, 10.99973593639901814, 1.199719254218460707 ) ) ;
#209886 = CARTESIAN_POINT ( 'NONE',  ( 0.9306671693925671063, 0.1315677519515070781, 1.865966016356377821 ) ) ;
#209887 = CARTESIAN_POINT ( 'NONE',  ( 1.364683531249988535, 3.405208333674749621, -0.7879004041258239610 ) ) ;
#209888 = CARTESIAN_POINT ( 'NONE',  ( 3.515888537569244132, -0.5802020150980004010, 1.927815774739343180 ) ) ;
#209890 = CARTESIAN_POINT ( 'NONE',  ( 2.267339977356534142, 1.934377090824404455, -0.8611398932509596316 ) ) ;
#209889 = CARTESIAN_POINT ( 'NONE',  ( -5.910991785878165317, 8.879612269291090598, -1.082531754730538864 ) ) ;
#209891 = CARTESIAN_POINT ( 'NONE',  ( 6.825078400183544503, 6.034152930826206962, 2.739236550662868197 ) ) ;
#209892 = CARTESIAN_POINT ( 'NONE',  ( 3.332542965736586371, -1.235447621225284509, 1.661183390374972424 ) ) ;
#209893 = CARTESIAN_POINT ( 'NONE',  ( 5.508355548902068577, 9.648441583686274470, 0.7998128361456331437 ) ) ;
#209895 = CARTESIAN_POINT ( 'NONE',  ( 4.552840656090682891, 4.206068941727564514, 1.214306433183764966E-14 ) ) ;
#209894 = CARTESIAN_POINT ( 'NONE',  ( 0.4860219701983969909, -2.075441973172939214, -0.2518264690121001514 ) ) ;
#209897 = EDGE_LOOP ( 'NONE', ( #99711, #64883, #37795, #24302 ) ) ;
#209896 = CARTESIAN_POINT ( 'NONE',  ( 5.561492448144861989, 0.3540975402388062965, -1.790731494587729067 ) ) ;
#209898 = CARTESIAN_POINT ( 'NONE',  ( 8.372323551638698902, 9.726464550788689323, 1.199719254218462483 ) ) ;
#209899 = CARTESIAN_POINT ( 'NONE',  ( 2.487170525094726248, 8.243531156566618279, -2.499999999999888534 ) ) ;
#209900 = CARTESIAN_POINT ( 'NONE',  ( 10.14021943694179839, 13.64433865160459192, -7.295449844790285354 ) ) ;
#209901 = CARTESIAN_POINT ( 'NONE',  ( 6.475609205405274515, 2.113627995098281254, -0.6344055572156809264 ) ) ;
#209902 = CARTESIAN_POINT ( 'NONE',  ( 0.6823417656249969321, 11.33854166700806765, -1.181850606188757036 ) ) ;
#209903 = CARTESIAN_POINT ( 'NONE',  ( 4.617770051018644573, -0.5065499601877522240, 1.843912185298258066 ) ) ;
#209904 = CARTESIAN_POINT ( 'NONE',  ( -8.134002093194872884, 11.57708731111429401, 1.199719254218453823 ) ) ;
#209905 =( BOUNDED_SURFACE ( )  B_SPLINE_SURFACE ( 1, 2, ( 
 ( #5811, #187786, #71887, #39415, #192045, #24207, #173716, #59929, #90310, #122903, #109826, #156381, #123960, #155304, #6886, #206170, #77242, #27428, #171542, #158507, #140146, #41573, #106603, #188861, #56735, #142287, #7963, #57800, #40499, #175837, #92469, #190980, #44778, #23135, #75122, #172631, #207241, #189928, #42644, #141231, #139069, #74054, #193129, #26353, #108754, #72964, #174778, #143359, #107687, #208298, #43708, #205094, #58865, #89252, #25292, #76180, #9047, #209356, #10107, #91392, #61002, #157453, #125022, #126084, #93526, #159568, #11165, #127158, #63139, #95668, #131394, #177965, #147599, #46910, #197391, #129301, #45843, #163852, #113027, #162786, #47986, #110884, #62077, #179034, #213617, #30652, #111962, #195277, #146553, #212573, #96738, #64211, #14364, #98849, #145504, #29578, #15432, #115153, #161720, #181148, #13312, #194197, #144434, #79385, #128234, #211502, #80455, #148661, #130352, #180093, #164900, #196343, #114102, #31717, #176890, #94593, #97792, #81521, #65243, #160635, #132449, #49033, #32770, #16493, #82574, #228, #66300, #198447, #28503, #12236, #78310, #210436, #41044, #167044, #35960, #23693, #56209, #89803, #73515, #184336, #156924, #8513, #102038, #151865, #1304, #6367, #100954, #117279, #139617, #118349, #205640, #168107, #106077, #74594, #19706, #140698, #122373, #99908, #90860, #50093, #133508, #72436, #85785, #18636, #188330, #138537, #116215, #165968, #24758, #17553, #83639, #84716, #172100, #204561, #182202, #39970, #150803, #155847, #7434, #57279, #149726, #2367, #200574, #123440, #68444, #189402, #173178, #107153, #33829, #67364, #34881, #51157, #199512, #183277, #134573, #52220, #124496, #125556, #75658, #209893, #25823, #92995, #178491, #58340, #46362, #61531, #30101, #79903, #127697, #112482, #45300, #177423, #206712, #190455, #142824, #42114, #160102, #193657, #27968, #26891, #62587, #162242, #108226, #94062, #78833, #111419, #174251, #144954, #141765, #59400, #96191, #191517, #13828, #43182, #159039, #110357, #29041, #95124, #77779, #9582, #210960 ),
 ( #11705, #208831, #143900, #60461, #194723, #10632, #109295, #161173, #128750, #175304, #91933, #76708, #207773, #157993, #126618, #192581, #12759, #44236, #176361, #51694, #131904, #115666, #113553, #130862, #147069, #181660, #67890, #752, #80980, #63665, #64720, #14885, #149175, #179556, #32231, #117816, #212022, #200043, #66818, #183806, #19164, #132961, #35416, #198964, #116733, #146011, #129819, #82034, #195801, #99371, #50608, #33287, #180606, #1831, #101494, #47438, #165423, #18086, #182732, #31177, #84174, #213090, #196858, #167564, #48496, #97250, #114615, #98302, #49540, #34351, #100424, #17020, #163304, #150263, #164367, #15951, #83096, #197912, #148128, #214129, #166495, #134035, #65757, #6105, #22353, #123190, #152384, #55954, #122107, #53821, #71103, #3962, #188072, #137221, #37562, #203241, #39701, #88465, #105810, #171836, #5028, #189151, #40790, #54885, #187006, #36487, #38637, #136145, #70030, #23429, #153455, #89540, #121039, #138283, #106895, #104716, #172921, #154525, #135086, #85238, #151326, #168624, #170764, #72175, #119951, #204298, #155591, #2894, #201100, #57023, #52740, #118874, #202163, #7176, #73247, #68967, #139354, #185926, #205384, #184860, #102564, #20227, #86312, #103642, #169694, #21282, #87388, #76463, #62354, #11458, #157738, #210728, #25574, #142572, #193420, #111175, #92747, #59148, #128515, #191264, #9335, #45064, #91685, #61288, #175059, #177176, #42930, #174003, #77531, #26646, #208579, #176120, #24497, #190205, #158791, #127449, #10388, #75408, #109040, #60212, #126373, #192332, #43991, #110109, #12523, #125306, #141521, #143652, #28793, #207529, #94877, #27720, #107974, #58085, #93814, #41865, #159855, #209647, #194483, #160929, #78596, #144716, #46126, #112243, #90608, #156667, #8259, #74343, #140447, #206458, #124247, #199794, #48262, #195563, #197670, #179320, #166244, #116490, #98076, #95950, #31995, #163070, #47199, #17834, #80745, #180371, #66574, #30941, #129576, #182479, #14651, #130631, #162005, #13594, #212852, #83917, #34107, #178254, #165179, #146833, #114376 ) ),
 .UNSPECIFIED., .F., .F., .T. ) 
 B_SPLINE_SURFACE_WITH_KNOTS ( ( 2, 2 ),
 ( 3, 2, 2, 2, 2, 2, 2, 2, 2, 2, 2, 2, 2, 2, 2, 2, 2, 2, 2, 2, 2, 2, 2, 2, 2, 2, 2, 2, 2, 2, 2, 2, 2, 2, 2, 2, 2, 2, 2, 2, 2, 2, 2, 2, 2, 2, 2, 2, 2, 2, 2, 2, 2, 2, 2, 2, 2, 2, 2, 2, 2, 2, 2, 2, 2, 2, 2, 2, 2, 2, 2, 2, 2, 2, 2, 2, 2, 2, 2, 2, 2, 2, 2, 2, 2, 2, 2, 2, 2, 2, 2, 2, 2, 2, 2, 2, 2, 2, 2, 2, 2, 2, 2, 2, 2, 2, 2, 2, 2, 2, 2, 2, 2, 2, 2, 2, 2, 2, 2, 2, 3 ),
 ( 0.000000000000000000, 1.000000000000000000 ),
 ( 0.000000000000000000, 0.008333333333333333218, 0.01666666666666666644, 0.02500000000000000139, 0.03333333333333333287, 0.04166666666666666435, 0.05000000000000000278, 0.05833333333333333426, 0.06666666666666666574, 0.07499999999999999722, 0.08333333333333332871, 0.09166666666666666019, 0.1000000000000000056, 0.1083333333333333370, 0.1166666666666666685, 0.1250000000000000000, 0.1333333333333333315, 0.1416666666666666630, 0.1499999999999999944, 0.1583333333333333259, 0.1666666666666666574, 0.1749999999999999889, 0.1833333333333333204, 0.1916666666666666796, 0.2000000000000000111, 0.2083333333333333426, 0.2166666666666666741, 0.2250000000000000056, 0.2333333333333333370, 0.2416666666666666685, 0.2500000000000000000, 0.2583333333333333592, 0.2666666666666666630, 0.2750000000000000222, 0.2833333333333333259, 0.2916666666666666852, 0.2999999999999999889, 0.3083333333333333481, 0.3166666666666666519, 0.3250000000000000111, 0.3333333333333333148, 0.3416666666666666741, 0.3499999999999999778, 0.3583333333333333370, 0.3666666666666666408, 0.3750000000000000000, 0.3833333333333333592, 0.3916666666666666630, 0.4000000000000000222, 0.4083333333333333259, 0.4166666666666666852, 0.4249999999999999889, 0.4333333333333333481, 0.4416666666666666519, 0.4500000000000000111, 0.4583333333333333148, 0.4666666666666666741, 0.4749999999999999778, 0.4833333333333333370, 0.4916666666666666408, 0.5000000000000000000, 0.5083333333333333037, 0.5166666666666667185, 0.5250000000000000222, 0.5333333333333333259, 0.5416666666666666297, 0.5500000000000000444, 0.5583333333333333481, 0.5666666666666666519, 0.5749999999999999556, 0.5833333333333333703, 0.5916666666666666741, 0.5999999999999999778, 0.6083333333333332815, 0.6166666666666666963, 0.6250000000000000000, 0.6333333333333333037, 0.6416666666666667185, 0.6500000000000000222, 0.6583333333333333259, 0.6666666666666666297, 0.6750000000000000444, 0.6833333333333333481, 0.6916666666666666519, 0.6999999999999999556, 0.7083333333333333703, 0.7166666666666666741, 0.7249999999999999778, 0.7333333333333332815, 0.7416666666666666963, 0.7500000000000000000, 0.7583333333333333037, 0.7666666666666667185, 0.7750000000000000222, 0.7833333333333333259, 0.7916666666666666297, 0.8000000000000000444, 0.8083333333333333481, 0.8166666666666666519, 0.8249999999999999556, 0.8333333333333333703, 0.8416666666666666741, 0.8499999999999999778, 0.8583333333333332815, 0.8666666666666666963, 0.8750000000000000000, 0.8833333333333333037, 0.8916666666666667185, 0.9000000000000000222, 0.9083333333333333259, 0.9166666666666666297, 0.9250000000000000444, 0.9333333333333333481, 0.9416666666666666519, 0.9499999999999999556, 0.9583333333333333703, 0.9666666666666666741, 0.9749999999999999778, 0.9833333333333332815, 0.9916666666666666963, 1.000000000000000000 ),
 .UNSPECIFIED. ) 
 GEOMETRIC_REPRESENTATION_ITEM ( )  RATIONAL_B_SPLINE_SURFACE ( (
 ( 1.000000000000000000, 0.8660254037844387076, 1.000000000000000000, 0.8660254037844387076, 1.000000000000000000, 0.8660254037844387076, 1.000000000000000000, 0.8660254037844387076, 1.000000000000000000, 0.8660254037844387076, 1.000000000000000000, 0.8660254037844387076, 1.000000000000000000, 0.8660254037844387076, 1.000000000000000000, 0.8660254037844387076, 1.000000000000000000, 0.8660254037844387076, 1.000000000000000000, 0.8660254037844387076, 1.000000000000000000, 0.8660254037844387076, 1.000000000000000000, 0.8660254037844387076, 1.000000000000000000, 0.8660254037844387076, 1.000000000000000000, 0.8660254037844387076, 1.000000000000000000, 0.8660254037844387076, 1.000000000000000000, 0.8660254037844387076, 1.000000000000000000, 0.8660254037844387076, 1.000000000000000000, 0.8660254037844387076, 1.000000000000000000, 0.8660254037844387076, 1.000000000000000000, 0.8660254037844387076, 1.000000000000000000, 0.8660254037844387076, 1.000000000000000000, 0.8660254037844387076, 1.000000000000000000, 0.8660254037844387076, 1.000000000000000000, 0.8660254037844387076, 1.000000000000000000, 0.8660254037844387076, 1.000000000000000000, 0.8660254037844387076, 1.000000000000000000, 0.8660254037844387076, 1.000000000000000000, 0.8660254037844387076, 1.000000000000000000, 0.8660254037844387076, 1.000000000000000000, 0.8660254037844387076, 1.000000000000000000, 0.8660254037844387076, 1.000000000000000000, 0.8660254037844387076, 1.000000000000000000, 0.8660254037844387076, 1.000000000000000000, 0.8660254037844387076, 1.000000000000000000, 0.8660254037844387076, 1.000000000000000000, 0.8660254037844387076, 1.000000000000000000, 0.8660254037844387076, 1.000000000000000000, 0.8660254037844387076, 1.000000000000000000, 0.8660254037844387076, 1.000000000000000000, 0.8660254037844387076, 1.000000000000000000, 0.8660254037844387076, 1.000000000000000000, 0.8660254037844387076, 1.000000000000000000, 0.8660254037844387076, 1.000000000000000000, 0.8660254037844387076, 1.000000000000000000, 0.8660254037844387076, 1.000000000000000000, 0.8660254037844387076, 1.000000000000000000, 0.8660254037844387076, 1.000000000000000000, 0.8660254037844387076, 1.000000000000000000, 0.8660254037844387076, 1.000000000000000000, 0.8660254037844387076, 1.000000000000000000, 0.8660254037844387076, 1.000000000000000000, 0.8660254037844387076, 1.000000000000000000, 0.8660254037844387076, 1.000000000000000000, 0.8660254037844387076, 1.000000000000000000, 0.8660254037844387076, 1.000000000000000000, 0.8660254037844387076, 1.000000000000000000, 0.8660254037844387076, 1.000000000000000000, 0.8660254037844387076, 1.000000000000000000, 0.8660254037844387076, 1.000000000000000000, 0.8660254037844387076, 1.000000000000000000, 0.8660254037844387076, 1.000000000000000000, 0.8660254037844387076, 1.000000000000000000, 0.8660254037844387076, 1.000000000000000000, 0.8660254037844387076, 1.000000000000000000, 0.8660254037844387076, 1.000000000000000000, 0.8660254037844387076, 1.000000000000000000, 0.8660254037844387076, 1.000000000000000000, 0.8660254037844387076, 1.000000000000000000, 0.8660254037844387076, 1.000000000000000000, 0.8660254037844387076, 1.000000000000000000, 0.8660254037844387076, 1.000000000000000000, 0.8660254037844387076, 1.000000000000000000, 0.8660254037844387076, 1.000000000000000000, 0.8660254037844387076, 1.000000000000000000, 0.8660254037844387076, 1.000000000000000000, 0.8660254037844387076, 1.000000000000000000, 0.8660254037844387076, 1.000000000000000000, 0.8660254037844387076, 1.000000000000000000, 0.8660254037844387076, 1.000000000000000000, 0.8660254037844387076, 1.000000000000000000, 0.8660254037844387076, 1.000000000000000000, 0.8660254037844387076, 1.000000000000000000, 0.8660254037844387076, 1.000000000000000000, 0.8660254037844387076, 1.000000000000000000, 0.8660254037844387076, 1.000000000000000000, 0.8660254037844387076, 1.000000000000000000, 0.8660254037844387076, 1.000000000000000000, 0.8660254037844387076, 1.000000000000000000, 0.8660254037844387076, 1.000000000000000000, 0.8660254037844387076, 1.000000000000000000, 0.8660254037844387076, 1.000000000000000000, 0.8660254037844387076, 1.000000000000000000, 0.8660254037844387076, 1.000000000000000000, 0.8660254037844387076, 1.000000000000000000, 0.8660254037844387076, 1.000000000000000000, 0.8660254037844387076, 1.000000000000000000, 0.8660254037844387076, 1.000000000000000000, 0.8660254037844387076, 1.000000000000000000, 0.8660254037844387076, 1.000000000000000000, 0.8660254037844387076, 1.000000000000000000, 0.8660254037844387076, 1.000000000000000000, 0.8660254037844387076, 1.000000000000000000, 0.8660254037844387076, 1.000000000000000000, 0.8660254037844387076, 1.000000000000000000, 0.8660254037844387076, 1.000000000000000000, 0.8660254037844387076, 1.000000000000000000, 0.8660254037844387076, 1.000000000000000000, 0.8660254037844387076, 1.000000000000000000, 0.8660254037844387076, 1.000000000000000000, 0.8660254037844387076, 1.000000000000000000, 0.8660254037844387076, 1.000000000000000000, 0.8660254037844387076, 1.000000000000000000, 0.8660254037844387076, 1.000000000000000000, 0.8660254037844387076, 1.000000000000000000, 0.8660254037844387076, 1.000000000000000000, 0.8660254037844387076, 1.000000000000000000, 0.8660254037844387076, 1.000000000000000000, 0.8660254037844387076, 1.000000000000000000, 0.8660254037844387076, 1.000000000000000000, 0.8660254037844387076, 1.000000000000000000),
 ( 1.000000000000000000, 0.8660254037844387076, 1.000000000000000000, 0.8660254037844387076, 1.000000000000000000, 0.8660254037844387076, 1.000000000000000000, 0.8660254037844387076, 1.000000000000000000, 0.8660254037844387076, 1.000000000000000000, 0.8660254037844387076, 1.000000000000000000, 0.8660254037844387076, 1.000000000000000000, 0.8660254037844387076, 1.000000000000000000, 0.8660254037844387076, 1.000000000000000000, 0.8660254037844387076, 1.000000000000000000, 0.8660254037844387076, 1.000000000000000000, 0.8660254037844387076, 1.000000000000000000, 0.8660254037844387076, 1.000000000000000000, 0.8660254037844387076, 1.000000000000000000, 0.8660254037844387076, 1.000000000000000000, 0.8660254037844387076, 1.000000000000000000, 0.8660254037844387076, 1.000000000000000000, 0.8660254037844387076, 1.000000000000000000, 0.8660254037844387076, 1.000000000000000000, 0.8660254037844387076, 1.000000000000000000, 0.8660254037844387076, 1.000000000000000000, 0.8660254037844387076, 1.000000000000000000, 0.8660254037844387076, 1.000000000000000000, 0.8660254037844387076, 1.000000000000000000, 0.8660254037844387076, 1.000000000000000000, 0.8660254037844387076, 1.000000000000000000, 0.8660254037844387076, 1.000000000000000000, 0.8660254037844387076, 1.000000000000000000, 0.8660254037844387076, 1.000000000000000000, 0.8660254037844387076, 1.000000000000000000, 0.8660254037844387076, 1.000000000000000000, 0.8660254037844387076, 1.000000000000000000, 0.8660254037844387076, 1.000000000000000000, 0.8660254037844387076, 1.000000000000000000, 0.8660254037844387076, 1.000000000000000000, 0.8660254037844387076, 1.000000000000000000, 0.8660254037844387076, 1.000000000000000000, 0.8660254037844387076, 1.000000000000000000, 0.8660254037844387076, 1.000000000000000000, 0.8660254037844387076, 1.000000000000000000, 0.8660254037844387076, 1.000000000000000000, 0.8660254037844387076, 1.000000000000000000, 0.8660254037844387076, 1.000000000000000000, 0.8660254037844387076, 1.000000000000000000, 0.8660254037844387076, 1.000000000000000000, 0.8660254037844387076, 1.000000000000000000, 0.8660254037844387076, 1.000000000000000000, 0.8660254037844387076, 1.000000000000000000, 0.8660254037844387076, 1.000000000000000000, 0.8660254037844387076, 1.000000000000000000, 0.8660254037844387076, 1.000000000000000000, 0.8660254037844387076, 1.000000000000000000, 0.8660254037844387076, 1.000000000000000000, 0.8660254037844387076, 1.000000000000000000, 0.8660254037844387076, 1.000000000000000000, 0.8660254037844387076, 1.000000000000000000, 0.8660254037844387076, 1.000000000000000000, 0.8660254037844387076, 1.000000000000000000, 0.8660254037844387076, 1.000000000000000000, 0.8660254037844387076, 1.000000000000000000, 0.8660254037844387076, 1.000000000000000000, 0.8660254037844387076, 1.000000000000000000, 0.8660254037844387076, 1.000000000000000000, 0.8660254037844387076, 1.000000000000000000, 0.8660254037844387076, 1.000000000000000000, 0.8660254037844387076, 1.000000000000000000, 0.8660254037844387076, 1.000000000000000000, 0.8660254037844387076, 1.000000000000000000, 0.8660254037844387076, 1.000000000000000000, 0.8660254037844387076, 1.000000000000000000, 0.8660254037844387076, 1.000000000000000000, 0.8660254037844387076, 1.000000000000000000, 0.8660254037844387076, 1.000000000000000000, 0.8660254037844387076, 1.000000000000000000, 0.8660254037844387076, 1.000000000000000000, 0.8660254037844387076, 1.000000000000000000, 0.8660254037844387076, 1.000000000000000000, 0.8660254037844387076, 1.000000000000000000, 0.8660254037844387076, 1.000000000000000000, 0.8660254037844387076, 1.000000000000000000, 0.8660254037844387076, 1.000000000000000000, 0.8660254037844387076, 1.000000000000000000, 0.8660254037844387076, 1.000000000000000000, 0.8660254037844387076, 1.000000000000000000, 0.8660254037844387076, 1.000000000000000000, 0.8660254037844387076, 1.000000000000000000, 0.8660254037844387076, 1.000000000000000000, 0.8660254037844387076, 1.000000000000000000, 0.8660254037844387076, 1.000000000000000000, 0.8660254037844387076, 1.000000000000000000, 0.8660254037844387076, 1.000000000000000000, 0.8660254037844387076, 1.000000000000000000, 0.8660254037844387076, 1.000000000000000000, 0.8660254037844387076, 1.000000000000000000, 0.8660254037844387076, 1.000000000000000000, 0.8660254037844387076, 1.000000000000000000, 0.8660254037844387076, 1.000000000000000000, 0.8660254037844387076, 1.000000000000000000, 0.8660254037844387076, 1.000000000000000000, 0.8660254037844387076, 1.000000000000000000, 0.8660254037844387076, 1.000000000000000000, 0.8660254037844387076, 1.000000000000000000, 0.8660254037844387076, 1.000000000000000000, 0.8660254037844387076, 1.000000000000000000, 0.8660254037844387076, 1.000000000000000000, 0.8660254037844387076, 1.000000000000000000, 0.8660254037844387076, 1.000000000000000000, 0.8660254037844387076, 1.000000000000000000, 0.8660254037844387076, 1.000000000000000000, 0.8660254037844387076, 1.000000000000000000, 0.8660254037844387076, 1.000000000000000000, 0.8660254037844387076, 1.000000000000000000, 0.8660254037844387076, 1.000000000000000000, 0.8660254037844387076, 1.000000000000000000, 0.8660254037844387076, 1.000000000000000000, 0.8660254037844387076, 1.000000000000000000, 0.8660254037844387076, 1.000000000000000000, 0.8660254037844387076, 1.000000000000000000, 0.8660254037844387076, 1.000000000000000000, 0.8660254037844387076, 1.000000000000000000) ) ) 
 REPRESENTATION_ITEM ( '' )  SURFACE ( )  );
#209906 = CARTESIAN_POINT ( 'NONE',  ( 5.957918438201454059, 9.038323046955323292, -1.199719254218440723 ) ) ;
#209907 = DIRECTION ( 'NONE',  ( -1.000000000000000000, 0.000000000000000000, 0.000000000000000000 ) ) ;
#209908 = CARTESIAN_POINT ( 'NONE',  ( 2.846849068745292755, 6.265148313604064434, 0.000000000000000000 ) ) ;
#209909 = CARTESIAN_POINT ( 'NONE',  ( 9.499050059654537748, -8.104757123234188398, -0.1520312049662329856 ) ) ;
#209910 = CARTESIAN_POINT ( 'NONE',  ( 3.323720213644492993, 7.029424015893889433, 1.040834085586084257E-14 ) ) ;
#209911 = ORIENTED_EDGE ( 'NONE', *, *, #2058, .T. ) ;
#209912 = VECTOR ( 'NONE', #13748, 1000.000000000000000 ) ;
#209913 = DIRECTION ( 'NONE',  ( -0.000000000000000000, 1.000000000000000000, -0.000000000000000000 ) ) ;
#209914 = EDGE_CURVE ( 'NONE', #180119, #86578, #82311, .T. ) ;
#209915 = CARTESIAN_POINT ( 'NONE',  ( 10.99970480893080627, -5.907420853759282053, 0.08058608058608522640 ) ) ;
#209916 = CARTESIAN_POINT ( 'NONE',  ( 5.342795052237045539, 8.390955439988655229, -1.199719254218450271 ) ) ;
#209917 = DIRECTION ( 'NONE',  ( -1.224646799147343593E-16, 0.000000000000000000, -1.000000000000000000 ) ) ;
#209918 = CARTESIAN_POINT ( 'NONE',  ( -5.896403733238388511, 7.170697087194168873, 1.136063563240964802 ) ) ;
#209919 = CARTESIAN_POINT ( 'NONE',  ( -6.073689629242160493, 8.109057205581079231, -1.443375672974059665 ) ) ;
#209920 = CARTESIAN_POINT ( 'NONE',  ( 4.695201269034174452, 4.372156323494968966, 1.214306433183764966E-14 ) ) ;
#209921 = CARTESIAN_POINT ( 'NONE',  ( 2.377736956781382638, -1.911501772163497481, 0.4737601246572603064 ) ) ;
#209922 = CARTESIAN_POINT ( 'NONE',  ( 2.987907820627898836, -2.013986125068282007, 0.1017690403029153645 ) ) ;
#209923 = CARTESIAN_POINT ( 'NONE',  ( -7.857113714319432063, 9.125386407249497012, 1.199719254218462483 ) ) ;
#209924 = CARTESIAN_POINT ( 'NONE',  ( 6.042093733545556233, 7.078139439671806699, -1.199719254218452047 ) ) ;
#209925 = CARTESIAN_POINT ( 'NONE',  ( 6.727182134110222478, 7.629137130509071163, 2.789055895399249252 ) ) ;
#209926 = CARTESIAN_POINT ( 'NONE',  ( 4.119203469048302146, -2.097337170177868693, 0.6352863671069891582 ) ) ;
#209927 = DIRECTION ( 'NONE',  ( 0.000000000000000000, -1.000000000000000000, 0.000000000000000000 ) ) ;
#209928 = CARTESIAN_POINT ( 'NONE',  ( 2.098540742119249458, -0.5114569845777928725, -1.857200404858405207 ) ) ;
#209929 = CARTESIAN_POINT ( 'NONE',  ( -10.13202086811422475, 10.71511252242175161, -0.7998128361456291469 ) ) ;
#209930 = CARTESIAN_POINT ( 'NONE',  ( 1.284279953904121641, 3.034610286488902187, 0.7750000000000117906 ) ) ;
#209931 = CARTESIAN_POINT ( 'NONE',  ( 0.1329588055935760349, 4.094961471249922269, -2.400852151441670745 ) ) ;
#209932 = DIRECTION ( 'NONE',  ( 0.000000000000000000, -1.000000000000000000, 0.000000000000000000 ) ) ;
#209933 = CARTESIAN_POINT ( 'NONE',  ( 6.760712154708803823, 11.03924794713562818, 1.040834085586084257E-14 ) ) ;
#209934 = CARTESIAN_POINT ( 'NONE',  ( 6.810273232766058449, 6.839740281182199233, 1.040834085586084257E-14 ) ) ;
#209935 = CARTESIAN_POINT ( 'NONE',  ( -5.690973801496453710, 5.856266416803207697, -2.499999999999995115 ) ) ;
#209936 = CARTESIAN_POINT ( 'NONE',  ( 6.102578539926878598, 7.252668063737060855, -1.082531754730548412 ) ) ;
#209937 = ORIENTED_EDGE ( 'NONE', *, *, #181023, .T. ) ;
#209939 = CARTESIAN_POINT ( 'NONE',  ( 2.139316306618759711, 0.002201468654887753229, 2.013265973851806834 ) ) ;
#209938 = CARTESIAN_POINT ( 'NONE',  ( 6.005383971424570255, -1.826508537601937432, 0.2321369796495567073 ) ) ;
#209940 = CARTESIAN_POINT ( 'NONE',  ( 3.901994836520364718, 0.3331327188077978785, 2.274008445091058928 ) ) ;
#209942 = CARTESIAN_POINT ( 'NONE',  ( 2.535811996613965391, 1.140603387277869585, 1.470366759043324478 ) ) ;
#209941 = CARTESIAN_POINT ( 'NONE',  ( -0.1291982275798443380, 0.7147424134107607241, -2.157361641090648874 ) ) ;
#209943 = CARTESIAN_POINT ( 'NONE',  ( 1.642778471875001811, -2.792708332855376785, 2.845375778867859751 ) ) ;
#209944 = CARTESIAN_POINT ( 'NONE',  ( 5.080287894202283105, 0.9478536798121822704, 1.660923459347658282 ) ) ;
#209945 = CARTESIAN_POINT ( 'NONE',  ( -8.345207244411405156, 9.694828859023472134, 1.199719254218462483 ) ) ;
#209946 = CARTESIAN_POINT ( 'NONE',  ( -4.150204419558982671, 7.856005899545188242, 0.7216878364870338292 ) ) ;
#209948 = CARTESIAN_POINT ( 'NONE',  ( 3.397188523315307407, 1.473948685399184333, 1.151750840393983344 ) ) ;
#209947 = CARTESIAN_POINT ( 'NONE',  ( 5.073812392315714348, -1.160337598488449196, 1.738990438290926921 ) ) ;
#209949 = CARTESIAN_POINT ( 'NONE',  ( 5.775410249741494972, 8.721433810464993996, -1.082531754730537088 ) ) ;
#209950 = ORIENTED_EDGE ( 'NONE', *, *, #34900, .T. ) ;
#209951 = ADVANCED_FACE ( 'NONE', ( #122691 ), #120436, .F. ) ;
#209952 = CARTESIAN_POINT ( 'NONE',  ( 0.000000000000000000, 7.000000000000000000, 0.000000000000000000 ) ) ;
#209953 = DIRECTION ( 'NONE',  ( 1.000000000000000000, 0.000000000000000000, 0.000000000000000000 ) ) ;
#209954 = CARTESIAN_POINT ( 'NONE',  ( 6.604117967919251875, -1.724316898024110811, 0.05080964468639861259 ) ) ;
#209955 = CARTESIAN_POINT ( 'NONE',  ( -5.605406444246153974, 8.627059054007450101, -1.199719254218440723 ) ) ;
#209956 = CARTESIAN_POINT ( 'NONE',  ( 1.089978434334002433, -0.4226591196558672214, 1.681707840898168937 ) ) ;
#209957 = CARTESIAN_POINT ( 'NONE',  ( 1.902112725515536118, 3.289212146679096893, 0.4096023912811769252 ) ) ;
#209958 = CARTESIAN_POINT ( 'NONE',  ( -15.75000000000000000, 11.29999999999999893, 0.6999999999999992895 ) ) ;
#209959 = CARTESIAN_POINT ( 'NONE',  ( 5.770445249457275771, -0.9694031614774318850, -1.942678356158732855 ) ) ;
#209960 = CARTESIAN_POINT ( 'NONE',  ( 4.916531288042031989, 1.256637652550334883, -1.324621001416517840 ) ) ;
#209961 = CARTESIAN_POINT ( 'NONE',  ( 1.938261246079517219, -1.053878627966830184, 1.654468565904606558 ) ) ;
#209962 = CARTESIAN_POINT ( 'NONE',  ( 0.08772780073029294579, -0.5597381814076306528, 2.041856491864118439 ) ) ;
#209963 = CARTESIAN_POINT ( 'NONE',  ( -9.561524646135538319, 12.17819805862340310, -1.599625672291263179 ) ) ;
#209964 = CARTESIAN_POINT ( 'NONE',  ( 6.968000882419564945, 10.21675256520979858, 1.199719254218460707 ) ) ;
#209965 = CARTESIAN_POINT ( 'NONE',  ( 2.719513590175401063, 1.792643918890064247, 1.132349250948051500 ) ) ;
#209966 = CARTESIAN_POINT ( 'NONE',  ( -5.260200412422220140, 5.239248024021764039, -0.7216878364870207285 ) ) ;
#209967 = SURFACE_STYLE_FILL_AREA ( #92005 ) ;
#209968 = CARTESIAN_POINT ( 'NONE',  ( -5.061731940678604325, 6.567192784585701659, -1.227863150880079246 ) ) ;
#209969 = CARTESIAN_POINT ( 'NONE',  ( 0.5146170122050791607, 0.7890519337857507809, 1.914186188738425942 ) ) ;
#209971 = CARTESIAN_POINT ( 'NONE',  ( -0.7500000000000179856, 13.32291666734946389, 1.299038105676658228 ) ) ;
#209970 = CARTESIAN_POINT ( 'NONE',  ( -11.34781316621061009, 4.021557182957057996, 3.687128006872979924 ) ) ;
#209973 = VERTEX_POINT ( 'NONE', #158308 ) ;
#209972 = CARTESIAN_POINT ( 'NONE',  ( 2.965722808067718486, -1.817245444403335020, -1.277177951966218084 ) ) ;
#209974 = CARTESIAN_POINT ( 'NONE',  ( 1.143681411288837824, 0.9377895679426456743, 2.098875006570381618 ) ) ;
#209976 = CARTESIAN_POINT ( 'NONE',  ( 5.330950330247254065, -1.940297947978512960, -0.6998911787638012472 ) ) ;
#209975 = CARTESIAN_POINT ( 'NONE',  ( 4.518945272056516416, 4.166524327021037699, 0.7998128361456341429 ) ) ;
#209978 = CARTESIAN_POINT ( 'NONE',  ( -1.737500000000000266, -1.458333333333332371, -3.009438278150923907 ) ) ;
#209977 = CARTESIAN_POINT ( 'NONE',  ( 4.030516805012513082, 7.924296382481737844, 0.000000000000000000 ) ) ;
#209979 = CARTESIAN_POINT ( 'NONE',  ( 0.2329586101569866563, 0.2513371725885656938, -1.880733749865989068 ) ) ;
#209980 = B_SPLINE_CURVE_WITH_KNOTS ( 'NONE', 3,
 ( #137708, #93237, #175540, #189635, #203729, #56447, #40201 ),
 .UNSPECIFIED., .F., .F.,
 ( 4, 3, 4 ),
 ( 0.0001135037245265641654, 0.001517139415464318795, 0.002007692284160929319 ),
 .UNSPECIFIED. ) ;
#209981 = CARTESIAN_POINT ( 'NONE',  ( 6.093280168761200599, -0.6138376400152152357, 1.736067454429328416 ) ) ;
#209982 = CYLINDRICAL_SURFACE ( 'NONE', #101294, 1.000000000000000222 ) ;
#209983 = EDGE_CURVE ( 'NONE', #38200, #69383, #195260, .T. ) ;
#209984 = CARTESIAN_POINT ( 'NONE',  ( 4.704842999142070603, 5.447737239542574272, -1.199719254218452047 ) ) ;
#209985 = CARTESIAN_POINT ( 'NONE',  ( 3.082691909922595563, -0.1251556739016151387, -1.720276473149193297 ) ) ;
#209986 = CARTESIAN_POINT ( 'NONE',  ( 0.8664231474371617558, -1.968446048378743374, -0.4370742218882397445 ) ) ;
#209987 = CARTESIAN_POINT ( 'NONE',  ( 2.672825289193903942, 1.627854652907471777, 1.623211659370107363 ) ) ;
#209988 = CARTESIAN_POINT ( 'NONE',  ( 1.364683531249988535, 3.967708333674751842, -0.7879004041258239610 ) ) ;
#209989 = CARTESIAN_POINT ( 'NONE',  ( 2.882378335548450465, -1.165601267607863978, 1.938926327226223822 ) ) ;
#209990 = CARTESIAN_POINT ( 'NONE',  ( 5.039724086851991913, -1.488677873513370331, -1.490019843855681536 ) ) ;
#209991 = CARTESIAN_POINT ( 'NONE',  ( -5.804299160426224624, 9.785783097223662352, -0.7216878364870338292 ) ) ;
#209992 = CARTESIAN_POINT ( 'NONE',  ( 4.147515422935190266, 0.5979684684156804098, -1.665763606213203518 ) ) ;
#209993 = CARTESIAN_POINT ( 'NONE',  ( 6.634017235788401301, 6.634108284708264414, 0.7998128361456341429 ) ) ;
#209995 = CARTESIAN_POINT ( 'NONE',  ( -0.01123377539814351088, -0.5141151231248282105, -2.242550872947962404 ) ) ;
#209994 = CARTESIAN_POINT ( 'NONE',  ( 7.635176783151273128, 8.936736330878529699, 1.199719254218452935 ) ) ;
#209996 = CARTESIAN_POINT ( 'NONE',  ( 4.962772036422566480, 0.1772586797372834311, -1.832584332494808121 ) ) ;
#209997 = CARTESIAN_POINT ( 'NONE',  ( -4.761938266897808525, 6.578680616179308771, 1.599625672291267398 ) ) ;
#209998 = CARTESIAN_POINT ( 'NONE',  ( 4.148431815657221300, 7.783661518334664464, 1.040834085586084257E-14 ) ) ;
#209999 = CARTESIAN_POINT ( 'NONE',  ( -1.499999999999997780, 3.650000000000021227, 1.214306433183764966E-14 ) ) ;
#210000 = CARTESIAN_POINT ( 'NONE',  ( 4.084055714405177895, -2.167483682527316713, -0.3223708474724209516 ) ) ;
#210001 = CARTESIAN_POINT ( 'NONE',  ( -2.923754682041362241, 6.562797562356882608, 0.7998128361456341429 ) ) ;
#210002 = CARTESIAN_POINT ( 'NONE',  ( 0.4086240214899770073, 7.376738131363499207, -1.961326491624068913 ) ) ;
#210003 = EDGE_CURVE ( 'NONE', #123093, #136751, #210333, .T. ) ;
#210004 = LINE ( 'NONE', #82148, #52463 ) ;
#210005 = CARTESIAN_POINT ( 'NONE',  ( -1.364683531249997417, 4.509375000341424133, 1.214306433183764966E-14 ) ) ;
#210006 = CARTESIAN_POINT ( 'NONE',  ( 2.912629423498619197, 1.395154039405178903, -1.328744637545350882 ) ) ;
#210007 = CARTESIAN_POINT ( 'NONE',  ( 0.6823417656249969321, 9.026041667008065872, -1.181850606188757036 ) ) ;
#210008 = CARTESIAN_POINT ( 'NONE',  ( -3.145128448690310830, 6.613140923539910787, -0.7216878364870267237 ) ) ;
#210009 = CARTESIAN_POINT ( 'NONE',  ( 0.3873739525321840960, -2.094434250752406079, -0.7407286751721677831 ) ) ;
#210010 = ORIENTED_EDGE ( 'NONE', *, *, #29537, .T. ) ;
#210012 = SURFACE_STYLE_USAGE ( .BOTH. , #176475 ) ;
#210011 = CARTESIAN_POINT ( 'NONE',  ( 0.000000000000000000, 5.999999999999998224, 0.000000000000000000 ) ) ;
#210013 = CARTESIAN_POINT ( 'NONE',  ( 2.869522067586683711, 6.499526178826442013, 0.7998128361456362523 ) ) ;
#210014 = CARTESIAN_POINT ( 'NONE',  ( 7.721398836998350390, -5.907420853759296264, -7.721398836998385917 ) ) ;
#210015 = CARTESIAN_POINT ( 'NONE',  ( -5.602498012743507338, 5.726462300312828546, -0.1687859242097844992 ) ) ;
#210016 = CARTESIAN_POINT ( 'NONE',  ( 0.1990047979249099375, 6.441647462706413307, -3.222196616944341674 ) ) ;
#210017 = CARTESIAN_POINT ( 'NONE',  ( 2.401564422585287684, -0.6675299454344629790, -1.607540830017651023 ) ) ;
#210018 = FACE_OUTER_BOUND ( 'NONE', #83645, .T. ) ;
#210019 = CARTESIAN_POINT ( 'NONE',  ( 0.4019237886466778820, 10.85491455036742714, 1.500000000000001554 ) ) ;
#210020 = CARTESIAN_POINT ( 'NONE',  ( -1.402160292154681736E-14, 1.759375000341421469, -1.575800808251659024 ) ) ;
#210021 = CARTESIAN_POINT ( 'NONE',  ( 6.455963997168007396, 2.156291961557708525, -0.1537611777119098910 ) ) ;
#210022 = CARTESIAN_POINT ( 'NONE',  ( 6.057081135787192316, 1.604708697955498087, -1.128374156723031430 ) ) ;
#210023 = CARTESIAN_POINT ( 'NONE',  ( -9.646789991323334590, 11.21334206375407305, 1.199719254218462483 ) ) ;
#210024 = CARTESIAN_POINT ( 'NONE',  ( -4.731432421044865499, 8.463828891286912182, -0.7216878364870257245 ) ) ;
#210025 = CONICAL_SURFACE ( 'NONE', #116712, 1249.999999999991587, 0.8960553845713407073 ) ;
#210026 = CARTESIAN_POINT ( 'NONE',  ( 5.331013795412237855, 0.1550192300789655642, 2.156197635354038411 ) ) ;
#210028 = VERTEX_POINT ( 'NONE', #210223 ) ;
#210027 = CARTESIAN_POINT ( 'NONE',  ( 1.253848497529134409, -2.775557561562891351E-14, 0.5275650105875644424 ) ) ;
#210029 = CARTESIAN_POINT ( 'NONE',  ( 1.364683531249990311, 4.613541667008083103, 0.7879004041258500513 ) ) ;
#210030 = CARTESIAN_POINT ( 'NONE',  ( 0.2450992160058732550, -1.441561472518913867, -1.191725768352129622 ) ) ;
#210031 = CARTESIAN_POINT ( 'NONE',  ( 5.923113090906284128, 0.7054357044574584013, 1.584025686543149680 ) ) ;
#210032 = ADVANCED_FACE ( 'NONE', ( #160425 ), #111745, .T. ) ;
#210034 = CARTESIAN_POINT ( 'NONE',  ( 2.911879292414458309, -1.082406496695037301, -1.905547650945007776 ) ) ;
#210033 = CARTESIAN_POINT ( 'NONE',  ( -0.6801582343750247617, 0.09895833367471601472, -1.178068619123872729 ) ) ;
#210035 = CARTESIAN_POINT ( 'NONE',  ( 3.434905211628926480, 2.250879548190734436, 0.5077644651142860788 ) ) ;
#210036 = CARTESIAN_POINT ( 'NONE',  ( 5.993449436079309578, 1.557461279572001756, 1.349564693925601189 ) ) ;
#210037 = CARTESIAN_POINT ( 'NONE',  ( 0.9021669503554888836, 1.471007182523446311, -1.267884427665219471 ) ) ;
#210038 = CARTESIAN_POINT ( 'NONE',  ( -4.704316113817535339, 8.432193199521691440, 0.7216878364870458196 ) ) ;
#210040 = ADVANCED_FACE ( 'NONE', ( #128026 ), #179882, .F. ) ;
#210039 = CARTESIAN_POINT ( 'NONE',  ( 1.734723475976807094E-15, -3.469446951953614189E-15, -0.2879360613984097150 ) ) ;
#210041 = CARTESIAN_POINT ( 'NONE',  ( -6.720112740279242658, -7.154544010627095219, 6.827626583076779276 ) ) ;
#210042 = CARTESIAN_POINT ( 'NONE',  ( 4.289387122732970958, -0.003046686910593982868, -2.120778211268215419 ) ) ;
#210043 = CARTESIAN_POINT ( 'NONE',  ( -0.3868239129444561164, 2.972657967446814542, 11.65375889120575614 ) ) ;
#210044 = CARTESIAN_POINT ( 'NONE',  ( 1.916638904718031000, -1.319229391439219246, -1.525043083973671498 ) ) ;
#210045 = CARTESIAN_POINT ( 'NONE',  ( -6.087247782411500552, 7.164505836643929371, 1.082531754730549967 ) ) ;
#210046 = CARTESIAN_POINT ( 'NONE',  ( 5.245248717291847385, -1.895131572898335115, 1.130396782059706950 ) ) ;
#210047 = CARTESIAN_POINT ( 'NONE',  ( -5.646044625448194410, 5.551749915969804938, 0.000000000000000000 ) ) ;
#210048 = CARTESIAN_POINT ( 'NONE',  ( -10.30245174296173793, 3.603753425775782393, 5.948123287112152546 ) ) ;
#210049 = DIRECTION ( 'NONE',  ( -6.314299915563594049E-62, -8.546850786086437571E-32, -1.000000000000000000 ) ) ;
#210050 = CARTESIAN_POINT ( 'NONE',  ( -7.910256278930404505, 8.193330178365746619, -0.7998128361456362523 ) ) ;
#210052 = CARTESIAN_POINT ( 'NONE',  ( -4.847922445338252118, 7.813604065273374921, -1.199719254218453823 ) ) ;
#210051 = CARTESIAN_POINT ( 'NONE',  ( -4.709679585977568195, 8.347295923589904021, 0.7007048023343342980 ) ) ;
#210053 = CARTESIAN_POINT ( 'NONE',  ( -5.851773230888425381, 7.216290455326334730, 1.198155855505623535 ) ) ;
#210054 = VERTEX_POINT ( 'NONE', #29366 ) ;
#210055 = CARTESIAN_POINT ( 'NONE',  ( 5.014554672588167783, 1.422794387333496946, -1.491179163509145811 ) ) ;
#210056 = CARTESIAN_POINT ( 'NONE',  ( 4.076713200428175199, 7.699573933034834283, -0.5988845815774744841 ) ) ;
#210057 = CARTESIAN_POINT ( 'NONE',  ( -5.346851039111045978, 6.199209027673978412, -1.060622344683157747 ) ) ;
#210058 = CARTESIAN_POINT ( 'NONE',  ( -6.389970470742427189, 6.349387058821269747, -0.7998128361456291469 ) ) ;
#210059 = CARTESIAN_POINT ( 'NONE',  ( -5.178288325776719603, 5.006034233019745372, 0.000000000000000000 ) ) ;
#210060 = CARTESIAN_POINT ( 'NONE',  ( 4.178382104804970076, 0.9538709814062135139, 1.780240436319034503 ) ) ;
#210061 = CARTESIAN_POINT ( 'NONE',  ( 0.7499999999999885647, 0.5666666666666875241, -1.299038105676652899 ) ) ;
#210063 = CARTESIAN_POINT ( 'NONE',  ( 8.053180056837369705, 11.37883191874353805, -1.082531754730543083 ) ) ;
#210062 = CARTESIAN_POINT ( 'NONE',  ( -5.829079699232685208, 5.765290835385048496, 0.000000000000000000 ) ) ;
#210064 = CARTESIAN_POINT ( 'NONE',  ( 6.109920781252839994, 10.27999134477033216, 1.040834085586084257E-14 ) ) ;
#210065 = CARTESIAN_POINT ( 'NONE',  ( 3.204032760728621643, -2.058606879712703286, 0.09948017704831073338 ) ) ;
#210066 = CARTESIAN_POINT ( 'NONE',  ( 3.358046224211252095, 0.04667712216412447934, -2.016033814150198999 ) ) ;
#210067 = ORIENTED_EDGE ( 'NONE', *, *, #8236, .T. ) ;
#210068 = CARTESIAN_POINT ( 'NONE',  ( 1.902112725515556990, 3.289212146679096893, -0.4096023912812432055 ) ) ;
#210069 = CARTESIAN_POINT ( 'NONE',  ( 4.029797971759831121, 5.724516938518342535, -1.599625672291255185 ) ) ;
#210070 = AXIS2_PLACEMENT_3D ( 'NONE', #196222, #65121, #99780 ) ;
#210072 = EDGE_LOOP ( 'NONE', ( #10862, #116876, #12659, #196616, #192763, #17976, #184285, #187785 ) ) ;
#210071 = CARTESIAN_POINT ( 'NONE',  ( -0.4545350412506695692, 7.933623023433764132, -1.993241281637189832 ) ) ;
#210073 = CARTESIAN_POINT ( 'NONE',  ( 2.741564358335503382, -1.928455994415989139, -0.5879317209081732498 ) ) ;
#210074 = CARTESIAN_POINT ( 'NONE',  ( 2.361056629804247020, 1.805642548105116596, -0.3588866333120652174 ) ) ;
#210075 = CARTESIAN_POINT ( 'NONE',  ( 0.6808296902291348651, -1.277277952767090774, 1.921808783382691788 ) ) ;
#210076 = CARTESIAN_POINT ( 'NONE',  ( 6.086684617892325733, 6.065829907154645539, -0.7998128361456481317 ) ) ;
#210077 = CARTESIAN_POINT ( 'NONE',  ( 2.882270108570818223, -1.113908571083363164, 1.852364028112465810 ) ) ;
#210078 = CARTESIAN_POINT ( 'NONE',  ( 8.503988664269582998, 10.94440607977979063, 1.599625672291281386 ) ) ;
#210079 = CARTESIAN_POINT ( 'NONE',  ( -6.586563698140583512, 6.578745824119123675, 1.040834085586084257E-14 ) ) ;
#210080 = AXIS2_PLACEMENT_3D ( 'NONE', #156312, #142219, #91325 ) ;
#210081 = ORIENTED_EDGE ( 'NONE', *, *, #54609, .F. ) ;
#210082 = LINE ( 'NONE', #82218, #4245 ) ;
#210083 = CARTESIAN_POINT ( 'NONE',  ( 0.8658264364783776479, 0.9185255527898968930, 1.629538061279064642 ) ) ;
#210084 = CARTESIAN_POINT ( 'NONE',  ( 5.243030984088811408, -1.691212405323471835, 1.012918505260449464 ) ) ;
#210086 = CARTESIAN_POINT ( 'NONE',  ( 8.066738210006674237, 11.39464976410773467, 1.082531754730558626 ) ) ;
#210085 = CARTESIAN_POINT ( 'NONE',  ( -1.201851678989727383E-14, 3.821875000341423689, 1.575800808251672791 ) ) ;
#210088 = CARTESIAN_POINT ( 'NONE',  ( 0.04788047853313340263, -1.708876078042343316, -1.396090968258607790 ) ) ;
#210087 = CARTESIAN_POINT ( 'NONE',  ( -6.144869935491728441, 8.192100896205577243, -1.599625672291263179 ) ) ;
#210089 = CARTESIAN_POINT ( 'NONE',  ( 6.426242046702522082, 1.060841730010402495, 1.777776562702712226 ) ) ;
#210090 = CARTESIAN_POINT ( 'NONE',  ( 5.795220594837462436, 8.848508896363995291, -1.199719254218440723 ) ) ;
#210091 = CARTESIAN_POINT ( 'NONE',  ( -5.982172092127739482, 8.002286745614243912, -1.599625672291263179 ) ) ;
#210092 = CARTESIAN_POINT ( 'NONE',  ( 6.639320575229257670, 1.230867875982581738, 2.315960674347458781 ) ) ;
#210093 = CARTESIAN_POINT ( 'NONE',  ( 4.909034519618480807, 1.714790629392642707, 0.9726076082038226378 ) ) ;
#210094 = CARTESIAN_POINT ( 'NONE',  ( 6.152604576718359475, 1.998398145963925954, 0.2921455800133450631 ) ) ;
#210095 = CARTESIAN_POINT ( 'NONE',  ( -0.7500000000000215383, 0.9729166673494854534, 1.299038105676659116 ) ) ;
#210096 = CARTESIAN_POINT ( 'NONE',  ( 4.424672798056923817, 1.421823072290354872, -1.817590327873227052 ) ) ;
#210097 = CARTESIAN_POINT ( 'NONE',  ( 2.202078444200939789, 0.7933530804136761372, -1.904077301569401914 ) ) ;
#210098 = CARTESIAN_POINT ( 'NONE',  ( 7.131225611108088280, 9.342849184424693476, 1.443375672974076540 ) ) ;
#210099 = CARTESIAN_POINT ( 'NONE',  ( 5.529746549527311039, 7.544733289238903851, -1.599625672291281386 ) ) ;
#210100 = CARTESIAN_POINT ( 'NONE',  ( 3.413620815590684199, 7.204584394822967752, 0.7998128361456281477 ) ) ;
#210101 = CARTESIAN_POINT ( 'NONE',  ( 0.6823417656249882723, 2.238541667008084435, -1.181850606188749264 ) ) ;
#210102 = CARTESIAN_POINT ( 'NONE',  ( 5.388439706788500594, 5.251210844200210559, 0.7998128361456352531 ) ) ;
#210103 = CARTESIAN_POINT ( 'NONE',  ( 4.473827502385202770, 8.163289819517311585, 1.040834085586084257E-14 ) ) ;
#210104 = CARTESIAN_POINT ( 'NONE',  ( 4.404835846824251888, 0.5749587956990888094, 2.093619418667266530 ) ) ;
#210106 = CARTESIAN_POINT ( 'NONE',  ( 4.282634502089007533, 1.642705626968201216, -0.8318752211165170163 ) ) ;
#210105 = CARTESIAN_POINT ( 'NONE',  ( -3.470524135418306511, 5.072030796119872953, -1.443375672974053447 ) ) ;
#210108 = CARTESIAN_POINT ( 'NONE',  ( 10.32992389895506413, 1.000000000000000888, 6.106772653521394645 ) ) ;
#210107 = CARTESIAN_POINT ( 'NONE',  ( -11.92051736251533534, 11.15180243792676862, 1.381800029228856808 ) ) ;
#210109 = CARTESIAN_POINT ( 'NONE',  ( 5.038714576072483631, -1.879839391954684746, 1.126354835186346603 ) ) ;
#210110 = DIRECTION ( 'NONE',  ( -0.000000000000000000, -1.000000000000000000, -0.000000000000000000 ) ) ;
#210111 = CARTESIAN_POINT ( 'NONE',  ( 6.297788943421148922, -0.7692995465161235336, 2.127847719713715335 ) ) ;
#210112 = EDGE_LOOP ( 'NONE', ( #179215, #171432 ) ) ;
#210113 = CARTESIAN_POINT ( 'NONE',  ( -4.096253560606756494, 7.689279582349398012, -0.7399548657811344521 ) ) ;
#210114 = PLANE ( 'NONE',  #37584 ) ;
#210115 = CARTESIAN_POINT ( 'NONE',  ( 4.666526410304530970, 8.402211131567142388, 0.5382107299411863499 ) ) ;
#210116 = CARTESIAN_POINT ( 'NONE',  ( -5.031484404002922517, 6.963427452793760963, 1.443375672974058777 ) ) ;
#210117 = CARTESIAN_POINT ( 'NONE',  ( -2.985343197443135033, 6.427599869489915463, 0.3821323783160038290 ) ) ;
#210118 = CARTESIAN_POINT ( 'NONE',  ( 0.2855648877363594629, -0.8402267237041045611, 1.557686187855854554 ) ) ;
#210119 = CARTESIAN_POINT ( 'NONE',  ( 4.863935948449842783, 0.6292040250746065988, -1.912316011988722586 ) ) ;
#210120 = CARTESIAN_POINT ( 'NONE',  ( 6.928380191783277908, 8.041863964290678624, 1.199719254218462483 ) ) ;
#210121 = CARTESIAN_POINT ( 'NONE',  ( 4.313572747864121482, -0.3622951029728087580, 2.074398424781583206 ) ) ;
#210122 = CARTESIAN_POINT ( 'NONE',  ( 2.530754833220005384, -1.591195339209892312, 1.066270812275710966 ) ) ;
#210123 = CARTESIAN_POINT ( 'NONE',  ( 2.171277156482887882, 5.684907115872006145, -0.7998128361456291469 ) ) ;
#210124 = CARTESIAN_POINT ( 'NONE',  ( 3.631270037613967716, 0.05078019485712419873, -1.969077574667767783 ) ) ;
#210125 = CARTESIAN_POINT ( 'NONE',  ( 5.168225562285083896, 2.017301038980311656, -0.1031631561184200713 ) ) ;
#210126 = CARTESIAN_POINT ( 'NONE',  ( 2.149089010626914931, -1.500894351328721621, -1.116326037436713881 ) ) ;
#210129 = ORIENTED_EDGE ( 'NONE', *, *, #4927, .F. ) ;
#210128 = CARTESIAN_POINT ( 'NONE',  ( 1.810667312839256304, -0.5133170510521027907, -1.842115474350584980 ) ) ;
#210127 = CARTESIAN_POINT ( 'NONE',  ( 5.127475435434773132, -1.636205250265274191, 0.5461684234016728201 ) ) ;
#210131 = CARTESIAN_POINT ( 'NONE',  ( 4.853455804012222430, 5.725081861844796727, 1.082531754730560403 ) ) ;
#210130 = CARTESIAN_POINT ( 'NONE',  ( 1.594636444620714633, -2.196503929104542951, -0.2137616909994101977 ) ) ;
#210132 = CARTESIAN_POINT ( 'NONE',  ( 1.364683531249988535, 2.676041667008082214, 0.7879004041258500513 ) ) ;
#210133 = CARTESIAN_POINT ( 'NONE',  ( 7.618792255875527886, 10.97600916757510170, 1.199719254218460707 ) ) ;
#210134 = CARTESIAN_POINT ( 'NONE',  ( 11.41381678389391574, 12.57120581758927003, -3.704697885617874942 ) ) ;
#210135 = CARTESIAN_POINT ( 'NONE',  ( -0.9486429539237212216, 3.225839070649073825, -1.028101543438966425 ) ) ;
#210136 = CARTESIAN_POINT ( 'NONE',  ( -3.744022975668146902, 7.519777238254811813, -0.7998128361456282587 ) ) ;
#210137 = CARTESIAN_POINT ( 'NONE',  ( 6.389500218612170990, -8.186910008818841789, 7.047919418996371199 ) ) ;
#210138 = CARTESIAN_POINT ( 'NONE',  ( 1.486871883557450369, 1.994755712061954123, 0.5540851298423480342 ) ) ;
#210139 = CARTESIAN_POINT ( 'NONE',  ( 1.499999999999989120, 2.275000000000019895, 1.214306433183764966E-14 ) ) ;
#210140 = CARTESIAN_POINT ( 'NONE',  ( 6.474182045725470402, 7.511966127223233869, -1.199719254218446718 ) ) ;
#210141 = CARTESIAN_POINT ( 'NONE',  ( -6.958359152311683893, 9.141171649162195934, -1.599625672291263179 ) ) ;
#210142 = CARTESIAN_POINT ( 'NONE',  ( 5.011674058906918638, 5.875983152593414971, 1.199719254218452047 ) ) ;
#210143 = CARTESIAN_POINT ( 'NONE',  ( 0.2057307448365216507, 1.498047248056989522, 1.354806506954453482 ) ) ;
#210144 = SURFACE_SIDE_STYLE ('',( #27141 ) ) ;
#210145 = CARTESIAN_POINT ( 'NONE',  ( -1.364683531249997417, 2.509375000341422357, 1.214306433183764966E-14 ) ) ;
#210146 = ORIENTED_EDGE ( 'NONE', *, *, #192419, .F. ) ;
#210148 = CARTESIAN_POINT ( 'NONE',  ( 2.659370686574860976, 6.254349567645977714, -0.7998128361456291469 ) ) ;
#210147 = CARTESIAN_POINT ( 'NONE',  ( 6.883263157960391787, -0.001104538646235289417, 1.946037152736757925 ) ) ;
#210149 = CARTESIAN_POINT ( 'NONE',  ( 4.534529724472468715, 1.956261425488527106, -0.4871295050740409582 ) ) ;
#210150 = CARTESIAN_POINT ( 'NONE',  ( 4.663251631000405517, 1.785207739607551414, -0.6954431434487169383 ) ) ;
#210151 =( LENGTH_UNIT ( ) NAMED_UNIT ( * ) SI_UNIT ( .MILLI., .METRE. ) );
#210152 = CARTESIAN_POINT ( 'NONE',  ( 2.542740116143254347, -1.820367712357463530, 1.220030464664762393 ) ) ;
#210153 = CARTESIAN_POINT ( 'NONE',  ( -1.931056844935879147, 3.481093093210128053, 0.3999999999999836464 ) ) ;
#210154 = CARTESIAN_POINT ( 'NONE',  ( -1.500000000000015099, 1.160416667349484898, -0.8660254037844313801 ) ) ;
#210155 = CARTESIAN_POINT ( 'NONE',  ( 5.625249212676971311, 1.777412282398885823, 0.9453524948108845694 ) ) ;
#210156 = ADVANCED_BREP_SHAPE_REPRESENTATION ( '', ( #23845, #200407 ), #193485 ) ;
#210157 = CARTESIAN_POINT ( 'NONE',  ( -5.045605722580076780, 9.038290442985410067, -0.7998128361456231517 ) ) ;
#210159 = CARTESIAN_POINT ( 'NONE',  ( 5.466459189643565253, -2.065842013452086956, -0.4630074653421185071 ) ) ;
#210158 = CARTESIAN_POINT ( 'NONE',  ( -3.958617665510283601, 4.681104033592509595, -1.082531754730549967 ) ) ;
#210160 = CARTESIAN_POINT ( 'NONE',  ( -8.012344526598182026E-15, 10.10937500034140157, -1.575800808251669460 ) ) ;
#210162 = CARTESIAN_POINT ( 'NONE',  ( -7.065734331377342414, 8.272386803808890576, -1.199719254218452047 ) ) ;
#210161 = CARTESIAN_POINT ( 'NONE',  ( 3.650014318109519262, 0.7545864325827613683, 1.950000943494380135 ) ) ;
#210164 = ORIENTED_EDGE ( 'NONE', *, *, #182674, .T. ) ;
#210163 = CARTESIAN_POINT ( 'NONE',  ( 1.500562974171329333, 1.412943827846969702, -0.9888553570028703055 ) ) ;
#210165 = CARTESIAN_POINT ( 'NONE',  ( 4.869442314738527067, -1.792836814666173062, -1.132239877606910472 ) ) ;
#210166 = CARTESIAN_POINT ( 'NONE',  ( 4.801558957534076022, 8.753569217098425170, 0.7998128361456462443 ) ) ;
#210167 = EDGE_CURVE ( 'NONE', #92970, #758, #172317, .T. ) ;
#210168 = FILL_AREA_STYLE ('',( #161456 ) ) ;
#210169 = CARTESIAN_POINT ( 'NONE',  ( 6.938893903907228378E-15, 10.64264068711930733, 1.214306433183764966E-14 ) ) ;
#210170 = CYLINDRICAL_SURFACE ( 'NONE', #212866, 0.04999999999999991257 ) ;
#210171 = CARTESIAN_POINT ( 'NONE',  ( 7.006866460164219212, 7.069099046480051385, -0.7998128361456281477 ) ) ;
#210172 = VERTEX_POINT ( 'NONE', #146338 ) ;
#210173 = FACE_OUTER_BOUND ( 'NONE', #140975, .T. ) ;
#210175 = CARTESIAN_POINT ( 'NONE',  ( 1.734716041023535160, 1.690356777636679686, 0.6517371015684128022 ) ) ;
#210174 = CARTESIAN_POINT ( 'NONE',  ( 5.006703865196457492, 9.063181286029688977, 0.000000000000000000 ) ) ;
#210176 = CARTESIAN_POINT ( 'NONE',  ( -4.543954038874438162, 8.453030145328826350, 1.040834085586084257E-14 ) ) ;
#210177 = AXIS2_PLACEMENT_3D ( 'NONE', #183613, #138082, #153249 ) ;
#210178 = CARTESIAN_POINT ( 'NONE',  ( 2.354312230267378236, 5.898448035287240820, -0.7998128361456281477 ) ) ;
#210179 = EDGE_LOOP ( 'NONE', ( #11440, #154786, #53178, #143246 ) ) ;
#210180 = CARTESIAN_POINT ( 'NONE',  ( 5.200434439293556643, 8.224868058221247225, -1.199719254218452047 ) ) ;
#210181 = CARTESIAN_POINT ( 'NONE',  ( 2.385177931559249398, 0.08740048966574034961, -1.809473338476126569 ) ) ;
#210182 = CARTESIAN_POINT ( 'NONE',  ( 6.539320575229250920, 2.072231551265828475, 2.205269387046896679 ) ) ;
#210183 = FILL_AREA_STYLE ('',( #110641 ) ) ;
#210184 = CARTESIAN_POINT ( 'NONE',  ( 4.215071147998584955, 7.318223152490296535, 0.8720340548805920466 ) ) ;
#210185 = ADVANCED_FACE ( 'NONE', ( #195057 ), #106647, .F. ) ;
#210186 = CARTESIAN_POINT ( 'NONE',  ( 4.053051418270800177, 1.573051355563404252, -0.9941624863331417483 ) ) ;
#210187 = EDGE_CURVE ( 'NONE', #204424, #183827, #19990, .T. ) ;
#210188 = CARTESIAN_POINT ( 'NONE',  ( 1.335391617855705926, 0.5546556490612590817, -1.833562831147776739 ) ) ;
#210189 = CARTESIAN_POINT ( 'NONE',  ( 1.272165501999738435, -1.161393580401563375, 1.408505525491813515 ) ) ;
#210190 = CARTESIAN_POINT ( 'NONE',  ( -11.97929049433705373, 13.88000000000000078, 0.7046979865771783036 ) ) ;
#210191 = CARTESIAN_POINT ( 'NONE',  ( -4.123088111887291518, 7.824370207261548416, 0.000000000000000000 ) ) ;
#210193 = CIRCLE ( 'NONE', #106515, 0.07999999999999998779 ) ;
#210192 = VECTOR ( 'NONE', #192602, 1000.000000000000000 ) ;
#210194 = CARTESIAN_POINT ( 'NONE',  ( 4.596293493935747598, 8.372084169494645067, 0.08663659024946840370 ) ) ;
#210195 = FILL_AREA_STYLE ('',( #113855 ) ) ;
#210196 = DIRECTION ( 'NONE',  ( 0.000000000000000000, 0.000000000000000000, 1.000000000000000000 ) ) ;
#210197 = CARTESIAN_POINT ( 'NONE',  ( 6.480434237652115570, 10.50433101066207442, 0.7216878364870438212 ) ) ;
#210198 = CARTESIAN_POINT ( 'NONE',  ( 6.139503339746209321, 1.821095124518475217, -0.7503768741054758218 ) ) ;
#210199 = CARTESIAN_POINT ( 'NONE',  ( -5.901876940650454095, 5.779944607047298177, -0.7998128361456291469 ) ) ;
#210200 = CARTESIAN_POINT ( 'NONE',  ( -11.97185388258315086, 9.720000092796073687, -0.8311143155443163621 ) ) ;
#210201 = CARTESIAN_POINT ( 'NONE',  ( -0.02340959012393610192, -0.1578203421408593821, -2.056509962333047614 ) ) ;
#210202 = CARTESIAN_POINT ( 'NONE',  ( -0.7500000000000006661, 9.989583334016129967, -1.299038105676657340 ) ) ;
#210203 = CARTESIAN_POINT ( 'NONE',  ( 5.473632971755619359, 1.856580101505003411, -0.5137103415125721106 ) ) ;
#210204 = CARTESIAN_POINT ( 'NONE',  ( -7.217017841176048165, 7.314275657660511243, 1.040834085586084257E-14 ) ) ;
#210205 = CARTESIAN_POINT ( 'NONE',  ( 1.518276268637512194, 1.228937244518006011, -1.350148523839814096 ) ) ;
#210206 = CARTESIAN_POINT ( 'NONE',  ( 2.262606014870732096, 0.9450075053254001212, 1.994452002680577429 ) ) ;
#210207 = DIRECTION ( 'NONE',  ( 0.000000000000000000, 1.000000000000000000, 0.000000000000000000 ) ) ;
#210208 = FACE_OUTER_BOUND ( 'NONE', #117817, .T. ) ;
#210209 = EDGE_LOOP ( 'NONE', ( #151668, #126378, #207947, #169504 ) ) ;
#210210 = CARTESIAN_POINT ( 'NONE',  ( 0.7659823462377189918, -1.960405762330315049, 0.1893847968462581133 ) ) ;
#210211 = CARTESIAN_POINT ( 'NONE',  ( 2.788543057918268619, 1.664307371569521132, -1.000645113138714848 ) ) ;
#210212 = CARTESIAN_POINT ( 'NONE',  ( 0.3157796101352361440, -1.620936768121715499, 1.198674607299075934 ) ) ;
#210214 = CARTESIAN_POINT ( 'NONE',  ( 5.840631046605349042, -1.815184518647503742, -0.4092948386957768747 ) ) ;
#210213 = CARTESIAN_POINT ( 'NONE',  ( -5.444481204339554736, 8.509589284108232121, 1.199719254218454489 ) ) ;
#210215 = CARTESIAN_POINT ( 'NONE',  ( 6.886615681098613884, 6.999082814228660077, 0.000000000000000000 ) ) ;
#210216 = DIRECTION ( 'NONE',  ( 0.000000000000000000, 0.000000000000000000, 1.000000000000000000 ) ) ;
#210217 = CARTESIAN_POINT ( 'NONE',  ( 4.070745140982080734, 3.981847363168877774, -0.7493180678802955352 ) ) ;
#210218 = CARTESIAN_POINT ( 'NONE',  ( -4.904298879841297421, 6.744767997946721216, 1.599625672291267398 ) ) ;
#210219 = CARTESIAN_POINT ( 'NONE',  ( -6.454563648557663846, 9.688018802362710957, -1.199719254218452047 ) ) ;
#210220 = CARTESIAN_POINT ( 'NONE',  ( 1.329895901633147748, 1.076045675571284166, -1.909117696414885934 ) ) ;
#210221 = CARTESIAN_POINT ( 'NONE',  ( 5.029711800989886683, 4.970344644017389513, 1.040834085586084257E-14 ) ) ;
#210222 = CARTESIAN_POINT ( 'NONE',  ( 1.117161918529060416E-16, 3.466143782776612170, -2.000000000000000000 ) ) ;
#210223 = CARTESIAN_POINT ( 'NONE',  ( -10.49167311136684511, 5.343773310534622567, 5.730690286876297002 ) ) ;
#210224 = CARTESIAN_POINT ( 'NONE',  ( 2.226930044512597906, -0.0006860120723567450030, 1.825872481329051222 ) ) ;
#210225 = CARTESIAN_POINT ( 'NONE',  ( 1.403499169894465659, 7.376709478544011489, 4.304123474985813935 ) ) ;
#210226 = CARTESIAN_POINT ( 'NONE',  ( -5.115504031057831469, 4.862509545855891346, 0.7998128361456341429 ) ) ;
#210227 = CARTESIAN_POINT ( 'NONE',  ( -5.492869780704572769, 7.580512000422499952, -1.348893862496753249 ) ) ;
#210228 = DIRECTION ( 'NONE',  ( -1.276756478318932585E-15, 1.000000000000000000, -1.665334536937738262E-16 ) ) ;
#210229 = CARTESIAN_POINT ( 'NONE',  ( 8.055515824813896941, 12.54985222892493368, 0.7998128361456462443 ) ) ;
#210230 = CARTESIAN_POINT ( 'NONE',  ( 0.8910897993890665170, 1.699419447932304594, -0.9074141512597186932 ) ) ;
#210231 = CARTESIAN_POINT ( 'NONE',  ( 5.682460714699895554, 1.171467074228413674, -1.573401077569417605 ) ) ;
#210232 = CIRCLE ( 'NONE', #148102, 11.49999999999998934 ) ;
#210233 = CARTESIAN_POINT ( 'NONE',  ( -6.042130013184518589, 10.20090211535728031, -0.7998128361456291469 ) ) ;
#210234 = CARTESIAN_POINT ( 'NONE',  ( 6.308621549060418054, 6.254479983525607523, 0.7998128361456341429 ) ) ;
#210235 = CARTESIAN_POINT ( 'NONE',  ( 4.757479570170550787, 2.167726397749652367, -0.3216086267831194112 ) ) ;
#210236 = DIRECTION ( 'NONE',  ( 0.000000000000000000, 0.000000000000000000, -1.000000000000000000 ) ) ;
#210237 = CARTESIAN_POINT ( 'NONE',  ( 4.030184149050713316, 1.145922430192683805, 1.723988044715178081 ) ) ;
#210239 = CARTESIAN_POINT ( 'NONE',  ( -0.6823417656250212460, 0.8635416670080899859, 1.181850606188755259 ) ) ;
#210238 = CARTESIAN_POINT ( 'NONE',  ( -0.1296875068448159751, 0.001480089298542403009, -1.826395826379861864 ) ) ;
#210240 = ORIENTED_EDGE ( 'NONE', *, *, #189291, .T. ) ;
#210241 = ORIENTED_EDGE ( 'NONE', *, *, #162125, .T. ) ;
#210242 = CARTESIAN_POINT ( 'NONE',  ( 4.289826696582184518, 1.777288211397337170, -1.457785959652138530 ) ) ;
#210244 = ORIENTED_EDGE ( 'NONE', *, *, #31849, .T. ) ;
#210243 = CARTESIAN_POINT ( 'NONE',  ( 7.348156068926750883, 8.635565504245116486, -1.082531754730537976 ) ) ;
#210246 = CARTESIAN_POINT ( 'NONE',  ( 1.001543065824772753E-15, -0.7218749995220414828, 3.793834371823811669 ) ) ;
#210245 = CARTESIAN_POINT ( 'NONE',  ( 4.421367491832258523, 8.172362817197399210, 0.7216878364870257245 ) ) ;
#210247 = CARTESIAN_POINT ( 'NONE',  ( -11.41381675112460670, 13.53016735491474343, 3.704697986577268232 ) ) ;
#210248 = DIRECTION ( 'NONE',  ( -0.8660254037844382635, 0.5000000000000006661, 1.725633230170963324E-31 ) ) ;
#210249 = CARTESIAN_POINT ( 'NONE',  ( 3.486211078826762844, -0.3796756879693505837, -1.904310675543115394 ) ) ;
#210250 = ORIENTED_EDGE ( 'NONE', *, *, #127713, .T. ) ;
#210251 = CARTESIAN_POINT ( 'NONE',  ( 8.988692655735958326, 12.47026328412523988, -1.082531754730543083 ) ) ;
#210252 = EDGE_CURVE ( 'NONE', #29424, #151228, #193980, .T. ) ;
#210253 = ORIENTED_EDGE ( 'NONE', *, *, #73270, .T. ) ;
#210254 = CARTESIAN_POINT ( 'NONE',  ( 5.730699431777452446, 1.279516236652695316, -1.421498520143074540 ) ) ;
#210255 = CYLINDRICAL_SURFACE ( 'NONE', #86180, 1.250000000000000000 ) ;
#210256 = CARTESIAN_POINT ( 'NONE',  ( 6.821331452548096586, -0.1252896706360993595, 1.696280295671446448 ) ) ;
#210257 = CARTESIAN_POINT ( 'NONE',  ( 4.399625206644591557, -1.976670321813909892, 0.3981083777728141038 ) ) ;
#210258 = CARTESIAN_POINT ( 'NONE',  ( -0.4019237886467001974, 9.801335450315370679, 1.500000000000001998 ) ) ;
#210259 = CARTESIAN_POINT ( 'NONE',  ( 1.383733252933561086, 2.037972573443189717, -0.8472329510355591786 ) ) ;
#210261 = CARTESIAN_POINT ( 'NONE',  ( -4.394251184604987870, 5.259619482528146150, 1.082531754730549078 ) ) ;
#210260 = CARTESIAN_POINT ( 'NONE',  ( -9.398826802771548472, 11.98838390803207865, -1.599625672291263179 ) ) ;
#210263 = CARTESIAN_POINT ( 'NONE',  ( 0.07459516483346910476, 0.007201286963451345932, -1.755573347271717655 ) ) ;
#210262 = CARTESIAN_POINT ( 'NONE',  ( 1.939510448661335484, 0.7990184383764920018, -1.932127011870365951 ) ) ;
#210264 = CARTESIAN_POINT ( 'NONE',  ( 6.012342310302175363, -1.897698807000438359, 0.6819931642896917001 ) ) ;
#210266 = CARTESIAN_POINT ( 'NONE',  ( 3.240441643373017211, 0.5569673610456173929, 2.223450396423230391 ) ) ;
#210265 = CARTESIAN_POINT ( 'NONE',  ( 5.682802662783380754, 6.658966523782627434, 1.199719254218452935 ) ) ;
#210267 = CARTESIAN_POINT ( 'NONE',  ( 0.9545595967530025039, 0.3431710391763979073, -1.705965249089304470 ) ) ;
#210268 = CARTESIAN_POINT ( 'NONE',  ( -7.065207446497166366, 9.336104335703744539, 0.000000000000000000 ) ) ;
#210269 = CARTESIAN_POINT ( 'NONE',  ( 1.000851265249177890, 1.706856028473648257, 0.3036596661522768525 ) ) ;
#210270 = CARTESIAN_POINT ( 'NONE',  ( 1.360316468749973140, 0.5468750003413819227, -2.081668171172168513E-14 ) ) ;
#210271 = CARTESIAN_POINT ( 'NONE',  ( -11.94105721237523099, 13.40000000000000036, -1.187919463087248939 ) ) ;
#210272 = CARTESIAN_POINT ( 'NONE',  ( 0.9948528382496389932, 2.139055259286365640, 0.3712904390174593949 ) ) ;
#210273 = CARTESIAN_POINT ( 'NONE',  ( 2.096888995370162156, 1.803417055948232761, 0.9023429676050932491 ) ) ;
#210274 = CARTESIAN_POINT ( 'NONE',  ( 4.062500000000002665, -1.451031289061280205, -1.451031289060952467 ) ) ;
#210275 = CARTESIAN_POINT ( 'NONE',  ( -0.7500000000000006661, 1.639583334016154970, -1.299038105676652011 ) ) ;
#210276 = CARTESIAN_POINT ( 'NONE',  ( 6.287721633157377532, 1.330437191854600076, 1.393544807510539218 ) ) ;
#210277 = CARTESIAN_POINT ( 'NONE',  ( -1.364683531250014514, 12.33854166700806054, -0.7879004041258335089 ) ) ;
#210278 = CARTESIAN_POINT ( 'NONE',  ( 3.814843914748572207, -0.6992408500761657653, -2.108525230111441218 ) ) ;
#210279 = ORIENTED_EDGE ( 'NONE', *, *, #54844, .T. ) ;
#210280 = CARTESIAN_POINT ( 'NONE',  ( 3.188928480291387313, 8.980740528189222971, 2.451733079074398969 ) ) ;
#210281 = CARTESIAN_POINT ( 'NONE',  ( 0.000000000000000000, 3.300000000000025135, 1.561251128379126385E-14 ) ) ;
#210282 = CARTESIAN_POINT ( 'NONE',  ( 8.860417081730671995, 10.29590700256267155, 1.199719254218453823 ) ) ;
#210283 = AXIS2_PLACEMENT_3D ( 'NONE', #169792, #11280, #154623 ) ;
#210284 = CARTESIAN_POINT ( 'NONE',  ( 5.231891002347484054, 1.715934187082169604, 0.2900348964059005774 ) ) ;
#210285 = CARTESIAN_POINT ( 'NONE',  ( 4.896903505236655185, 0.3334610245491422265, 1.933150054703360654 ) ) ;
#210287 = CARTESIAN_POINT ( 'NONE',  ( -6.616015773788831211, 7.781401826584148473, 1.082531754730549967 ) ) ;
#210286 = CARTESIAN_POINT ( 'NONE',  ( 3.225950485047770933, 5.851027101609320269, 1.199719254218450271 ) ) ;
#210288 = CARTESIAN_POINT ( 'NONE',  ( 5.594708818112484217, 5.774250729507366842, 0.6894988139244704328 ) ) ;
#210289 = CARTESIAN_POINT ( 'NONE',  ( 5.097078980560620920, 1.884938936817718069, -1.250935519564094767 ) ) ;
#210290 = CARTESIAN_POINT ( 'NONE',  ( 2.066913078360913314, 1.530046405743747506, -1.383527225477628297 ) ) ;
#210291 = CARTESIAN_POINT ( 'NONE',  ( -6.181627972826976958, 9.299317504018391745, 1.199719254218452047 ) ) ;
#210292 = VERTEX_POINT ( 'NONE', #82359 ) ;
#210293 = CARTESIAN_POINT ( 'NONE',  ( 1.499999999999987121, 0.8270833340161471980, -0.8660254037844253849 ) ) ;
#210294 = CARTESIAN_POINT ( 'NONE',  ( 3.602682612693074660, 1.476495159181415939, -1.148357684351591912 ) ) ;
#210295 = CARTESIAN_POINT ( 'NONE',  ( 2.777623227853244003, 1.486122661887591123, -0.8934276201044144550 ) ) ;
#210296 = EDGE_CURVE ( 'NONE', #16835, #160077, #106501, .T. ) ;
#210297 = CARTESIAN_POINT ( 'NONE',  ( 6.163654587501778970, 1.125051486859941718, 1.880622087419632882 ) ) ;
#210298 = CARTESIAN_POINT ( 'NONE',  ( 0.9212656856641410208, 2.039593612490635532, 0.8430313063367624871 ) ) ;
#210299 = CARTESIAN_POINT ( 'NONE',  ( 3.555696680978126079, 0.5271953485486252644, -2.096301903996622862 ) ) ;
#210300 = CARTESIAN_POINT ( 'NONE',  ( 4.945229674018920107, 0.6074099038847360355, -1.844580613826458437 ) ) ;
#210301 = CARTESIAN_POINT ( 'NONE',  ( -4.243338890952911058, 5.013278796608906518, -1.082531754730543971 ) ) ;
#210304 = ORIENTED_EDGE ( 'NONE', *, *, #107353, .F. ) ;
#210303 = UNCERTAINTY_MEASURE_WITH_UNIT (LENGTH_MEASURE( 1.000000000000000082E-05 ), #71987, 'distance_accuracy_value', 'NONE');
#210302 = CARTESIAN_POINT ( 'NONE',  ( 6.925078400183548588, 0.0006614011395407459748, 1.855452278108092656 ) ) ;
#210305 = FILL_AREA_STYLE ('',( #94465 ) ) ;
#210306 = EDGE_CURVE ( 'NONE', #54687, #143545, #148051, .T. ) ;
#210307 = CARTESIAN_POINT ( 'NONE',  ( 4.254136489245101238, 7.273159757992218921, 0.9281648423343953347 ) ) ;
#210308 = FACE_OUTER_BOUND ( 'NONE', #33754, .T. ) ;
#210309 = CARTESIAN_POINT ( 'NONE',  ( -0.1401555495076401980, -1.643345231473653190, -1.339971704266910812 ) ) ;
#210310 = CARTESIAN_POINT ( 'NONE',  ( 1.360316468749949825, 2.244791667008100511, 0.7853790794158780342 ) ) ;
#210311 = CARTESIAN_POINT ( 'NONE',  ( 5.326796142270829648, 0.8146286751641409474, -1.844708973168760924 ) ) ;
#210312 = CARTESIAN_POINT ( 'NONE',  ( -8.157201976916404362, 12.66848607304450702, -0.7998128361456281477 ) ) ;
#210313 = CARTESIAN_POINT ( 'NONE',  ( 8.945682426918439845, 9.331051007693339727, 1.040834085586084257E-14 ) ) ;
#210314 = CARTESIAN_POINT ( 'NONE',  ( 10.50000000000000178, 0.000000000000000000, 3.599999999999999201 ) ) ;
#210315 = CARTESIAN_POINT ( 'NONE',  ( 2.842213963582499670, 1.811911227886909614, 0.2232855069103783507 ) ) ;
#210316 = CARTESIAN_POINT ( 'NONE',  ( 2.608667852368121043, -0.8438080161984360394, -2.039271889284439254 ) ) ;
#210317 = EDGE_LOOP ( 'NONE', ( #30423, #160148, #105141, #81542 ) ) ;
#210318 = CARTESIAN_POINT ( 'NONE',  ( -4.462041952228954500, 6.299077925724123617, -1.443375672974066548 ) ) ;
#210319 = CARTESIAN_POINT ( 'NONE',  ( 2.520459579114900261, -4.179124432053225036, -2.338646355340254779 ) ) ;
#210320 = CARTESIAN_POINT ( 'NONE',  ( -8.681298431451969222, 9.022603012982438386, 1.040834085586084257E-14 ) ) ;
#210321 = CARTESIAN_POINT ( 'NONE',  ( 0.5276105490271070231, -0.2919958673943868765, 1.998420469645475483 ) ) ;
#210322 = CARTESIAN_POINT ( 'NONE',  ( 1.067215373428985092, -1.669322716927954753, 1.307481345630675529 ) ) ;
#210323 = VERTEX_POINT ( 'NONE', #144229 ) ;
#210324 = CARTESIAN_POINT ( 'NONE',  ( -4.776215253764153346, 8.794277906025310898, -0.7998128361456362523 ) ) ;
#210325 = CARTESIAN_POINT ( 'NONE',  ( 1.551354284286353247, 1.404667267363783667, 1.220738542487237677 ) ) ;
#210326 = CARTESIAN_POINT ( 'NONE',  ( 3.948449050077836642, 5.629609863222681199, 1.599625672291267398 ) ) ;
#210327 = CARTESIAN_POINT ( 'NONE',  ( 1.112450467520700537, -0.9725818059473789745, -1.930612204972524282 ) ) ;
#210328 = CARTESIAN_POINT ( 'NONE',  ( 6.574846728087075931, -0.8593996854794653251, 1.822268861383633309 ) ) ;
#210329 = ORIENTED_EDGE ( 'NONE', *, *, #147396, .F. ) ;
#210330 = ORIENTED_EDGE ( 'NONE', *, *, #131984, .T. ) ;
#210331 = CARTESIAN_POINT ( 'NONE',  ( -8.462260433223891098, 13.02438760540324481, -0.7998128361456281477 ) ) ;
#210332 = CARTESIAN_POINT ( 'NONE',  ( 3.475057130574196407, 0.04366187338752242769, -1.825333387291371512 ) ) ;
#210333 = CIRCLE ( 'NONE', #85720, 0.7500000000000006661 ) ;
#210335 = CARTESIAN_POINT ( 'NONE',  ( -5.444063778538836829, 6.456803583937833046, -1.314021404191120901 ) ) ;
#210334 = CARTESIAN_POINT ( 'NONE',  ( -4.305596300791617814, 7.180890229968955651, 1.199719254218452935 ) ) ;
#210336 = CARTESIAN_POINT ( 'NONE',  ( 6.296370465541430761, 6.973533528358998979, 0.9269300130883666444 ) ) ;
#210337 = CARTESIAN_POINT ( 'NONE',  ( 6.784528966312857179, -1.956291195211720346, 0.4871289682274528299 ) ) ;
#210338 = CARTESIAN_POINT ( 'NONE',  ( 5.964778383650899407, 0.1308802983275309528, -1.836551591404868233 ) ) ;
#210339 = CARTESIAN_POINT ( 'NONE',  ( 0.07700591528354228110, 6.948790505698306141, -2.505847838500625979 ) ) ;
#210340 = CARTESIAN_POINT ( 'NONE',  ( 4.951972348128318657, 0.7275260799690360658, -2.190091995644850797 ) ) ;
#210341 = CARTESIAN_POINT ( 'NONE',  ( 6.527324610336440180, 6.579909898339485252, 0.7998128361456331437 ) ) ;
#210342 = CARTESIAN_POINT ( 'NONE',  ( 6.450466699499744827, 0.6713059571747861387, 2.054807225473152865 ) ) ;
#210343 = CARTESIAN_POINT ( 'NONE',  ( 1.698673089578231599, 1.615691133820891467, 1.077277171393706379 ) ) ;
#210344 = EDGE_LOOP ( 'NONE', ( #59323, #182702, #208846, #202776 ) ) ;
#210345 = CARTESIAN_POINT ( 'NONE',  ( 4.306267096541755990, -2.002170989124392175, 1.128539623919281754 ) ) ;
#210346 = DIRECTION ( 'NONE',  ( -0.000000000000000000, -1.000000000000000000, -0.000000000000000000 ) ) ;
#210347 = CARTESIAN_POINT ( 'NONE',  ( -3.383641855062333281, 6.105276709951447778, -1.199719254218452047 ) ) ;
#210348 = EDGE_CURVE ( 'NONE', #47983, #77834, #175728, .T. ) ;
#210349 = CARTESIAN_POINT ( 'NONE',  ( 4.645289301550183936, -1.446173438076237217, -1.186536486241091204 ) ) ;
#210350 = ORIENTED_EDGE ( 'NONE', *, *, #195398, .T. ) ;
#210351 = COLOUR_RGB ( '', 0.31764706, 0.68627451, 0.89019608) ;
#210354 = CARTESIAN_POINT ( 'NONE',  ( -4.423703259808839938, 8.383013913077441259, 0.7998128361456352531 ) ) ;
#210353 = CARTESIAN_POINT ( 'NONE',  ( -0.7500000000000006661, 0.1395833340161536928, -1.299038105676652011 ) ) ;
#210352 = CARTESIAN_POINT ( 'NONE',  ( 2.548957913124219044, 0.2380835140640499836, 1.897471792728817386 ) ) ;
#210355 = CARTESIAN_POINT ( 'NONE',  ( 4.020313978404310262, -1.133593497508533110, -1.893353337301090233 ) ) ;
#210356 = CARTESIAN_POINT ( 'NONE',  ( -4.326850534687610050, 7.334764357162455894, 1.087911940796560284 ) ) ;
#210357 = CARTESIAN_POINT ( 'NONE',  ( 4.227444969362701421, 3.826440640544909400, 1.214306433183764966E-14 ) ) ;
#210358 = CARTESIAN_POINT ( 'NONE',  ( 5.926322542504858681, 8.007405281046052536, -1.443375672974078761 ) ) ;
#210359 = CARTESIAN_POINT ( 'NONE',  ( -5.112833325684908559, 8.018703742390766109, -1.082531754730549967 ) ) ;
#210360 = CARTESIAN_POINT ( 'NONE',  ( 1.229685887263828770, -1.247259403286736124, -1.526659406866498481 ) ) ;
#210361 = CARTESIAN_POINT ( 'NONE',  ( 1.185104535163916228, -2.251984199834490052, -0.5028348148315447963 ) ) ;
#210362 = CARTESIAN_POINT ( 'NONE',  ( 2.330453122711079850, -1.209328770571056921, 1.544706564130463811 ) ) ;
#210363 = CARTESIAN_POINT ( 'NONE',  ( -6.445975688654486113, 6.485002823043818587, -0.7998128361456361413 ) ) ;
#210364 = CARTESIAN_POINT ( 'NONE',  ( 5.787952559958898568, -1.304071791706362449, -1.598039198280821749 ) ) ;
#210365 = CARTESIAN_POINT ( 'NONE',  ( 5.531363484695522637, 5.555604941673978558, -0.7216878364870207285 ) ) ;
#210366 = CARTESIAN_POINT ( 'NONE',  ( 3.867818961648523235, 7.734482231890414283, 1.040834085586084257E-14 ) ) ;
#210367 = ORIENTED_EDGE ( 'NONE', *, *, #105557, .T. ) ;
#210368 = CARTESIAN_POINT ( 'NONE',  ( -8.597841969360544567, 13.18256606422934674, 0.7998128361456341429 ) ) ;
#210369 = LINE ( 'NONE', #63066, #17711 ) ;
#210370 = CARTESIAN_POINT ( 'NONE',  ( 9.236128959407556849, 11.79856975744075598, -1.599625672291262513 ) ) ;
#210371 = CARTESIAN_POINT ( 'NONE',  ( 2.202231255880624516, 0.8340544509695562159, -2.004656366586863303 ) ) ;
#210372 =( LENGTH_UNIT ( ) NAMED_UNIT ( * ) SI_UNIT ( .MILLI., .METRE. ) );
#210373 = CARTESIAN_POINT ( 'NONE',  ( -1.734723475976807094E-15, 2.999999999999988898, -6.938893903907228378E-15 ) ) ;
#210374 = CARTESIAN_POINT ( 'NONE',  ( -10.48884024596653397, 1.000000000000000888, 5.608780650328914597 ) ) ;
#210375 = CARTESIAN_POINT ( 'NONE',  ( 2.688565094423268853, -0.3157439183511835945, -1.843535313746543336 ) ) ;
#210376 = CARTESIAN_POINT ( 'NONE',  ( 0.2630567961459496784, -1.839733103847444928, -0.9287307787974752316 ) ) ;
#210378 = FILL_AREA_STYLE_COLOUR ( '', #65625 ) ;
#210377 = CARTESIAN_POINT ( 'NONE',  ( 0.07775346131142897577, 0.6705917366217004627, -2.369298483346020667 ) ) ;
#210379 = CARTESIAN_POINT ( 'NONE',  ( 1.364683531249986537, -0.1364583329919154264, 0.7879004041258500513 ) ) ;
#210380 = CARTESIAN_POINT ( 'NONE',  ( 2.068876254944008508, -1.477226179422253649, 1.214308343151893510 ) ) ;
#210381 = MECHANICAL_DESIGN_GEOMETRIC_PRESENTATION_REPRESENTATION (  '', ( #203406 ), #141179 ) ;
#210382 = CARTESIAN_POINT ( 'NONE',  ( 4.486996778590452983, 1.580468086399078542, -0.7966448122273452892 ) ) ;
#210383 = CARTESIAN_POINT ( 'NONE',  ( 2.402860538037488780, -0.3286879766849961082, -1.883663324302800035 ) ) ;
#210384 = CARTESIAN_POINT ( 'NONE',  ( -4.771579997005698459, 7.654261532226910525, -1.199719254218452047 ) ) ;
#210386 = CARTESIAN_POINT ( 'NONE',  ( 5.519116348382159032, -1.729776616345682028, 0.8233883490022309015 ) ) ;
#210385 = CARTESIAN_POINT ( 'NONE',  ( 1.772826578343066117, 3.950000000000009059, 0.4499999999999590994 ) ) ;
#210387 = CARTESIAN_POINT ( 'NONE',  ( 1.499999999999985123, 0.2958333333333566517, -0.8660254037844323793 ) ) ;
#210388 = CARTESIAN_POINT ( 'NONE',  ( 6.461384246211865801, 1.636644077835234246, 1.095356925007910265 ) ) ;
#210389 = CARTESIAN_POINT ( 'NONE',  ( -0.6823417656250246877, -0.8864583329919115684, 1.181850606188755259 ) ) ;
#210390 = AXIS2_PLACEMENT_3D ( 'NONE', #78605, #30951, #146842 ) ;
#210391 = FILL_AREA_STYLE_COLOUR ( '', #117102 ) ;
#210392 = CARTESIAN_POINT ( 'NONE',  ( 5.348468966913380029, 0.5439794105128460400, 1.789823788735760646 ) ) ;
#210394 = ORIENTED_EDGE ( 'NONE', *, *, #37214, .T. ) ;
#210393 = CARTESIAN_POINT ( 'NONE',  ( 1.172165686010542274, -1.159919637379997814, 1.409874495853599141 ) ) ;
#210396 = CARTESIAN_POINT ( 'NONE',  ( 4.802738015080052492, 8.126035781178083894, 0.8349615142884360131 ) ) ;
#210395 = CARTESIAN_POINT ( 'NONE',  ( 4.494872972331320327, -0.4818267175418550208, -2.153482813429814069 ) ) ;
#210397 = CARTESIAN_POINT ( 'NONE',  ( -0.6823417656250003738, -0.7822916663252423852, -1.181850606188749264 ) ) ;
#210398 = CARTESIAN_POINT ( 'NONE',  ( 3.262228214153365169, -2.060424958539575524, 0.09861793142403557644 ) ) ;
#210399 = CARTESIAN_POINT ( 'NONE',  ( -6.679363233026820446, 10.94434087183997129, 0.000000000000000000 ) ) ;
#210400 = FILL_AREA_STYLE ('',( #176851 ) ) ;
#210401 = CARTESIAN_POINT ( 'NONE',  ( 8.191097360950562845, 12.70803068775103739, -0.7998128361456352531 ) ) ;
#210402 = CARTESIAN_POINT ( 'NONE',  ( 1.300105796840295813, 3.592889250479052610, 0.4336863642760066528 ) ) ;
#210403 = CARTESIAN_POINT ( 'NONE',  ( 1.347111479062088405E-15, 5.999999999999998224, 11.00000000000000000 ) ) ;
#210404 = CARTESIAN_POINT ( 'NONE',  ( 5.885121196783658526, 9.023669275293071834, 1.199719254218452047 ) ) ;
#210405 = VERTEX_POINT ( 'NONE', #66082 ) ;
#210406 = CARTESIAN_POINT ( 'NONE',  ( 5.635237798060349412, -0.04710594754482424346, -2.069988403558701062 ) ) ;
#210407 = CARTESIAN_POINT ( 'NONE',  ( 1.364683531249988757, -0.05312499965857975237, 0.000000000000000000 ) ) ;
#210408 = CARTESIAN_POINT ( 'NONE',  ( 2.935029080331118756, 0.2613785356864756770, 2.145644965459513109 ) ) ;
#210409 = CARTESIAN_POINT ( 'NONE',  ( -4.896236220255085314, 8.042264628280536343, 0.9566786516278618091 ) ) ;
#210410 = CARTESIAN_POINT ( 'NONE',  ( 3.018227828326583762, -2.017275923677069205, 0.1012127129823153504 ) ) ;
#210411 = CARTESIAN_POINT ( 'NONE',  ( 6.720655732516626735, 6.034942950145537388, 2.668627893128409756 ) ) ;
#210412 = B_SPLINE_CURVE_WITH_KNOTS ( 'NONE', 1,
 ( #103181, #120575 ),
 .UNSPECIFIED., .F., .F.,
 ( 2, 2 ),
 ( 0.2143153648627435515, 0.6378831769527150142 ),
 .UNSPECIFIED. ) ;
#210413 = ORIENTED_EDGE ( 'NONE', *, *, #91968, .F. ) ;
#210415 = CARTESIAN_POINT ( 'NONE',  ( 8.297226821883377568, 8.782445501726501291, -0.7216878364870267237 ) ) ;
#210414 = CARTESIAN_POINT ( 'NONE',  ( 3.475000000000000533, -0.4958333333333350690, -2.006292185433951047 ) ) ;
#210416 = CARTESIAN_POINT ( 'NONE',  ( -3.309598895067336510, 6.875299454304925284, 0.000000000000000000 ) ) ;
#210417 = CARTESIAN_POINT ( 'NONE',  ( 1.868375392651611122, -1.978555653031977446, -0.3886301775877995524 ) ) ;
#210418 = CARTESIAN_POINT ( 'NONE',  ( 6.269083535738129598, 2.097726667780253074, -0.6343229546324488100 ) ) ;
#210419 = CARTESIAN_POINT ( 'NONE',  ( 0.7499999999999920064, 5.264583334016151639, 1.299038105676669330 ) ) ;
#210420 = CARTESIAN_POINT ( 'NONE',  ( 5.009976098083095408, -0.6827417919906975108, 1.786564173047608062 ) ) ;
#210421 = CARTESIAN_POINT ( 'NONE',  ( -3.144601563365788444, 5.756120026313656268, -1.199719254218452935 ) ) ;
#210422 = CARTESIAN_POINT ( 'NONE',  ( 4.948362878863507675, 8.716914425408678113, -0.7216878364870267237 ) ) ;
#210424 = CARTESIAN_POINT ( 'NONE',  ( 3.339470413395662085, 0.4871825726840799398, -1.956567533273507964 ) ) ;
#210423 = CARTESIAN_POINT ( 'NONE',  ( -8.554831740098665094, 11.00372300158037042, 1.443375672974064550 ) ) ;
#210425 = CARTESIAN_POINT ( 'NONE',  ( 0.6823417656249934904, 13.50520833367473195, 1.181850606188764807 ) ) ;
#210426 = CARTESIAN_POINT ( 'NONE',  ( -3.383641855062333281, 6.105276709951447778, -1.199719254218452047 ) ) ;
#210427 = CARTESIAN_POINT ( 'NONE',  ( 4.752814332062330394, -1.383916046847250669, 1.029161146002472549 ) ) ;
#210428 = CARTESIAN_POINT ( 'NONE',  ( -0.1399997263889611598, 2.874570648431204578, -2.488748559936367233 ) ) ;
#210429 = CARTESIAN_POINT ( 'NONE',  ( 9.571693261567954636, 12.19006144329456731, 1.443375672974076540 ) ) ;
#210430 = CARTESIAN_POINT ( 'NONE',  ( -3.380278471875000523, -0.05468749976102194044, 0.000000000000000000 ) ) ;
#210431 = CARTESIAN_POINT ( 'NONE',  ( 6.471393748265543699, 5.229711127717882491, 2.420000000000010587 ) ) ;
#210432 = CARTESIAN_POINT ( 'NONE',  ( 1.200149190772631158, 0.8425179731405306738, -1.891261800508976298 ) ) ;
#210433 = DIRECTION ( 'NONE',  ( 0.000000000000000000, 0.000000000000000000, 1.000000000000000000 ) ) ;
#210434 = VERTEX_POINT ( 'NONE', #32553 ) ;
#210435 = CARTESIAN_POINT ( 'NONE',  ( 5.215404452620196807, 1.484227587358154077, 1.038217761341611922 ) ) ;
#210436 = CARTESIAN_POINT ( 'NONE',  ( 6.690022453700429139, 6.769724048930809701, 0.7998128361456331437 ) ) ;
#210437 = FACE_OUTER_BOUND ( 'NONE', #188428, .T. ) ;
#210438 = CARTESIAN_POINT ( 'NONE',  ( 6.533875575962896143, -1.755123972569608615, 0.4478894030855648523 ) ) ;
#210439 = CARTESIAN_POINT ( 'NONE',  ( 5.682275777458846377, 7.722684055159064975, 1.443375672974064550 ) ) ;
#210440 =( GEOMETRIC_REPRESENTATION_CONTEXT ( 3 ) GLOBAL_UNCERTAINTY_ASSIGNED_CONTEXT ( ( #32091 ) ) GLOBAL_UNIT_ASSIGNED_CONTEXT ( ( #209041, #214083, #68915 ) ) REPRESENTATION_CONTEXT ( 'NONE', 'WORKASPACE' ) );
#210441 = CARTESIAN_POINT ( 'NONE',  ( 1.651133652709662947, 0.8391591008036050070, 1.022755049771794988 ) ) ;
#210442 = CARTESIAN_POINT ( 'NONE',  ( 2.554835828347111093, -1.907293181126702653, -1.079063956894068754 ) ) ;
#210443 = ORIENTED_EDGE ( 'NONE', *, *, #163845, .F. ) ;
#210444 = ADVANCED_FACE ( 'NONE', ( #112813 ), #137844, .T. ) ;
#210446 = CARTESIAN_POINT ( 'NONE',  ( 7.567422294721922960, 11.98040977715095323, 0.7998128361456462443 ) ) ;
#210445 = CARTESIAN_POINT ( 'NONE',  ( 0.3089402658475807195, -1.578002999302514642, 1.165503548361209063 ) ) ;
#210447 = CARTESIAN_POINT ( 'NONE',  ( 4.517137023955775099, -1.749796063449124084, 0.7800368752974867759 ) ) ;
#210448 = FACE_OUTER_BOUND ( 'NONE', #85929, .T. ) ;
#210449 = CARTESIAN_POINT ( 'NONE',  ( -6.457230086593013674, 6.786253674495239530, 0.3580049749655131452 ) ) ;
#210450 = FILL_AREA_STYLE ('',( #78325 ) ) ;
#210451 = CARTESIAN_POINT ( 'NONE',  ( 1.364683531249986537, -0.5947916663252456049, -0.7879004041258309554 ) ) ;
#210453 = ORIENTED_EDGE ( 'NONE', *, *, #187293, .F. ) ;
#210452 = CARTESIAN_POINT ( 'NONE',  ( 5.666945020832177882, 6.674152614801420746, 1.082531754730558626 ) ) ;
#210454 = CARTESIAN_POINT ( 'NONE',  ( -7.212574532790087645, 11.35849468832304154, -0.7216878364870267237 ) ) ;
#210455 = CARTESIAN_POINT ( 'NONE',  ( 2.254944280175336324, -1.671361177491991201, 1.370965666894090385 ) ) ;
#210456 = CARTESIAN_POINT ( 'NONE',  ( -3.149236820124241110, 6.896136400112061970, -0.7998128361456481317 ) ) ;
#210457 = CARTESIAN_POINT ( 'NONE',  ( 4.740510986633625024, 5.559626234941203116, -1.199719254218450271 ) ) ;
#210458 = CARTESIAN_POINT ( 'NONE',  ( 1.483130931141176889, 1.688290157389197077, -0.6950536248920418103 ) ) ;
#210459 = DIRECTION ( 'NONE',  ( -0.9989777552170298058, -5.711963089865910869E-16, -0.04520447523801467832 ) ) ;
#210460 = CARTESIAN_POINT ( 'NONE',  ( 5.122008332510333162, -0.9777984688263160473, -1.541441239866998103 ) ) ;
#210461 = EDGE_CURVE ( 'NONE', #166319, #179385, #23706, .T. ) ;
#210462 = CARTESIAN_POINT ( 'NONE',  ( 8.521429491328973427, 12.47146749443822422, 8.416430775921163843 ) ) ;
#210463 = CARTESIAN_POINT ( 'NONE',  ( 2.865378420500460876, -1.565876230000915692, -1.097592462808501645 ) ) ;
#210464 = VERTEX_POINT ( 'NONE', #151647 ) ;
#210465 = CARTESIAN_POINT ( 'NONE',  ( 3.771889708208826075, -1.940809680921409486, 0.3342159591338197400 ) ) ;
#210466 = ORIENTED_EDGE ( 'NONE', *, *, #41782, .F. ) ;
#210467 = CARTESIAN_POINT ( 'NONE',  ( 5.653840721119872903, 0.7909470656678599942, 1.773883556849734644 ) ) ;
#210468 = ORIENTED_EDGE ( 'NONE', *, *, #58497, .T. ) ;
#210469 = CARTESIAN_POINT ( 'NONE',  ( -5.803772275101700906, 8.928762199997411386, -1.199719254218452047 ) ) ;
#210471 = CARTESIAN_POINT ( 'NONE',  ( 5.519825572852568030, -0.5132647233585425628, 2.057443900658859182 ) ) ;
#210470 = CARTESIAN_POINT ( 'NONE',  ( 5.006703865196457492, 9.063181286029688977, 0.000000000000000000 ) ) ;
#210472 = CARTESIAN_POINT ( 'NONE',  ( 7.146556367734771875, 8.470642196179646533, 1.082531754730549967 ) ) ;
#210474 = ORIENTED_EDGE ( 'NONE', *, *, #159272, .T. ) ;
#210473 = CARTESIAN_POINT ( 'NONE',  ( 4.213462193461685601, 1.537813053725526569, 1.136448645172025262 ) ) ;
#210475 = CARTESIAN_POINT ( 'NONE',  ( 4.774589472192324102, 6.991777125168484375, -1.402305405395011251 ) ) ;
#210476 = CARTESIAN_POINT ( 'NONE',  ( 1.499999999999985789, -1.099999999999982991, 0.000000000000000000 ) ) ;
#210477 = CARTESIAN_POINT ( 'NONE',  ( 0.2884678563945877738, -1.037960011796670523, 1.947446179978419512 ) ) ;
#210478 = CARTESIAN_POINT ( 'NONE',  ( 5.373694559265936199, 0.3904673514037678150, -1.974700560916352154 ) ) ;
#210479 = CARTESIAN_POINT ( 'NONE',  ( -11.41381675112453387, 19.00000000000000000, -3.704697986577182522 ) ) ;
#210480 = CARTESIAN_POINT ( 'NONE',  ( 6.199803715563785289, -0.6102442156579389598, 1.720816905678754782 ) ) ;
#210481 = CARTESIAN_POINT ( 'NONE',  ( 0.9067890187421032699, 0.5993529260880943177, 1.981728858978973218 ) ) ;
#210482 = CARTESIAN_POINT ( 'NONE',  ( -6.724481002698115439, 10.78905223654906109, -0.7216878364870267237 ) ) ;
#210483 = AXIS2_PLACEMENT_3D ( 'NONE', #95182, #12818, #209953 ) ;
#210484 = CARTESIAN_POINT ( 'NONE',  ( -6.165548087794384458, 6.979908488848794335, -0.9162763116292941268 ) ) ;
#210485 = CARTESIAN_POINT ( 'NONE',  ( -1.225000000000033396, 2.062500000682796042, -2.949029909160572061E-14 ) ) ;
#210486 = CARTESIAN_POINT ( 'NONE',  ( 6.578970801323708706, -0.09418725797194843485, -1.868394071727994543 ) ) ;
#210487 = CARTESIAN_POINT ( 'NONE',  ( 5.452350330990040739, 9.512825819463730070, 0.7998128361456462443 ) ) ;
#210488 = CARTESIAN_POINT ( 'NONE',  ( -4.111146893441842920, 5.819424013814012753, 1.599625672291267175 ) ) ;
#210489 = B_SPLINE_CURVE_WITH_KNOTS ( 'NONE', 3,
 ( #57299, #189426, #10657, #11725, #191540, #41067, #125578 ),
 .UNSPECIFIED., .F., .F.,
 ( 4, 3, 4 ),
 ( 0.0001126021370637016465, 0.0006031550062628992376, 0.002006790698585265206 ),
 .UNSPECIFIED. ) ;
#210490 = CARTESIAN_POINT ( 'NONE',  ( 4.162516854595432747, 4.815023404238158555, 1.199719254218464037 ) ) ;
#210491 = CARTESIAN_POINT ( 'NONE',  ( -1.364683531250000748, 11.17187500034139802, 0.000000000000000000 ) ) ;
#210492 = CARTESIAN_POINT ( 'NONE',  ( -5.111587607552082524, 5.922272616020886282, 1.199719254218450271 ) ) ;
#210494 = CARTESIAN_POINT ( 'NONE',  ( -7.445362632559989535, 8.715286488521982733, 1.199719254218452047 ) ) ;
#210493 = CARTESIAN_POINT ( 'NONE',  ( -11.86145017354119879, 11.00485634456123840, -1.100000000000000533 ) ) ;
#210495 = CARTESIAN_POINT ( 'NONE',  ( 3.445721922217106936, -1.531427584095602867, -0.8135701209448819027 ) ) ;
#210496 = CARTESIAN_POINT ( 'NONE',  ( -3.581325132304157943, 7.329963087663487364, -0.7998128361456281477 ) ) ;
#210497 = CIRCLE ( 'NONE', #58365, 0.05000000000000002359 ) ;
#210498 = CARTESIAN_POINT ( 'NONE',  ( 1.200149190772631158, 0.8425179731405306738, -1.891261800508976298 ) ) ;
#210499 = CARTESIAN_POINT ( 'NONE',  ( 2.073964263283359699, -0.9022394416563597197, 1.915483482535395909 ) ) ;
#210500 = CARTESIAN_POINT ( 'NONE',  ( 4.168242161197552420, 6.950367390450747251, -1.199719254218452047 ) ) ;
#210501 = CARTESIAN_POINT ( 'NONE',  ( 7.052212457402625922, 11.37933163361175382, -0.7998128361456291469 ) ) ;
#210502 = FACE_OUTER_BOUND ( 'NONE', #31017, .T. ) ;
#210503 = CARTESIAN_POINT ( 'NONE',  ( 0.7605272443651526215, -0.6583816729706105653, -1.856300379560266833 ) ) ;
#210504 = CARTESIAN_POINT ( 'NONE',  ( 4.618624277135228162, 7.133842259902017702, 1.345135577604664512 ) ) ;
#210505 = CARTESIAN_POINT ( 'NONE',  ( 3.877268743828258479, 7.467304601200877023, 0.7216878364870298324 ) ) ;
#210507 = CARTESIAN_POINT ( 'NONE',  ( 5.138177029454847222, 6.057256624861201644, 1.082531754730560403 ) ) ;
#210506 = CARTESIAN_POINT ( 'NONE',  ( 3.475000000000000533, -1.895833333333332815, -2.006292185433951047 ) ) ;
#210508 = CARTESIAN_POINT ( 'NONE',  ( 2.168323659614699750, -1.408312831382242614, 1.808550206204377009 ) ) ;
#210509 = CARTESIAN_POINT ( 'NONE',  ( 0.5393321728033515505, -1.288848960320065462, -1.293324666950084190 ) ) ;
#210510 = CARTESIAN_POINT ( 'NONE',  ( 3.867365959033176814, -1.592763314076732106, -1.058159689705892692 ) ) ;
#210511 = CARTESIAN_POINT ( 'NONE',  ( 6.150558962454855561, 7.204682206732687000, 1.199719254218452047 ) ) ;
#210512 = CARTESIAN_POINT ( 'NONE',  ( 7.090551149822735155, 9.295395646258437949, 1.443375672974076540 ) ) ;
#210513 = CARTESIAN_POINT ( 'NONE',  ( -8.402302512167102222, 10.82577223566020841, -1.599625672291263179 ) ) ;
#210514 = EDGE_CURVE ( 'NONE', #161745, #9995, #36802, .T. ) ;
#210515 = CARTESIAN_POINT ( 'NONE',  ( 1.652591521987197831, 1.991881122867325660, 0.2913371046347946747 ) ) ;
#210516 = CARTESIAN_POINT ( 'NONE',  ( 1.674581101246939374, 1.321464807213859505, -1.450045219730737633 ) ) ;
#210517 = CARTESIAN_POINT ( 'NONE',  ( -7.621654909176601045, 12.04368116068139472, 0.7998128361456481317 ) ) ;
#210518 = CARTESIAN_POINT ( 'NONE',  ( -7.039708073993679704, 9.236078724457858158, 1.599625672291283607 ) ) ;
#210519 = CARTESIAN_POINT ( 'NONE',  ( -7.446209719563359641, -5.223431457505076203, -8.064677165291183059 ) ) ;
#210521 = CARTESIAN_POINT ( 'NONE',  ( 3.713518252986651724, -1.743675808792734205, 0.3021571867034832382 ) ) ;
#210520 = CARTESIAN_POINT ( 'NONE',  ( 4.628904841183094199, -1.911603206638176511, 0.8469096376574613005 ) ) ;
#210522 = CARTESIAN_POINT ( 'NONE',  ( -1.878313713276878127, 14.99999999999692157, 12.68000002627078082 ) ) ;
#210524 = CARTESIAN_POINT ( 'NONE',  ( 6.714806895146447907, -0.1657305019511661481, 2.255884130952827249 ) ) ;
#210523 = CARTESIAN_POINT ( 'NONE',  ( 1.598423149420349132, 8.713846000021357341, -2.499999999999988898 ) ) ;
#210525 = CARTESIAN_POINT ( 'NONE',  ( 4.154071219024037198, -1.287471232310585467, 1.171156097612672253 ) ) ;
#210526 = CARTESIAN_POINT ( 'NONE',  ( 10.22692794340986921, 10.82583744360002243, 0.000000000000000000 ) ) ;
#210527 =( GEOMETRIC_REPRESENTATION_CONTEXT ( 3 ) GLOBAL_UNCERTAINTY_ASSIGNED_CONTEXT ( ( #1684 ) ) GLOBAL_UNIT_ASSIGNED_CONTEXT ( ( #105985, #23597, #178409 ) ) REPRESENTATION_CONTEXT ( 'NONE', 'WORKASPACE' ) );
#210528 = CARTESIAN_POINT ( 'NONE',  ( -0.1104750535120268828, 5.720715034752038797, -2.697548938405624597 ) ) ;
#210529 = CARTESIAN_POINT ( 'NONE',  ( 4.991369361657826964, 1.659364262194364725, 0.5025568866975324012 ) ) ;
#210530 =( BOUNDED_CURVE ( )  B_SPLINE_CURVE ( 2, ( #127481, #157765, #206488 ),
 .UNSPECIFIED., .F., .T. ) 
 B_SPLINE_CURVE_WITH_KNOTS ( ( 3, 3 ),
 ( 0.5204868702216902676, 0.5236290400471614870 ),
 .UNSPECIFIED. ) 
 CURVE ( )  GEOMETRIC_REPRESENTATION_ITEM ( )  RATIONAL_B_SPLINE_CURVE ( ( 0.9334758596551839815, 0.9292753537475906267, 0.9631703981915431534 ) ) 
 REPRESENTATION_ITEM ( '' )  );
#210531 = CARTESIAN_POINT ( 'NONE',  ( 4.598189031992506948, 0.9324077545292840385, -1.960920063828344384 ) ) ;
#210532 = CARTESIAN_POINT ( 'NONE',  ( 2.659370686574860976, 6.254349567645977714, -0.7998128361456291469 ) ) ;
#210533 = CARTESIAN_POINT ( 'NONE',  ( -0.1353153266233823870, -2.055576600424202649, -0.5074567962913156816 ) ) ;
#210534 = CARTESIAN_POINT ( 'NONE',  ( 6.343749999995762501, 1.895863743059895246, 0.7852924748296488122 ) ) ;
#210535 = CARTESIAN_POINT ( 'NONE',  ( 0.7499999999999902300, 5.597916667349482900, -1.299038105676658228 ) ) ;
#210536 = CARTESIAN_POINT ( 'NONE',  ( 3.663036927850862323, -1.698304795282145063, -0.9092769472496107230 ) ) ;
#210537 = CARTESIAN_POINT ( 'NONE',  ( -1.500000000000008216, 10.28125000068279249, 3.469446951953614189E-15 ) ) ;
#210538 = CARTESIAN_POINT ( 'NONE',  ( 6.539320575229294441, -0.001643797937642132567, 2.203502507913539521 ) ) ;
#210539 = VERTEX_POINT ( 'NONE', #150584 ) ;
#210540 = CARTESIAN_POINT ( 'NONE',  ( 6.883263157960370471, 7.052343128562386987, 2.644342559190917541 ) ) ;
#210541 = CARTESIAN_POINT ( 'NONE',  ( 1.499999999999989120, 2.525000000000020339, 1.214306433183764966E-14 ) ) ;
#210542 = CARTESIAN_POINT ( 'NONE',  ( 4.798696304233017074, 7.685897223992134819, -1.199719254218452047 ) ) ;
#210543 = CARTESIAN_POINT ( 'NONE',  ( 2.772393654007713870, 2.210366155326251025, -0.2202761458626761870 ) ) ;
#210544 = CARTESIAN_POINT ( 'NONE',  ( -15.75000000000000000, 12.69999999999998153, 1.799999999999999600 ) ) ;
#210545 = CARTESIAN_POINT ( 'NONE',  ( 5.978782553946477840, 9.919070713005490703, 1.040834085586084257E-14 ) ) ;
#210546 = CARTESIAN_POINT ( 'NONE',  ( -8.446366511189330240, 12.79791866312216442, 0.7216878364870317197 ) ) ;
#210547 = CARTESIAN_POINT ( 'NONE',  ( 8.014278199453778839, 8.522615118883788199, 0.000000000000000000 ) ) ;
#210548 = CARTESIAN_POINT ( 'NONE',  ( 0.3873425458618062200, -0.6819987885887256462, -1.897696807414723796 ) ) ;
#210550 = CARTESIAN_POINT ( 'NONE',  ( 5.775849841709651322, -2.013224797598807569, 0.4483296186361291902 ) ) ;
#210549 = CARTESIAN_POINT ( 'NONE',  ( 9.240045382913317340, 10.73880668727576015, -1.199719254218446718 ) ) ;
#210551 = CARTESIAN_POINT ( 'NONE',  ( 11.84668730067608600, 19.00000000000000000, -1.320000000000001616 ) ) ;
#210552 = CARTESIAN_POINT ( 'NONE',  ( -5.427341564172148303, 5.226320001155936090, 0.000000000000000000 ) ) ;
#210553 = CARTESIAN_POINT ( 'NONE',  ( 0.7499999999999902300, 5.347916667349482012, -1.299038105676658228 ) ) ;
#210554 = CARTESIAN_POINT ( 'NONE',  ( -1.364683531250012516, 0.5302083336747518416, 0.7879004041258379498 ) ) ;
#210555 = CARTESIAN_POINT ( 'NONE',  ( 6.837182164354378422, -1.670574593475544489, 0.8415915117672703172 ) ) ;
#210556 = CARTESIAN_POINT ( 'NONE',  ( 5.889268099914369614, -0.6330491082502353040, -1.614684210577774115 ) ) ;
#210557 = CARTESIAN_POINT ( 'NONE',  ( 5.179165720741062628, 1.174484231026547976, 1.284593650646998375 ) ) ;
#210558 = EDGE_CURVE ( 'NONE', #64100, #92493, #58206, .T. ) ;
#210559 = CARTESIAN_POINT ( 'NONE',  ( 2.947136817621052618, -1.875550406973557349, -1.317825558608209713 ) ) ;
#210560 = CARTESIAN_POINT ( 'NONE',  ( -1.402160292154681736E-14, -0.1781249996585796136, 1.575800808251672791 ) ) ;
#210561 = CARTESIAN_POINT ( 'NONE',  ( 1.587592257565925813, -1.832131100469553520, -0.1817911664281982032 ) ) ;
#210562 = FACE_BOUND ( 'NONE', #88203, .T. ) ;
#210563 = CARTESIAN_POINT ( 'NONE',  ( 2.406250000000001776, 1.895863743164033277, -0.7852924748301132185 ) ) ;
#210564 = CARTESIAN_POINT ( 'NONE',  ( 1.711645973048509850, -1.812212506298327197, 0.2199163931802459171 ) ) ;
#210565 = CARTESIAN_POINT ( 'NONE',  ( 2.883435573726996548, -0.5880205015329244000, -1.928751729079546173 ) ) ;
#210566 = CARTESIAN_POINT ( 'NONE',  ( 1.781448188194576066, 1.512826363221421833, 1.585725795389548942 ) ) ;
#210567 = CARTESIAN_POINT ( 'NONE',  ( 9.272768930052142977, 15.45663049227336039, -8.558335171112736006 ) ) ;
#210568 = CARTESIAN_POINT ( 'NONE',  ( 4.770599357992978184, -1.377743202910805875, 1.592837501749831519 ) ) ;
#210569 = CARTESIAN_POINT ( 'NONE',  ( -6.925517538482230506, 6.974191971184389160, 0.7998128361456341429 ) ) ;
#210570 = CARTESIAN_POINT ( 'NONE',  ( 7.837025389534266751, 13.96141657329141061, 9.967208473298693860 ) ) ;
#210571 = CARTESIAN_POINT ( 'NONE',  ( 1.170471352854907776, -0.9292243337341490328, -1.850172451097586990 ) ) ;
#210572 = CARTESIAN_POINT ( 'NONE',  ( 3.994848817520957773, 7.812407387083109001, 1.040834085586084257E-14 ) ) ;
#210573 = CARTESIAN_POINT ( 'NONE',  ( -1.360316468750066843, -0.09895833299191045263, -0.7853790794159082322 ) ) ;
#210574 = CARTESIAN_POINT ( 'NONE',  ( 4.301511568767760529, 1.893648340000140040, -0.9544086401246790752 ) ) ;
#210575 = ITEM_DEFINED_TRANSFORMATION ( 'NONE', 'NONE', #187122,  #200407 ) ;
#210576 = B_SPLINE_CURVE_WITH_KNOTS ( 'NONE', 3,
 ( #40022, #106134, #121347, #124554, #38952, #57332, #105034, #155905, #42169, #189460 ),
 .UNSPECIFIED., .F., .F.,
 ( 4, 3, 3, 4 ),
 ( 0.000000000000000000, 0.0001239189758929266515, 0.0002508800143817408444, 0.0003785579584827512443 ),
 .UNSPECIFIED. ) ;
#210578 = ADVANCED_FACE ( 'NONE', ( #117062 ), #69284, .T. ) ;
#210577 = CARTESIAN_POINT ( 'NONE',  ( 6.305291373979138747, 1.520805759102667132, 1.009792402853857407 ) ) ;
#210579 = ORIENTED_EDGE ( 'NONE', *, *, #59736, .T. ) ;
#210580 = CARTESIAN_POINT ( 'NONE',  ( -4.620296487206990932, 8.612372678375294299, 0.000000000000000000 ) ) ;
#210581 = CARTESIAN_POINT ( 'NONE',  ( 8.238550898598388628, 12.76339314834017102, 0.7998128361456462443 ) ) ;
#210582 = CARTESIAN_POINT ( 'NONE',  ( 6.549997608733495902, 7.774656977344789333, -1.082531754730548412 ) ) ;
#210583 = CARTESIAN_POINT ( 'NONE',  ( 1.737499999999999378, -1.822916665710751172, -3.009438278150925683 ) ) ;
#210584 = AXIS2_PLACEMENT_3D ( 'NONE', #115103, #185351, #20706 ) ;
#210585 = CARTESIAN_POINT ( 'NONE',  ( -4.394814349124112951, 8.279033840620114049, -0.7998128361456281477 ) ) ;
#210586 = CARTESIAN_POINT ( 'NONE',  ( 6.416280414004661203, -2.120105685773795212, 0.05337830808049835035 ) ) ;
#210587 = CARTESIAN_POINT ( 'NONE',  ( 0.8332068151313138937, 0.1548093300561304564, 2.100314307419436588 ) ) ;
#210588 = CARTESIAN_POINT ( 'NONE',  ( -4.522526758610270647, 7.433975764090723359, -1.199719254218453823 ) ) ;
#210589 = CARTESIAN_POINT ( 'NONE',  ( 9.077347539549325717, 10.54899253668443393, -1.199719254218446718 ) ) ;
#210590 = CARTESIAN_POINT ( 'NONE',  ( 5.489040303513849750, 0.1347565666095333348, 1.856089258439092893 ) ) ;
#210591 = CARTESIAN_POINT ( 'NONE',  ( 8.938903350111612411, 9.323142084752035430, -0.7998128361456221525 ) ) ;
#210592 = CARTESIAN_POINT ( 'NONE',  ( 0.4254946254920577431, 3.044090126848993716, 0.4192457809173404382 ) ) ;
#210593 = CARTESIAN_POINT ( 'NONE',  ( -2.959422669532919326, 6.674686557755516780, 0.7998128361456352531 ) ) ;
#210594 = CARTESIAN_POINT ( 'NONE',  ( -7.998947442382709383, 12.27592974951444660, 0.7216878364870478180 ) ) ;
#210595 = CARTESIAN_POINT ( 'NONE',  ( -9.915825940873133959, 4.173851563286998356, 6.175246223022227809 ) ) ;
#210596 = DIRECTION ( 'NONE',  ( 0.000000000000000000, -1.000000000000000000, -0.000000000000000000 ) ) ;
#210598 = CARTESIAN_POINT ( 'NONE',  ( 2.154674626568295892, -0.5202524484802829585, -1.891573884155263396 ) ) ;
#210597 = CARTESIAN_POINT ( 'NONE',  ( -5.520141099058386125, 9.591915048876776595, 0.000000000000000000 ) ) ;
#210599 = CARTESIAN_POINT ( 'NONE',  ( 0.7257156204387126275, -2.052300050329861847, 0.6792298617422781737 ) ) ;
#210601 = CARTESIAN_POINT ( 'NONE',  ( -6.116367690567846793, 6.009388118678342217, 0.2715307625813894177 ) ) ;
#210600 = CARTESIAN_POINT ( 'NONE',  ( -5.448397627845328550, 7.449826213943242514, 1.599625672291263179 ) ) ;
#210602 = CARTESIAN_POINT ( 'NONE',  ( -1.402160292154681736E-14, 0.5718750003414239114, 1.575800808251672791 ) ) ;
#210603 = CARTESIAN_POINT ( 'NONE',  ( 2.459901920361181826, 1.337243170739129239, 1.103576756174700746 ) ) ;
#210604 = CARTESIAN_POINT ( 'NONE',  ( 2.044474178175458068, -1.396829902048246197, -1.037857226380611619 ) ) ;
#210605 = CIRCLE ( 'NONE', #41166, 0.07999999999999933553 ) ;
#210606 = CARTESIAN_POINT ( 'NONE',  ( 6.724481002698112775, 8.868313807946373473, -1.443375672974057666 ) ) ;
#210607 = CARTESIAN_POINT ( 'NONE',  ( -12.93484866278744150, 7.732355869717920882, 1.092763313629060873 ) ) ;
#210608 = CARTESIAN_POINT ( 'NONE',  ( 0.8079699768257715409, -1.730602710733687877, 1.034004433739174500 ) ) ;
#210609 = CARTESIAN_POINT ( 'NONE',  ( 6.925078400183590333, 2.958959781645562170, 2.496897724761244497 ) ) ;
#210610 = CARTESIAN_POINT ( 'NONE',  ( -5.496904935697871863, 5.377753611261092637, 0.7998128361456281477 ) ) ;
#210611 = ADVANCED_FACE ( 'NONE', ( #201419 ), #199293, .T. ) ;
#210612 = CARTESIAN_POINT ( 'NONE',  ( 1.235163454902254765, -1.783154728128878652, 0.8411200730164528627 ) ) ;
#210614 = CARTESIAN_POINT ( 'NONE',  ( -5.641601317062247212, 7.675230518029648508, -1.443375672974066548 ) ) ;
#210613 = CARTESIAN_POINT ( 'NONE',  ( 5.730699431777452446, 1.279516236652695316, -1.421498520143074540 ) ) ;
#210615 = CARTESIAN_POINT ( 'NONE',  ( -5.438229012412888252, 9.358701257874761481, -0.7216878364870338292 ) ) ;
#210616 = CARTESIAN_POINT ( 'NONE',  ( 6.062430963966053632, 7.101866208495718702, -1.199719254218452047 ) ) ;
#210617 = CARTESIAN_POINT ( 'NONE',  ( -7.632314129850253259, 7.869064337772231355, 0.7998128361456341429 ) ) ;
#210618 = CARTESIAN_POINT ( 'NONE',  ( 0.8737014391667098367, 0.3917534382160395290, -1.981132022265948756 ) ) ;
#210619 = CARTESIAN_POINT ( 'NONE',  ( 1.347111479061784496E-15, 0.06698729810653621108, -10.99999999999751665 ) ) ;
#210620 = CARTESIAN_POINT ( 'NONE',  ( 4.753107839025799031, -1.856540859070819005, 1.370308287008913606 ) ) ;
#210621 = CARTESIAN_POINT ( 'NONE',  ( 5.986763597034562068, 1.890319730748804439, 0.5246630281777532323 ) ) ;
#210622 = CARTESIAN_POINT ( 'NONE',  ( 3.186327686730246800, 1.093712407854827706, -1.628379936052851917 ) ) ;
#210623 = CARTESIAN_POINT ( 'NONE',  ( 9.911173986789782120, 11.52179005846497972, -1.199719254218440723 ) ) ;
#210624 = CARTESIAN_POINT ( 'NONE',  ( -9.549101787482188186, 15.20623330905540982, 7.267872539799826725 ) ) ;
#210625 = EDGE_LOOP ( 'NONE', ( #168926, #110009, #46679, #149083 ) ) ;
#210626 = CARTESIAN_POINT ( 'NONE',  ( 1.499367237992894841, -0.2534978968403051591, 2.102027841304268119 ) ) ;
#210628 = CARTESIAN_POINT ( 'NONE',  ( -6.561256274009600986, 9.742217188731485678, -1.199719254218440723 ) ) ;
#210627 = CARTESIAN_POINT ( 'NONE',  ( -5.271422797614987665, 5.044414773505913274, -0.7998128361456221525 ) ) ;
#210629 = CARTESIAN_POINT ( 'NONE',  ( 1.042614295247261680, -1.450156864641814369, -1.134287774663629733 ) ) ;
#210630 = ORIENTED_EDGE ( 'NONE', *, *, #208819, .T. ) ;
#210631 = CARTESIAN_POINT ( 'NONE',  ( 11.01852871259909961, 9.193369260742729310, 4.626256781840949017 ) ) ;
#210632 = CARTESIAN_POINT ( 'NONE',  ( 2.935903058640790597, -2.042584291827519660, 0.5695675404085094318 ) ) ;
#210633 = CARTESIAN_POINT ( 'NONE',  ( 0.7499999999999920064, 4.514583334016150751, 1.299038105676669330 ) ) ;
#210634 = CARTESIAN_POINT ( 'NONE',  ( 8.860417081730671995, 10.29590700256267155, 1.199719254218453823 ) ) ;
#210635 = FACE_OUTER_BOUND ( 'NONE', #35298, .T. ) ;
#210636 = CARTESIAN_POINT ( 'NONE',  ( 3.409498948718358680, -0.4055148060846422431, 2.020306737620365389 ) ) ;
#210638 = CARTESIAN_POINT ( 'NONE',  ( -0.006632162239710717895, -1.840811702136424088, -0.04651623371411393176 ) ) ;
#210637 = CARTESIAN_POINT ( 'NONE',  ( -6.665805079413154921, 10.92852302595736447, 0.7998128361456481317 ) ) ;
#210639 = CARTESIAN_POINT ( 'NONE',  ( -1.201851678989727383E-14, 3.571875000341422357, 1.575800808251672791 ) ) ;
#210640 = DIRECTION ( 'NONE',  ( -1.276756478318932585E-15, 1.000000000000000000, -1.665334536937738262E-16 ) ) ;
#210641 = CARTESIAN_POINT ( 'NONE',  ( 1.364708430267706829, 3.684592235245700564, 0.6235921627254619182 ) ) ;
#210642 = PRESENTATION_LAYER_ASSIGNMENT (  '', '', ( #20298 ) ) ;
#210643 = CARTESIAN_POINT ( 'NONE',  ( -0.004863692847738298151, -0.4900785244342681368, -2.159743284330918112 ) ) ;
#210644 = CARTESIAN_POINT ( 'NONE',  ( 3.093345431676647994, 1.942085262481594965, -1.160266548027958367 ) ) ;
#210645 = CARTESIAN_POINT ( 'NONE',  ( -9.381879110976678149, 11.00824238663667565, 1.082531754730558626 ) ) ;
#210646 = CARTESIAN_POINT ( 'NONE',  ( 2.935611553675514518, -1.744650271585326484, 0.4875094811955403284 ) ) ;
#210647 = CARTESIAN_POINT ( 'NONE',  ( 3.344859342474030939, -1.692025585574646662, -0.8982749641134063490 ) ) ;
#210648 = CARTESIAN_POINT ( 'NONE',  ( 4.562978833902987752, 1.602482145440896399, -1.310924660355553106 ) ) ;
#210649 = CARTESIAN_POINT ( 'NONE',  ( -1.201851678989727383E-14, 2.384375000341416584, 1.575800808251672791 ) ) ;
#210650 = CARTESIAN_POINT ( 'NONE',  ( 1.955877382181537838, 1.966306777096353153, -0.1432868284926436253 ) ) ;
#210651 = CARTESIAN_POINT ( 'NONE',  ( 0.3055242992691169501, -0.5169788762636564616, 1.855657374570508278 ) ) ;
#210652 = CARTESIAN_POINT ( 'NONE',  ( 2.623731232481395725, -1.075365945362505293, -1.530472918023266571 ) ) ;
#210654 = CARTESIAN_POINT ( 'NONE',  ( 4.807910157829258679, 8.239027388120819140, -0.8806314816870459694 ) ) ;
#210653 = CARTESIAN_POINT ( 'NONE',  ( 1.542099375240197245, -1.674077152000338797, -1.588604925253054745 ) ) ;
#210655 = CARTESIAN_POINT ( 'NONE',  ( 2.594024687173156263, 0.8801344893799438740, -1.639794913454610148 ) ) ;
#210656 = CARTESIAN_POINT ( 'NONE',  ( 0.6823417656249917140, 3.592708333674754506, 1.181850606188765695 ) ) ;
#210657 = CARTESIAN_POINT ( 'NONE',  ( 6.549293068304288923, 1.796493013226226232, -1.013385894242497809 ) ) ;
#210658 = AXIS2_PLACEMENT_3D ( 'NONE', #75162, #125064, #189967 ) ;
#210659 = CARTESIAN_POINT ( 'NONE',  ( -6.437424008390261854, 6.404749519410410485, 0.7998128361456341429 ) ) ;
#210660 = CARTESIAN_POINT ( 'NONE',  ( 6.103141704446003679, 10.27208242182903142, 0.7998128361456462443 ) ) ;
#210661 = CARTESIAN_POINT ( 'NONE',  ( -1.399654745096419406, 3.350671350837230555, 0.07090406488317851919 ) ) ;
#210662 = CARTESIAN_POINT ( 'NONE',  ( 5.913134528375765697, 1.855721070963678443, 0.9956851948400150532 ) ) ;
#210663 = CARTESIAN_POINT ( 'NONE',  ( -0.6823417656250212460, 3.863541667008085767, 1.181850606188767472 ) ) ;
#210664 = CARTESIAN_POINT ( 'NONE',  ( 5.852838158510675015, -1.708014377640250991, 1.324763891615586386 ) ) ;
#210665 = CARTESIAN_POINT ( 'NONE',  ( 6.024083573256426405, -2.004181050114914875, 0.2492093081243785258 ) ) ;
#210666 = CARTESIAN_POINT ( 'NONE',  ( -1.402160292154681736E-14, -0.6781249996585819728, 1.575800808251672791 ) ) ;
#210667 = CARTESIAN_POINT ( 'NONE',  ( -3.795919822146283540, 6.412028311603867436, -1.082531754730549967 ) ) ;
#210670 = CARTESIAN_POINT ( 'NONE',  ( 4.284013352238246419, 6.021101549076499637, -1.443375672974051449 ) ) ;
#210669 = CARTESIAN_POINT ( 'NONE',  ( 6.825078400183593352, 2.989295776279639938, 2.209688085509611710 ) ) ;
#210668 = CARTESIAN_POINT ( 'NONE',  ( 7.537407054554579489, 7.758339416593960536, 0.000000000000000000 ) ) ;
#210671 = CARTESIAN_POINT ( 'NONE',  ( -3.793249116773374396, 7.647484079536056356, 0.7998128361456352531 ) ) ;
#210672 = CARTESIAN_POINT ( 'NONE',  ( 4.206267736153862735, 1.236801365491456028, -1.592660703826812352 ) ) ;
#210673 = CARTESIAN_POINT ( 'NONE',  ( -6.191269702934848240, 10.37489842006599616, 0.000000000000000000 ) ) ;
#210675 = CARTESIAN_POINT ( 'NONE',  ( -7.417719440008134768, 7.826629899530511025, 0.7216878364870317197 ) ) ;
#210674 = CARTESIAN_POINT ( 'NONE',  ( -9.991996023591624976, 10.75967623705280296, 1.040834085586084257E-14 ) ) ;
#210676 = CARTESIAN_POINT ( 'NONE',  ( 0.6823417656249899377, 4.676041667008086655, -1.181850606188754593 ) ) ;
#210678 = CARTESIAN_POINT ( 'NONE',  ( -1.364683531250014514, 8.838541667008069425, -0.7879004041258335089 ) ) ;
#210677 = CARTESIAN_POINT ( 'NONE',  ( 6.315313271410192719, -0.2696487299426887363, 2.144762774094311375 ) ) ;
#210679 = CARTESIAN_POINT ( 'NONE',  ( -11.07621050858439915, 5.829138686674238734, -4.513195650290508176 ) ) ;
#210681 = CARTESIAN_POINT ( 'NONE',  ( -0.1060672704247594272, -0.8202269080865699502, -1.729793120397028927 ) ) ;
#210680 = CARTESIAN_POINT ( 'NONE',  ( -7.348156068482412095, 7.675196289425353591, 1.040834085586084257E-14 ) ) ;
#210682 = CARTESIAN_POINT ( 'NONE',  ( 0.6823417656249864960, -1.011458332991911568, -1.181850606188749264 ) ) ;
#210683 = CARTESIAN_POINT ( 'NONE',  ( 6.539320575229236709, 1.252639605590207150, 2.218328189723097754 ) ) ;
#210684 = CARTESIAN_POINT ( 'NONE',  ( 1.822448697576475540, 1.608646582964175176, 0.6229558172686412432 ) ) ;
#210685 = CARTESIAN_POINT ( 'NONE',  ( 5.969332771766739931, 10.18624834369502885, -0.7998128361456481317 ) ) ;
#210686 = CARTESIAN_POINT ( 'NONE',  ( 6.204791576909545192, 7.267953590263130259, -1.199719254218452047 ) ) ;
#210687 = CIRCLE ( 'NONE', #193531, 11.54340198673881979 ) ;
#210688 = CARTESIAN_POINT ( 'NONE',  ( -11.33363864608102567, 7.663751225690653257, -3.950522364644465156 ) ) ;
#210689 = CARTESIAN_POINT ( 'NONE',  ( 6.661405586796748324, 0.3194099797865917467, -1.842918054787325843 ) ) ;
#210690 = CARTESIAN_POINT ( 'NONE',  ( 0.6803381722274345345, 0.9942335676262317179, 1.750384451323853785 ) ) ;
#210691 = CARTESIAN_POINT ( 'NONE',  ( 3.628125149645112568, -1.312672481567092708, -1.773765351669121415 ) ) ;
#210692 = CARTESIAN_POINT ( 'NONE',  ( 5.700102493039955753, 0.8868678402436469543, -1.981866098488117789 ) ) ;
#210693 = VERTEX_POINT ( 'NONE', #200358 ) ;
#210694 = CARTESIAN_POINT ( 'NONE',  ( 3.464990776744291345, 6.200183785247111778, 1.199719254218452047 ) ) ;
#210695 = CARTESIAN_POINT ( 'NONE',  ( 9.124274191872634887, 11.66807252865000244, -1.443375672974058777 ) ) ;
#210697 = CARTESIAN_POINT ( 'NONE',  ( 3.392203995056555232, -0.8197896108859267228, -1.842441248588816860 ) ) ;
#210696 = CARTESIAN_POINT ( 'NONE',  ( 3.686284471605893120, 1.179319764668992576, 1.762089746328721507 ) ) ;
#210699 = VERTEX_POINT ( 'NONE', #52007 ) ;
#210698 = CARTESIAN_POINT ( 'NONE',  ( 2.988311359655666077, -1.075548189349010864, 1.457604102852279926 ) ) ;
#210700 = CARTESIAN_POINT ( 'NONE',  ( 6.200875153403774043, 8.327716660428123419, -1.599625672291283607 ) ) ;
#210701 = ORIENTED_EDGE ( 'NONE', *, *, #62042, .F. ) ;
#210702 = ADVANCED_FACE ( 'NONE', ( #18419 ), #67151, .T. ) ;
#210703 = CARTESIAN_POINT ( 'NONE',  ( 0.07479286986305370977, 0.004866263145587856019, -1.855573292446038414 ) ) ;
#210704 = CIRCLE ( 'NONE', #214065, 11.92000000000000171 ) ;
#210705 = CARTESIAN_POINT ( 'NONE',  ( 5.717788096661236885, 7.693838750903348789, 1.599625672291267398 ) ) ;
#210707 = CARTESIAN_POINT ( 'NONE',  ( 1.411203511878999173, -1.802517209299081102, 0.6490724346438890846 ) ) ;
#210706 = CARTESIAN_POINT ( 'NONE',  ( -4.711622075948912247, 5.455646162483875017, -1.199719254218446718 ) ) ;
#210708 = CARTESIAN_POINT ( 'NONE',  ( -2.679728069698085857, 0.4610709815545790957, -0.1059060488087512769 ) ) ;
#210709 = CARTESIAN_POINT ( 'NONE',  ( -4.873231614920269017, 4.964772094600380825, -0.6757755802003853063 ) ) ;
#210710 = CARTESIAN_POINT ( 'NONE',  ( 0.6823417656249882723, 1.488541667008083547, -1.181850606188749264 ) ) ;
#210711 = DIRECTION ( 'NONE',  ( -1.000000000000000000, 8.673617379884035472E-16, 0.000000000000000000 ) ) ;
#210712 = CARTESIAN_POINT ( 'NONE',  ( -9.001723924469462901, 12.58942944760136484, -1.199719254218446718 ) ) ;
#210713 = CARTESIAN_POINT ( 'NONE',  ( 4.944278945467968533, 2.155654431248493985, 0.1625706239713892443 ) ) ;
#210714 = CARTESIAN_POINT ( 'NONE',  ( -5.316205630334268406, 6.335233002545657577, -1.082531754730549967 ) ) ;
#210715 = CARTESIAN_POINT ( 'NONE',  ( -6.291865805193673111, 9.498204651771386509, -1.199719254218452047 ) ) ;
#210716 = CARTESIAN_POINT ( 'NONE',  ( 3.375340920106313813, -1.871962376360849278, -0.9962781187466958066 ) ) ;
#210718 = CARTESIAN_POINT ( 'NONE',  ( -12.00288634729131232, 5.507422065878898820, 4.496070577805427959 ) ) ;
#210717 = CARTESIAN_POINT ( 'NONE',  ( -0.1296875068448125334, 2.048176110289974261, -2.243787855586779401 ) ) ;
#210719 =( BOUNDED_CURVE ( )  B_SPLINE_CURVE ( 2, ( #46641, #15170, #1036, #96476, #213365, #150535, #195007, #163588, #17293 ),
 .UNSPECIFIED., .F., .T. ) 
 B_SPLINE_CURVE_WITH_KNOTS ( ( 3, 2, 2, 2, 3 ),
 ( 0.8482142857142856984, 0.8511904761904761640, 0.8571428571428570953, 0.8630952380952381375, 0.8660714285714286031 ),
 .UNSPECIFIED. ) 
 CURVE ( )  GEOMETRIC_REPRESENTATION_ITEM ( )  RATIONAL_B_SPLINE_CURVE ( ( 0.9330127018922194093, 0.9330127018922194093, 1.000000000000000000, 0.8660254037844387076, 1.000000000000000000, 0.8660254037844387076, 1.000000000000000000, 0.9330127018922194093, 0.9330127018922194093 ) ) 
 REPRESENTATION_ITEM ( '' )  );
#210720 = CARTESIAN_POINT ( 'NONE',  ( 4.007068486172041588, 1.689080509644375505, 1.016306131198143836 ) ) ;
#210721 = CARTESIAN_POINT ( 'NONE',  ( 6.240485052285455581, 1.095381943021833449, -1.567431287326017664 ) ) ;
#210722 = EDGE_LOOP ( 'NONE', ( #50964, #108849 ) ) ;
#210723 =( NAMED_UNIT ( * ) SI_UNIT ( $, .STERADIAN. ) SOLID_ANGLE_UNIT ( ) );
#210724 = CARTESIAN_POINT ( 'NONE',  ( 6.654754201047359707, -0.5240520113350942699, -1.898494369619908140 ) ) ;
#210725 = CARTESIAN_POINT ( 'NONE',  ( 3.099484260031000193, -1.939694849350329431, 0.09605879933238459234 ) ) ;
#210726 = VERTEX_POINT ( 'NONE', #119192 ) ;
#210727 = CARTESIAN_POINT ( 'NONE',  ( -2.959422669532919326, 6.674686557755516780, 0.7998128361456352531 ) ) ;
#210728 = CARTESIAN_POINT ( 'NONE',  ( 4.877901405866606588, 8.912911750144889567, 0.7998128361456341429 ) ) ;
#210730 = CARTESIAN_POINT ( 'NONE',  ( 6.277588818327314080, 7.282607361925381717, 1.199719254218462483 ) ) ;
#210729 = CARTESIAN_POINT ( 'NONE',  ( 2.062552408159121775, -1.911915923569502684, -0.8461947581326088041 ) ) ;
#210731 = CARTESIAN_POINT ( 'NONE',  ( 3.214691819771663628, 6.764574533126651801, -0.7216878364870338292 ) ) ;
#210733 = VERTEX_POINT ( 'NONE', #85557 ) ;
#210732 = CARTESIAN_POINT ( 'NONE',  ( 0.02954414540562703972, -1.776926038569931254, 0.3510683431443075153 ) ) ;
#210734 = CARTESIAN_POINT ( 'NONE',  ( 4.547634279845023109, -1.704780727694398479, -1.401453192282381188 ) ) ;
#210735 = AXIS2_PLACEMENT_3D ( 'NONE', #125993, #79296, #43617 ) ;
#210736 = CARTESIAN_POINT ( 'NONE',  ( 3.610573252990852744, -0.8922430012947217826, -2.018528625508857921 ) ) ;
#210737 = CARTESIAN_POINT ( 'NONE',  ( 7.639129486296027061, 10.99973593639901814, 1.199719254218460707 ) ) ;
#210738 = CARTESIAN_POINT ( 'NONE',  ( 1.499999999999990674, 8.627523663848661428, 2.579999999999999627 ) ) ;
#210739 = CARTESIAN_POINT ( 'NONE',  ( 1.207504981961624813, 1.448612403150219885, 1.248453992567559512 ) ) ;
#210740 = CARTESIAN_POINT ( 'NONE',  ( 9.642873567817520808, 12.27310513391906532, 1.599625672291279388 ) ) ;
#210741 = CARTESIAN_POINT ( 'NONE',  ( 4.598136200040512378, 0.8882050449813773119, -1.870312673664726644 ) ) ;
#210743 = CARTESIAN_POINT ( 'NONE',  ( 3.379894511112140787, 1.369989894601089775, 1.672159933133889442 ) ) ;
#210742 = DIRECTION ( 'NONE',  ( -5.551115123125766062E-17, 0.000000000000000000, 1.000000000000000000 ) ) ;
#210744 = CARTESIAN_POINT ( 'NONE',  ( 4.898067072109578035, -0.7382639882421681010, -2.063579870930781546 ) ) ;
#210745 = PRESENTATION_LAYER_ASSIGNMENT (  '', '', ( #162368 ) ) ;
#210746 = CARTESIAN_POINT ( 'NONE',  ( 8.401248741962376698, 12.95320729893149370, 0.7998128361456462443 ) ) ;
#210747 = CARTESIAN_POINT ( 'NONE',  ( 4.044555541517573793, 7.746237447724527492, 0.4662041258270445132 ) ) ;
#210748 = CARTESIAN_POINT ( 'NONE',  ( -0.4583599637079636691, 7.954360040267954624, 1.947354497276237550 ) ) ;
#210749 = CARTESIAN_POINT ( 'NONE',  ( 4.050854035433010480, 7.948023151305657841, 0.000000000000000000 ) ) ;
#210750 = CARTESIAN_POINT ( 'NONE',  ( 1.642778471875000035, -2.413541666188709911, -2.845375778867859751 ) ) ;
#210751 = CARTESIAN_POINT ( 'NONE',  ( -5.167592825464113915, 6.057888380243431570, 1.199719254218452935 ) ) ;
#210752 = CARTESIAN_POINT ( 'NONE',  ( 0.5807041986926939625, -0.7231374404764076003, 1.882475062126743204 ) ) ;
#210753 = B_SPLINE_CURVE_WITH_KNOTS ( 'NONE', 3,
 ( #116768, #12791, #196890, #195833, #31210, #146042 ),
 .UNSPECIFIED., .F., .F.,
 ( 4, 2, 4 ),
 ( 0.000000000000000000, 0.0003779448103413553901, 0.0007558896206827107802 ),
 .UNSPECIFIED. ) ;
#210754 = CARTESIAN_POINT ( 'NONE',  ( -7.199016379176422120, 11.34267684244042584, 0.000000000000000000 ) ) ;
#210755 = CARTESIAN_POINT ( 'NONE',  ( 6.235824307642648279, 6.239826211863360506, 0.000000000000000000 ) ) ;
#210756 = CARTESIAN_POINT ( 'NONE',  ( 4.891501605334720004, -1.894957309059261297, 0.8341102180390786991 ) ) ;
#210757 = CARTESIAN_POINT ( 'NONE',  ( 3.369672229528171581, 1.879407295867494554, -0.4226879870903621494 ) ) ;
#210759 = CARTESIAN_POINT ( 'NONE',  ( -0.01795374796791787686, -2.016030408028956167, -0.04665595434990427171 ) ) ;
#210758 = B_SPLINE_CURVE_WITH_KNOTS ( 'NONE', 3,
 ( #123478, #67402, #41083, #139657, #51192, #38930, #56250, #17589, #72475, #204598, #33862, #74630, #99941, #55183, #22650, #166005 ),
 .UNSPECIFIED., .F., .F.,
 ( 4, 2, 2, 2, 2, 2, 2, 4 ),
 ( 8.045963024324400998E-05, 0.002777617397444224687, 0.004126196281044714788, 0.005474775164645207491, 0.006823354048245700194, 0.008171932931846193765, 0.009520511815446686468, 0.01086909069904717917 ),
 .UNSPECIFIED. ) ;
#210760 = CARTESIAN_POINT ( 'NONE',  ( 4.690231075323689325, 7.559354456931247412, 1.199719254218462483 ) ) ;
#210761 = CARTESIAN_POINT ( 'NONE',  ( 9.649767104172532584, 4.268299563709526012, 7.133807922836909121 ) ) ;
#210762 = CARTESIAN_POINT ( 'NONE',  ( 4.364079147461279895, -1.964463519307905193, 0.1404744649011815116 ) ) ;
#210763 = CARTESIAN_POINT ( 'NONE',  ( 0.04132284026489921325, -1.696808583893465894, -1.386471574116483696 ) ) ;
#210764 = CARTESIAN_POINT ( 'NONE',  ( 4.318856058802469811, 1.670182456744148336, 0.7377305746401883191 ) ) ;
#210765 = CARTESIAN_POINT ( 'NONE',  ( 6.373741612200160667, 9.489763409991955001, 1.082531754730549078 ) ) ;
#210766 = CARTESIAN_POINT ( 'NONE',  ( 2.684151225381301575, 6.075334163012737321, 0.000000000000000000 ) ) ;
#210767 = CARTESIAN_POINT ( 'NONE',  ( -7.282664789195997912, 8.525472337930658284, 1.199719254218452047 ) ) ;
#210768 = CARTESIAN_POINT ( 'NONE',  ( 5.611095471209277541, 7.639640364534566075, 1.599625672291268286 ) ) ;
#210769 = ORIENTED_EDGE ( 'NONE', *, *, #55423, .T. ) ;
#210771 = CARTESIAN_POINT ( 'NONE',  ( 5.572526294291941795, 0.8198877612898677336, 1.838878804361820274 ) ) ;
#210770 = CARTESIAN_POINT ( 'NONE',  ( 1.680954830071922812, 1.270413995023990106, 1.332975479855981416 ) ) ;
#210772 = CARTESIAN_POINT ( 'NONE',  ( 0.9138903340461038693, 0.6688396875448484602, 2.198942881657910853 ) ) ;
#210773 = CARTESIAN_POINT ( 'NONE',  ( 5.155110299917927463, 1.633153276354940342, -1.086568599608192409 ) ) ;
#210774 = CARTESIAN_POINT ( 'NONE',  ( -7.718669524881690336, 7.899535955317097624, 0.7998128361456462443 ) ) ;
#210775 = DIRECTION ( 'NONE',  ( 0.000000000000000000, -0.7999999999999999334, -0.5999999999999999778 ) ) ;
#210776 = CARTESIAN_POINT ( 'NONE',  ( -5.434120640978981065, 5.234228924097238611, -0.7998128361456221525 ) ) ;
#210777 = CARTESIAN_POINT ( 'NONE',  ( -3.935609729716867289, 7.813571461303467913, 0.7998128361456352531 ) ) ;
#210779 = CARTESIAN_POINT ( 'NONE',  ( 6.825078400183545391, 0.005516643811322509937, 1.755566376062764222 ) ) ;
#210778 = CARTESIAN_POINT ( 'NONE',  ( 1.241864343681793548, 2.088520813897582151, 0.09894013698169208670 ) ) ;
#210780 = CARTESIAN_POINT ( 'NONE',  ( -7.720982897393583677, -5.823938088759706311, 7.834948825496934610 ) ) ;
#210781 = CARTESIAN_POINT ( 'NONE',  ( 0.6823417656249899377, 3.488541667008085323, -1.181850606188754593 ) ) ;
#210782 = CARTESIAN_POINT ( 'NONE',  ( 0.7666889417085223091, 1.677783727127066804, -0.4624100818488885434 ) ) ;
#210783 = CARTESIAN_POINT ( 'NONE',  ( 7.623762449586013901, 7.788811034138823253, 1.040834085586084257E-14 ) ) ;
#210785 = CARTESIAN_POINT ( 'NONE',  ( 0.3423093779009716564, 3.099999999999991651, 0.3999999999999646061 ) ) ;
#210784 = CARTESIAN_POINT ( 'NONE',  ( 1.821370322827225330, -3.246393418362380038E-15, -0.2913868168252300994 ) ) ;
#210786 = CARTESIAN_POINT ( 'NONE',  ( 1.646655695949898135, -1.458533453692168358, 0.9204839396419748354 ) ) ;
#210787 = CARTESIAN_POINT ( 'NONE',  ( 1.347511689332027807, 0.6317163119916607839, -2.098556723903362009 ) ) ;
#210788 = CARTESIAN_POINT ( 'NONE',  ( 4.231241840954825584, 0.1069408422738199749, 2.204416794138922331 ) ) ;
#210789 = CARTESIAN_POINT ( 'NONE',  ( -11.48243876534946217, 12.29999999999998295, 3.199999999999997957 ) ) ;
#210790 = CARTESIAN_POINT ( 'NONE',  ( 1.780376006863694904, -1.203675225865230569, -1.806662255390781180 ) ) ;
#210791 = CARTESIAN_POINT ( 'NONE',  ( 0.2580658466875830337, 0.6954254843183353962, 1.688255465954719536 ) ) ;
#210792 = CARTESIAN_POINT ( 'NONE',  ( 3.327469932021313692, -1.606305723110455608, -1.379610029357878798 ) ) ;
#210793 = CARTESIAN_POINT ( 'NONE',  ( 6.639320575229291421, 7.053415594291638335, 2.394893074302415936 ) ) ;
#210794 = ORIENTED_EDGE ( 'NONE', *, *, #139645, .F. ) ;
#210796 = CARTESIAN_POINT ( 'NONE',  ( -1.402160292154681736E-14, -0.3656249996585805295, 1.575800808251672791 ) ) ;
#210795 = CARTESIAN_POINT ( 'NONE',  ( 3.931398753607476593, -1.581038262191627686, -1.660111252351449185 ) ) ;
#210797 = CARTESIAN_POINT ( 'NONE',  ( 2.184835310096557404, 5.700724961754617404, 1.040834085586084257E-14 ) ) ;
#210798 = CARTESIAN_POINT ( 'NONE',  ( 2.517010073631369860, 6.088262185878572375, -0.7998128361456281477 ) ) ;
#210799 = CARTESIAN_POINT ( 'NONE',  ( 5.883471028171038952, 0.1659795297097066691, -2.215133764073994982 ) ) ;
#210800 = CARTESIAN_POINT ( 'NONE',  ( -6.399085315970142851, 8.488685506763726352, -1.443375672974059665 ) ) ;
#210801 = CARTESIAN_POINT ( 'NONE',  ( 3.877268743828266029, 6.506935386899531437, 1.082531754730558626 ) ) ;
#210802 = CARTESIAN_POINT ( 'NONE',  ( -7.009202228140744673, 10.16085778526412042, -1.082531754730537088 ) ) ;
#210803 = CARTESIAN_POINT ( 'NONE',  ( 5.899206235721897507, 6.055031161196562373, 0.000000000000000000 ) ) ;
#210804 = ORIENTED_EDGE ( 'NONE', *, *, #203693, .F. ) ;
#210805 = CARTESIAN_POINT ( 'NONE',  ( 4.483046177357690176, -2.016033783801042034, -0.04667830911464498911 ) ) ;
#210807 = CARTESIAN_POINT ( 'NONE',  ( 2.465751394709358113, -0.4561089685623443968, 2.011347002571160836 ) ) ;
#210806 = CARTESIAN_POINT ( 'NONE',  ( 5.799137018343234473, 7.788745826199009237, -1.599625672291262513 ) ) ;
#210808 = CARTESIAN_POINT ( 'NONE',  ( 1.528150327639969719, -3.232243495192087757, 2.908546201585544999 ) ) ;
#210809 = CARTESIAN_POINT ( 'NONE',  ( 5.872089928050205465, 6.023395468912922546, -0.7216878364870458196 ) ) ;
#210810 = CARTESIAN_POINT ( 'NONE',  ( 0.000000000000000000, -9.999999999999994671, 0.000000000000000000 ) ) ;
#210811 = CARTESIAN_POINT ( 'NONE',  ( -1.364683531250010295, 5.488541667008087543, -0.7879004041258300672 ) ) ;
#210812 = CARTESIAN_POINT ( 'NONE',  ( 5.085950966588184130, -2.174626929279792176, -0.2704268894557353975 ) ) ;
#210813 = CARTESIAN_POINT ( 'NONE',  ( 2.092422861153935276, -0.4390285686692517175, 1.967888031366466395 ) ) ;
#210814 = CARTESIAN_POINT ( 'NONE',  ( 2.155570461979210428, 0.7887370375637430264, 1.663910549085621415 ) ) ;
#210815 = CARTESIAN_POINT ( 'NONE',  ( 5.770966940911189447, 9.884545197705074671, -0.7998128361456291469 ) ) ;
#210816 =( NAMED_UNIT ( * ) PLANE_ANGLE_UNIT ( ) SI_UNIT ( $, .RADIAN. ) );
#210817 = CARTESIAN_POINT ( 'NONE',  ( 4.805575371506604299, -0.4859443722219913830, 1.759630929660048526 ) ) ;
#210818 = CARTESIAN_POINT ( 'NONE',  ( 6.486953984781112403, -2.015912550161761629, 0.05229459904129707404 ) ) ;
#210819 = CARTESIAN_POINT ( 'NONE',  ( -7.069687034522070590, 10.33538640932937724, -1.199719254218440723 ) ) ;
#210821 = CARTESIAN_POINT ( 'NONE',  ( -6.818824913030298696, 6.919993584815607335, 0.7998128361456341429 ) ) ;
#210820 = CARTESIAN_POINT ( 'NONE',  ( 5.541944591929171438, 0.9225863094920858654, -2.066052574227566385 ) ) ;
#210822 = CARTESIAN_POINT ( 'NONE',  ( 0.2586047683651994666, 0.8082109201883975746, 1.945024607815620366 ) ) ;
#210823 = CARTESIAN_POINT ( 'NONE',  ( -6.774234028683526532, 7.932303117332766718, 1.199719254218452047 ) ) ;
#210824 = CARTESIAN_POINT ( 'NONE',  ( 6.753933077901968396, 11.03133902419432566, 0.7998128361456462443 ) ) ;
#210825 = CARTESIAN_POINT ( 'NONE',  ( 1.360316468749975582, 2.776041667008103175, 0.7853790794158820310 ) ) ;
#210826 = DIRECTION ( 'NONE',  ( 0.6517139959213666955, 0.4936023552085019861, 0.5758694144099204548 ) ) ;
#210828 = EDGE_CURVE ( 'NONE', #6177, #172406, #34074, .T. ) ;
#210827 = CARTESIAN_POINT ( 'NONE',  ( -8.064402442030170093, 8.302891025323665630, 0.7998128361456602331 ) ) ;
#210829 = CARTESIAN_POINT ( 'NONE',  ( -1.734723475976807094E-15, 2.999999999999988898, -6.938893903907228378E-15 ) ) ;
#210830 = CARTESIAN_POINT ( 'NONE',  ( 6.393551957296131683, 9.616838495890963401, 1.199719254218452047 ) ) ;
#210831 = CARTESIAN_POINT ( 'NONE',  ( 4.626207451132414938, 6.895778996938287442, -1.211788453915439989 ) ) ;
#210832 = CARTESIAN_POINT ( 'NONE',  ( -10.16825202056928390, 10.96530823352674133, 0.7216878364870438212 ) ) ;
#210833 = CARTESIAN_POINT ( 'NONE',  ( 3.357896860617498369, -1.684415915708385114, -1.448384614443619434 ) ) ;
#210834 = CARTESIAN_POINT ( 'NONE',  ( -1.451998047843676476, 7.315968950353781253, 4.301760722578348073 ) ) ;
#210836 = CIRCLE ( 'NONE', #128067, 0.07999999999999959921 ) ;
#210835 = CARTESIAN_POINT ( 'NONE',  ( -5.448397627845328550, 7.449826213943242514, 1.599625672291263179 ) ) ;
#210837 = CARTESIAN_POINT ( 'NONE',  ( 5.937581207780954884, 9.014596278131406848, -1.199719254218440723 ) ) ;
#210838 = CARTESIAN_POINT ( 'NONE',  ( 3.473055881322492322, 1.772541284497713976, 0.8411618914155660764 ) ) ;
#210839 = CARTESIAN_POINT ( 'NONE',  ( 6.419949431270806528, 7.448694743692793274, 1.199719254218462483 ) ) ;
#210840 = CARTESIAN_POINT ( 'NONE',  ( -4.047283575590383542, 7.579128156381162107, 0.3715214982176785474 ) ) ;
#210841 = CARTESIAN_POINT ( 'NONE',  ( 5.183294799126148433, 4.941598775268944976, 1.040834085586084257E-14 ) ) ;
#210842 = CARTESIAN_POINT ( 'NONE',  ( -3.960390268967665328, 6.674186842887300131, 1.082531754730549967 ) ) ;
#210844 = ORIENTED_EDGE ( 'NONE', *, *, #72882, .F. ) ;
#210843 = CARTESIAN_POINT ( 'NONE',  ( -5.883875478650828050, 9.808345791827219884, 0.7216878364870458196 ) ) ;
#210845 = CARTESIAN_POINT ( 'NONE',  ( 2.883181758455736432, -1.960942133159260692, -0.8077274430827171559 ) ) ;
#210846 = CARTESIAN_POINT ( 'NONE',  ( -5.743814354044916470, 6.730146830254374990, -1.199719254218453823 ) ) ;
#210847 = CARTESIAN_POINT ( 'NONE',  ( 4.750933126423753095, -1.738186171353903742, 1.284983810367075208 ) ) ;
#210848 = CARTESIAN_POINT ( 'NONE',  ( 2.682954136603598272, 1.303717545168959990, 1.300458928786947688 ) ) ;
#210849 = CARTESIAN_POINT ( 'NONE',  ( -5.219248474292968787, 6.450796296714536915, 1.173595342525960206 ) ) ;
#210850 = CARTESIAN_POINT ( 'NONE',  ( 0.6823417656249882723, 0.2385416670080825474, -1.181850606188749264 ) ) ;
#210851 = CARTESIAN_POINT ( 'NONE',  ( 6.070193552946823168, -1.654735283430305515, -0.5392940629580407208 ) ) ;
#210852 = CARTESIAN_POINT ( 'NONE',  ( 1.499999999999990896, 3.306250000682818602, 1.214306433183764966E-14 ) ) ;
#210853 = CARTESIAN_POINT ( 'NONE',  ( 4.853455804012216213, 6.685451076146141425, 1.443375672974062551 ) ) ;
#210854 = CARTESIAN_POINT ( 'NONE',  ( -0.4366903032815979135, -8.287795860939835890, 10.40306649911375736 ) ) ;
#210855 = CARTESIAN_POINT ( 'NONE',  ( 3.063507763784904192, 0.3185916186679502715, -2.137983152197140413 ) ) ;
#210856 = CARTESIAN_POINT ( 'NONE',  ( 4.622422610786712127, 0.4444332032229811325, -1.966343831704894907 ) ) ;
#210857 = CARTESIAN_POINT ( 'NONE',  ( -8.310784975052671442, 11.67937098999472667, -1.082531754730543083 ) ) ;
#210858 = CARTESIAN_POINT ( 'NONE',  ( 2.729541802387557059, -2.017400560480298033, 0.7770373237434913261 ) ) ;
#210859 = EDGE_CURVE ( 'NONE', #25627, #195274, #182801, .T. ) ;
#210860 = CARTESIAN_POINT ( 'NONE',  ( 4.077382496314372773, 1.857369029195341525, -0.6610406152272005897 ) ) ;
#210861 = CARTESIAN_POINT ( 'NONE',  ( 4.599131018191075171, -0.5143685224620330176, 1.872658368587260647 ) ) ;
#210864 = ORIENTED_EDGE ( 'NONE', *, *, #131239, .F. ) ;
#210863 = DIRECTION ( 'NONE',  ( -3.491481338843133355E-15, 0.000000000000000000, -1.000000000000000000 ) ) ;
#210862 = CARTESIAN_POINT ( 'NONE',  ( -8.473482818416664841, 11.86918514058604757, -1.082531754730543083 ) ) ;
#210865 = CARTESIAN_POINT ( 'NONE',  ( -6.444921918449773024, 8.612437886315108315, 1.599625672291269396 ) ) ;
#210866 = CARTESIAN_POINT ( 'NONE',  ( -1.040834085586084257E-14, 0.000000000000000000, -9.579665964948867796 ) ) ;
#210868 = VERTEX_POINT ( 'NONE', #1088 ) ;
#210867 = CARTESIAN_POINT ( 'NONE',  ( -5.503684012504701961, 5.385662534202396934, 0.000000000000000000 ) ) ;
#210869 = CARTESIAN_POINT ( 'NONE',  ( -7.470179451005382276, 11.65903375957422128, 0.7216878364870458196 ) ) ;
#210870 = CARTESIAN_POINT ( 'NONE',  ( 0.8860939741733677710, 1.483344945610004295, 1.634051305214024641 ) ) ;
#210871 = CARTESIAN_POINT ( 'NONE',  ( -1.642778471875000035, -0.8677083328553769626, -2.845375778867859751 ) ) ;
#210872 = CARTESIAN_POINT ( 'NONE',  ( 5.928557400228100960, -1.247251702497784942, 1.514172074262534196 ) ) ;
#210873 = CARTESIAN_POINT ( 'NONE',  ( -1.001543065824772872E-14, 5.384375000341415252, 1.575800808251672791 ) ) ;
#210874 = CARTESIAN_POINT ( 'NONE',  ( 1.499999999999990896, 4.056250000682819490, 1.214306433183764966E-14 ) ) ;
#210875 = CARTESIAN_POINT ( 'NONE',  ( 5.555833580239399438, 6.383300830698137140, -1.210397860111110946 ) ) ;
#210876 = CARTESIAN_POINT ( 'NONE',  ( 0.07499057489264347731, 6.948553613792602057, -2.550573651218261517 ) ) ;
#210877 = CARTESIAN_POINT ( 'NONE',  ( 5.525302006934727395, -1.171079710934025186, -1.420692760577553226 ) ) ;
#210878 = ORIENTED_EDGE ( 'NONE', *, *, #123768, .F. ) ;
#210879 = CARTESIAN_POINT ( 'NONE',  ( 0.6801582343749692505, -0.5260416663252707181, 1.178068619123786132 ) ) ;
#210880 = CARTESIAN_POINT ( 'NONE',  ( -7.857113714319432063, 9.125386407249497012, 1.199719254218462483 ) ) ;
#210881 = CARTESIAN_POINT ( 'NONE',  ( -1.007805743535968412, -8.868899487089072003E-15, 0.8044584510992147663 ) ) ;
#210882 = CARTESIAN_POINT ( 'NONE',  ( 5.765915565743810589, 0.6138260544302427402, -2.029845472315944921 ) ) ;
#210883 = FILL_AREA_STYLE_COLOUR ( '', #4497 ) ;
#210884 = CARTESIAN_POINT ( 'NONE',  ( 5.341022448779654930, 8.318611059296550536, 1.199719254218462483 ) ) ;
#210885 = CARTESIAN_POINT ( 'NONE',  ( 6.766874334510889710, -1.882258232876810045, -0.8394616043497000746 ) ) ;
#210888 = CARTESIAN_POINT ( 'NONE',  ( 3.948646536499214932, -1.533023199436277961, -1.019512891124202403 ) ) ;
#210887 = CARTESIAN_POINT ( 'NONE',  ( 2.295144308211858331, -1.664110045376477443, 0.8333370299275147941 ) ) ;
#210886 = CARTESIAN_POINT ( 'NONE',  ( -10.31538147864342925, 4.824606379122443833, 6.138819041055270098 ) ) ;
#210889 = CARTESIAN_POINT ( 'NONE',  ( 8.097244055859613709, 10.46987070330147063, -1.599625672291262513 ) ) ;
#210890 = CARTESIAN_POINT ( 'NONE',  ( 8.832353407160718817, 3.956598013261175772, 7.432338980325266853 ) ) ;
#210891 = CARTESIAN_POINT ( 'NONE',  ( -5.121948170912633991, 9.197632976031879792, -0.7998128361456362523 ) ) ;
#210892 = DIRECTION ( 'NONE',  ( 0.000000000000000000, 1.000000000000000000, 0.000000000000000000 ) ) ;
#210893 = ADVANCED_FACE ( 'NONE', ( #185177 ), #78858, .F. ) ;
#210894 = CARTESIAN_POINT ( 'NONE',  ( 3.721466898765386500, -0.1629207441977159332, 2.200919931280575170 ) ) ;
#210895 = CARTESIAN_POINT ( 'NONE',  ( 5.958357971250668683, 0.9089415708923481718, 2.071969630155451547 ) ) ;
#210896 = CARTESIAN_POINT ( 'NONE',  ( -7.212574532790110737, 7.517017831117667193, -0.7216878364870278340 ) ) ;
#210897 = CARTESIAN_POINT ( 'NONE',  ( 6.363521484574993003, -1.460773276151544176, -1.071267404939825640 ) ) ;
#210898 = CARTESIAN_POINT ( 'NONE',  ( 6.122283701245728516, 1.895932525083013465, 0.2736375990538899572 ) ) ;
#210899 = CARTESIAN_POINT ( 'NONE',  ( 1.359357947053562156E-15, 0.000000000000000000, -11.09999999999999964 ) ) ;
#210900 = VECTOR ( 'NONE', #212843, 1000.000000000000000 ) ;
#210901 = CARTESIAN_POINT ( 'NONE',  ( 6.350466393003619814, 0.5888352225367661230, 1.775644890098279749 ) ) ;
#210902 = DIRECTION ( 'NONE',  ( 0.7592566023653005702, 0.6507913734559639396, 0.000000000000000000 ) ) ;
#210903 = CARTESIAN_POINT ( 'NONE',  ( 6.578955313817166584, -0.09182192948648319752, -1.767577901409943086 ) ) ;
#210904 = CARTESIAN_POINT ( 'NONE',  ( 1.815639016007553730, -1.320828798922760949, -1.523793687088881299 ) ) ;
#210906 = CARTESIAN_POINT ( 'NONE',  ( 3.053452221204506323, -1.721964003836244039, -1.212301904834027333 ) ) ;
#210905 = CARTESIAN_POINT ( 'NONE',  ( -10.16591625214838679, 10.75465713712827487, 1.040834085586084257E-14 ) ) ;
#210907 = CARTESIAN_POINT ( 'NONE',  ( 8.772289083241844310, 10.19309100432570148, -1.199719254218446718 ) ) ;
#210909 = CARTESIAN_POINT ( 'NONE',  ( -9.016335848287868160, 10.47781223021269170, 1.199719254218462483 ) ) ;
#210908 = CARTESIAN_POINT ( 'NONE',  ( -1.500000000000013101, -0.3291666666666463459, 0.8660254037844403729 ) ) ;
#210910 = CARTESIAN_POINT ( 'NONE',  ( -15.75000000000000000, 13.79999999999998295, 3.199999999999997957 ) ) ;
#210911 = CARTESIAN_POINT ( 'NONE',  ( 2.513930914015961804, -0.6297079463782135900, 1.919214091249999088 ) ) ;
#210912 = CARTESIAN_POINT ( 'NONE',  ( -0.6823417656250212460, 4.051041667008085767, 1.181850606188767472 ) ) ;
#210913 = CARTESIAN_POINT ( 'NONE',  ( 10.54788032175191326, 11.40820791823982994, 0.7216878364870317197 ) ) ;
#210914 = CARTESIAN_POINT ( 'NONE',  ( 3.708425082824120533, -0.8722964037291662809, -1.977944213000272455 ) ) ;
#210915 = CARTESIAN_POINT ( 'NONE',  ( 6.770317605177710085, 8.992066187497757213, 1.599625672291268286 ) ) ;
#210917 = DIRECTION ( 'NONE',  ( 0.000000000000000000, 0.000000000000000000, -1.000000000000000000 ) ) ;
#210916 = CARTESIAN_POINT ( 'NONE',  ( 8.018721507839716267, 8.319872945426633137, -0.7998128361456341429 ) ) ;
#210918 = CARTESIAN_POINT ( 'NONE',  ( 10.01911233037457905, 11.75168114260095109, 1.082531754730548412 ) ) ;
#210920 = CARTESIAN_POINT ( 'NONE',  ( 8.996714940757932766, 14.55825685055163987, -7.941925727616619746 ) ) ;
#210919 = CARTESIAN_POINT ( 'NONE',  ( 0.6784789811392475389, -1.161776791282279397, -1.834017514133066129 ) ) ;
#210921 = CARTESIAN_POINT ( 'NONE',  ( -5.070386261830872598, 8.859275038870594088, 0.7216878364870458196 ) ) ;
#210922 = CARTESIAN_POINT ( 'NONE',  ( 1.364683531249988757, 0.6343750003414208027, 0.000000000000000000 ) ) ;
#210923 = CARTESIAN_POINT ( 'NONE',  ( 1.997856853652695497, -2.190977152517746163, 0.05759783203293508680 ) ) ;
#210924 = CARTESIAN_POINT ( 'NONE',  ( 6.883263157960365142, 1.273421409013283823, 2.069651443392322765 ) ) ;
#210925 = CARTESIAN_POINT ( 'NONE',  ( 2.272703622300107362, -1.391801132404853147, 1.783687758696401504 ) ) ;
#210926 = CARTESIAN_POINT ( 'NONE',  ( -8.182509401047415309, 9.505014708432145909, 1.199719254218462483 ) ) ;
#210927 = CARTESIAN_POINT ( 'NONE',  ( -3.267151830768959098, 4.834763107362302748, -1.443375672974058777 ) ) ;
#210928 = CARTESIAN_POINT ( 'NONE',  ( 1.364683531249988535, 3.967708333674751842, -0.7879004041258239610 ) ) ;
#210929 = CARTESIAN_POINT ( 'NONE',  ( 5.685886686578042415, 7.314606927785019863, 1.221034997698521307 ) ) ;
#210930 = CARTESIAN_POINT ( 'NONE',  ( -0.7500000000000179856, 12.04166666666666607, 1.299038105676658228 ) ) ;
#210931 = CARTESIAN_POINT ( 'NONE',  ( 5.966997003790217136, 8.054858819212300958, -1.443375672974078761 ) ) ;
#210932 = CARTESIAN_POINT ( 'NONE',  ( 4.674921082483953327, 0.0007207667814621705445, -1.769921774705035755 ) ) ;
#210933 = STYLED_ITEM ( 'NONE', ( #12611 ), #156107 ) ;
#210934 = CARTESIAN_POINT ( 'NONE',  ( 8.422639742587595180, 10.84949900448412130, -1.599625672291268286 ) ) ;
#210935 = CARTESIAN_POINT ( 'NONE',  ( 0.9738169395155724661, 2.029595412481857153, -0.5617393031529455127 ) ) ;
#210936 = CARTESIAN_POINT ( 'NONE',  ( 0.6823417656249934904, 9.942708333674735499, 1.181850606188764807 ) ) ;
#210937 = CARTESIAN_POINT ( 'NONE',  ( -3.959863383643135393, 6.777535159962392086, 1.199719254218452935 ) ) ;
#210938 = CARTESIAN_POINT ( 'NONE',  ( 5.870720304489429608, -0.2986452421533461465, -1.994069804803912049 ) ) ;
#210939 = ORIENTED_EDGE ( 'NONE', *, *, #68743, .T. ) ;
#210940 = ADVANCED_FACE ( 'NONE', ( #2146 ), #49870, .F. ) ;
#210941 = CARTESIAN_POINT ( 'NONE',  ( 3.959713429720784106, 1.856571849420919795, -0.2284545790810637578 ) ) ;
#210942 = CARTESIAN_POINT ( 'NONE',  ( 3.239188805615275335, -0.1476314317495740769, -2.065021578984991724 ) ) ;
#210943 = CARTESIAN_POINT ( 'NONE',  ( -4.923019175093582334, 8.757623114335565617, 0.7216878364870267237 ) ) ;
#210944 = CARTESIAN_POINT ( 'NONE',  ( -1.419999999999997708, 8.627523663848661428, -2.579999999999990301 ) ) ;
#210945 = FACE_OUTER_BOUND ( 'NONE', #195885, .T. ) ;
#210946 = DIRECTION ( 'NONE',  ( -3.451266460341926649E-31, -5.200010849845536803E-32, 1.000000000000000000 ) ) ;
#210947 = CARTESIAN_POINT ( 'NONE',  ( 6.825078400183575589, -0.005632053428735600553, 2.144262460745151255 ) ) ;
#210948 = CARTESIAN_POINT ( 'NONE',  ( -1.364683531250014514, -0.7614583329919104582, -0.7879004041258359514 ) ) ;
#210949 = CARTESIAN_POINT ( 'NONE',  ( 2.805073129645048624, -1.632656238785214597, 1.087510969322850629 ) ) ;
#210950 = CARTESIAN_POINT ( 'NONE',  ( 0.5794536021234627521, 1.392335491182377316, -1.458330535474762213 ) ) ;
#210951 = CARTESIAN_POINT ( 'NONE',  ( -4.659162064951642535, 5.464719159645540003, 1.199719254218452935 ) ) ;
#210952 = CARTESIAN_POINT ( 'NONE',  ( 7.422199028477372451, 10.74665040227725044, -1.199719254218441611 ) ) ;
#210953 = CARTESIAN_POINT ( 'NONE',  ( 0.6318452133688509109, 0.9670987946563678328, -1.601024004909731513 ) ) ;
#210954 = CARTESIAN_POINT ( 'NONE',  ( -1.364683531250012516, 3.280208333674756727, 0.7879004041258379498 ) ) ;
#210955 = CARTESIAN_POINT ( 'NONE',  ( 2.900642264033539863, -1.984120583840060625, -0.3400495124021261084 ) ) ;
#210957 = CARTESIAN_POINT ( 'NONE',  ( 2.073964263283359699, -0.9022394416563597197, 1.915483482535395909 ) ) ;
#210956 = CARTESIAN_POINT ( 'NONE',  ( -6.900736999675794792, 7.153207375817628666, 1.040834085586084257E-14 ) ) ;
#210958 = CARTESIAN_POINT ( 'NONE',  ( 10.40189579028154832, 9.152068647944213708, -6.036026366622869510 ) ) ;
#210959 = CARTESIAN_POINT ( 'NONE',  ( 3.947765587739564097, 1.497496809916948779, 1.429883829622953462 ) ) ;
#210960 = CARTESIAN_POINT ( 'NONE',  ( 8.167861197590044142, 8.493869250135347215, 0.000000000000000000 ) ) ;
#210962 = CARTESIAN_POINT ( 'NONE',  ( 4.701980345841006326, 4.380065246436280368, 0.7998128361456341429 ) ) ;
#210961 = CARTESIAN_POINT ( 'NONE',  ( 6.351524237630270520, 2.085149843271947301, -0.1523318108044656727 ) ) ;
#210964 = ORIENTED_EDGE ( 'NONE', *, *, #6048, .F. ) ;
#210963 = CARTESIAN_POINT ( 'NONE',  ( 5.860330175037709921, 0.7421476303169188826, 1.668095884353037128 ) ) ;
#210965 = CARTESIAN_POINT ( 'NONE',  ( 8.028399517586572998, 12.51821653715971472, -0.7998128361456352531 ) ) ;
#210966 = CARTESIAN_POINT ( 'NONE',  ( 11.96407947313512743, 8.207545470847758651, -0.7892166907401461096 ) ) ;
#210967 = AXIS2_PLACEMENT_3D ( 'NONE', #177377, #144910, #80933 ) ;
#210968 = CARTESIAN_POINT ( 'NONE',  ( 6.616270032800761314, -1.034323699838369359, -1.949367651511712207 ) ) ;
#210969 = CARTESIAN_POINT ( 'NONE',  ( 1.364683531249997417, 10.54687500034139802, 2.602085213965210642E-15 ) ) ;
#210970 = CARTESIAN_POINT ( 'NONE',  ( 5.514289750425454883, -1.912461473380810961, 0.004301308668797076962 ) ) ;
#210971 = CARTESIAN_POINT ( 'NONE',  ( -9.809487834687324437, 11.40315621434539395, 1.199719254218462483 ) ) ;
#210972 = CARTESIAN_POINT ( 'NONE',  ( 5.282873410819217241, 9.315102745931094219, -0.7998128361456281477 ) ) ;
#210973 = CARTESIAN_POINT ( 'NONE',  ( -1.360316468750048857, 1.942708333674827426, 0.7853790794158581612 ) ) ;
#210974 = EDGE_CURVE ( 'NONE', #6682, #60595, #138489, .T. ) ;
#210975 = CARTESIAN_POINT ( 'NONE',  ( 5.671388329218120639, 5.511041227042920099, 1.040834085586084257E-14 ) ) ;
#210976 = EDGE_LOOP ( 'NONE', ( #80990, #38539, #3, #60465, #113210, #16070 ) ) ;
#210977 = CYLINDRICAL_SURFACE ( 'NONE', #137549, 8.049999999999993605 ) ;
#210978 = CIRCLE ( 'NONE', #6892, 0.08000000000000020983 ) ;
#210979 = CARTESIAN_POINT ( 'NONE',  ( 4.376139848268215893, -1.078761963904120602, 1.527931137620001989 ) ) ;
#210980 = CARTESIAN_POINT ( 'NONE',  ( -11.07790593930098311, 13.79999999999999893, 0.6999999999999992895 ) ) ;
#210981 = CARTESIAN_POINT ( 'NONE',  ( 7.205232291019763480, 7.370802192470005565, -0.7998128361456341429 ) ) ;
#210982 = CARTESIAN_POINT ( 'NONE',  ( -11.04986239659823433, 13.60939231485699352, -1.056426191432995765 ) ) ;
#210983 = CARTESIAN_POINT ( 'NONE',  ( -5.850575378433040541, 7.204527765336914413, 1.160475518089182811 ) ) ;
#210984 = CARTESIAN_POINT ( 'NONE',  ( -4.758548728716557541, 8.495464583570553785, 1.040834085586084257E-14 ) ) ;
#210985 = CARTESIAN_POINT ( 'NONE',  ( 4.033714395265605823, 4.664753868353354704, -1.199719254218446718 ) ) ;
#210986 = CARTESIAN_POINT ( 'NONE',  ( 1.006626315519317139, 0.5665869296403948097, 1.886213005043664515 ) ) ;
#210987 = ADVANCED_FACE ( 'NONE', ( #165757 ), #144838, .F. ) ;
#210988 = CARTESIAN_POINT ( 'NONE',  ( 3.392203995056555232, -0.8197896108859267228, -1.842441248588816860 ) ) ;
#210989 = CARTESIAN_POINT ( 'NONE',  ( -7.531718027591449705, 8.745758106066849891, 1.199719254218462483 ) ) ;
#210990 = CARTESIAN_POINT ( 'NONE',  ( 4.369470645354133431, 8.319742529546998000, 0.7998128361456271485 ) ) ;
#210991 = CARTESIAN_POINT ( 'NONE',  ( -0.4465194593918104249, 3.080450244942127380, 0.4155024747329021939 ) ) ;
#210992 = CARTESIAN_POINT ( 'NONE',  ( 3.257961296797746265, 0.9855263100190698733, 1.957416934251283935 ) ) ;
#210993 = SURFACE_SIDE_STYLE ('',( #178525 ) ) ;
#210994 = CARTESIAN_POINT ( 'NONE',  ( 2.362220099979424059, 0.8219310624981416291, 1.742368475122471727 ) ) ;
#210995 = CARTESIAN_POINT ( 'NONE',  ( -8.676328237741483207, 12.20980114641871062, -1.199719254218446718 ) ) ;
#210996 = ADVANCED_FACE ( 'NONE', ( #156980 ), #203547, .F. ) ;
#210997 = DIRECTION ( 'NONE',  ( -1.276756478318932191E-15, 1.000000000000000000, -3.330669073875483426E-16 ) ) ;
#210998 = FACE_OUTER_BOUND ( 'NONE', #78955, .T. ) ;
#210999 = CARTESIAN_POINT ( 'NONE',  ( -9.645406396194509568, 4.042443384815813445, -6.587269312116742270 ) ) ;
#211000 = CARTESIAN_POINT ( 'NONE',  ( 7.476431642932036326, 10.80992178580769014, 1.199719254218460707 ) ) ;
#211001 = CARTESIAN_POINT ( 'NONE',  ( 4.625302960556422427, 8.547937220624488575, 1.040834085586084257E-14 ) ) ;
#211002 = CARTESIAN_POINT ( 'NONE',  ( 3.297657676621871925, 4.870353260857385180, 1.599625672291267398 ) ) ;
#211003 = CARTESIAN_POINT ( 'NONE',  ( 6.712695452541852070, 7.004101914153185504, 0.000000000000000000 ) ) ;
#211004 = VERTEX_POINT ( 'NONE', #55202 ) ;
#211006 = CARTESIAN_POINT ( 'NONE',  ( 1.471341131262299706, -1.727646810417843959, -1.033094421854539036 ) ) ;
#211005 = CARTESIAN_POINT ( 'NONE',  ( 5.161589042655139181, 0.9124512986629171873, 1.599201395118980740 ) ) ;
#211007 = CARTESIAN_POINT ( 'NONE',  ( 4.481968937923656249, 2.098976780363570604, 0.9367997793626892111 ) ) ;
#211009 = CARTESIAN_POINT ( 'NONE',  ( 2.272090887488043887, -0.8719313595505603365, -1.644003247725301264 ) ) ;
#211008 = CARTESIAN_POINT ( 'NONE',  ( -0.1290005225502432740, 4.081813041011835175, -2.728655865233818201 ) ) ;
#211011 = CARTESIAN_POINT ( 'NONE',  ( 3.285556943750000514, -2.063541666188710266, 1.896917185911906500 ) ) ;
#211010 = APPLICATION_CONTEXT ( 'automotive_design' ) ;
#211012 = CARTESIAN_POINT ( 'NONE',  ( 6.883263157960364254, -0.007059606330772384697, 2.153658854459545857 ) ) ;
#211013 = CARTESIAN_POINT ( 'NONE',  ( 5.379139070037473935, -1.731557697741787916, -0.8120211572784155063 ) ) ;
#211014 = CARTESIAN_POINT ( 'NONE',  ( -7.263417608619167076, 9.497073181520933716, -1.599625672291263179 ) ) ;
#211015 = CARTESIAN_POINT ( 'NONE',  ( -6.021229618244897885, 7.157760988441397743, 1.082531754730548412 ) ) ;
#211017 = CARTESIAN_POINT ( 'NONE',  ( 2.940157781200231746, 1.856316385841882965, 0.2306766016651334850 ) ) ;
#211016 = CARTESIAN_POINT ( 'NONE',  ( 4.353126977966869759, 0.4563941458865827805, -2.040161790709469791 ) ) ;
#211018 = CARTESIAN_POINT ( 'NONE',  ( 5.477130870240836558, 9.333810415348903433, -0.7216878364870267237 ) ) ;
#211019 = CARTESIAN_POINT ( 'NONE',  ( 4.220665892555866883, 3.818531717603609987, -0.7998128361456211532 ) ) ;
#211020 = CARTESIAN_POINT ( 'NONE',  ( 0.1370650511771386582, -7.902328468025380914, -10.96100467917833221 ) ) ;
#211021 = CARTESIAN_POINT ( 'NONE',  ( 5.443894040360703457, 0.6935754108010495633, -1.579493244201269908 ) ) ;
#211022 = CARTESIAN_POINT ( 'NONE',  ( -5.280010757518168063, 8.247430752824802980, -1.199719254218446718 ) ) ;
#211023 = FILL_AREA_STYLE ('',( #64785 ) ) ;
#211024 = CARTESIAN_POINT ( 'NONE',  ( 0.2999999999999686806, 3.975028841772344723, -0.9637995837462834947 ) ) ;
#211025 = CARTESIAN_POINT ( 'NONE',  ( 1.836970198721030181E-16, 13.49999999999999822, 1.500000000000000222 ) ) ;
#211026 = CARTESIAN_POINT ( 'NONE',  ( 5.489208499878581726, 0.1525156608223678933, 2.165750181564994215 ) ) ;
#211027 = CARTESIAN_POINT ( 'NONE',  ( 4.424309136736732206, 1.121156565774838354, -1.440799707636587712 ) ) ;
#211028 = CARTESIAN_POINT ( 'NONE',  ( 1.375751926856683127, -1.915142299924106339, 0.4244507266663796741 ) ) ;
#211029 = CARTESIAN_POINT ( 'NONE',  ( -0.03531552556956805977, -2.054970391365168680, -0.5093743926467135807 ) ) ;
#211030 = CARTESIAN_POINT ( 'NONE',  ( 0.6823417656249899377, 3.988541667008085767, -1.181850606188754593 ) ) ;
#211031 = CARTESIAN_POINT ( 'NONE',  ( 3.836594282542909795, 6.459481848733281240, 1.082531754730558626 ) ) ;
#211032 = CARTESIAN_POINT ( 'NONE',  ( 7.751511138711133064, 10.06651563329490529, -1.599625672291262513 ) ) ;
#211033 = CARTESIAN_POINT ( 'NONE',  ( 2.174623584685225541, 0.9092215167782154994, 1.915816808323366871 ) ) ;
#211034 = CARTESIAN_POINT ( 'NONE',  ( -3.795919822146289313, 5.451659097302528068, -1.443375672974053447 ) ) ;
#211035 = LINE ( 'NONE', #13903, #49567 ) ;
#211036 = CARTESIAN_POINT ( 'NONE',  ( -3.267151830768946663, 6.755501535964989479, -0.7216878364870257245 ) ) ;
#211037 = CARTESIAN_POINT ( 'NONE',  ( 0.6024989291013755910, 2.064475859885641640, 0.1558578049991043990 ) ) ;
#211039 = CARTESIAN_POINT ( 'NONE',  ( 1.499999999999993117, 13.88541666734946034, 0.8660254037844409281 ) ) ;
#211038 = CARTESIAN_POINT ( 'NONE',  ( 6.883263157960403333, 6.034387817901857964, 2.748704107105720773 ) ) ;
#211041 = ORIENTED_EDGE ( 'NONE', *, *, #3651, .F. ) ;
#211040 = CARTESIAN_POINT ( 'NONE',  ( 2.719623178692368359, 1.877883874979644263, 1.186199984364836313 ) ) ;
#211042 = CARTESIAN_POINT ( 'NONE',  ( 1.196342457394595993, 2.030139636617489085, 1.078195451733245047 ) ) ;
#211044 = CARTESIAN_POINT ( 'NONE',  ( 5.295784840496287060, -1.454754056633072778, -1.462402424637335052 ) ) ;
#211043 = CARTESIAN_POINT ( 'NONE',  ( 4.220665892555866883, 3.818531717603609987, -0.7998128361456211532 ) ) ;
#211046 = CARTESIAN_POINT ( 'NONE',  ( 0.000000000000000000, -2.537500000000000977, -4.012584370867899430 ) ) ;
#211045 = CARTESIAN_POINT ( 'NONE',  ( 6.527324610336440180, 6.579909898339485252, 0.7998128361456331437 ) ) ;
#211047 = CARTESIAN_POINT ( 'NONE',  ( 6.235824307642648279, 6.239826211863360506, 0.000000000000000000 ) ) ;
#211048 = CARTESIAN_POINT ( 'NONE',  ( 0.2333540202161427102, 1.346341334450983140, -2.298657068330804076 ) ) ;
#211049 = CARTESIAN_POINT ( 'NONE',  ( 5.741722636381445533, 1.839460222191912964, 0.08393339073512617876 ) ) ;
#211051 = VERTEX_POINT ( 'NONE', #154837 ) ;
#211050 = CARTESIAN_POINT ( 'NONE',  ( 3.948449050077836642, 5.629609863222681199, 1.599625672291267398 ) ) ;
#211052 = CARTESIAN_POINT ( 'NONE',  ( -0.2104748580754183807, 4.084054299358617079, -2.658391380015924010 ) ) ;
#211053 = CARTESIAN_POINT ( 'NONE',  ( 1.588428401085600461, -0.2480725091915989278, -1.706701089166535512 ) ) ;
#211054 = CARTESIAN_POINT ( 'NONE',  ( 1.376185782568883020, -2.007256511855738612, -0.1928315418098166534 ) ) ;
#211055 = CARTESIAN_POINT ( 'NONE',  ( 1.987358909443589283, -2.298030411116751992, 0.06136411900238383788 ) ) ;
#211056 = CARTESIAN_POINT ( 'NONE',  ( 1.364683531249990311, 4.446875000341417028, 1.214306433183764966E-14 ) ) ;
#211057 = CARTESIAN_POINT ( 'NONE',  ( 2.214515517796631805, -1.065126590517451843, -1.995962479041712534 ) ) ;
#211058 = CARTESIAN_POINT ( 'NONE',  ( 3.651088154774425387, -1.721711045478736102, 1.212656735320973400 ) ) ;
#211059 = CARTESIAN_POINT ( 'NONE',  ( -7.783789588021474692, 8.253711738879413673, 0.7216878364870317197 ) ) ;
#211060 = CARTESIAN_POINT ( 'NONE',  ( 2.987294507434365087, 1.248747198882380394, 1.254300180652974550 ) ) ;
#211061 = CARTESIAN_POINT ( 'NONE',  ( 5.660692828905515839, 6.562895374266609849, -1.199719254218445830 ) ) ;
#211063 = CARTESIAN_POINT ( 'NONE',  ( 5.583585467610721054, -1.033564708330332316, 2.046191781174087509 ) ) ;
#211062 = CARTESIAN_POINT ( 'NONE',  ( 3.702785349863636277, 7.334016984900627811, -0.7216878364870338292 ) ) ;
#211064 = B_SPLINE_CURVE_WITH_KNOTS ( 'NONE', 3,
 ( #13267, #163804, #44730, #12195, #177917, #172859 ),
 .UNSPECIFIED., .F., .F.,
 ( 4, 2, 4 ),
 ( 1.087951779939714852E-13, 0.0004226202102664585575, 0.0008452404204241236070 ),
 .UNSPECIFIED. ) ;
#211065 = CARTESIAN_POINT ( 'NONE',  ( 5.068220161613846031, -1.734768455660203434, -0.6171159064975312303 ) ) ;
#211067 = EDGE_CURVE ( 'NONE', #175025, #204806, #130643, .T. ) ;
#211066 = CARTESIAN_POINT ( 'NONE',  ( -3.588104209110990706, 7.337872010604796991, 1.040834085586084257E-14 ) ) ;
#211068 = CARTESIAN_POINT ( 'NONE',  ( 5.978782553502139940, 6.077593855281705260, -0.7216878364870257245 ) ) ;
#211069 = CARTESIAN_POINT ( 'NONE',  ( -0.7500000000000215383, 2.941666666666689522, 1.299038105676671107 ) ) ;
#211070 = CARTESIAN_POINT ( 'NONE',  ( 4.593798273609356997, -2.190911875110569174, -0.05534364095756416635 ) ) ;
#211071 = CARTESIAN_POINT ( 'NONE',  ( -5.057354993097396445, 5.859001232490445688, -1.199719254218446718 ) ) ;
#211072 = CARTESIAN_POINT ( 'NONE',  ( 0.1341411654174105572, 8.212692222353361160, -2.039118504324965109 ) ) ;
#211073 = CARTESIAN_POINT ( 'NONE',  ( 5.305644874903189034, 7.627616123249468139, -1.238305686157632701 ) ) ;
#211074 = CARTESIAN_POINT ( 'NONE',  ( -0.6823417656249969321, 3.967708333674754950, -1.181850606188749264 ) ) ;
#211075 = CARTESIAN_POINT ( 'NONE',  ( 2.754421912756400026, 0.6492094756798562072, 1.813941749866236242 ) ) ;
#211076 = CARTESIAN_POINT ( 'NONE',  ( 0.6823417656249934904, 8.942708333674733723, 1.181850606188764807 ) ) ;
#211077 = CARTESIAN_POINT ( 'NONE',  ( -3.470524135418294520, 6.992769224722559684, -0.7216878364870267237 ) ) ;
#211078 = CARTESIAN_POINT ( 'NONE',  ( 6.521762860236213655, -0.4636855090699961712, 2.076960040381255812 ) ) ;
#211079 = CARTESIAN_POINT ( 'NONE',  ( -5.804299160426237059, 7.865044668620976509, -1.443375672974066548 ) ) ;
#211080 = ORIENTED_EDGE ( 'NONE', *, *, #111897, .T. ) ;
#211082 = CARTESIAN_POINT ( 'NONE',  ( 4.294896950644969458, 7.100883960644856607, 1.224551608757080245 ) ) ;
#211081 = CARTESIAN_POINT ( 'NONE',  ( -3.851925040058333582, 7.508013290127760087, -0.7216878364870458196 ) ) ;
#211083 = CARTESIAN_POINT ( 'NONE',  ( 5.192936529234042808, 6.017179691316550283, -1.199719254218452047 ) ) ;
#211084 = LINE ( 'NONE', #207892, #718 ) ;
#211085 = CARTESIAN_POINT ( 'NONE',  ( -2.324999999999999289, 0.05106137233530610997, -0.5000000000000003331 ) ) ;
#211086 = CARTESIAN_POINT ( 'NONE',  ( 0.1914555686804124413, 7.015040164655834687, -3.986720219540934362 ) ) ;
#211087 = CARTESIAN_POINT ( 'NONE',  ( -0.6823417656250212460, 4.613541667008086655, 1.181850606188767472 ) ) ;
#211088 = CARTESIAN_POINT ( 'NONE',  ( 2.383973883943972805, -0.2989522671389834851, -1.714397271258593092 ) ) ;
#211089 = DIRECTION ( 'NONE',  ( 1.000000000000000000, -0.000000000000000000, -0.000000000000000000 ) ) ;
#211090 = CARTESIAN_POINT ( 'NONE',  ( 0.5198770262540284293, 1.941052373433370670, -0.2841105942011297736 ) ) ;
#211091 = CARTESIAN_POINT ( 'NONE',  ( 1.364683531249986537, -0.3239583329919163424, 0.7879004041258500513 ) ) ;
#211092 = LINE ( 'NONE', #149312, #191343 ) ;
#211093 = CARTESIAN_POINT ( 'NONE',  ( 6.192270064542984898, -2.150811787302907785, -0.2168040374768212541 ) ) ;
#211094 = CARTESIAN_POINT ( 'NONE',  ( -8.839026081105473054, 12.39961529701003684, -1.199719254218446718 ) ) ;
#211095 = CARTESIAN_POINT ( 'NONE',  ( -5.707619481228814351, 9.602713794834864203, -0.7216878364870207285 ) ) ;
#211096 = CARTESIAN_POINT ( 'NONE',  ( 6.086834708314957432, -0.3123483334277510348, -2.138898144987111838 ) ) ;
#211098 = ORIENTED_EDGE ( 'NONE', *, *, #209526, .F. ) ;
#211097 = CARTESIAN_POINT ( 'NONE',  ( -0.2106725631050176961, 4.086973797293973476, -2.558389695104481554 ) ) ;
#211099 = CARTESIAN_POINT ( 'NONE',  ( -1.201851678989727383E-14, 4.196875000341417028, -1.575800808251660134 ) ) ;
#211100 = CARTESIAN_POINT ( 'NONE',  ( 0.3329892237508432773, -1.712944741146247063, 0.7519245212838022718 ) ) ;
#211101 = CARTESIAN_POINT ( 'NONE',  ( 6.081315976822482483, 1.162057296412899676, -1.286934115659829736 ) ) ;
#211103 = CARTESIAN_POINT ( 'NONE',  ( 3.228257827484398490, 2.138632370135685523, 0.4780590757816546854 ) ) ;
#211102 = CARTESIAN_POINT ( 'NONE',  ( -0.6801582343750420812, -0.06770833299193229626, 1.178068619123801675 ) ) ;
#211104 = CARTESIAN_POINT ( 'NONE',  ( 2.960362034815271048, 2.296572897674476810, -0.2250602657276803420 ) ) ;
#211105 = CARTESIAN_POINT ( 'NONE',  ( 5.958293153512181917, 0.8310434803317863217, 1.885964484847465705 ) ) ;
#211106 = CARTESIAN_POINT ( 'NONE',  ( 1.482261173788253394, -0.2847754331270537231, -1.920845095517382362 ) ) ;
#211107 = CARTESIAN_POINT ( 'NONE',  ( -5.816084710138169633, 8.768887347594400694, 1.082531754730548412 ) ) ;
#211108 = CARTESIAN_POINT ( 'NONE',  ( -0.1288460037566284688, -8.008893676011963336, -9.499262961676866013 ) ) ;
#211109 = FACE_OUTER_BOUND ( 'NONE', #164926, .T. ) ;
#211110 = CARTESIAN_POINT ( 'NONE',  ( 4.008146050417991546, -0.8085630067716749192, 1.960596031080278356 ) ) ;
#211111 = SURFACE_STYLE_FILL_AREA ( #12909 ) ;
#211112 = CARTESIAN_POINT ( 'NONE',  ( 2.004529941291322448, -1.955172360644286789, 0.4926429297785542283 ) ) ;
#211113 = CARTESIAN_POINT ( 'NONE',  ( -6.548225005276122168, 6.741943382351338165, 0.7216878364870317197 ) ) ;
#211114 = CARTESIAN_POINT ( 'NONE',  ( 5.139771110516938357, -1.557344429106276573, -1.563758303505815572 ) ) ;
#211115 = CARTESIAN_POINT ( 'NONE',  ( 3.285556943750000514, -0.7510416661887079348, 1.896917185911906500 ) ) ;
#211116 = CARTESIAN_POINT ( 'NONE',  ( 1.886507792743700940E-16, 13.20000000000000284, 1.540450515248283025 ) ) ;
#211117 = CARTESIAN_POINT ( 'NONE',  ( 0.3283667639546791195, 1.746078182827022429, 0.5332771064449209897 ) ) ;
#211118 = CARTESIAN_POINT ( 'NONE',  ( -6.454563648557663846, 9.688018802362710957, -1.199719254218452047 ) ) ;
#211120 = CARTESIAN_POINT ( 'NONE',  ( 6.825078400183511640, 3.679815135839346496, 2.758192972206894744 ) ) ;
#211119 = CARTESIAN_POINT ( 'NONE',  ( -4.611335679197930304, 8.465601755996580380, 0.3353434889079315862 ) ) ;
#211121 = CARTESIAN_POINT ( 'NONE',  ( -10.41980074470002648, 5.020554563858687480, 5.279403930596816785 ) ) ;
#211122 = VERTEX_POINT ( 'NONE', #206765 ) ;
#211123 = CARTESIAN_POINT ( 'NONE',  ( 4.557529213136806590, 0.4535224272249741562, -2.010195360780684393 ) ) ;
#211124 = CARTESIAN_POINT ( 'NONE',  ( -3.505400730386704341E-15, 2.703125000341406459, 1.570758158831794260 ) ) ;
#211125 = CARTESIAN_POINT ( 'NONE',  ( -0.07933191752142512709, -7.643695121331865572, 9.499668754586258146 ) ) ;
#211126 = CARTESIAN_POINT ( 'NONE',  ( -6.254388934605767503, 6.191208599995166040, 0.7998128361456341429 ) ) ;
#211127 = CARTESIAN_POINT ( 'NONE',  ( -3.817502770699643388, 6.611447778194983194, 1.199719254218452935 ) ) ;
#211128 = CARTESIAN_POINT ( 'NONE',  ( 3.053383268589305644, -1.780226508164801213, 0.9538969713841909392 ) ) ;
#211129 = CARTESIAN_POINT ( 'NONE',  ( -1.500000000000013101, 0.9208333333333594828, 0.8660254037844403729 ) ) ;
#211131 = CARTESIAN_POINT ( 'NONE',  ( 8.270110514656021650, 11.63191745286530576, 1.082531754730557072 ) ) ;
#211130 = CARTESIAN_POINT ( 'NONE',  ( -4.573896719763875574, 6.429575154514868274, -1.599625672291271394 ) ) ;
#211132 = CARTESIAN_POINT ( 'NONE',  ( 7.983053520348166288, 8.207983950027992748, -0.7998128361456281477 ) ) ;
#211133 = CARTESIAN_POINT ( 'NONE',  ( 2.553650737195617637, 0.5510486643308718513, -1.985768735985605549 ) ) ;
#211134 = CARTESIAN_POINT ( 'NONE',  ( 3.410779880581996437, -1.203353552534730309, -1.617818353255598085 ) ) ;
#211135 = ORIENTED_EDGE ( 'NONE', *, *, #5562, .F. ) ;
#211136 =( BOUNDED_CURVE ( )  B_SPLINE_CURVE ( 3, ( #21934, #88044, #154115, #110759 ),
 .UNSPECIFIED., .F., .T. ) 
 B_SPLINE_CURVE_WITH_KNOTS ( ( 4, 4 ),
 ( 0.5000000000000011102, 1.000000000000000000 ),
 .UNSPECIFIED. ) 
 CURVE ( )  GEOMETRIC_REPRESENTATION_ITEM ( )  RATIONAL_B_SPLINE_CURVE ( ( 0.9999999999999985567, 0.3333333333333333703, 0.3333333333333348691, 1.000000000000000000 ) ) 
 REPRESENTATION_ITEM ( '' )  );
#211137 = CARTESIAN_POINT ( 'NONE',  ( 0.000000000000000000, 13.49999999999999822, 0.000000000000000000 ) ) ;
#211138 = CARTESIAN_POINT ( 'NONE',  ( 4.761938266897790761, 6.578680616179308771, 1.599625672291267398 ) ) ;
#211140 = ORIENTED_EDGE ( 'NONE', *, *, #171813, .T. ) ;
#211139 = CARTESIAN_POINT ( 'NONE',  ( 1.734723475976807094E-15, 14.55305236562695193, 11.95586206896570580 ) ) ;
#211141 = CARTESIAN_POINT ( 'NONE',  ( 3.145861080134567000, -0.1455099638626895786, -2.010896398064919488 ) ) ;
#211142 = CARTESIAN_POINT ( 'NONE',  ( 0.8492453639068753279, 1.839163117542693904, -0.08803940487626948919 ) ) ;
#211143 = CARTESIAN_POINT ( 'NONE',  ( 0.08326089795122111614, -2.240168680488762387, -0.5538300120674977123 ) ) ;
#211144 = CARTESIAN_POINT ( 'NONE',  ( 3.888156192069020634, 7.758209000714329839, 1.040834085586084257E-14 ) ) ;
#211145 = CARTESIAN_POINT ( 'NONE',  ( 2.267066545249882381, -1.975312647937790711, -0.8782872871702240847 ) ) ;
#211146 = CARTESIAN_POINT ( 'NONE',  ( -4.609409038966248318, 5.440360635957812718, -1.082531754730544860 ) ) ;
#211147 = CARTESIAN_POINT ( 'NONE',  ( 5.032460059670339270, 0.6174496738353585368, 2.025276144886530627 ) ) ;
#211148 = EDGE_CURVE ( 'NONE', #72069, #184329, #145361, .T. ) ;
#211149 = CARTESIAN_POINT ( 'NONE',  ( 3.028993686180006861, 2.741750000184225211, -2.499999999999995115 ) ) ;
#211150 = CARTESIAN_POINT ( 'NONE',  ( 0.7603692911175019553, -1.357789551990191246, 1.287012767582619510 ) ) ;
#211151 = CARTESIAN_POINT ( 'NONE',  ( 6.227413254736037906, -1.856526228437559434, 0.6636957074077839414 ) ) ;
#211153 = CARTESIAN_POINT ( 'NONE',  ( 7.741342523278692767, 11.01502146292508044, 1.082531754730558626 ) ) ;
#211152 = CARTESIAN_POINT ( 'NONE',  ( -0.6823417656250212460, 3.551041667008085323, 1.181850606188767472 ) ) ;
#211155 = CARTESIAN_POINT ( 'NONE',  ( 5.865875422609286183, 2.075172955015105014, -0.3584678469405917500 ) ) ;
#211154 = CARTESIAN_POINT ( 'NONE',  ( -6.714312387265696458, 8.856450423275211037, 1.599625672291283607 ) ) ;
#211156 = CARTESIAN_POINT ( 'NONE',  ( 5.951642636407409093, 1.565221049572671719, 1.355249363302114318 ) ) ;
#211157 = CARTESIAN_POINT ( 'NONE',  ( 4.984594031318565932, 8.967110136513669616, 0.7998128361456462443 ) ) ;
#211158 = CARTESIAN_POINT ( 'NONE',  ( -7.250913225210214641, 7.353820272367037170, 0.7998128361456341429 ) ) ;
#211159 = CARTESIAN_POINT ( 'NONE',  ( 6.639320575229256782, 0.5729255850590134758, 2.155858052613166986 ) ) ;
#211160 = CARTESIAN_POINT ( 'NONE',  ( 5.436387729582301098, 1.942169232299725046, 0.3377773032272758380 ) ) ;
#211161 = CARTESIAN_POINT ( 'NONE',  ( -0.2046613956954954905, -0.1581703332043625232, -2.086340352340488646 ) ) ;
#211162 = CARTESIAN_POINT ( 'NONE',  ( -1.402160292154681736E-14, 0.1187500006828157706, -1.732050807568870754 ) ) ;
#211163 = CARTESIAN_POINT ( 'NONE',  ( 4.125798732227327292, -2.208944405816467338, 0.6678306985251744043 ) ) ;
#211164 = CARTESIAN_POINT ( 'NONE',  ( 1.920832408274443903, -1.461550516301242775, 1.455605961035913776 ) ) ;
#211165 = CARTESIAN_POINT ( 'NONE',  ( 5.992340707560141588, 9.934888558888093968, 0.7216878364870438212 ) ) ;
#211166 = CARTESIAN_POINT ( 'NONE',  ( 6.391743074199808916, 6.421731439513382433, -0.7998128361456481317 ) ) ;
#211167 = CARTESIAN_POINT ( 'NONE',  ( 3.790386463472274148, 6.579812086429759788, 1.199719254218452047 ) ) ;
#211168 = CARTESIAN_POINT ( 'NONE',  ( -1.364683531249997417, 2.571875000341422357, 1.214306433183764966E-14 ) ) ;
#211169 = CARTESIAN_POINT ( 'NONE',  ( 0.1453961305826048100, 14.48154449402677812, 11.99911913288686627 ) ) ;
#211170 = CARTESIAN_POINT ( 'NONE',  ( 6.602457619730771832, 6.805214765881779648, 0.7216878364870317197 ) ) ;
#211171 = CARTESIAN_POINT ( 'NONE',  ( 4.756392321286846858, -2.170573799849393470, -0.05792142139850359195 ) ) ;
#211172 = CARTESIAN_POINT ( 'NONE',  ( -0.4577034257980932552, -0.8887487162305418575, -3.253519940713586855 ) ) ;
#211174 = CARTESIAN_POINT ( 'NONE',  ( 3.614658571667620279, -0.1319153736358945894, 1.836568937333193485 ) ) ;
#211173 = CARTESIAN_POINT ( 'NONE',  ( -3.958617665510279160, 5.641473247893851628, -1.443375672974053447 ) ) ;
#211176 = CARTESIAN_POINT ( 'NONE',  ( 6.620655732516684822, 7.053712996964945248, 2.324417015927725760 ) ) ;
#211175 = CARTESIAN_POINT ( 'NONE',  ( -1.001543065824772872E-14, 4.571875000341418804, 1.575800808251672791 ) ) ;
#211177 = CARTESIAN_POINT ( 'NONE',  ( 4.933237592207079025, -1.549687834843778811, -1.549900206446311657 ) ) ;
#211178 = CARTESIAN_POINT ( 'NONE',  ( -10.95308175811721085, 11.29999999999999893, -1.800000000000001155 ) ) ;
#211179 = CARTESIAN_POINT ( 'NONE',  ( 5.664971525351325532, -2.042639428312309935, -0.9732368426803981176 ) ) ;
#211180 = ORIENTED_EDGE ( 'NONE', *, *, #91960, .T. ) ;
#211181 = CARTESIAN_POINT ( 'NONE',  ( -4.418902842294746947, 7.322973332268160718, -1.241058569461401362 ) ) ;
#211182 = CARTESIAN_POINT ( 'NONE',  ( 4.978670620768666844, 8.057607364700732688, 1.103355461389814662 ) ) ;
#211183 = AXIS2_PLACEMENT_3D ( 'NONE', #94896, #128532, #213918 ) ;
#211184 = CARTESIAN_POINT ( 'NONE',  ( -6.089020385868867180, 7.236850217336030511, -1.082531754730549967 ) ) ;
#211185 = CARTESIAN_POINT ( 'NONE',  ( 5.099275172515607579, 5.121778254122544283, -0.7216878364870458196 ) ) ;
#211186 = CARTESIAN_POINT ( 'NONE',  ( 0.8481071238514601429, 0.5083433500535933236, 1.695271877703796504 ) ) ;
#211187 =( BOUNDED_SURFACE ( )  B_SPLINE_SURFACE ( 1, 2, ( 
 ( #112956, #177896, #15359, #178967, #144368, #13245, #95602, #161650, #27359, #79318, #145434, #30582, #63065, #96663, #114030, #162716, #14288, #80383, #31645, #97722, #163780, #59863, #150731, #16421, #213550, #157, #164831, #84640, #115080, #182127, #53211, #147529, #135540, #2291, #119342, #169087, #68368, #201565, #134501, #52147, #50014, #116138, #3365, #185329, #65173, #36952, #131328, #98776, #82501, #67294, #33756, #148588, #200504, #85703, #132371, #151791, #66224, #198373, #181076, #99833, #165899, #17483, #199440, #103032, #83569, #118275, #81452, #149651, #1232, #133433, #197322, #48962, #51083, #69435, #32694, #117208, #183205, #34811, #100886, #166973, #18564, #184260, #19632, #35886, #101962, #168028, #5488, #38032, #8713, #137677, #22814, #123639, #87847, #186395, #173378, #71569, #187468, #4423, #70493, #55344, #140899, #91064, #20686, #7636, #203698, #105183, #170152, #104102, #120421, #205847, #153918, #121496, #21738, #24962, #156047, #40166, #108430, #86777, #138743, #39098, #56413, #171219, #106280, #204761, #202634, #88928, #42314, #89996, #172301, #136609, #23890, #206910, #154982, #57480, #107356, #54284, #122574, #6567, #72647, #152848, #188536, #73721, #139818, #189602, #157124, #41248, #74798, #58540, #190653, #124695, #209029, #146217, #126827, #159233, #194934, #27095, #211168, #110560, #46571, #192784, #109498, #12971, #176562, #11911, #111625, #174450, #125759, #28171, #62793, #94267, #175505, #44442, #210101, #61741, #160307, #127908, #77984, #162450, #144107, #193860, #161388, #177638, #45509, #191721, #112690, #93202, #60664, #29246, #95338, #130023, #80112, #79047, #145163, #128955, #178701, #30315, #212235, #10834, #96400, #14026, #143034, #63868, #76908, #196014, #47650, #26026, #92136, #158191, #9782, #75854, #141962, #207974, #59601, #43377, #99570, #966, #64924, #67031, #164568, #180812, #34556, #15098, #149384, #51891, #166703, #69167, #165634, #201301, #182940, #163512, #151528, #135287, #197061, #133168, #33497, #82238, #116940, #17222, #3097, #81187, #85443, #147265, #213297, #16153, #18294, #83299, #113761, #100627, #148329, #199168, #50814, #181861, #131073, #214329, #49749, #84380, #65961, #150467, #19363, #2028, #68097, #48699, #98506, #114813, #134232, #35618, #200241, #32438, #31381, #132110, #198118, #118014, #115876, #184003, #179765, #97457, #167766, #101696, #90804, #140642, #188272, #107098, #106022, #23636, #21478, #87587, #189347, #173121, #119078, #24702, #102771, #70235, #136348, #38836, #104919, #205585, #139558, #122315, #52941, #57222, #202369, #120157, #156868, #37768, #8454, #103840, #172043, #89744, #153659, #5228, #40987, #74542, #185059, #36684, #168826, #54018, #186133, #170960, #22560, #123382, #20430, #39913, #86513, #152578, #169889, #71302, #4165, #137415, #203434, #55088, #121237, #88665, #155793, #56153, #138481, #187207, #154725 ),
 ( #6308, #72382, #204503, #7377, #73456, #45253, #213835, #43131, #65453, #59348, #75604, #25771, #109247, #9531, #141715, #110305, #32985, #191466, #61482, #49248, #175255, #10585, #207725, #206655, #190401, #60410, #131602, #197604, #42059, #115369, #76660, #125503, #11656, #26841, #181361, #147816, #126571, #124444, #192531, #92944, #158989, #99061, #142774, #208780, #95075, #44185, #157938, #165116, #176313, #27917, #108172, #174198, #94013, #16708, #82793, #58287, #193611, #160052, #77729, #143851, #209843, #91883, #177375, #127647, #111371, #28989, #161124, #15646, #81734, #22026, #148867, #52437, #34043, #184547, #167256, #168319, #118563, #116423, #67578, #170439, #3644, #19915, #198656, #86000, #120715, #117498, #185616, #20966, #119632, #169381, #68654, #38316, #104392, #134777, #36168, #100116, #102246, #199729, #1514, #69723, #50305, #152074, #87063, #201851, #441, #200785, #66510, #135827, #182414, #186688, #132652, #17766, #53496, #37249, #183489, #103319, #153135, #166178, #83854, #149944, #133723, #51375, #35098, #4708, #70783, #101169, #136896, #18843, #202923, #54567, #2584, #84928, #151016, #3120, #54043, #118038, #20453, #187229, #52963, #36707, #34579, #51915, #68121, #168850, #203456, #136372, #2050, #199191, #200264, #150491, #70258, #100651, #167791, #38858, #50839, #121257, #202391, #104942, #154747, #120180, #170982, #186156, #37790, #35641, #101720, #55111, #22581, #116966, #88687, #182964, #84403, #134257, #119101, #185083, #71325, #153680, #103864, #67054, #137440, #184025, #19386, #166729, #85465, #18320, #151551, #69190, #86536, #169913, #135311, #152602, #201325, #4188, #155815, #107120, #157960, #206678, #176333, #126592, #58309, #59371, #9553, #141738, #75628, #44208, #73480, #191487, #43156, #189368, #124465, #139580, #109268, #190424, #173143, #42081, #175276, #207745, #108196, #125529, #6330, #172065, #74563, #26862, #140663, #7399, #24724, #174220, #25795, #8477, #91904, #92966, #208803, #41010, #205606, #159012, #10606, #57244, #76682, #123404, #89769, #39934, #90827, #23658, #156889, #142798, #110328, #60432, #192553, #27940, #94035, #72403, #138503, #204526, #188294, #106042, #209865, #61503, #160074, #11676, #77751, #143872, #175786, #157405, #144387, #94547, #76135, #74005, #10059, #141185, #173669, #210387, #58820, #158458, #44727, #8997, #107637, #160585, #207195, #108704, #140098, #206125, #190934, #62029, #12192, #156334, #143313, #124973, #26305, #91344, #25244, #41525, #127110, #75072, #42598, #174733, #78263, #77193, #27378, #29528, #7920, #59884, #92419, #191996, #142238, #93479, #126033, #123915, #208250, #177914, #11117, #159518, #57755, #209306, #128184, #43661, #193075, #28453, #189883, #109777, #60953, #110835, #176840, #194145, #45793, #111914, #50034, #83589, #116159, #182145, #149671, #51100, #213569, #48981, #199458, #181096, #1252, #183223, #161670 ) ),
 .UNSPECIFIED., .F., .F., .T. ) 
 B_SPLINE_SURFACE_WITH_KNOTS ( ( 2, 2 ),
 ( 3, 2, 2, 2, 2, 2, 2, 2, 2, 2, 2, 2, 2, 2, 2, 2, 2, 2, 2, 2, 2, 2, 2, 2, 2, 2, 2, 2, 2, 2, 2, 2, 2, 2, 2, 2, 2, 2, 2, 2, 2, 2, 2, 2, 2, 2, 2, 2, 2, 2, 2, 2, 2, 2, 2, 2, 2, 2, 2, 2, 2, 2, 2, 2, 2, 2, 2, 2, 2, 2, 2, 2, 2, 2, 2, 2, 2, 2, 2, 2, 2, 2, 2, 2, 2, 2, 2, 2, 2, 2, 2, 2, 2, 2, 2, 2, 2, 2, 2, 2, 2, 2, 2, 2, 2, 2, 2, 2, 2, 2, 2, 2, 2, 2, 2, 2, 2, 2, 2, 2, 2, 2, 2, 2, 2, 2, 2, 2, 2, 2, 2, 2, 2, 2, 2, 2, 2, 2, 2, 2, 2, 2, 2, 2, 2, 2, 2, 2, 2, 2, 2, 2, 2, 2, 2, 2, 2, 2, 2, 2, 2, 2, 2, 2, 2, 2, 2, 2, 3 ),
 ( 0.000000000000000000, 1.000000000000000000 ),
 ( 0.000000000000000000, 0.005952380952380952051, 0.01190476190476190410, 0.01785714285714285615, 0.02380952380952380820, 0.02976190476190476025, 0.03571428571428571230, 0.04166666666666666435, 0.04761904761904761640, 0.05357142857142856845, 0.05952380952380952051, 0.06547619047619047949, 0.07142857142857142461, 0.07738095238095238360, 0.08333333333333332871, 0.08928571428571428770, 0.09523809523809523281, 0.1011904761904761918, 0.1071428571428571369, 0.1130952380952380959, 0.1190476190476190410, 0.1250000000000000000, 0.1309523809523809590, 0.1369047619047619180, 0.1428571428571428492, 0.1488095238095238082, 0.1547619047619047672, 0.1607142857142857262, 0.1666666666666666574, 0.1726190476190476164, 0.1785714285714285754, 0.1845238095238095344, 0.1904761904761904656, 0.1964285714285714246, 0.2023809523809523836, 0.2083333333333333426, 0.2142857142857142738, 0.2202380952380952328, 0.2261904761904761918, 0.2321428571428571508, 0.2380952380952380820, 0.2440476190476190410, 0.2500000000000000000, 0.2559523809523809312, 0.2619047619047619180, 0.2678571428571428492, 0.2738095238095238360, 0.2797619047619047672, 0.2857142857142856984, 0.2916666666666666852, 0.2976190476190476164, 0.3035714285714285476, 0.3095238095238095344, 0.3154761904761904656, 0.3214285714285714524, 0.3273809523809523836, 0.3333333333333333148, 0.3392857142857143016, 0.3452380952380952328, 0.3511904761904761640, 0.3571428571428571508, 0.3630952380952380820, 0.3690476190476190688, 0.3750000000000000000, 0.3809523809523809312, 0.3869047619047619180, 0.3928571428571428492, 0.3988095238095238360, 0.4047619047619047672, 0.4107142857142856984, 0.4166666666666666852, 0.4226190476190476164, 0.4285714285714285476, 0.4345238095238095344, 0.4404761904761904656, 0.4464285714285714524, 0.4523809523809523836, 0.4583333333333333148, 0.4642857142857143016, 0.4702380952380952328, 0.4761904761904761640, 0.4821428571428571508, 0.4880952380952380820, 0.4940476190476190688, 0.5000000000000000000, 0.5059523809523809312, 0.5119047619047618625, 0.5178571428571429047, 0.5238095238095238360, 0.5297619047619047672, 0.5357142857142856984, 0.5416666666666666297, 0.5476190476190476719, 0.5535714285714286031, 0.5595238095238095344, 0.5654761904761904656, 0.5714285714285713969, 0.5773809523809523281, 0.5833333333333333703, 0.5892857142857143016, 0.5952380952380952328, 0.6011904761904761640, 0.6071428571428570953, 0.6130952380952381375, 0.6190476190476190688, 0.6250000000000000000, 0.6309523809523809312, 0.6369047619047618625, 0.6428571428571429047, 0.6488095238095238360, 0.6547619047619047672, 0.6607142857142856984, 0.6666666666666666297, 0.6726190476190476719, 0.6785714285714286031, 0.6845238095238095344, 0.6904761904761904656, 0.6964285714285713969, 0.7023809523809523281, 0.7083333333333333703, 0.7142857142857143016, 0.7202380952380952328, 0.7261904761904761640, 0.7321428571428570953, 0.7380952380952381375, 0.7440476190476190688, 0.7500000000000000000, 0.7559523809523809312, 0.7619047619047618625, 0.7678571428571429047, 0.7738095238095238360, 0.7797619047619047672, 0.7857142857142856984, 0.7916666666666666297, 0.7976190476190476719, 0.8035714285714286031, 0.8095238095238095344, 0.8154761904761904656, 0.8214285714285713969, 0.8273809523809523281, 0.8333333333333333703, 0.8392857142857143016, 0.8452380952380952328, 0.8511904761904761640, 0.8571428571428570953, 0.8630952380952381375, 0.8690476190476190688, 0.8750000000000000000, 0.8809523809523809312, 0.8869047619047618625, 0.8928571428571429047, 0.8988095238095238360, 0.9047619047619047672, 0.9107142857142856984, 0.9166666666666666297, 0.9226190476190476719, 0.9285714285714286031, 0.9345238095238095344, 0.9404761904761904656, 0.9464285714285713969, 0.9523809523809523281, 0.9583333333333333703, 0.9642857142857143016, 0.9702380952380952328, 0.9761904761904761640, 0.9821428571428570953, 0.9880952380952381375, 0.9940476190476190688, 1.000000000000000000 ),
 .UNSPECIFIED. ) 
 GEOMETRIC_REPRESENTATION_ITEM ( )  RATIONAL_B_SPLINE_SURFACE ( (
 ( 1.000000000000000000, 0.8660254037844387076, 1.000000000000000000, 0.8660254037844387076, 1.000000000000000000, 0.8660254037844387076, 1.000000000000000000, 0.8660254037844387076, 1.000000000000000000, 0.8660254037844387076, 1.000000000000000000, 0.8660254037844387076, 1.000000000000000000, 0.8660254037844387076, 1.000000000000000000, 0.8660254037844387076, 1.000000000000000000, 0.8660254037844387076, 1.000000000000000000, 0.8660254037844387076, 1.000000000000000000, 0.8660254037844387076, 1.000000000000000000, 0.8660254037844387076, 1.000000000000000000, 0.8660254037844387076, 1.000000000000000000, 0.8660254037844387076, 1.000000000000000000, 0.8660254037844387076, 1.000000000000000000, 0.8660254037844387076, 1.000000000000000000, 0.8660254037844387076, 1.000000000000000000, 0.8660254037844387076, 1.000000000000000000, 0.8660254037844387076, 1.000000000000000000, 0.8660254037844387076, 1.000000000000000000, 0.8660254037844387076, 1.000000000000000000, 0.8660254037844387076, 1.000000000000000000, 0.8660254037844387076, 1.000000000000000000, 0.8660254037844387076, 1.000000000000000000, 0.8660254037844387076, 1.000000000000000000, 0.8660254037844387076, 1.000000000000000000, 0.8660254037844387076, 1.000000000000000000, 0.8660254037844387076, 1.000000000000000000, 0.8660254037844387076, 1.000000000000000000, 0.8660254037844387076, 1.000000000000000000, 0.8660254037844387076, 1.000000000000000000, 0.8660254037844387076, 1.000000000000000000, 0.8660254037844387076, 1.000000000000000000, 0.8660254037844387076, 1.000000000000000000, 0.8660254037844387076, 1.000000000000000000, 0.8660254037844387076, 1.000000000000000000, 0.8660254037844387076, 1.000000000000000000, 0.8660254037844387076, 1.000000000000000000, 0.8660254037844387076, 1.000000000000000000, 0.8660254037844387076, 1.000000000000000000, 0.8660254037844387076, 1.000000000000000000, 0.8660254037844387076, 1.000000000000000000, 0.8660254037844387076, 1.000000000000000000, 0.8660254037844387076, 1.000000000000000000, 0.8660254037844387076, 1.000000000000000000, 0.8660254037844387076, 1.000000000000000000, 0.8660254037844387076, 1.000000000000000000, 0.8660254037844387076, 1.000000000000000000, 0.8660254037844387076, 1.000000000000000000, 0.8660254037844387076, 1.000000000000000000, 0.8660254037844387076, 1.000000000000000000, 0.8660254037844387076, 1.000000000000000000, 0.8660254037844387076, 1.000000000000000000, 0.8660254037844387076, 1.000000000000000000, 0.8660254037844387076, 1.000000000000000000, 0.8660254037844387076, 1.000000000000000000, 0.8660254037844387076, 1.000000000000000000, 0.8660254037844387076, 1.000000000000000000, 0.8660254037844387076, 1.000000000000000000, 0.8660254037844387076, 1.000000000000000000, 0.8660254037844387076, 1.000000000000000000, 0.8660254037844387076, 1.000000000000000000, 0.8660254037844387076, 1.000000000000000000, 0.8660254037844387076, 1.000000000000000000, 0.8660254037844387076, 1.000000000000000000, 0.8660254037844387076, 1.000000000000000000, 0.8660254037844387076, 1.000000000000000000, 0.8660254037844387076, 1.000000000000000000, 0.8660254037844387076, 1.000000000000000000, 0.8660254037844387076, 1.000000000000000000, 0.8660254037844387076, 1.000000000000000000, 0.8660254037844387076, 1.000000000000000000, 0.8660254037844387076, 1.000000000000000000, 0.8660254037844387076, 1.000000000000000000, 0.8660254037844387076, 1.000000000000000000, 0.8660254037844387076, 1.000000000000000000, 0.8660254037844387076, 1.000000000000000000, 0.8660254037844387076, 1.000000000000000000, 0.8660254037844387076, 1.000000000000000000, 0.8660254037844387076, 1.000000000000000000, 0.8660254037844387076, 1.000000000000000000, 0.8660254037844387076, 1.000000000000000000, 0.8660254037844387076, 1.000000000000000000, 0.8660254037844387076, 1.000000000000000000, 0.8660254037844387076, 1.000000000000000000, 0.8660254037844387076, 1.000000000000000000, 0.8660254037844387076, 1.000000000000000000, 0.8660254037844387076, 1.000000000000000000, 0.8660254037844387076, 1.000000000000000000, 0.8660254037844387076, 1.000000000000000000, 0.8660254037844387076, 1.000000000000000000, 0.8660254037844387076, 1.000000000000000000, 0.8660254037844387076, 1.000000000000000000, 0.8660254037844387076, 1.000000000000000000, 0.8660254037844387076, 1.000000000000000000, 0.8660254037844387076, 1.000000000000000000, 0.8660254037844387076, 1.000000000000000000, 0.8660254037844387076, 1.000000000000000000, 0.8660254037844387076, 1.000000000000000000, 0.8660254037844387076, 1.000000000000000000, 0.8660254037844387076, 1.000000000000000000, 0.8660254037844387076, 1.000000000000000000, 0.8660254037844387076, 1.000000000000000000, 0.8660254037844387076, 1.000000000000000000, 0.8660254037844387076, 1.000000000000000000, 0.8660254037844387076, 1.000000000000000000, 0.8660254037844387076, 1.000000000000000000, 0.8660254037844387076, 1.000000000000000000, 0.8660254037844387076, 1.000000000000000000, 0.8660254037844387076, 1.000000000000000000, 0.8660254037844387076, 1.000000000000000000, 0.8660254037844387076, 1.000000000000000000, 0.8660254037844387076, 1.000000000000000000, 0.8660254037844387076, 1.000000000000000000, 0.8660254037844387076, 1.000000000000000000, 0.8660254037844387076, 1.000000000000000000, 0.8660254037844387076, 1.000000000000000000, 0.8660254037844387076, 1.000000000000000000, 0.8660254037844387076, 1.000000000000000000, 0.8660254037844387076, 1.000000000000000000, 0.8660254037844387076, 1.000000000000000000, 0.8660254037844387076, 1.000000000000000000, 0.8660254037844387076, 1.000000000000000000, 0.8660254037844387076, 1.000000000000000000, 0.8660254037844387076, 1.000000000000000000, 0.8660254037844387076, 1.000000000000000000, 0.8660254037844387076, 1.000000000000000000, 0.8660254037844387076, 1.000000000000000000, 0.8660254037844387076, 1.000000000000000000, 0.8660254037844387076, 1.000000000000000000, 0.8660254037844387076, 1.000000000000000000, 0.8660254037844387076, 1.000000000000000000, 0.8660254037844387076, 1.000000000000000000, 0.8660254037844387076, 1.000000000000000000, 0.8660254037844387076, 1.000000000000000000, 0.8660254037844387076, 1.000000000000000000, 0.8660254037844387076, 1.000000000000000000, 0.8660254037844387076, 1.000000000000000000, 0.8660254037844387076, 1.000000000000000000, 0.8660254037844387076, 1.000000000000000000, 0.8660254037844387076, 1.000000000000000000, 0.8660254037844387076, 1.000000000000000000, 0.8660254037844387076, 1.000000000000000000, 0.8660254037844387076, 1.000000000000000000, 0.8660254037844387076, 1.000000000000000000, 0.8660254037844387076, 1.000000000000000000, 0.8660254037844387076, 1.000000000000000000, 0.8660254037844387076, 1.000000000000000000, 0.8660254037844387076, 1.000000000000000000, 0.8660254037844387076, 1.000000000000000000, 0.8660254037844387076, 1.000000000000000000, 0.8660254037844387076, 1.000000000000000000, 0.8660254037844387076, 1.000000000000000000, 0.8660254037844387076, 1.000000000000000000, 0.8660254037844387076, 1.000000000000000000, 0.8660254037844387076, 1.000000000000000000, 0.8660254037844387076, 1.000000000000000000, 0.8660254037844387076, 1.000000000000000000, 0.8660254037844387076, 1.000000000000000000, 0.8660254037844387076, 1.000000000000000000, 0.8660254037844387076, 1.000000000000000000, 0.8660254037844387076, 1.000000000000000000, 0.8660254037844387076, 1.000000000000000000, 0.8660254037844387076, 1.000000000000000000, 0.8660254037844387076, 1.000000000000000000, 0.8660254037844387076, 1.000000000000000000, 0.8660254037844387076, 1.000000000000000000, 0.8660254037844387076, 1.000000000000000000),
 ( 1.000000000000000000, 0.8660254037844387076, 1.000000000000000000, 0.8660254037844387076, 1.000000000000000000, 0.8660254037844387076, 1.000000000000000000, 0.8660254037844387076, 1.000000000000000000, 0.8660254037844387076, 1.000000000000000000, 0.8660254037844387076, 1.000000000000000000, 0.8660254037844387076, 1.000000000000000000, 0.8660254037844387076, 1.000000000000000000, 0.8660254037844387076, 1.000000000000000000, 0.8660254037844387076, 1.000000000000000000, 0.8660254037844387076, 1.000000000000000000, 0.8660254037844387076, 1.000000000000000000, 0.8660254037844387076, 1.000000000000000000, 0.8660254037844387076, 1.000000000000000000, 0.8660254037844387076, 1.000000000000000000, 0.8660254037844387076, 1.000000000000000000, 0.8660254037844387076, 1.000000000000000000, 0.8660254037844387076, 1.000000000000000000, 0.8660254037844387076, 1.000000000000000000, 0.8660254037844387076, 1.000000000000000000, 0.8660254037844387076, 1.000000000000000000, 0.8660254037844387076, 1.000000000000000000, 0.8660254037844387076, 1.000000000000000000, 0.8660254037844387076, 1.000000000000000000, 0.8660254037844387076, 1.000000000000000000, 0.8660254037844387076, 1.000000000000000000, 0.8660254037844387076, 1.000000000000000000, 0.8660254037844387076, 1.000000000000000000, 0.8660254037844387076, 1.000000000000000000, 0.8660254037844387076, 1.000000000000000000, 0.8660254037844387076, 1.000000000000000000, 0.8660254037844387076, 1.000000000000000000, 0.8660254037844387076, 1.000000000000000000, 0.8660254037844387076, 1.000000000000000000, 0.8660254037844387076, 1.000000000000000000, 0.8660254037844387076, 1.000000000000000000, 0.8660254037844387076, 1.000000000000000000, 0.8660254037844387076, 1.000000000000000000, 0.8660254037844387076, 1.000000000000000000, 0.8660254037844387076, 1.000000000000000000, 0.8660254037844387076, 1.000000000000000000, 0.8660254037844387076, 1.000000000000000000, 0.8660254037844387076, 1.000000000000000000, 0.8660254037844387076, 1.000000000000000000, 0.8660254037844387076, 1.000000000000000000, 0.8660254037844387076, 1.000000000000000000, 0.8660254037844387076, 1.000000000000000000, 0.8660254037844387076, 1.000000000000000000, 0.8660254037844387076, 1.000000000000000000, 0.8660254037844387076, 1.000000000000000000, 0.8660254037844387076, 1.000000000000000000, 0.8660254037844387076, 1.000000000000000000, 0.8660254037844387076, 1.000000000000000000, 0.8660254037844387076, 1.000000000000000000, 0.8660254037844387076, 1.000000000000000000, 0.8660254037844387076, 1.000000000000000000, 0.8660254037844387076, 1.000000000000000000, 0.8660254037844387076, 1.000000000000000000, 0.8660254037844387076, 1.000000000000000000, 0.8660254037844387076, 1.000000000000000000, 0.8660254037844387076, 1.000000000000000000, 0.8660254037844387076, 1.000000000000000000, 0.8660254037844387076, 1.000000000000000000, 0.8660254037844387076, 1.000000000000000000, 0.8660254037844387076, 1.000000000000000000, 0.8660254037844387076, 1.000000000000000000, 0.8660254037844387076, 1.000000000000000000, 0.8660254037844387076, 1.000000000000000000, 0.8660254037844387076, 1.000000000000000000, 0.8660254037844387076, 1.000000000000000000, 0.8660254037844387076, 1.000000000000000000, 0.8660254037844387076, 1.000000000000000000, 0.8660254037844387076, 1.000000000000000000, 0.8660254037844387076, 1.000000000000000000, 0.8660254037844387076, 1.000000000000000000, 0.8660254037844387076, 1.000000000000000000, 0.8660254037844387076, 1.000000000000000000, 0.8660254037844387076, 1.000000000000000000, 0.8660254037844387076, 1.000000000000000000, 0.8660254037844387076, 1.000000000000000000, 0.8660254037844387076, 1.000000000000000000, 0.8660254037844387076, 1.000000000000000000, 0.8660254037844387076, 1.000000000000000000, 0.8660254037844387076, 1.000000000000000000, 0.8660254037844387076, 1.000000000000000000, 0.8660254037844387076, 1.000000000000000000, 0.8660254037844387076, 1.000000000000000000, 0.8660254037844387076, 1.000000000000000000, 0.8660254037844387076, 1.000000000000000000, 0.8660254037844387076, 1.000000000000000000, 0.8660254037844387076, 1.000000000000000000, 0.8660254037844387076, 1.000000000000000000, 0.8660254037844387076, 1.000000000000000000, 0.8660254037844387076, 1.000000000000000000, 0.8660254037844387076, 1.000000000000000000, 0.8660254037844387076, 1.000000000000000000, 0.8660254037844387076, 1.000000000000000000, 0.8660254037844387076, 1.000000000000000000, 0.8660254037844387076, 1.000000000000000000, 0.8660254037844387076, 1.000000000000000000, 0.8660254037844387076, 1.000000000000000000, 0.8660254037844387076, 1.000000000000000000, 0.8660254037844387076, 1.000000000000000000, 0.8660254037844387076, 1.000000000000000000, 0.8660254037844387076, 1.000000000000000000, 0.8660254037844387076, 1.000000000000000000, 0.8660254037844387076, 1.000000000000000000, 0.8660254037844387076, 1.000000000000000000, 0.8660254037844387076, 1.000000000000000000, 0.8660254037844387076, 1.000000000000000000, 0.8660254037844387076, 1.000000000000000000, 0.8660254037844387076, 1.000000000000000000, 0.8660254037844387076, 1.000000000000000000, 0.8660254037844387076, 1.000000000000000000, 0.8660254037844387076, 1.000000000000000000, 0.8660254037844387076, 1.000000000000000000, 0.8660254037844387076, 1.000000000000000000, 0.8660254037844387076, 1.000000000000000000, 0.8660254037844387076, 1.000000000000000000, 0.8660254037844387076, 1.000000000000000000, 0.8660254037844387076, 1.000000000000000000, 0.8660254037844387076, 1.000000000000000000, 0.8660254037844387076, 1.000000000000000000, 0.8660254037844387076, 1.000000000000000000, 0.8660254037844387076, 1.000000000000000000, 0.8660254037844387076, 1.000000000000000000, 0.8660254037844387076, 1.000000000000000000, 0.8660254037844387076, 1.000000000000000000, 0.8660254037844387076, 1.000000000000000000, 0.8660254037844387076, 1.000000000000000000, 0.8660254037844387076, 1.000000000000000000, 0.8660254037844387076, 1.000000000000000000, 0.8660254037844387076, 1.000000000000000000, 0.8660254037844387076, 1.000000000000000000, 0.8660254037844387076, 1.000000000000000000, 0.8660254037844387076, 1.000000000000000000, 0.8660254037844387076, 1.000000000000000000, 0.8660254037844387076, 1.000000000000000000, 0.8660254037844387076, 1.000000000000000000, 0.8660254037844387076, 1.000000000000000000, 0.8660254037844387076, 1.000000000000000000, 0.8660254037844387076, 1.000000000000000000, 0.8660254037844387076, 1.000000000000000000, 0.8660254037844387076, 1.000000000000000000, 0.8660254037844387076, 1.000000000000000000, 0.8660254037844387076, 1.000000000000000000, 0.8660254037844387076, 1.000000000000000000, 0.8660254037844387076, 1.000000000000000000, 0.8660254037844387076, 1.000000000000000000, 0.8660254037844387076, 1.000000000000000000, 0.8660254037844387076, 1.000000000000000000, 0.8660254037844387076, 1.000000000000000000, 0.8660254037844387076, 1.000000000000000000, 0.8660254037844387076, 1.000000000000000000, 0.8660254037844387076, 1.000000000000000000, 0.8660254037844387076, 1.000000000000000000, 0.8660254037844387076, 1.000000000000000000, 0.8660254037844387076, 1.000000000000000000, 0.8660254037844387076, 1.000000000000000000, 0.8660254037844387076, 1.000000000000000000, 0.8660254037844387076, 1.000000000000000000, 0.8660254037844387076, 1.000000000000000000, 0.8660254037844387076, 1.000000000000000000, 0.8660254037844387076, 1.000000000000000000, 0.8660254037844387076, 1.000000000000000000, 0.8660254037844387076, 1.000000000000000000, 0.8660254037844387076, 1.000000000000000000, 0.8660254037844387076, 1.000000000000000000) ) ) 
 REPRESENTATION_ITEM ( '' )  SURFACE ( )  );
#211188 = CARTESIAN_POINT ( 'NONE',  ( 5.356112940025661295, 0.8138243144468767509, -1.841424879227879119 ) ) ;
#211189 = CARTESIAN_POINT ( 'NONE',  ( 6.551614543901692400, 8.666636272683888365, 1.599625672291281386 ) ) ;
#211190 = CARTESIAN_POINT ( 'NONE',  ( 4.647555896809190124, -1.626162052001564717, -1.338137134695188468 ) ) ;
#211191 = CARTESIAN_POINT ( 'NONE',  ( 1.651812010259229968, 0.9862763539280462455, 1.642055979085883299 ) ) ;
#211192 = CARTESIAN_POINT ( 'NONE',  ( 4.708759422647839976, 4.387974169377582001, -0.7998128361456211532 ) ) ;
#211193 = CARTESIAN_POINT ( 'NONE',  ( 2.629305401816001808, 0.09940027615944720119, -1.967183499748959452 ) ) ;
#211194 = CARTESIAN_POINT ( 'NONE',  ( 5.045178214694073127, 0.1526089617210572014, 2.014106518579480642 ) ) ;
#211195 = CARTESIAN_POINT ( 'NONE',  ( 1.569004590881704075, 0.1408476687595125731, -1.865417194689425795 ) ) ;
#211196 = CARTESIAN_POINT ( 'NONE',  ( 1.978885927095444863, 1.829411362569667743, 0.7090815385668995940 ) ) ;
#211199 = VERTEX_POINT ( 'NONE', #58399 ) ;
#211198 = CARTESIAN_POINT ( 'NONE',  ( 1.212987991671743204, 1.561712320281399835, -1.103468303573502673 ) ) ;
#211197 = CARTESIAN_POINT ( 'NONE',  ( 4.828557952505812878, 1.651878126777156730, 0.4964739870837226454 ) ) ;
#211201 = CARTESIAN_POINT ( 'NONE',  ( 6.331294547901813452, 6.488857848747989543, 1.040834085586084257E-14 ) ) ;
#211200 = CARTESIAN_POINT ( 'NONE',  ( 1.172829962703396456, -1.397616723802884708, 1.707921395779465890 ) ) ;
#211202 = AXIS2_PLACEMENT_3D ( 'NONE', #66377, #101034, #36034 ) ;
#211203 = CARTESIAN_POINT ( 'NONE',  ( 0.6823417656249882723, 1.988541667008083991, -1.181850606188749264 ) ) ;
#211204 = CARTESIAN_POINT ( 'NONE',  ( 9.264299036839600987, 9.702770385934682551, -0.7998128361456281477 ) ) ;
#211205 = CARTESIAN_POINT ( 'NONE',  ( 6.789956943122251509, -0.7972922127613899512, 1.690610701080223821 ) ) ;
#211206 = CARTESIAN_POINT ( 'NONE',  ( -0.1021852871783679312, 7.053056311350174745, -4.037408415133499240 ) ) ;
#211207 = CARTESIAN_POINT ( 'NONE',  ( -5.607353961982827428, 5.583904275368083425, -0.3699160404166280114 ) ) ;
#211208 = CARTESIAN_POINT ( 'NONE',  ( 6.948098034395241207, -0.8905871627266357393, 1.867117781285509537 ) ) ;
#211209 = CARTESIAN_POINT ( 'NONE',  ( 0.7134375191242479097, -1.748147108003229810, -1.108949491591210146 ) ) ;
#211210 = CARTESIAN_POINT ( 'NONE',  ( 1.499999999999987121, 1.795833333333355819, -0.8660254037844253849 ) ) ;
#211211 = CARTESIAN_POINT ( 'NONE',  ( 6.972971076130050072, 7.029554431773520129, 1.040834085586084257E-14 ) ) ;
#211212 = CARTESIAN_POINT ( 'NONE',  ( -7.901704598666176693, 8.113076874732334076, 0.7998128361456602331 ) ) ;
#211213 = CARTESIAN_POINT ( 'NONE',  ( 4.908934136599710563, 7.884784371745123366, 1.199719254218451159 ) ) ;
#211214 = CARTESIAN_POINT ( 'NONE',  ( 4.899148033862871898, -0.2601683324335196668, -2.104413843559429065 ) ) ;
#211215 = CARTESIAN_POINT ( 'NONE',  ( 4.543917759235442944, 5.330267469643351852, 1.199719254218452935 ) ) ;
#211216 = CARTESIAN_POINT ( 'NONE',  ( -1.364683531250012516, 2.238541667008087988, -0.7879004041258289570 ) ) ;
#211218 = EDGE_CURVE ( 'NONE', #106229, #90065, #85874, .T. ) ;
#211217 = CARTESIAN_POINT ( 'NONE',  ( -0.7500000000000215383, 3.441666666666689967, 1.299038105676671107 ) ) ;
#211220 = CARTESIAN_POINT ( 'NONE',  ( 9.951321562750607086, 11.67259191370631477, -1.082531754730537088 ) ) ;
#211219 = CARTESIAN_POINT ( 'NONE',  ( 6.303176765056641706, -1.658072099422291057, 1.048360225930293321 ) ) ;
#211221 = CARTESIAN_POINT ( 'NONE',  ( 4.200545946899570282, -1.388273439763810790, -1.462221600879671790 ) ) ;
#211222 = CARTESIAN_POINT ( 'NONE',  ( 3.907376549751972572, -1.831493090834277249, 0.5616838290606884776 ) ) ;
#211223 = CARTESIAN_POINT ( 'NONE',  ( 1.927518781310177065, -1.434474475899261581, -1.656937093973806174 ) ) ;
#211224 = CYLINDRICAL_SURFACE ( 'NONE', #177310, 6.200000000000000178 ) ;
#211225 = CARTESIAN_POINT ( 'NONE',  ( -1.402160292154681736E-14, 0.1187500006828157706, -1.732050807568870754 ) ) ;
#211226 = CARTESIAN_POINT ( 'NONE',  ( 4.816656863388896426, -0.6821788116995251006, -1.894207565886153910 ) ) ;
#211227 = CARTESIAN_POINT ( 'NONE',  ( -5.585069213825653023, 8.603332285183535433, -1.199719254218440723 ) ) ;
#211228 = CARTESIAN_POINT ( 'NONE',  ( 5.976184116172984950, -2.107040639921609504, -0.2072291863110999888 ) ) ;
#211229 = PRESENTATION_STYLE_ASSIGNMENT (( #145224 ) ) ;
#211231 = CARTESIAN_POINT ( 'NONE',  ( -6.444921918449773024, 8.612437886315108315, 1.599625672291269396 ) ) ;
#211230 = CARTESIAN_POINT ( 'NONE',  ( 3.386350598701783454, -0.4101191253191734387, -2.049945593880502681 ) ) ;
#211233 = ORIENTED_EDGE ( 'NONE', *, *, #41850, .F. ) ;
#211232 = CARTESIAN_POINT ( 'NONE',  ( 1.764246635482754622, -1.222956780391671439, 1.216502489609740723 ) ) ;
#211234 = CARTESIAN_POINT ( 'NONE',  ( 5.695592476053610298, 1.958610405324921588, -0.8133567297157192622 ) ) ;
#211235 = CARTESIAN_POINT ( 'NONE',  ( 5.392392409933256303, 7.314210449720692786, 1.599625672291267398 ) ) ;
#211236 = CARTESIAN_POINT ( 'NONE',  ( 7.547439985188200140, -6.717993526550342764, 7.827294160508124321 ) ) ;
#211237 = CARTESIAN_POINT ( 'NONE',  ( 6.725651841507260364, -7.791858861492839239, -6.710064404886719736 ) ) ;
#211238 = CARTESIAN_POINT ( 'NONE',  ( 6.765682348419287173, 7.852049813699357728, 1.199719254218462483 ) ) ;
#211239 = VERTEX_POINT ( 'NONE', #190512 ) ;
#211240 = CARTESIAN_POINT ( 'NONE',  ( -11.78331023100045627, 9.799999999999982947, 1.799999999999999600 ) ) ;
#211241 = AXIS2_PLACEMENT_3D ( 'NONE', #192435, #29963, #11563 ) ;
#211243 = CARTESIAN_POINT ( 'NONE',  ( 2.244508708441519840, 1.757319924227723762, 0.4390839574351864671 ) ) ;
#211242 = CARTESIAN_POINT ( 'NONE',  ( 5.611095471209277541, 7.639640364534566075, 1.599625672291268286 ) ) ;
#211244 = CARTESIAN_POINT ( 'NONE',  ( -6.170932472514347289, 10.35117165124207972, 0.000000000000000000 ) ) ;
#211245 = VERTEX_POINT ( 'NONE', #107212 ) ;
#211246 = CARTESIAN_POINT ( 'NONE',  ( 3.785751206713845018, 5.439795712631356750, 1.599625672291267398 ) ) ;
#211247 = ORIENTED_EDGE ( 'NONE', *, *, #191199, .T. ) ;
#211248 = CARTESIAN_POINT ( 'NONE',  ( 5.899733120602060232, 6.912052057904395141, -1.199719254218452047 ) ) ;
#211249 = CARTESIAN_POINT ( 'NONE',  ( 2.473076435208894530, -1.576862618776267100, -0.8914009245391883995 ) ) ;
#211250 = DIRECTION ( 'NONE',  ( 0.000000000000000000, -1.000000000000000000, 0.000000000000000000 ) ) ;
#211251 = CIRCLE ( 'NONE', #97185, 0.5000000000000013323 ) ;
#211252 = CARTESIAN_POINT ( 'NONE',  ( -10.94305301526627439, -8.100264386820972717, 0.2223449190352171922 ) ) ;
#211253 = CARTESIAN_POINT ( 'NONE',  ( 9.049177462117294013, 12.64479190819049670, -1.199719254218446718 ) ) ;
#211254 = CARTESIAN_POINT ( 'NONE',  ( 4.341180335511626964, 7.176948212357606494, 1.029809165597308063 ) ) ;
#211255 = ORIENTED_EDGE ( 'NONE', *, *, #134736, .F. ) ;
#211256 = CARTESIAN_POINT ( 'NONE',  ( 4.211269073929763351, -1.546465011353677532, -1.035020834652039090 ) ) ;
#211257 = CARTESIAN_POINT ( 'NONE',  ( 2.038566206862189478, -1.479296367703235360, 1.217016582141629666 ) ) ;
#211258 = CARTESIAN_POINT ( 'NONE',  ( 6.809608091213839920, -0.4246860027747687560, 1.886121680295702596 ) ) ;
#211259 = CARTESIAN_POINT ( 'NONE',  ( -3.929058411375426108, -1.000000000000000888, 0.7499999999999988898 ) ) ;
#211260 = CARTESIAN_POINT ( 'NONE',  ( 4.605417112443645600, 8.360468292628990383, 0.2083848827989076002 ) ) ;
#211261 = CARTESIAN_POINT ( 'NONE',  ( 7.084367489069545069E-14, 8.210952333604106812, 2.038660652713624177 ) ) ;
#211262 = CARTESIAN_POINT ( 'NONE',  ( -2.819732761962335577, 5.273143408055916304, -1.082531754730543971 ) ) ;
#211263 = CARTESIAN_POINT ( 'NONE',  ( 8.487040972474689582, 9.964264558384387627, -1.082531754730543083 ) ) ;
#211264 = CARTESIAN_POINT ( 'NONE',  ( 4.311352223092364433, -1.634989290354519342, -1.097634987119990191 ) ) ;
#211265 = EDGE_CURVE ( 'NONE', #21086, #183752, #206929, .T. ) ;
#211266 = CARTESIAN_POINT ( 'NONE',  ( -5.915435094264120508, 5.795762452929912101, 0.000000000000000000 ) ) ;
#211267 = CARTESIAN_POINT ( 'NONE',  ( -0.4261201057540620618, 6.933630421979442460, 3.775327195640994393 ) ) ;
#211268 = CARTESIAN_POINT ( 'NONE',  ( 0.6914939563917784637, -0.7507456521842426067, 1.951374281879012962 ) ) ;
#211269 = CARTESIAN_POINT ( 'NONE',  ( 3.125598124496329360E-16, 2.519999999999999130, 2.000000000000000000 ) ) ;
#211270 = CARTESIAN_POINT ( 'NONE',  ( 5.543948526327937998, 0.7806568236609288114, -1.761304856208524283 ) ) ;
#211271 = CARTESIAN_POINT ( 'NONE',  ( -6.018930129462987999, 9.109503353427070849, 1.199719254218452047 ) ) ;
#211272 = EDGE_CURVE ( 'NONE', #29472, #78316, #113617, .T. ) ;
#211273 = CARTESIAN_POINT ( 'NONE',  ( 1.342497868159111984, 0.3520595052693386018, 1.791136884925909056 ) ) ;
#211274 = CARTESIAN_POINT ( 'NONE',  ( 1.752831059180045115, 0.6944836804415283060, 2.094827981560241970 ) ) ;
#211275 = CARTESIAN_POINT ( 'NONE',  ( -6.269955220449294764, 6.909144929749425401, 0.7818200943594469932 ) ) ;
#211276 = CARTESIAN_POINT ( 'NONE',  ( -0.1229892814952095459, -1.709044814581164973, -0.8582256167319823881 ) ) ;
#211277 = EDGE_LOOP ( 'NONE', ( #186246, #153870, #67327, #154822 ) ) ;
#211278 = ORIENTED_EDGE ( 'NONE', *, *, #63234, .F. ) ;
#211279 = CARTESIAN_POINT ( 'NONE',  ( 0.2210688645036896216, -1.757681936009440893, -0.8888059845142733950 ) ) ;
#211280 = CARTESIAN_POINT ( 'NONE',  ( 1.206472709818911637, 1.713414686832109179, 0.9141866466196489904 ) ) ;
#211281 = CARTESIAN_POINT ( 'NONE',  ( 1.001327120302420548, 1.985796081718914419, 0.3474166314290441648 ) ) ;
#211283 = CARTESIAN_POINT ( 'NONE',  ( 5.524199568661091853, 0.9153802634506421620, 1.620121770064205213 ) ) ;
#211282 = CARTESIAN_POINT ( 'NONE',  ( -6.469175572376043348, 7.576401584974034265, 1.199719254218452047 ) ) ;
#211284 = CARTESIAN_POINT ( 'NONE',  ( 6.008198349511364000, 7.038594824965278995, 1.199719254218453823 ) ) ;
#211285 = DIRECTION ( 'NONE',  ( 0.000000000000000000, 0.000000000000000000, -1.000000000000000000 ) ) ;
#211286 = CARTESIAN_POINT ( 'NONE',  ( 6.509000000000039421, 2.968845098214094147, 2.453284407971462411 ) ) ;
#211287 = CARTESIAN_POINT ( 'NONE',  ( -5.742041750587549842, 6.657802449562273850, 1.199719254218450271 ) ) ;
#211288 = CARTESIAN_POINT ( 'NONE',  ( -7.747558435566414659, 8.003516027774422170, -0.7998128361456362523 ) ) ;
#211289 = CARTESIAN_POINT ( 'NONE',  ( 1.786939262935317130, 1.904797134731281538, -1.083727916527020607 ) ) ;
#211290 = CARTESIAN_POINT ( 'NONE',  ( 3.212919216758630014, 6.692230152952963529, 0.000000000000000000 ) ) ;
#211291 = FACE_OUTER_BOUND ( 'NONE', #74415, .T. ) ;
#211292 = CARTESIAN_POINT ( 'NONE',  ( 4.042376459914751585, 3.868111981006289835, -2.500000000000000444 ) ) ;
#211293 = CARTESIAN_POINT ( 'NONE',  ( 1.594096589105632011, -1.816728215151931058, -0.1805768397986490248 ) ) ;
#211294 = CARTESIAN_POINT ( 'NONE',  ( -2.435661151949389147, 5.993355110582911038, 0.7998128361456341429 ) ) ;
#211296 = EDGE_CURVE ( 'NONE', #80951, #22839, #210576, .T. ) ;
#211295 = CARTESIAN_POINT ( 'NONE',  ( -5.251085567194491155, 5.020688004682002159, -0.7998128361456221525 ) ) ;
#211297 = CARTESIAN_POINT ( 'NONE',  ( -6.087900257701670981, 7.118292344597175081, -1.149031449265491167 ) ) ;
#211298 = CARTESIAN_POINT ( 'NONE',  ( 6.609000000000038177, 2.443064466336189788, 2.382833824652215160 ) ) ;
#211299 = CARTESIAN_POINT ( 'NONE',  ( 9.673906298550626559, 11.24497775551929557, 1.199719254218452047 ) ) ;
#211300 = CARTESIAN_POINT ( 'NONE',  ( 1.154767827468632824, -1.519305277103833118, 1.184426060187010465 ) ) ;
#211301 = CARTESIAN_POINT ( 'NONE',  ( 5.858247074779933783, -1.961936380223072263, -0.003592477671530979431 ) ) ;
#211302 = CARTESIAN_POINT ( 'NONE',  ( -7.340850106795412167, 10.65174332698158643, 1.199719254218453823 ) ) ;
#211303 = CARTESIAN_POINT ( 'NONE',  ( 6.094553744542824170, 7.069066442510145265, 1.199719254218462483 ) ) ;
#211304 = CARTESIAN_POINT ( 'NONE',  ( 5.355090213057959403, 0.4282289882464126451, -2.149144931432686256 ) ) ;
#211305 = AXIS2_PLACEMENT_3D ( 'NONE', #175668, #62959, #158351 ) ;
#211306 = CARTESIAN_POINT ( 'NONE',  ( 3.714044015139744914, 6.420469553383295391, 1.199719254218462483 ) ) ;
#211307 = CARTESIAN_POINT ( 'NONE',  ( 3.819242646454374057, -1.823515126939363462, -0.9802443236400715243 ) ) ;
#211309 = CARTESIAN_POINT ( 'NONE',  ( 1.364683531249988535, 1.676041667008085101, 0.7879004041258500513 ) ) ;
#211308 = CARTESIAN_POINT ( 'NONE',  ( 8.576050019794697832, 13.83380793569078016, 8.329213815152254341 ) ) ;
#211310 = EDGE_LOOP ( 'NONE', ( #94842, #123676, #113062, #64238 ) ) ;
#211311 = CARTESIAN_POINT ( 'NONE',  ( 3.991116696687820209, -2.292486273863734603, 0.1698809440028921647 ) ) ;
#211313 = VERTEX_POINT ( 'NONE', #6422 ) ;
#211312 = CARTESIAN_POINT ( 'NONE',  ( 6.643132081016105417, 10.69414516125339887, 0.7216878364870438212 ) ) ;
#211315 = CARTESIAN_POINT ( 'NONE',  ( -4.067082894419624672, 6.728385229256075739, 1.082531754730560403 ) ) ;
#211314 = CARTESIAN_POINT ( 'NONE',  ( 6.211043768836181478, 7.379210830797944709, 1.082531754730549967 ) ) ;
#211316 = DIRECTION ( 'NONE',  ( 0.000000000000000000, 0.000000000000000000, -1.000000000000000000 ) ) ;
#211317 = DIRECTION ( 'NONE',  ( 1.084202172485501673E-15, -1.000000000000000000, 4.336808689942006692E-15 ) ) ;
#211318 = CARTESIAN_POINT ( 'NONE',  ( 3.714730536668510830, -0.1420231480665778423, 1.936809614188730544 ) ) ;
#211319 = ORIENTED_EDGE ( 'NONE', *, *, #82890, .F. ) ;
#211320 = CARTESIAN_POINT ( 'NONE',  ( -11.21996551234719774, 1.000000000000000888, 3.949207502427040772 ) ) ;
#211321 = CARTESIAN_POINT ( 'NONE',  ( 5.168181644781757456, 1.909928461159452251, -0.09994665148223277895 ) ) ;
#211322 = CARTESIAN_POINT ( 'NONE',  ( 6.493153095729292446, 1.497681883954028237, -0.8552637798607003461 ) ) ;
#211323 = CARTESIAN_POINT ( 'NONE',  ( 4.592982591267942283, 1.756852934926198317, 0.9896879400849432074 ) ) ;
#211324 = CARTESIAN_POINT ( 'NONE',  ( 1.499999999999993117, 11.10416666666666785, 0.8660254037844408170 ) ) ;
#211325 = CARTESIAN_POINT ( 'NONE',  ( 0.1709339574563934483, -1.438030690398562239, 1.674123062825278563 ) ) ;
#211327 = CARTESIAN_POINT ( 'NONE',  ( -4.123088112331656951, 6.864000993478624579, 1.082531754730549967 ) ) ;
#211326 = CARTESIAN_POINT ( 'NONE',  ( -3.838364070418780027, 7.492192144726518954, 0.0001517565043702621237 ) ) ;
#211329 = CARTESIAN_POINT ( 'NONE',  ( 6.749276393231373739, -1.423207027788903067, -1.051611706393209111 ) ) ;
#211328 = CARTESIAN_POINT ( 'NONE',  ( 1.271554197678253839, 1.246673013970694077, 1.678101005879296004 ) ) ;
#211330 = CARTESIAN_POINT ( 'NONE',  ( 5.274064633610318076, 1.777012466945230962, -0.9530095070046653571 ) ) ;
#211332 = CARTESIAN_POINT ( 'NONE',  ( 2.677988851928223557, -1.177355775514120850, 1.966668201240986402 ) ) ;
#211331 = CARTESIAN_POINT ( 'NONE',  ( 3.711900195091365262, 7.552577004240394132, -0.7998128361456362523 ) ) ;
#211333 = CARTESIAN_POINT ( 'NONE',  ( 0.5326489567317398421, -1.227437504408007474, -1.234024486680666000 ) ) ;
#211334 = CIRCLE ( 'NONE', #24558, 0.05000000000000002359 ) ;
#211335 = CARTESIAN_POINT ( 'NONE',  ( 2.889785579457926801, 6.440540434672812786, -0.3822207396134719715 ) ) ;
#211336 = CARTESIAN_POINT ( 'NONE',  ( 0.7547592729708142434, -1.719773315039843986, -0.2198852240756724863 ) ) ;
#211337 = CARTESIAN_POINT ( 'NONE',  ( -1.360316468749995789, 0.9218750003414100114, -6.938893903907228378E-15 ) ) ;
#211338 = CARTESIAN_POINT ( 'NONE',  ( -11.49966000274993583, 12.35767154435234083, 3.429881629452983915 ) ) ;
#211339 = CARTESIAN_POINT ( 'NONE',  ( 1.416727708472965253, 0.8794254021464522619, 1.985261695379604507 ) ) ;
#211340 = CARTESIAN_POINT ( 'NONE',  ( 2.536342520008515233, 0.6839386381054488595, 1.897109991223707937 ) ) ;
#211341 = CARTESIAN_POINT ( 'NONE',  ( 3.812500000000003109, 1.451031289061270213, 1.451031289060960905 ) ) ;
#211342 = CARTESIAN_POINT ( 'NONE',  ( 1.499999999999989120, 1.306250000682816825, 0.000000000000000000 ) ) ;
#211343 = CARTESIAN_POINT ( 'NONE',  ( 0.3406813593837527687, 0.3259726575214479394, 1.898462188649749249 ) ) ;
#211344 = CARTESIAN_POINT ( 'NONE',  ( -1.402160292154681736E-14, 13.17187500034139980, 1.575800808251682339 ) ) ;
#211345 = CARTESIAN_POINT ( 'NONE',  ( 3.850012423022421082, -1.533692773617735705, -1.607201352943017802 ) ) ;
#211346 = ORIENTED_EDGE ( 'NONE', *, *, #168152, .F. ) ;
#211347 = CARTESIAN_POINT ( 'NONE',  ( 7.015401035077338143, 6.062865449010541141, 2.437084766375292144 ) ) ;
#211348 = CARTESIAN_POINT ( 'NONE',  ( -1.500000000000001332, -0.5999999999999755529, 0.000000000000000000 ) ) ;
#211349 = CARTESIAN_POINT ( 'NONE',  ( 8.158255747121103241, 10.54105100977322174, 1.599625672291281386 ) ) ;
#211350 = CARTESIAN_POINT ( 'NONE',  ( 6.739811759324814133, 8.956476034002680109, -1.443375672974078761 ) ) ;
#211351 = CARTESIAN_POINT ( 'NONE',  ( 4.053524740805938720, 3.831459740469437936, 1.214306433183764966E-14 ) ) ;
#211352 = CARTESIAN_POINT ( 'NONE',  ( 5.495574104867783305, -1.740626723225440209, 0.008114992421901638317 ) ) ;
#211354 = CARTESIAN_POINT ( 'NONE',  ( 3.701569118832209959, -1.483977648892897960, -1.283320388228793130 ) ) ;
#211353 = CIRCLE ( 'NONE', #138723, 1.250000000000000222 ) ;
#211356 = CARTESIAN_POINT ( 'NONE',  ( -6.127922243696855453, 7.211959374810172463, 1.082531754730549967 ) ) ;
#211355 = CARTESIAN_POINT ( 'NONE',  ( 4.304877467538922531, 4.981110786005563007, 1.199719254218464037 ) ) ;
#211357 = CARTESIAN_POINT ( 'NONE',  ( -1.499708767979548218, 4.349101188573495591, -0.07854769233531130879 ) ) ;
#211358 = CARTESIAN_POINT ( 'NONE',  ( 4.095213043127944097, 1.914038588809761299, -1.205934879490217382 ) ) ;
#211359 = CARTESIAN_POINT ( 'NONE',  ( 1.680209433476518521, -1.144093268944153641, -1.716113171863597797 ) ) ;
#211360 = CARTESIAN_POINT ( 'NONE',  ( -7.314787569772770226, 8.492672571945082183, -1.199719254218452935 ) ) ;
#211361 = CARTESIAN_POINT ( 'NONE',  ( 2.536292628665572479, 1.067014414141453704, -1.995120597088717806 ) ) ;
#211362 = ORIENTED_EDGE ( 'NONE', *, *, #206094, .F. ) ;
#211363 = CARTESIAN_POINT ( 'NONE',  ( -0.7500000000000215383, 0.9729166673494854534, 1.299038105676659116 ) ) ;
#211364 = CARTESIAN_POINT ( 'NONE',  ( 3.338976900156843453, -1.651226333174139693, 0.8788041501476551165 ) ) ;
#211365 = CARTESIAN_POINT ( 'NONE',  ( 2.074501327421875096, -0.7402772072304538709, 1.568325542203717227 ) ) ;
#211366 = CARTESIAN_POINT ( 'NONE',  ( -0.09359539843449991847, -0.9867227890145138236, -2.066685918926200571 ) ) ;
#211367 = CARTESIAN_POINT ( 'NONE',  ( 6.264718444480717352, -1.637942392629457178, 1.625721277839597745 ) ) ;
#211368 = CARTESIAN_POINT ( 'NONE',  ( 4.065412822539622439, 0.2671453805177248508, -2.145074402785766665 ) ) ;
#211369 = CARTESIAN_POINT ( 'NONE',  ( 4.892492844921223494, 1.613610725055414141, -1.080192228897313145 ) ) ;
#211370 = CARTESIAN_POINT ( 'NONE',  ( -3.917943204224928699, 4.633650495426258509, -1.082531754730548412 ) ) ;
#211371 = DIRECTION ( 'NONE',  ( -1.000000000000000000, 0.000000000000000000, 0.000000000000000000 ) ) ;
#211372 = CARTESIAN_POINT ( 'NONE',  ( 4.532311885504772597, 6.983620743164907552, 1.170841521963662091 ) ) ;
#211373 = CARTESIAN_POINT ( 'NONE',  ( -0.3423093779010132898, 2.999999999999995559, 0.3423093779010045745 ) ) ;
#211374 = CARTESIAN_POINT ( 'NONE',  ( 4.936577329151614180, 4.931964103531220722, -0.7216878364870458196 ) ) ;
#211375 = CARTESIAN_POINT ( 'NONE',  ( 0.6801582343749761339, 1.973958333674710630, 1.178068619123801675 ) ) ;
#211376 = CARTESIAN_POINT ( 'NONE',  ( 6.135388727473008785, 0.6351960432287793168, 1.913804721665197883 ) ) ;
#211377 = CARTESIAN_POINT ( 'NONE',  ( -10.31505594189871111, 10.92865344183699428, -0.7998128361456291469 ) ) ;
#211378 = CARTESIAN_POINT ( 'NONE',  ( 8.446893396513862839, 9.813462703143045474, -1.199719254218445830 ) ) ;
#211379 = DIRECTION ( 'NONE',  ( 0.000000000000000000, -1.000000000000000000, 0.000000000000000000 ) ) ;
#211380 = CARTESIAN_POINT ( 'NONE',  ( 3.070728972534173096, -1.687097908962056803, -0.6982200720766564839 ) ) ;
#211381 = CARTESIAN_POINT ( 'NONE',  ( -0.1296875068448125057, 0.2507808023153486054, -1.861542470327881560 ) ) ;
#211382 = ORIENTED_EDGE ( 'NONE', *, *, #193016, .F. ) ;
#211383 = CARTESIAN_POINT ( 'NONE',  ( -3.485854892044994102, 7.080931450778859215, -0.7216878364870458196 ) ) ;
#211384 = UNCERTAINTY_MEASURE_WITH_UNIT (LENGTH_MEASURE( 1.000000000000000082E-05 ), #123553, 'distance_accuracy_value', 'NONE');
#211385 = CARTESIAN_POINT ( 'NONE',  ( 1.642778471875001811, -3.930208332855376074, 2.845375778867859751 ) ) ;
#211386 = CARTESIAN_POINT ( 'NONE',  ( -6.997979842947967377, 11.31606025008131233, -0.7998128361456291469 ) ) ;
#211387 = CARTESIAN_POINT ( 'NONE',  ( -0.1227786480478709891, -1.806133744752127068, -0.9041943026713550324 ) ) ;
#211388 = CARTESIAN_POINT ( 'NONE',  ( 0.7156801077207708417, 1.735845614737155707, 1.217653249118654468 ) ) ;
#211389 = CARTESIAN_POINT ( 'NONE',  ( -6.622231685632140596, 6.690634819517756959, 0.000000000000000000 ) ) ;
#211390 = CARTESIAN_POINT ( 'NONE',  ( 1.709564315929460232, 0.5465817987246027743, -1.778839887662834185 ) ) ;
#211391 = CARTESIAN_POINT ( 'NONE',  ( 3.571683402196252910, 6.254382171615883834, 1.199719254218462483 ) ) ;
#211392 = CARTESIAN_POINT ( 'NONE',  ( 6.403207051292992169, 1.711950105385249055, 1.147064539034772679 ) ) ;
#211393 = CARTESIAN_POINT ( 'NONE',  ( 6.012342310302175363, -1.897698807000438359, 0.6819931642896917001 ) ) ;
#211394 = ORIENTED_EDGE ( 'NONE', *, *, #79201, .T. ) ;
#211395 = VERTEX_POINT ( 'NONE', #125615 ) ;
#211396 = DIRECTION ( 'NONE',  ( 0.000000000000000000, 1.000000000000000000, 0.000000000000000000 ) ) ;
#211397 = CARTESIAN_POINT ( 'NONE',  ( -9.622536337397040285, 12.24937836509514710, 1.599625672291281386 ) ) ;
#211398 = CARTESIAN_POINT ( 'NONE',  ( 3.422296110638740174, 1.157362003623555236, -1.411967061744797691 ) ) ;
#211399 = AXIS2_PLACEMENT_3D ( 'NONE', #74762, #139785, #6532 ) ;
#211401 = CARTESIAN_POINT ( 'NONE',  ( 0.9311234436981512541, -2.903130369558482027, -3.475000000000000977 ) ) ;
#211400 = CARTESIAN_POINT ( 'NONE',  ( -5.276058054373441664, 6.184431147304315424, -1.199719254218453823 ) ) ;
#211402 = CARTESIAN_POINT ( 'NONE',  ( 6.468016842275610578, 6.857101109195174793, 0.6445861549769070775 ) ) ;
#211403 = CARTESIAN_POINT ( 'NONE',  ( 6.450546045330813882, 1.388275245401158431, 1.462219883709668045 ) ) ;
#211404 = CARTESIAN_POINT ( 'NONE',  ( 6.140549721451361798, -1.552764191669778304, 0.9890077265983505672 ) ) ;
#211405 = CARTESIAN_POINT ( 'NONE',  ( 0.07680821025391608436, 6.948789780205374633, -2.405840108717867132 ) ) ;
#211406 = CARTESIAN_POINT ( 'NONE',  ( 3.352467919438668620, 2.307868970251240714, 0.0003179301051748489328 ) ) ;
#211407 = CARTESIAN_POINT ( 'NONE',  ( 6.879836604291781121, 6.991173891287354003, -0.7998128361456341429 ) ) ;
#211408 = CARTESIAN_POINT ( 'NONE',  ( 5.993488848236776967, 1.632462841753023808, 1.416962642945495565 ) ) ;
#211409 = CARTESIAN_POINT ( 'NONE',  ( 1.399837892970667630, -0.7005499098489911258, -1.811468074468420841 ) ) ;
#211410 = ADVANCED_FACE ( 'NONE', ( #41103 ), #173234, .F. ) ;
#211411 = ORIENTED_EDGE ( 'NONE', *, *, #201770, .T. ) ;
#211412 = EDGE_CURVE ( 'NONE', #73220, #36604, #88780, .T. ) ;
#211413 = CARTESIAN_POINT ( 'NONE',  ( 4.394144163123720581, 0.1076087731387373875, 2.295966082354545801 ) ) ;
#211414 = CARTESIAN_POINT ( 'NONE',  ( 0.000000000000000000, -2.500000000000002220, 0.000000000000000000 ) ) ;
#211415 = CARTESIAN_POINT ( 'NONE',  ( -3.156015896931072540, 6.904045323053366268, 0.000000000000000000 ) ) ;
#211416 = CARTESIAN_POINT ( 'NONE',  ( 5.155093292349416600, -1.580716073637401076, -1.000049079914612449 ) ) ;
#211419 = CARTESIAN_POINT ( 'NONE',  ( -5.957882158562513908, 5.915560371269843465, -0.7998128361456362523 ) ) ;
#211418 = CARTESIAN_POINT ( 'NONE',  ( 1.499999999999987121, 0.07708333401615156955, -0.8660254037844323793 ) ) ;
#211417 = CARTESIAN_POINT ( 'NONE',  ( 1.336036003918249948, -1.064896177285217016, -1.588262137521757822 ) ) ;
#211420 = CARTESIAN_POINT ( 'NONE',  ( 3.756632125300945368, 0.7937082651479386852, 2.059386989456575279 ) ) ;
#211421 = B_SPLINE_CURVE_WITH_KNOTS ( 'NONE', 3,
 ( #60674, #190663, #144116, #74807, #30326, #157134, #8725, #206921 ),
 .UNSPECIFIED., .F., .F.,
 ( 4, 2, 2, 4 ),
 ( 0.001370800379555754591, 0.001589083288849510098, 0.001807366198143265388, 0.002243932016730776184 ),
 .UNSPECIFIED. ) ;
#211422 = CARTESIAN_POINT ( 'NONE',  ( 6.105879690743165926E-15, -11.10000000000000675, 0.2598076211376223466 ) ) ;
#211423 = CARTESIAN_POINT ( 'NONE',  ( 3.083589872104280705, 5.684939719841914929, 1.199719254218450271 ) ) ;
#211424 = CARTESIAN_POINT ( 'NONE',  ( 6.549997608733495902, 7.774656977344789333, -1.082531754730548412 ) ) ;
#211425 = CARTESIAN_POINT ( 'NONE',  ( -4.243865776277440993, 4.909930479533815451, -1.199719254218446718 ) ) ;
#211426 = CARTESIAN_POINT ( 'NONE',  ( -7.092323753280154186, 7.447001598347859463, 0.7216878364870317197 ) ) ;
#211427 = CARTESIAN_POINT ( 'NONE',  ( 1.774623370849885085, -1.870687226035630646, -0.6220538675408300300 ) ) ;
#211428 = CARTESIAN_POINT ( 'NONE',  ( 0.8159566880532771460, -0.3350741789154148553, 2.283031499596111402 ) ) ;
#211429 = CARTESIAN_POINT ( 'NONE',  ( 2.769914238037580745, -1.940913097850523128, 0.2850433363836765155 ) ) ;
#211430 = CARTESIAN_POINT ( 'NONE',  ( 5.770399673640999261, -0.9225087518928692942, -1.844811731271531086 ) ) ;
#211431 = CARTESIAN_POINT ( 'NONE',  ( 5.666945020832181434, 5.713783400500082266, 0.7216878364870317197 ) ) ;
#211432 = CARTESIAN_POINT ( 'NONE',  ( 5.825163275726873202, 6.825053905550038991, 1.199719254218452047 ) ) ;
#211433 = EDGE_LOOP ( 'NONE', ( #105980, #28786, #131803, #176786 ) ) ;
#211434 = CARTESIAN_POINT ( 'NONE',  ( -10.08065090696061716, 11.71951313199760136, -1.199719254218441611 ) ) ;
#211435 = CARTESIAN_POINT ( 'NONE',  ( 0.4499999999999677591, 3.999999999999961808, -0.8338124244296144516 ) ) ;
#211436 = CARTESIAN_POINT ( 'NONE',  ( 8.615316546479974136, 12.13862083994696839, 1.199719254218450271 ) ) ;
#211437 = CARTESIAN_POINT ( 'NONE',  ( 0.5148107762544695820, 0.8296010825015688317, 2.006500992472683098 ) ) ;
#211438 = CARTESIAN_POINT ( 'NONE',  ( -1.500000000000001110, 12.27083333333333925, 0.8660254037844418162 ) ) ;
#211439 = CARTESIAN_POINT ( 'NONE',  ( 0.000000000000000000, 6.161115872820241535, 0.000000000000000000 ) ) ;
#211440 = DIRECTION ( 'NONE',  ( 9.436895709313856232E-16, -0.8656921114426507913, -0.5005768354468325132 ) ) ;
#211441 = CARTESIAN_POINT ( 'NONE',  ( 2.618241971997347317, 1.224968108320439342, -1.413705424714882586 ) ) ;
#211442 = CARTESIAN_POINT ( 'NONE',  ( 6.503215372615936296, 1.793156143535659108, 1.206815395834538451 ) ) ;
#211443 = CARTESIAN_POINT ( 'NONE',  ( 6.727182134110231360, 6.039168392632435989, 2.405853653942995773 ) ) ;
#211444 = CARTESIAN_POINT ( 'NONE',  ( -0.6823417656250246877, -0.9489583329919115684, 1.181850606188755259 ) ) ;
#211445 = CARTESIAN_POINT ( 'NONE',  ( 2.139182944796279351, 0.001596215867826628054, 1.912461472203148771 ) ) ;
#211446 = CARTESIAN_POINT ( 'NONE',  ( 4.328786618740396719, 0.08755327933733339507, 1.767792532789840498 ) ) ;
#211447 = CARTESIAN_POINT ( 'NONE',  ( 1.945825403448407487, -1.250168254263404277, -1.447093241409423081 ) ) ;
#211448 = CARTESIAN_POINT ( 'NONE',  ( -4.042302355168801320, 7.867769847672247074, 0.7998128361456341429 ) ) ;
#211449 = CARTESIAN_POINT ( 'NONE',  ( 5.466386403393696192, -1.869944189333021090, -0.4150143681153609654 ) ) ;
#211450 = CARTESIAN_POINT ( 'NONE',  ( 1.464175926609780964E-14, -2.843749999044085097, -3.475000000000000533 ) ) ;
#211451 = CARTESIAN_POINT ( 'NONE',  ( 0.2915762745691782287, -1.893489616766583339, 0.8377075429084477332 ) ) ;
#211452 = CARTESIAN_POINT ( 'NONE',  ( -0.7499999999999972244, 5.108333333333353821, -1.299038105676652011 ) ) ;
#211453 = CARTESIAN_POINT ( 'NONE',  ( 2.303126745213024851, -0.3670769733005623814, -2.088442229865586697 ) ) ;
#211454 = CARTESIAN_POINT ( 'NONE',  ( 4.750782166719051069, -1.502237938222051650, 1.114538048626475986 ) ) ;
#211456 = ORIENTED_EDGE ( 'NONE', *, *, #39650, .T. ) ;
#211455 = CARTESIAN_POINT ( 'NONE',  ( 2.226930044512597906, -0.0006860120723567450030, 1.825872481329051222 ) ) ;
#211458 = CARTESIAN_POINT ( 'NONE',  ( 5.234661009243278151, 7.693064604033777343, 1.208367059251337361 ) ) ;
#211457 = CARTESIAN_POINT ( 'NONE',  ( 4.969440760808212509, 0.2186952961555181096, -2.196011921426939129 ) ) ;
#211459 = CARTESIAN_POINT ( 'NONE',  ( -1.364683531250010295, 5.592708333674750953, 0.7879004041258379498 ) ) ;
#211460 = CARTESIAN_POINT ( 'NONE',  ( 1.363816705371086568, -0.5030291501087379435, 2.000271598109978566 ) ) ;
#211461 = CARTESIAN_POINT ( 'NONE',  ( 6.799577732453452761, 7.891594428405881878, -1.199719254218446718 ) ) ;
#211462 = CARTESIAN_POINT ( 'NONE',  ( -7.609150525767646833, 9.900428251527500834, -1.599625672291263179 ) ) ;
#211463 = DIRECTION ( 'NONE',  ( 0.000000000000000000, -0.000000000000000000, 1.000000000000000000 ) ) ;
#211464 = CARTESIAN_POINT ( 'NONE',  ( 1.423138914311261827, 3.910616352936421958, -0.4995195405159349455 ) ) ;
#211465 = VECTOR ( 'NONE', #214051, 1000.000000000000000 ) ;
#211466 = CARTESIAN_POINT ( 'NONE',  ( 0.000000000000000000, 8.600000000000017408, 0.4000000000000045186 ) ) ;
#211467 = CARTESIAN_POINT ( 'NONE',  ( 5.936491157937257235, 8.019268665717216749, 1.599625672291268286 ) ) ;
#211468 = ORIENTED_EDGE ( 'NONE', *, *, #113810, .T. ) ;
#211469 = CARTESIAN_POINT ( 'NONE',  ( 3.982925052038261526, 1.964963782255540359, 0.6523228965355857278 ) ) ;
#211470 = CARTESIAN_POINT ( 'NONE',  ( 1.499999999999989120, 5.545833333333350268, -0.8660254037844323793 ) ) ;
#211471 = CARTESIAN_POINT ( 'NONE',  ( 2.513140823169751847, 1.929641211675875878, 0.9743453106897670413 ) ) ;
#211472 = CARTESIAN_POINT ( 'NONE',  ( -5.947459870766462764, 7.133493745255431229, -1.104964307564069603 ) ) ;
#211473 = CARTESIAN_POINT ( 'NONE',  ( 1.629563124460619239, -0.2448459300014929063, 2.004692427041386615 ) ) ;
#211474 = CARTESIAN_POINT ( 'NONE',  ( 6.720655732516647163, -0.001531948155462491612, 2.073773125298985054 ) ) ;
#211475 = ORIENTED_EDGE ( 'NONE', *, *, #191370, .T. ) ;
#211476 = ADVANCED_FACE ( 'NONE', ( #175365 ), #26947, .T. ) ;
#211478 = CARTESIAN_POINT ( 'NONE',  ( 6.453317930424781856, 10.47269531889685545, -0.7216878364870267237 ) ) ;
#211477 = CARTESIAN_POINT ( 'NONE',  ( 1.737499999999999378, -1.516666666666666163, -3.009438278150925683 ) ) ;
#211479 = CARTESIAN_POINT ( 'NONE',  ( -6.084577077482911101, 10.32070003369722144, 0.000000000000000000 ) ) ;
#211480 = CARTESIAN_POINT ( 'NONE',  ( 1.657435761918718331, 1.928256795251210631, -0.5899901959932273288 ) ) ;
#211481 = CARTESIAN_POINT ( 'NONE',  ( 6.005464345382193869, -2.175231771021503668, 0.2666438670960933344 ) ) ;
#211482 = CARTESIAN_POINT ( 'NONE',  ( -0.7499999999999972244, 4.639583334016150751, -1.299038105676652899 ) ) ;
#211483 = CARTESIAN_POINT ( 'NONE',  ( 4.904515063324526025, -1.898637117948184017, -0.2282459111111398431 ) ) ;
#211484 = CARTESIAN_POINT ( 'NONE',  ( -4.600294193738529103, 4.261431402316699035, -0.7998128361456221525 ) ) ;
#211485 = CARTESIAN_POINT ( 'NONE',  ( 7.280365300414074703, 7.596107060012304402, -0.7216878364870257245 ) ) ;
#211487 = CARTESIAN_POINT ( 'NONE',  ( 1.757435634535610136, 1.928746520693159550, -0.5880414618760835266 ) ) ;
#211486 = CARTESIAN_POINT ( 'NONE',  ( -10.10046125205659173, 10.88621900359527572, -0.7216878364870267237 ) ) ;
#211488 = CARTESIAN_POINT ( 'NONE',  ( -8.012344526598182026E-15, 12.85937500034139802, -1.575800808251669460 ) ) ;
#211489 = CARTESIAN_POINT ( 'NONE',  ( -4.492547798081878874, 6.334668079219206049, 1.599625672291263179 ) ) ;
#211490 = CARTESIAN_POINT ( 'NONE',  ( 5.719686907728898539, -1.681737053624256628, 0.3821217278023018582 ) ) ;
#211491 = CARTESIAN_POINT ( 'NONE',  ( 6.393551957296131683, 9.616838495890963401, 1.199719254218452047 ) ) ;
#211492 = CARTESIAN_POINT ( 'NONE',  ( 9.788623719386617239, 11.48277776311499387, -1.082531754730537088 ) ) ;
#211493 = VECTOR ( 'NONE', #156563, 1000.000000000000000 ) ;
#211494 = CARTESIAN_POINT ( 'NONE',  ( 0.000000000000000000, 15.44694763437329676, 0.000000000000000000 ) ) ;
#211495 = ADVANCED_FACE ( 'NONE', ( #137531 ), #92825, .T. ) ;
#211496 = CARTESIAN_POINT ( 'NONE',  ( 4.379447312414087357, 5.068108938359919158, -1.199719254218452047 ) ) ;
#211497 = CARTESIAN_POINT ( 'NONE',  ( 11.94654170777226021, 9.948256738410641731, -1.134972293687621647 ) ) ;
#211498 = ORIENTED_EDGE ( 'NONE', *, *, #12527, .T. ) ;
#211499 = CARTESIAN_POINT ( 'NONE',  ( 1.270471156847551075, -0.9273748054965322840, -1.850965650132020635 ) ) ;
#211500 = EDGE_LOOP ( 'NONE', ( #12242, #22631, #27614, #4522 ) ) ;
#211501 = CARTESIAN_POINT ( 'NONE',  ( 4.617698128633199062, -0.4785133679615029556, 1.747060762061508621 ) ) ;
#211502 = CARTESIAN_POINT ( 'NONE',  ( 5.285699784481295183, 7.260012063351913625, 1.599625672291268286 ) ) ;
#211503 = CARTESIAN_POINT ( 'NONE',  ( 6.609999999999971898, -0.005249217919313342931, 2.280159464062641472 ) ) ;
#211504 = CARTESIAN_POINT ( 'NONE',  ( 6.182253972182746971, 0.9374619682817868505, 1.549891177688822452 ) ) ;
#211505 = CARTESIAN_POINT ( 'NONE',  ( 6.061904078641523697, 7.205214525570814210, -1.082531754730548412 ) ) ;
#211506 = CARTESIAN_POINT ( 'NONE',  ( 1.715332513650478674, 0.7127186716553410850, 0.8729729531562329115 ) ) ;
#211507 = CARTESIAN_POINT ( 'NONE',  ( 3.134921595499224445, -1.932508288125428741, 1.033376004005027715 ) ) ;
#211508 = VERTEX_POINT ( 'NONE', #11762 ) ;
#211509 = AXIS2_PLACEMENT_3D ( 'NONE', #32009, #181438, #210742 ) ;
#211511 = CARTESIAN_POINT ( 'NONE',  ( 9.023114925094663619, 10.48572115315399245, 1.199719254218453823 ) ) ;
#211510 = CARTESIAN_POINT ( 'NONE',  ( 0.1507198084474276056, -0.4258245693303016610, -1.922078969575198526 ) ) ;
#211512 = CARTESIAN_POINT ( 'NONE',  ( 4.376519623831674366, -0.4236097701148673900, -1.868001571610947043 ) ) ;
#211513 = CYLINDRICAL_SURFACE ( 'NONE', #97323, 0.09999999999999971412 ) ;
#211514 = CARTESIAN_POINT ( 'NONE',  ( 0.6823417656249882723, 0.09270833367475139752, 1.181850606188755259 ) ) ;
#211515 = CARTESIAN_POINT ( 'NONE',  ( 4.012850279964918165, 7.625483060026979842, -0.7216878364870197293 ) ) ;
#211516 = EDGE_CURVE ( 'NONE', #197417, #34146, #161969, .T. ) ;
#211517 = CARTESIAN_POINT ( 'NONE',  ( -9.666600336863641729, 10.38004793587015584, 1.040834085586084257E-14 ) ) ;
#211518 = CARTESIAN_POINT ( 'NONE',  ( 1.428841412761387986, 2.083414371474631377, 0.5762002773818803991 ) ) ;
#211519 = CARTESIAN_POINT ( 'NONE',  ( -3.637330350216213759, 7.465578851886037093, -0.7998128361456481317 ) ) ;
#211520 = CARTESIAN_POINT ( 'NONE',  ( 3.542423274920540432, 7.354853930707762721, -1.734723475976807094E-15 ) ) ;
#211521 = CARTESIAN_POINT ( 'NONE',  ( 2.133574855335911291, -1.190200692204022470, -1.384352166806518625 ) ) ;
#211522 = CARTESIAN_POINT ( 'NONE',  ( -3.903858165731105778, 6.641919395739846799, 1.199719254218464037 ) ) ;
#211523 = EDGE_CURVE ( 'NONE', #139784, #79300, #189619, .T. ) ;
#211524 = CARTESIAN_POINT ( 'NONE',  ( 4.119992258926360229, -0.9384382104282267267, -1.565754920925747973 ) ) ;
#211525 = CARTESIAN_POINT ( 'NONE',  ( 8.381989347167957405, 12.99464372445137883, 8.515743443721982331 ) ) ;
#211526 = ORIENTED_EDGE ( 'NONE', *, *, #153496, .F. ) ;
#211527 = CARTESIAN_POINT ( 'NONE',  ( 4.211352281912852824, -1.636193967830642748, -1.096030559421146133 ) ) ;
#211528 = ORIENTED_EDGE ( 'NONE', *, *, #127807, .F. ) ;
#211529 = CARTESIAN_POINT ( 'NONE',  ( 4.546391927783274056, -1.557747286768229600, 1.159548114344757019 ) ) ;
#211530 = VERTEX_POINT ( 'NONE', #179615 ) ;
#211531 = CARTESIAN_POINT ( 'NONE',  ( -7.286581212701773502, 7.465709267765667789, 0.7998128361456341429 ) ) ;
#211533 = CARTESIAN_POINT ( 'NONE',  ( 5.027636390373714903, -0.3086946445357250379, 2.097867224209007730 ) ) ;
#211532 = CARTESIAN_POINT ( 'NONE',  ( 5.722423353419669567, 8.833855124701747386, 1.199719254218451159 ) ) ;
#211534 = CARTESIAN_POINT ( 'NONE',  ( -3.188928480291339795, 8.980740528189214089, -2.451733079074510879 ) ) ;
#211535 = CARTESIAN_POINT ( 'NONE',  ( 2.772007568003355793, 1.902874960710929431, -0.1895390408453850317 ) ) ;
#211536 = CARTESIAN_POINT ( 'NONE',  ( 5.071574956294766068, 6.743279210435389359, -1.418366213760638317 ) ) ;
#211537 = CARTESIAN_POINT ( 'NONE',  ( 6.983263157960370116, 2.969675876345272414, 2.399270433241917466 ) ) ;
#211538 = VERTEX_POINT ( 'NONE', #192641 ) ;
#211539 = DIRECTION ( 'NONE',  ( 0.000000000000000000, -1.000000000000000000, 0.000000000000000000 ) ) ;
#211540 = CARTESIAN_POINT ( 'NONE',  ( 5.057293878089731187, -1.725371964895198840, 1.036928162195766889 ) ) ;
#211541 = CARTESIAN_POINT ( 'NONE',  ( 1.500000000000007105, 10.64264068711930733, 1.214306433183764966E-14 ) ) ;
#211542 = CARTESIAN_POINT ( 'NONE',  ( 6.182242880246401562, -0.9723386526096773341, 1.545037271442825100 ) ) ;
#211543 = CARTESIAN_POINT ( 'NONE',  ( 0.5024991115675537801, 2.064720838319131779, 0.1538615064654233477 ) ) ;
#211544 = CARTESIAN_POINT ( 'NONE',  ( -8.026063749610061748, 9.426457798375635022, -1.082531754730543971 ) ) ;
#211545 = CARTESIAN_POINT ( 'NONE',  ( -6.605427497552981642, 6.764401258476403278, 0.1916688254133581959 ) ) ;
#211546 = CARTESIAN_POINT ( 'NONE',  ( 0.000000000000000000, -9.999999999999994671, 0.000000000000000000 ) ) ;
#211547 = CARTESIAN_POINT ( 'NONE',  ( 3.285556943750000070, -2.734374999522042771, 0.000000000000000000 ) ) ;
#211548 = CARTESIAN_POINT ( 'NONE',  ( 5.276094334012385367, 9.307193822989793475, 1.040834085586084257E-14 ) ) ;
#211549 = AXIS2_PLACEMENT_3D ( 'NONE', #35139, #199772, #68697 ) ;
#211550 = CARTESIAN_POINT ( 'NONE',  ( -5.122283107864663343, 4.870418468797203637, 0.000000000000000000 ) ) ;
#211551 = ADVANCED_FACE ( 'NONE', ( #76764, #48556 ), #195861, .F. ) ;
#211552 = CARTESIAN_POINT ( 'NONE',  ( 0.6823417656249934904, 10.50520833367472839, 1.181850606188764807 ) ) ;
#211553 = CARTESIAN_POINT ( 'NONE',  ( -5.773074481320628948, 5.629675071162500544, 0.000000000000000000 ) ) ;
#211555 = CARTESIAN_POINT ( 'NONE',  ( -3.160459205317013076, 6.701303149596211206, -0.7216878364870458196 ) ) ;
#211554 = FACE_OUTER_BOUND ( 'NONE', #64388, .T. ) ;
#211556 = CARTESIAN_POINT ( 'NONE',  ( -4.557512192488103686, 8.468847991211438497, -0.7998128361456281477 ) ) ;
#211557 = CARTESIAN_POINT ( 'NONE',  ( 1.481394567461959522, -0.05474761849930119550, 2.069712792878583230 ) ) ;
#211558 = CARTESIAN_POINT ( 'NONE',  ( 2.654045540373184409, 1.135223644230592743, 1.786994778491631797 ) ) ;
#211559 = CARTESIAN_POINT ( 'NONE',  ( 6.726816770674637347, 10.99970333242910669, -0.7998128361456291469 ) ) ;
#211560 = CARTESIAN_POINT ( 'NONE',  ( 1.499999999999990896, 3.556250000682818602, 1.214306433183764966E-14 ) ) ;
#211561 = CARTESIAN_POINT ( 'NONE',  ( 0.4265231311835169792, -1.290831556599820074, 1.487489745873808555 ) ) ;
#211563 = B_SPLINE_CURVE_WITH_KNOTS ( 'NONE', 3,
 ( #61687, #127857, #162402, #29194, #178650, #146166, #191664 ),
 .UNSPECIFIED., .F., .F.,
 ( 4, 3, 4 ),
 ( 0.000000000000000000, 3.302265273836957072E-05, 4.223967315999526832E-05 ),
 .UNSPECIFIED. ) ;
#211562 = CARTESIAN_POINT ( 'NONE',  ( 4.650497622768338779, 7.104022005431295916, 1.360104839701151480 ) ) ;
#211564 = CARTESIAN_POINT ( 'NONE',  ( 4.853455804012222430, 5.725081861844796727, 1.082531754730560403 ) ) ;
#211566 = DIRECTION ( 'NONE',  ( -0.7592566023652995710, -0.6507913734559650498, 0.000000000000000000 ) ) ;
#211565 = CARTESIAN_POINT ( 'NONE',  ( -1.737500000000000266, -2.858333333333334281, -3.009438278150923907 ) ) ;
#211567 = CARTESIAN_POINT ( 'NONE',  ( 2.273717984289443717, 1.411852697042052185, 1.805783550510152935 ) ) ;
#211568 = CARTESIAN_POINT ( 'NONE',  ( 0.2756506080626683342, 1.048234779247591453, 1.494575289200591017 ) ) ;
#211569 = CARTESIAN_POINT ( 'NONE',  ( 2.127084423382288314, 1.709874882824816478, 0.8565708355050825062 ) ) ;
#211570 = CARTESIAN_POINT ( 'NONE',  ( 7.340813827156391191, 7.528980651296110160, 0.7998128361456281477 ) ) ;
#211571 = CARTESIAN_POINT ( 'NONE',  ( 7.307481607641395094, 8.588111966078864512, -1.082531754730537976 ) ) ;
#211572 = CARTESIAN_POINT ( 'NONE',  ( 1.265886429849511163, 0.5802531365422005649, -1.927800331509860632 ) ) ;
#211573 = CARTESIAN_POINT ( 'NONE',  ( 2.676550354755039773, 1.285117694784821518, -1.482265789204496143 ) ) ;
#211574 = CARTESIAN_POINT ( 'NONE',  ( -8.109748439268576803, 12.61312361245537517, 0.7998128361456481317 ) ) ;
#211575 = CARTESIAN_POINT ( 'NONE',  ( -7.552055258011950656, 8.769484874890757453, 1.199719254218462483 ) ) ;
#211576 = CARTESIAN_POINT ( 'NONE',  ( 1.743066579297358008E-15, 0.7500000006828128063, -1.225000000000021849 ) ) ;
#211578 = CARTESIAN_POINT ( 'NONE',  ( 3.309201167148849265, -0.3463371335676104223, 1.735430568453823374 ) ) ;
#211577 = CARTESIAN_POINT ( 'NONE',  ( 4.611325087297634795, -2.050354119209703008, 0.4075000692524420876 ) ) ;
#211579 = CARTESIAN_POINT ( 'NONE',  ( -0.3282377514116611716, 0.01116455005054403302, -1.225000005378890977 ) ) ;
#211581 = CARTESIAN_POINT ( 'NONE',  ( 6.351568543859240634, 2.286598795830016684, -0.1622092447367465551 ) ) ;
#211580 = CARTESIAN_POINT ( 'NONE',  ( 1.519536625744590363, 8.761901799250125578, -2.483436355453708444 ) ) ;
#211582 = CARTESIAN_POINT ( 'NONE',  ( 3.995860056160570384, -0.5486252962480555606, -1.651658045138884257 ) ) ;
#211583 = CARTESIAN_POINT ( 'NONE',  ( 9.023114925094663619, 10.48572115315399245, 1.199719254218453823 ) ) ;
#211584 = CARTESIAN_POINT ( 'NONE',  ( -0.1104750535120025967, -0.004616138082884357029, -2.103378236956429337 ) ) ;
#211585 = CARTESIAN_POINT ( 'NONE',  ( 3.989331682606485519, 1.645927443309925353, 0.5452122354672321869 ) ) ;
#211586 = CARTESIAN_POINT ( 'NONE',  ( 4.615793470729397718, 0.4799340867196815741, -2.117318520224883205 ) ) ;
#211587 = CARTESIAN_POINT ( 'NONE',  ( 4.033714395265605823, 4.664753868353354704, -1.199719254218446718 ) ) ;
#211588 = CARTESIAN_POINT ( 'NONE',  ( 6.139861302770143858, 2.010801613648224961, -0.1531635369260639090 ) ) ;
#211589 = CARTESIAN_POINT ( 'NONE',  ( 4.718750000000002665, -0.7852924748297362978, 1.895863743164184045 ) ) ;
#211590 = CARTESIAN_POINT ( 'NONE',  ( 1.499999999999989120, 5.077083334016151639, -0.8660254037844323793 ) ) ;
#211591 = CARTESIAN_POINT ( 'NONE',  ( 3.065363963417499615, 0.2843319914107733104, -1.905185398925368423 ) ) ;
#211592 = CARTESIAN_POINT ( 'NONE',  ( -6.009258394948636914E-15, 10.21875000068279604, -1.732050807568875195 ) ) ;
#211593 = CARTESIAN_POINT ( 'NONE',  ( 0.2939904269894151323, 2.070328538627811632, -0.8053792395062376874 ) ) ;
#211594 = ORIENTED_EDGE ( 'NONE', *, *, #30633, .T. ) ;
#211595 = CARTESIAN_POINT ( 'NONE',  ( 6.883263157960364254, 6.036844454314826081, 2.541088405340941492 ) ) ;
#211596 = CARTESIAN_POINT ( 'NONE',  ( -1.499999999999997780, 3.400000000000021227, 1.214306433183764966E-14 ) ) ;
#211597 = CARTESIAN_POINT ( 'NONE',  ( 5.660692828905515839, 6.562895374266609849, -1.199719254218445830 ) ) ;
#211598 = CARTESIAN_POINT ( 'NONE',  ( 1.612303553688280600, -0.7442547213242669546, 2.093046284049724370 ) ) ;
#211599 = CARTESIAN_POINT ( 'NONE',  ( 6.566857081534598350, 1.454584517406570132, -1.316677807353151097 ) ) ;
#211600 = CARTESIAN_POINT ( 'NONE',  ( 7.971831135155394321, 8.402817200543854170, -0.7216878364870267237 ) ) ;
#211601 = CARTESIAN_POINT ( 'NONE',  ( 0.2863318758520314034, 8.150007921796387222, 2.019927845748587192 ) ) ;
#211602 = VECTOR ( 'NONE', #106779, 1000.000000000000000 ) ;
#211603 = CARTESIAN_POINT ( 'NONE',  ( 4.390861645979372341, 6.216034235099629157, -1.599625672291269396 ) ) ;
#211604 = CARTESIAN_POINT ( 'NONE',  ( -4.502716413514313842, 5.386162249589033557, -1.082531754730549967 ) ) ;
#211606 = CARTESIAN_POINT ( 'NONE',  ( 6.074688485276667826, 1.387953460639863801, -1.525998863508086778 ) ) ;
#211605 = CARTESIAN_POINT ( 'NONE',  ( 9.083072846151447166, 12.68433652289702884, 1.199719254218450271 ) ) ;
#211607 = DIRECTION ( 'NONE',  ( -0.9982742078614211811, 0.000000000000000000, 0.05872483221476467591 ) ) ;
#211608 = CARTESIAN_POINT ( 'NONE',  ( -2.903417451620861289, 6.539070793532962611, 0.7998128361456341429 ) ) ;
#211609 = CARTESIAN_POINT ( 'NONE',  ( -1.201851678989727383E-14, 5.368750000682816825, -1.732050807568863648 ) ) ;
#211610 = CARTESIAN_POINT ( 'NONE',  ( 1.364683531249988535, 1.363541667008083769, 0.7879004041258500513 ) ) ;
#211611 = CARTESIAN_POINT ( 'NONE',  ( 6.643822754079466542, 0.7155741859487285694, -1.728458771772640512 ) ) ;
#211612 = CARTESIAN_POINT ( 'NONE',  ( 5.836466137708809399, 0.4949425091341461136, -1.662031903658898413 ) ) ;
#211613 = CARTESIAN_POINT ( 'NONE',  ( 5.337372294182569199, 0.6981903941610733133, -1.594458651668466898 ) ) ;
#211614 = CARTESIAN_POINT ( 'NONE',  ( 4.684505768721569652, 5.424010470718658716, -1.199719254218452047 ) ) ;
#211615 = CARTESIAN_POINT ( 'NONE',  ( 3.035043143063915760, -2.020573557004992971, 1.082744910948540307 ) ) ;
#211616 = CARTESIAN_POINT ( 'NONE',  ( 0.6823417656249899377, 4.988541667008086655, -1.181850606188754593 ) ) ;
#211617 = CARTESIAN_POINT ( 'NONE',  ( 1.165666007907351309, -1.169451938622353859, 1.422036577929463030 ) ) ;
#211618 = CARTESIAN_POINT ( 'NONE',  ( 4.051913702378651116, 7.757429176960653372, 0.5075685776039747799 ) ) ;
#211619 = DIRECTION ( 'NONE',  ( -0.000000000000000000, 1.000000000000000000, 1.804652791718263484E-16 ) ) ;
#211620 = CARTESIAN_POINT ( 'NONE',  ( 1.957752326685862077, 1.820926393389955988, -0.1310869387763091420 ) ) ;
#211621 = EDGE_CURVE ( 'NONE', #110521, #78570, #69355, .T. ) ;
#211622 = CARTESIAN_POINT ( 'NONE',  ( 2.356092462967720458, 0.09613450340887133572, -2.014232768679749430 ) ) ;
#211623 = CARTESIAN_POINT ( 'NONE',  ( 1.535386672163775668, -1.589036399888818618, -1.509351277865833563 ) ) ;
#211624 = CARTESIAN_POINT ( 'NONE',  ( 9.664668247050562044, 13.51658191024029243, -8.185676666504042132 ) ) ;
#211625 = CARTESIAN_POINT ( 'NONE',  ( 4.049914914165038127, 0.7116930038560628224, -1.982186593211773706 ) ) ;
#211626 = CARTESIAN_POINT ( 'NONE',  ( -7.389357414647957256, 8.579670724299436557, 1.199719254218450271 ) ) ;
#211627 = CARTESIAN_POINT ( 'NONE',  ( 8.597997168627587783, 14.01909641423478092, 7.911570108784474087 ) ) ;
#211628 = CARTESIAN_POINT ( 'NONE',  ( 1.012269475826784060, 2.068064858651061932, -0.09981174449213289779 ) ) ;
#211629 = CARTESIAN_POINT ( 'NONE',  ( 4.143988507271280319, 7.986403691791820414, -0.7998128361456221525 ) ) ;
#211630 = CARTESIAN_POINT ( 'NONE',  ( -1.360316468750042862, -0.5572916663252566183, 0.7853790794158701516 ) ) ;
#211631 = CARTESIAN_POINT ( 'NONE',  ( 3.949941927655271190, -1.463281269271698770, -1.534908012577620662 ) ) ;
#211632 = CARTESIAN_POINT ( 'NONE',  ( 6.428339884752386268, 1.046657586246093175, -1.495688092090130095 ) ) ;
#211633 = ORIENTED_EDGE ( 'NONE', *, *, #202732, .T. ) ;
#211634 = CARTESIAN_POINT ( 'NONE',  ( -6.805266759416629618, 6.904175738932996964, 0.000000000000000000 ) ) ;
#211635 = CARTESIAN_POINT ( 'NONE',  ( 9.856941372335116469, 11.45851867493453291, 1.199719254218450271 ) ) ;
#211636 = CARTESIAN_POINT ( 'NONE',  ( 5.017926250389229459, 8.868348035513836436, 0.000000000000000000 ) ) ;
#211637 = CARTESIAN_POINT ( 'NONE',  ( -3.475000000000000533, -2.406249999044082877, 0.000000000000000000 ) ) ;
#211638 = CARTESIAN_POINT ( 'NONE',  ( -5.850506979496850057, 6.784345216623154151, -1.199719254218446718 ) ) ;
#211639 = CARTESIAN_POINT ( 'NONE',  ( 0.01825978460381037782, -0.5840345307000054387, 2.143236301556954881 ) ) ;
#211640 = CARTESIAN_POINT ( 'NONE',  ( 1.413257319143443658, 1.857191001717144685, 0.9929431703323916558 ) ) ;
#211642 = CARTESIAN_POINT ( 'NONE',  ( -6.493429226302317225, 6.540365283632955773, 0.7998128361456341429 ) ) ;
#211641 = AXIS2_PLACEMENT_3D ( 'NONE', #74978, #156242, #155165 ) ;
#211643 = CARTESIAN_POINT ( 'NONE',  ( 7.377608144130607393, 11.75895993479440982, -0.7998128361456291469 ) ) ;
#211644 = CARTESIAN_POINT ( 'NONE',  ( 5.436322145542998641, -1.035505548906799023, 1.546008503351968821 ) ) ;
#211645 = CARTESIAN_POINT ( 'NONE',  ( 7.914208982075123799, 10.25632978388623684, -1.599625672291262513 ) ) ;
#211646 = CARTESIAN_POINT ( 'NONE',  ( 4.890372329093504611, 4.905069069454044417, -0.7147567316251844938 ) ) ;
#211647 = CARTESIAN_POINT ( 'NONE',  ( -5.320648938720212051, 5.172121614787156929, 0.000000000000000000 ) ) ;
#211648 = CARTESIAN_POINT ( 'NONE',  ( -10.16825202056928390, 10.96530823352674133, 0.7216878364870438212 ) ) ;
#211650 = CARTESIAN_POINT ( 'NONE',  ( 1.943732651021431224, 1.350599318427040840, 1.423195245143428433 ) ) ;
#211649 = CARTESIAN_POINT ( 'NONE',  ( -5.910464900553636269, 8.982960586366182554, -1.199719254218440723 ) ) ;
#211651 = CARTESIAN_POINT ( 'NONE',  ( 0.8663662989462637132, 1.066309655776727539, 1.880320099339624296 ) ) ;
#211653 = CARTESIAN_POINT ( 'NONE',  ( -6.048854636777848626, 6.051613005247792998, 0.5441514604978964220 ) ) ;
#211652 = CARTESIAN_POINT ( 'NONE',  ( -6.448838341955544173, 7.552674816150118708, 1.199719254218452047 ) ) ;
#211654 = CARTESIAN_POINT ( 'NONE',  ( 0.6823417656249899377, 0.8427083336747520637, 1.181850606188755259 ) ) ;
#211655 = CARTESIAN_POINT ( 'NONE',  ( 3.128000772048340927, 0.2569867100842055940, -1.714543959099825710 ) ) ;
#211656 = CARTESIAN_POINT ( 'NONE',  ( 2.870765623479579531, 1.652405209062355773, -0.5463526510798635272 ) ) ;
#211657 = CARTESIAN_POINT ( 'NONE',  ( 8.107412671292047790, 8.560995659369956101, 0.7216878364870458196 ) ) ;
#211658 = CARTESIAN_POINT ( 'NONE',  ( -10.94023239993386554, 4.766145680744502400, 4.420001064107922595 ) ) ;
#211659 = CARTESIAN_POINT ( 'NONE',  ( 2.460294058246147664, 0.8780975587320086762, 1.864460488959890139 ) ) ;
#211660 = EDGE_CURVE ( 'NONE', #54687, #188383, #30160, .T. ) ;
#211661 = EDGE_CURVE ( 'NONE', #73877, #3975, #177484, .T. ) ;
#211662 = CARTESIAN_POINT ( 'NONE',  ( 0.6849224457974397717, -1.076149790962807495, -1.704679027301945649 ) ) ;
#211663 = CARTESIAN_POINT ( 'NONE',  ( 6.825078400183568483, -0.002763825414428457399, 2.044262525762724270 ) ) ;
#211664 = CARTESIAN_POINT ( 'NONE',  ( -4.228163802615396705, 6.026220084508304708, -1.599625672291271394 ) ) ;
#211665 = CARTESIAN_POINT ( 'NONE',  ( 1.446098081747126951, 1.969109070040415910, 0.09893570862591105630 ) ) ;
#211667 = CARTESIAN_POINT ( 'NONE',  ( -5.099275172515603138, 8.002885897026576600, 1.082531754730549967 ) ) ;
#211666 = CARTESIAN_POINT ( 'NONE',  ( 6.047114369478562956, 0.1942372860762129894, 1.902532258075719351 ) ) ;
#211668 = CARTESIAN_POINT ( 'NONE',  ( -6.333067150914850174, 8.481940657524365434, 1.443375672974064550 ) ) ;
#211669 = CARTESIAN_POINT ( 'NONE',  ( 7.472478939787284169, 8.746922180287201698, 1.199719254218452935 ) ) ;
#211670 = CARTESIAN_POINT ( 'NONE',  ( -7.293360289508603600, 7.473618190706972086, 0.000000000000000000 ) ) ;
#211671 = CARTESIAN_POINT ( 'NONE',  ( 0.6979228276546626253, 1.358177971483988555, 1.494960626620364552 ) ) ;
#211672 = DIRECTION ( 'NONE',  ( 5.578564026256490882E-16, 1.000000000000000000, 9.066213480720158442E-32 ) ) ;
#211673 = CARTESIAN_POINT ( 'NONE',  ( 4.682853559034357183, -2.237096095179165633, -0.5655516052204231370 ) ) ;
#211674 = CARTESIAN_POINT ( 'NONE',  ( 5.547302793442128177, 1.730978599593002043, -0.9233319674036490898 ) ) ;
#211675 = EDGE_CURVE ( 'NONE', #6901, #197417, #126679, .T. ) ;
#211676 = CARTESIAN_POINT ( 'NONE',  ( 2.043732491806522056, 1.349072470436333715, 1.424505092005624807 ) ) ;
#211677 = CARTESIAN_POINT ( 'NONE',  ( 10.40996301719436090, 11.03937836301526687, 0.000000000000000000 ) ) ;
#211678 = CARTESIAN_POINT ( 'NONE',  ( 1.628336349302412112, 1.162346226930508264, 1.455206426644558571 ) ) ;
#211679 = ORIENTED_EDGE ( 'NONE', *, *, #98746, .T. ) ;
#211680 = CARTESIAN_POINT ( 'NONE',  ( 1.429080218188124585, -1.785550482114751203, 1.137718905448012352 ) ) ;
#211682 = CARTESIAN_POINT ( 'NONE',  ( -6.832419346282942563, 10.05857410638369487, 1.199719254218453823 ) ) ;
#211681 = CARTESIAN_POINT ( 'NONE',  ( -2.462777459176719308, 6.024990802348131780, -0.7998128361456281477 ) ) ;
#211683 = CARTESIAN_POINT ( 'NONE',  ( 0.5855841007226803008, -1.826885663252286740, -0.2280376995877145263 ) ) ;
#211684 = ORIENTED_EDGE ( 'NONE', *, *, #99041, .T. ) ;
#211685 = CARTESIAN_POINT ( 'NONE',  ( 3.872083141701920805, -2.139866411213369624, 0.3658599195538684290 ) ) ;
#211686 = CARTESIAN_POINT ( 'NONE',  ( 12.00020817714739785, 7.639625205866504842, -0.2088832295647653214 ) ) ;
#211687 = CARTESIAN_POINT ( 'NONE',  ( 1.986737319265439394, -1.300789755646198476, 1.674730562594067829 ) ) ;
#211688 = CARTESIAN_POINT ( 'NONE',  ( 1.499999999999989120, 4.327083334016148086, -0.8660254037844323793 ) ) ;
#211689 = CARTESIAN_POINT ( 'NONE',  ( 7.065770611016287006, 11.39514947949436774, 1.040834085586084257E-14 ) ) ;
#211690 = CARTESIAN_POINT ( 'NONE',  ( -1.040834085586084257E-14, -9.746166700180788567, -9.579665964948867796 ) ) ;
#211691 = VERTEX_POINT ( 'NONE', #31236 ) ;
#211692 = CARTESIAN_POINT ( 'NONE',  ( 3.040362567271452487, 2.044824973086068809, 0.2555446107466197714 ) ) ;
#211694 = CARTESIAN_POINT ( 'NONE',  ( 0.4855842612344652975, -1.827229208960782447, -0.2260576252584786672 ) ) ;
#211693 = CARTESIAN_POINT ( 'NONE',  ( -8.636707547105197946, 10.03491254549959777, -1.199719254218446718 ) ) ;
#211695 = CARTESIAN_POINT ( 'NONE',  ( -1.364683531250012516, 2.988541667008091096, -0.7879004041258289570 ) ) ;
#211696 = DIRECTION ( 'NONE',  ( 0.000000000000000000, -1.000000000000000000, 0.000000000000000000 ) ) ;
#211697 = CARTESIAN_POINT ( 'NONE',  ( 1.350460993223239425, 4.246634823808397741, 0.3113056364346962757 ) ) ;
#211698 = DIRECTION ( 'NONE',  ( 0.000000000000000000, 1.000000000000000000, 0.000000000000000000 ) ) ;
#211699 = CARTESIAN_POINT ( 'NONE',  ( 2.179354884421313088, -0.1095372306593382361, -2.259850278934079970 ) ) ;
#211700 = CONICAL_SURFACE ( 'NONE', #173566, 2.000000000000000000, 0.01725463330310792257 ) ;
#211701 = CARTESIAN_POINT ( 'NONE',  ( -7.863365906246048809, 12.11775129068834289, -0.7216878364870267237 ) ) ;
#211702 = CARTESIAN_POINT ( 'NONE',  ( 2.601584773815317497, 1.283861566028346779, 1.278364218381728090 ) ) ;
#211703 = CARTESIAN_POINT ( 'NONE',  ( 1.868237732200584977, -1.879526469796377164, -0.3696609625283857614 ) ) ;
#211704 = CARTESIAN_POINT ( 'NONE',  ( 3.543477799061961253, 1.872898848466747479, -0.8826743078152868849 ) ) ;
#211705 = CARTESIAN_POINT ( 'NONE',  ( -1.201851678989727383E-14, 1.134375000341418582, 1.575800808251672791 ) ) ;
#211706 = CARTESIAN_POINT ( 'NONE',  ( 1.498834128701274748, 1.612947343535120925, -1.133365233443942355 ) ) ;
#211707 = CARTESIAN_POINT ( 'NONE',  ( 6.094356125077982078, -1.917462007409322267, -0.1864201481798656301 ) ) ;
#211708 = CARTESIAN_POINT ( 'NONE',  ( 2.852262661058731386, 0.6285613048715790185, 1.762029509812724992 ) ) ;
#211710 = CARTESIAN_POINT ( 'NONE',  ( 5.061762083669725243, 7.855803969722688684, -1.119403510469544782 ) ) ;
#211709 = CARTESIAN_POINT ( 'NONE',  ( 1.278406981455294744, 1.378070038918308038, 1.850917983980376658 ) ) ;
#211711 = CARTESIAN_POINT ( 'NONE',  ( 2.418200368955259361, 0.7924288909779563239, 1.684046449600750561 ) ) ;
#211712 = CARTESIAN_POINT ( 'NONE',  ( 1.364683531249988535, 3.113541667008083991, 0.7879004041258500513 ) ) ;
#211713 = CARTESIAN_POINT ( 'NONE',  ( 4.879373355499653897, -0.1046096447297485965, 2.060157192773376611 ) ) ;
#211714 = CARTESIAN_POINT ( 'NONE',  ( -4.415151579544611238, 8.302760609444034046, -0.7998128361456281477 ) ) ;
#211715 = CARTESIAN_POINT ( 'NONE',  ( 6.642605195691581699, 9.837124264027149678, 1.199719254218462483 ) ) ;
#211716 = CARTESIAN_POINT ( 'NONE',  ( -1.390391755498394444, 3.551399914175640937, 0.5639175007713631560 ) ) ;
#211717 = SHAPE_REPRESENTATION ( 'sphere', ( #200407 ), #27579 ) ;
#211718 = CARTESIAN_POINT ( 'NONE',  ( 6.194376850977553417, -2.095475641407635425, -0.2099330270173524471 ) ) ;
#211719 = CARTESIAN_POINT ( 'NONE',  ( -1.364683531250012516, 2.801041667008090652, -0.7879004041258289570 ) ) ;
#211720 = CARTESIAN_POINT ( 'NONE',  ( 5.501312752317829791, 1.763641270444433085, 1.249554385337699802 ) ) ;
#211721 = CARTESIAN_POINT ( 'NONE',  ( 6.076820933934619084, -1.426746821240878704, 1.429770112406039795 ) ) ;
#211722 = CARTESIAN_POINT ( 'NONE',  ( 0.6823417656249882723, -0.3239583329919110133, -1.181850606188749264 ) ) ;
#211723 = CARTESIAN_POINT ( 'NONE',  ( -5.422898255786198440, 7.349800603215774331, -1.443375672974052559 ) ) ;
#211724 = ADVANCED_FACE ( 'NONE', ( #110416 ), #129878, .F. ) ;
#211727 = CARTESIAN_POINT ( 'NONE',  ( 4.528060117284229413, 7.266191989264828344, 1.082531754730558626 ) ) ;
#211726 = CARTESIAN_POINT ( 'NONE',  ( 6.825078400183550720, 7.629137130509051623, 2.355651831298340326 ) ) ;
#211725 = CARTESIAN_POINT ( 'NONE',  ( 7.212011367826596242, 7.378711115411311638, 0.000000000000000000 ) ) ;
#211728 = CARTESIAN_POINT ( 'NONE',  ( -6.154475385960665790, 6.144919136567696505, 0.000000000000000000 ) ) ;
#211729 = CARTESIAN_POINT ( 'NONE',  ( 5.014861385384292269, 0.1531656238677771009, 2.010801456750747285 ) ) ;
#211730 = CARTESIAN_POINT ( 'NONE',  ( -6.679363233026820446, 10.94434087183997129, 0.000000000000000000 ) ) ;
#211732 = CARTESIAN_POINT ( 'NONE',  ( -7.390603132780803719, 7.794994207765291172, -0.7216878364870338292 ) ) ;
#211731 = CARTESIAN_POINT ( 'NONE',  ( -2.656508033273816238, 5.186677574539687363, -1.199719254218446718 ) ) ;
#211733 = CARTESIAN_POINT ( 'NONE',  ( -1.364683531249997417, 5.759375000341418804, 1.214306433183764966E-14 ) ) ;
#211735 = CARTESIAN_POINT ( 'NONE',  ( -8.012344526598182026E-15, 9.046875000341405126, -1.575800808251669460 ) ) ;
#211734 = CARTESIAN_POINT ( 'NONE',  ( 5.524359596833869013, 1.291058806671550485, -1.733668313432787933 ) ) ;
#211736 = DIRECTION ( 'NONE',  ( 0.000000000000000000, 0.000000000000000000, 1.000000000000000000 ) ) ;
#211737 = CARTESIAN_POINT ( 'NONE',  ( -11.68215918550372123, 7.481139959555187069, 2.549995685925019462 ) ) ;
#211739 = CARTESIAN_POINT ( 'NONE',  ( 5.589470316598125876, -0.4871849528341637425, 1.956566939648955339 ) ) ;
#211738 = CARTESIAN_POINT ( 'NONE',  ( -6.358410854684789726, 8.441231968597481483, -1.443375672974058777 ) ) ;
#211740 = CARTESIAN_POINT ( 'NONE',  ( -1.364683531250014514, -0.1572916663252435232, 0.7879004041258379498 ) ) ;
#211741 = CARTESIAN_POINT ( 'NONE',  ( 2.015808680039221201, -0.8114285025175859145, -1.522100016238505216 ) ) ;
#211742 = CARTESIAN_POINT ( 'NONE',  ( 4.386945222473598527, 7.275797305264619652, -1.199719254218452047 ) ) ;
#211743 = AXIS2_PLACEMENT_3D ( 'NONE', #203189, #116684, #199994 ) ;
#211745 = CARTESIAN_POINT ( 'NONE',  ( 7.367930134383754215, 7.560616343061329125, -0.7998128361456341429 ) ) ;
#211744 = CARTESIAN_POINT ( 'NONE',  ( 7.212574532790092974, 9.437756259720353924, -1.443375672974057666 ) ) ;
#211746 = CARTESIAN_POINT ( 'NONE',  ( -11.77162061555259243, 8.648954000449407431, -2.104286885599118140 ) ) ;
#211747 = CARTESIAN_POINT ( 'NONE',  ( 6.063714619507535097, 1.842885348237649490, -0.3194776537047139264 ) ) ;
#211748 = CARTESIAN_POINT ( 'NONE',  ( 0.5572895418005788803, -1.725428541193659182, 1.036833936551822655 ) ) ;
#211749 = CARTESIAN_POINT ( 'NONE',  ( -1.432341765625004593, 8.320312500512100584, 8.673617379884035472E-16 ) ) ;
#211750 = CARTESIAN_POINT ( 'NONE',  ( 3.171135245091468491, -2.038329301889611589, -0.8460836234857532778 ) ) ;
#211751 = CARTESIAN_POINT ( 'NONE',  ( 5.594640809421455252, 2.137687854117083841, 0.3785394800270032167 ) ) ;
#211752 = VERTEX_POINT ( 'NONE', #163369 ) ;
#211753 = CARTESIAN_POINT ( 'NONE',  ( -1.500000000000015099, -0.3708333333333105331, -0.8660254037844383745 ) ) ;
#211754 = CARTESIAN_POINT ( 'NONE',  ( 9.693716643646601128, 10.41168362711695750, 0.7216878364870438212 ) ) ;
#211756 = CARTESIAN_POINT ( 'NONE',  ( 1.722280025409760329, 1.994874335020242695, 0.2930476355553628953 ) ) ;
#211755 = CARTESIAN_POINT ( 'NONE',  ( 3.440189854244297241, -1.264556376030629981, -1.702001827410426049 ) ) ;
#211758 = ORIENTED_EDGE ( 'NONE', *, *, #118355, .T. ) ;
#211757 = CARTESIAN_POINT ( 'NONE',  ( 1.740194394521710430, 1.041001882027743353, -1.482411077883559747 ) ) ;
#211759 = CARTESIAN_POINT ( 'NONE',  ( 5.550083779947807550, 7.568460058062819407, -1.599625672291283607 ) ) ;
#211760 = CARTESIAN_POINT ( 'NONE',  ( 6.810273232766058449, 6.839740281182199233, 1.040834085586084257E-14 ) ) ;
#211761 = PRESENTATION_LAYER_ASSIGNMENT (  '', '', ( #24999 ) ) ;
#211763 = CARTESIAN_POINT ( 'NONE',  ( 1.622146050056040512, 1.895417417167859497, 0.2770879218524437415 ) ) ;
#211762 = CARTESIAN_POINT ( 'NONE',  ( -3.066115294984855133, 6.728884944124295053, 0.7998128361456341429 ) ) ;
#211764 = AXIS2_PLACEMENT_3D ( 'NONE', #99938, #83668, #79419 ) ;
#211765 = DIRECTION ( 'NONE',  ( -1.000000000000000000, 0.000000000000000000, 0.000000000000000000 ) ) ;
#211766 = CARTESIAN_POINT ( 'NONE',  ( 4.961921032477176752, 8.732732271291288484, 1.040834085586084257E-14 ) ) ;
#211767 = CARTESIAN_POINT ( 'NONE',  ( 0.6823417656249882723, -0.01145833299191073573, -1.181850606188749264 ) ) ;
#211768 = LINE ( 'NONE', #63406, #112331 ) ;
#211769 = CARTESIAN_POINT ( 'NONE',  ( -9.592557376868645846, 11.15007068022363157, -1.199719254218441611 ) ) ;
#211770 = EDGE_CURVE ( 'NONE', #193425, #173258, #54803, .T. ) ;
#211771 = CARTESIAN_POINT ( 'NONE',  ( 5.664953204072169513, -1.952404353424816774, -0.9282482345986733385 ) ) ;
#211772 = CARTESIAN_POINT ( 'NONE',  ( -5.641601317062259646, 5.754492089426966217, -0.7216878364870338292 ) ) ;
#211773 = CARTESIAN_POINT ( 'NONE',  ( 5.017926250833595780, 7.907978821730911712, -1.082531754730548412 ) ) ;
#211774 = CARTESIAN_POINT ( 'NONE',  ( 2.795306286867365486, -0.1602278063087131110, -2.114629986603839829 ) ) ;
#211776 = CARTESIAN_POINT ( 'NONE',  ( -11.79406710134376191, 4.782197168659454434, 4.941180684906744780 ) ) ;
#211775 = CARTESIAN_POINT ( 'NONE',  ( -0.1298852118743892559, 2.894271690123681573, -2.215574276383952768 ) ) ;
#211777 = CARTESIAN_POINT ( 'NONE',  ( 2.917208927397921592, -0.1969847599093167145, 1.961514860040159292 ) ) ;
#211778 = EDGE_LOOP ( 'NONE', ( #131818, #75930, #192013, #175099 ) ) ;
#211780 = EDGE_CURVE ( 'NONE', #188370, #7182, #13355, .T. ) ;
#211779 = CARTESIAN_POINT ( 'NONE',  ( -0.5000000000000143219, 3.949999999999981526, 0.4999999999999553690 ) ) ;
#211781 = CARTESIAN_POINT ( 'NONE',  ( 0.8892259839063383353, 0.1505779921940515187, 2.064926437897919964 ) ) ;
#211782 = CARTESIAN_POINT ( 'NONE',  ( 2.466655979050590197, 0.09513121245676225968, -1.939734245173969640 ) ) ;
#211783 = ORIENTED_EDGE ( 'NONE', *, *, #65745, .T. ) ;
#211784 = CARTESIAN_POINT ( 'NONE',  ( 2.292764405579248876, 5.531449493117344574, 0.4111059650438048663 ) ) ;
#211786 = CARTESIAN_POINT ( 'NONE',  ( 6.773846765317333762, -7.552951973956472997, 6.773846765317311558 ) ) ;
#211785 = CARTESIAN_POINT ( 'NONE',  ( -5.750066545971566079, 8.762142499391876171, 1.082531754730550855 ) ) ;
#211788 = CARTESIAN_POINT ( 'NONE',  ( 4.971035877704902184, 8.951292290631053916, 1.040834085586084257E-14 ) ) ;
#211787 = CARTESIAN_POINT ( 'NONE',  ( 2.800817752552913209, 1.766549217158249085, 1.117748608743725169 ) ) ;
#211789 = CARTESIAN_POINT ( 'NONE',  ( 4.055297343818931033, 6.784911763547157193, 1.082531754730549078 ) ) ;
#211791 = VERTEX_POINT ( 'NONE', #70094 ) ;
#211790 = CARTESIAN_POINT ( 'NONE',  ( 6.217437059193511750, 1.592560689453832001, 1.058264445519964125 ) ) ;
#211792 = CARTESIAN_POINT ( 'NONE',  ( 3.862124860921032354, 2.190326239153097543, -0.2693113811002012525 ) ) ;
#211793 = AXIS2_PLACEMENT_3D ( 'NONE', #2204, #132281, #98685 ) ;
#211794 = CARTESIAN_POINT ( 'NONE',  ( 2.907470687441279455, 1.863611109782586484, 1.181582751932461095 ) ) ;
#211795 = CARTESIAN_POINT ( 'NONE',  ( 8.718056468787178659, 10.12981962079525289, 1.199719254218462483 ) ) ;
#211796 = SURFACE_SIDE_STYLE ('',( #131677 ) ) ;
#211797 = CARTESIAN_POINT ( 'NONE',  ( 2.051281676579026492, -1.707476168062868060, 0.8611843332394366612 ) ) ;
#211798 =( BOUNDED_SURFACE ( )  B_SPLINE_SURFACE ( 1, 2, ( 
 ( #193695, #143937, #176400, #10671, #29077, #113591, #28005, #95162, #112516, #111458, #97289, #46400, #179594, #163346, #208866, #194763, #129855, #45339, #76742, #61571, #161211, #78871, #12798, #144994, #128784, #178530, #32272, #142864, #30140, #44274, #60496, #130903, #110395, #81017, #96228, #11741, #79944, #213130, #196896, #48535, #114654, #98339, #94102, #185968, #164404, #115706, #18124, #201140, #17056, #66857, #70071, #37601, #51729, #166536, #117851, #84213, #131942, #49581, #136184, #165461, #183843, #181696, #197953, #36522, #33326, #99408, #790, #83137, #149215, #102609, #202204, #133003, #199003, #50647, #116774, #20268, #35455, #1867, #150301, #148165, #19201, #53858, #182771, #101533, #34388, #200081, #119991, #100460, #85280, #4002, #2935, #135124, #167603, #151366, #67927, #15988, #134072, #69007, #52778, #82073, #214168, #65793, #118917, #184898, #168664, #86352, #152423, #206493, #72210, #6140, #24536, #123223, #59184, #154564, #55991, #7211, #71140, #122142, #23469, #205421, #190242, #38674, #204333, #40824, #106934, #22392, #75442, #73285, #156705, #172957, #90644, #8295, #104753, #140481, #5064, #25610, #125339, #170802, #137257, #157773, #89577, #188110, #155626, #74379, #58123, #124282, #41900, #139388, #141554, #108011, #207561, #174037, #54923, #57059, #138317, #88501, #191302, #91722, #21320, #39741, #153494, #9371, #103682, #203277, #169731, #105845, #87427, #121075, #187042, #171872, #189187, #64522, #93853, #26682, #110144, #176157, #195598, #130668, #159890, #63458, #44026, #160965, #112276, #29900, #27757, #42970, #79701, #80781, #163105, #11498, #146869, #143692, #113349, #12555, #77569, #28827, #209684, #14685, #78629, #95985, #46163, #178293, #194515, #192370, #145816, #158829, #179354, #212891, #61328, #10425, #97051, #94916, #127487, #144754, #13628, #162037, #211821, #129612, #177214, #109080, #47234, #175095, #30976, #208617, #210765, #193458, #45102, #92784, #76497, #142609, #111212, #60251, #126408, #62385, #128550, #18942, #33088, #168414, #184645, #68753, #65554 ),
 ( #35196, #36265, #99162, #199831, #166280, #115466, #148966, #165215, #49347, #16805, #82891, #539, #180408, #66605, #147916, #164163, #101270, #200882, #17869, #132751, #131700, #98112, #133818, #83953, #198754, #117596, #197705, #50403, #181458, #213933, #196656, #116521, #85027, #182512, #34142, #150043, #100211, #134875, #1614, #151115, #52527, #32026, #67674, #183587, #51472, #48297, #167355, #2682, #118662, #102343, #20011, #86097, #152171, #3740, #114408, #69815, #15749, #81833, #189994, #37343, #8033, #204075, #136993, #71952, #156449, #154306, #70881, #104495, #39478, #138062, #157521, #135921, #87159, #55727, #172696, #203020, #124027, #155365, #91459, #6950, #54662, #201941, #119731, #121882, #9116, #41644, #107758, #185709, #188928, #38414, #171610, #120810, #186787, #5878, #53596, #122968, #106673, #170538, #103417, #187852, #90380, #22123, #88235, #153230, #74124, #40565, #173784, #105577, #139129, #23204, #89318, #73031, #205157, #56799, #24274, #140219, #206239, #169478, #57865, #4800, #21062, #25359, #79455, #110955, #43783, #10177, #191051, #12303, #44849, #109896, #210511, #76251, #175908, #142361, #26428, #75191, #93599, #112032, #92538, #27499, #176962, #159643, #161789, #28578, #178035, #13380, #58936, #94667, #62147, #11241, #141303, #60002, #126155, #143432, #192118, #208370, #77319, #160709, #30722, #207313, #209428, #108824, #125093, #129368, #42716, #145572, #61073, #127232, #193202, #95738, #78384, #144504, #128306, #194268, #45914, #96805, #174849, #158578, #29652, #211570, #63204, #195346, #46979, #165771, #113095, #179100, #119205, #19496, #199305, #117075, #137547, #18433, #185191, #183074, #50951, #103975, #100755, #34686, #68235, #166837, #84507, #135410, #55218, #2158, #36815, #187338, #102897, #150596, #17354, #1104, #85571, #105053, #71435, #203565, #67163, #70364, #134369, #53072, #200373, #52021, #101828, #83436, #4293, #202500, #118146, #184131, #69298, #186263, #35754, #167896, #151661, #37898, #136478, #121363, #3233, #20560, #201432, #168956, #86643, #152710, #54151 ) ),
 .UNSPECIFIED., .F., .F., .F. ) 
 B_SPLINE_SURFACE_WITH_KNOTS ( ( 2, 2 ),
 ( 3, 2, 2, 2, 2, 2, 2, 2, 2, 2, 2, 2, 2, 2, 2, 2, 2, 2, 2, 2, 2, 2, 2, 2, 2, 2, 2, 2, 2, 2, 2, 2, 2, 2, 2, 2, 2, 2, 2, 2, 2, 2, 2, 2, 2, 2, 2, 2, 2, 2, 2, 2, 2, 2, 2, 2, 2, 2, 2, 2, 2, 2, 2, 2, 2, 2, 2, 2, 2, 2, 2, 2, 2, 2, 2, 2, 2, 2, 2, 2, 2, 2, 2, 2, 2, 2, 2, 2, 2, 2, 2, 2, 2, 2, 2, 2, 2, 2, 2, 2, 2, 2, 2, 2, 2, 2, 2, 2, 2, 2, 2, 2, 2, 2, 2, 2, 2, 2, 2, 2, 3 ),
 ( 0.000000000000000000, 1.000000000000000000 ),
 ( 0.000000000000000000, 0.008333333333333333218, 0.01666666666666666644, 0.02500000000000000139, 0.03333333333333333287, 0.04166666666666666435, 0.05000000000000000278, 0.05833333333333333426, 0.06666666666666666574, 0.07499999999999999722, 0.08333333333333332871, 0.09166666666666666019, 0.1000000000000000056, 0.1083333333333333370, 0.1166666666666666685, 0.1250000000000000000, 0.1333333333333333315, 0.1416666666666666630, 0.1499999999999999944, 0.1583333333333333259, 0.1666666666666666574, 0.1749999999999999889, 0.1833333333333333204, 0.1916666666666666796, 0.2000000000000000111, 0.2083333333333333426, 0.2166666666666666741, 0.2250000000000000056, 0.2333333333333333370, 0.2416666666666666685, 0.2500000000000000000, 0.2583333333333333592, 0.2666666666666666630, 0.2750000000000000222, 0.2833333333333333259, 0.2916666666666666852, 0.2999999999999999889, 0.3083333333333333481, 0.3166666666666666519, 0.3250000000000000111, 0.3333333333333333148, 0.3416666666666666741, 0.3499999999999999778, 0.3583333333333333370, 0.3666666666666666408, 0.3750000000000000000, 0.3833333333333333592, 0.3916666666666666630, 0.4000000000000000222, 0.4083333333333333259, 0.4166666666666666852, 0.4249999999999999889, 0.4333333333333333481, 0.4416666666666666519, 0.4500000000000000111, 0.4583333333333333148, 0.4666666666666666741, 0.4749999999999999778, 0.4833333333333333370, 0.4916666666666666408, 0.5000000000000000000, 0.5083333333333333037, 0.5166666666666667185, 0.5250000000000000222, 0.5333333333333333259, 0.5416666666666666297, 0.5500000000000000444, 0.5583333333333333481, 0.5666666666666666519, 0.5749999999999999556, 0.5833333333333333703, 0.5916666666666666741, 0.5999999999999999778, 0.6083333333333332815, 0.6166666666666666963, 0.6250000000000000000, 0.6333333333333333037, 0.6416666666666667185, 0.6500000000000000222, 0.6583333333333333259, 0.6666666666666666297, 0.6750000000000000444, 0.6833333333333333481, 0.6916666666666666519, 0.6999999999999999556, 0.7083333333333333703, 0.7166666666666666741, 0.7249999999999999778, 0.7333333333333332815, 0.7416666666666666963, 0.7500000000000000000, 0.7583333333333333037, 0.7666666666666667185, 0.7750000000000000222, 0.7833333333333333259, 0.7916666666666666297, 0.8000000000000000444, 0.8083333333333333481, 0.8166666666666666519, 0.8249999999999999556, 0.8333333333333333703, 0.8416666666666666741, 0.8499999999999999778, 0.8583333333333332815, 0.8666666666666666963, 0.8750000000000000000, 0.8833333333333333037, 0.8916666666666667185, 0.9000000000000000222, 0.9083333333333333259, 0.9166666666666666297, 0.9250000000000000444, 0.9333333333333333481, 0.9416666666666666519, 0.9499999999999999556, 0.9583333333333333703, 0.9666666666666666741, 0.9749999999999999778, 0.9833333333333332815, 0.9916666666666666963, 1.000000000000000000 ),
 .UNSPECIFIED. ) 
 GEOMETRIC_REPRESENTATION_ITEM ( )  RATIONAL_B_SPLINE_SURFACE ( (
 ( 1.000000000000000000, 0.8660254037844387076, 1.000000000000000000, 0.8660254037844387076, 1.000000000000000000, 0.8660254037844387076, 1.000000000000000000, 0.8660254037844387076, 1.000000000000000000, 0.8660254037844387076, 1.000000000000000000, 0.8660254037844387076, 1.000000000000000000, 0.8660254037844387076, 1.000000000000000000, 0.8660254037844387076, 1.000000000000000000, 0.8660254037844387076, 1.000000000000000000, 0.8660254037844387076, 1.000000000000000000, 0.8660254037844387076, 1.000000000000000000, 0.8660254037844387076, 1.000000000000000000, 0.8660254037844387076, 1.000000000000000000, 0.8660254037844387076, 1.000000000000000000, 0.8660254037844387076, 1.000000000000000000, 0.8660254037844387076, 1.000000000000000000, 0.8660254037844387076, 1.000000000000000000, 0.8660254037844387076, 1.000000000000000000, 0.8660254037844387076, 1.000000000000000000, 0.8660254037844387076, 1.000000000000000000, 0.8660254037844387076, 1.000000000000000000, 0.8660254037844387076, 1.000000000000000000, 0.8660254037844387076, 1.000000000000000000, 0.8660254037844387076, 1.000000000000000000, 0.8660254037844387076, 1.000000000000000000, 0.8660254037844387076, 1.000000000000000000, 0.8660254037844387076, 1.000000000000000000, 0.8660254037844387076, 1.000000000000000000, 0.8660254037844387076, 1.000000000000000000, 0.8660254037844387076, 1.000000000000000000, 0.8660254037844387076, 1.000000000000000000, 0.8660254037844387076, 1.000000000000000000, 0.8660254037844387076, 1.000000000000000000, 0.8660254037844387076, 1.000000000000000000, 0.8660254037844387076, 1.000000000000000000, 0.8660254037844387076, 1.000000000000000000, 0.8660254037844387076, 1.000000000000000000, 0.8660254037844387076, 1.000000000000000000, 0.8660254037844387076, 1.000000000000000000, 0.8660254037844387076, 1.000000000000000000, 0.8660254037844387076, 1.000000000000000000, 0.8660254037844387076, 1.000000000000000000, 0.8660254037844387076, 1.000000000000000000, 0.8660254037844387076, 1.000000000000000000, 0.8660254037844387076, 1.000000000000000000, 0.8660254037844387076, 1.000000000000000000, 0.8660254037844387076, 1.000000000000000000, 0.8660254037844387076, 1.000000000000000000, 0.8660254037844387076, 1.000000000000000000, 0.8660254037844387076, 1.000000000000000000, 0.8660254037844387076, 1.000000000000000000, 0.8660254037844387076, 1.000000000000000000, 0.8660254037844387076, 1.000000000000000000, 0.8660254037844387076, 1.000000000000000000, 0.8660254037844387076, 1.000000000000000000, 0.8660254037844387076, 1.000000000000000000, 0.8660254037844387076, 1.000000000000000000, 0.8660254037844387076, 1.000000000000000000, 0.8660254037844387076, 1.000000000000000000, 0.8660254037844387076, 1.000000000000000000, 0.8660254037844387076, 1.000000000000000000, 0.8660254037844387076, 1.000000000000000000, 0.8660254037844387076, 1.000000000000000000, 0.8660254037844387076, 1.000000000000000000, 0.8660254037844387076, 1.000000000000000000, 0.8660254037844387076, 1.000000000000000000, 0.8660254037844387076, 1.000000000000000000, 0.8660254037844387076, 1.000000000000000000, 0.8660254037844387076, 1.000000000000000000, 0.8660254037844387076, 1.000000000000000000, 0.8660254037844387076, 1.000000000000000000, 0.8660254037844387076, 1.000000000000000000, 0.8660254037844387076, 1.000000000000000000, 0.8660254037844387076, 1.000000000000000000, 0.8660254037844387076, 1.000000000000000000, 0.8660254037844387076, 1.000000000000000000, 0.8660254037844387076, 1.000000000000000000, 0.8660254037844387076, 1.000000000000000000, 0.8660254037844387076, 1.000000000000000000, 0.8660254037844387076, 1.000000000000000000, 0.8660254037844387076, 1.000000000000000000, 0.8660254037844387076, 1.000000000000000000, 0.8660254037844387076, 1.000000000000000000, 0.8660254037844387076, 1.000000000000000000, 0.8660254037844387076, 1.000000000000000000, 0.8660254037844387076, 1.000000000000000000, 0.8660254037844387076, 1.000000000000000000, 0.8660254037844387076, 1.000000000000000000, 0.8660254037844387076, 1.000000000000000000, 0.8660254037844387076, 1.000000000000000000, 0.8660254037844387076, 1.000000000000000000, 0.8660254037844387076, 1.000000000000000000, 0.8660254037844387076, 1.000000000000000000, 0.8660254037844387076, 1.000000000000000000, 0.8660254037844387076, 1.000000000000000000, 0.8660254037844387076, 1.000000000000000000, 0.8660254037844387076, 1.000000000000000000, 0.8660254037844387076, 1.000000000000000000, 0.8660254037844387076, 1.000000000000000000, 0.8660254037844387076, 1.000000000000000000, 0.8660254037844387076, 1.000000000000000000, 0.8660254037844387076, 1.000000000000000000, 0.8660254037844387076, 1.000000000000000000, 0.8660254037844387076, 1.000000000000000000, 0.8660254037844387076, 1.000000000000000000, 0.8660254037844387076, 1.000000000000000000, 0.8660254037844387076, 1.000000000000000000, 0.8660254037844387076, 1.000000000000000000, 0.8660254037844387076, 1.000000000000000000, 0.8660254037844387076, 1.000000000000000000, 0.8660254037844387076, 1.000000000000000000, 0.8660254037844387076, 1.000000000000000000, 0.8660254037844387076, 1.000000000000000000, 0.8660254037844387076, 1.000000000000000000, 0.8660254037844387076, 1.000000000000000000, 0.8660254037844387076, 1.000000000000000000, 0.8660254037844387076, 1.000000000000000000, 0.8660254037844387076, 1.000000000000000000, 0.8660254037844387076, 1.000000000000000000, 0.8660254037844387076, 1.000000000000000000),
 ( 1.000000000000000000, 0.8660254037844387076, 1.000000000000000000, 0.8660254037844387076, 1.000000000000000000, 0.8660254037844387076, 1.000000000000000000, 0.8660254037844387076, 1.000000000000000000, 0.8660254037844387076, 1.000000000000000000, 0.8660254037844387076, 1.000000000000000000, 0.8660254037844387076, 1.000000000000000000, 0.8660254037844387076, 1.000000000000000000, 0.8660254037844387076, 1.000000000000000000, 0.8660254037844387076, 1.000000000000000000, 0.8660254037844387076, 1.000000000000000000, 0.8660254037844387076, 1.000000000000000000, 0.8660254037844387076, 1.000000000000000000, 0.8660254037844387076, 1.000000000000000000, 0.8660254037844387076, 1.000000000000000000, 0.8660254037844387076, 1.000000000000000000, 0.8660254037844387076, 1.000000000000000000, 0.8660254037844387076, 1.000000000000000000, 0.8660254037844387076, 1.000000000000000000, 0.8660254037844387076, 1.000000000000000000, 0.8660254037844387076, 1.000000000000000000, 0.8660254037844387076, 1.000000000000000000, 0.8660254037844387076, 1.000000000000000000, 0.8660254037844387076, 1.000000000000000000, 0.8660254037844387076, 1.000000000000000000, 0.8660254037844387076, 1.000000000000000000, 0.8660254037844387076, 1.000000000000000000, 0.8660254037844387076, 1.000000000000000000, 0.8660254037844387076, 1.000000000000000000, 0.8660254037844387076, 1.000000000000000000, 0.8660254037844387076, 1.000000000000000000, 0.8660254037844387076, 1.000000000000000000, 0.8660254037844387076, 1.000000000000000000, 0.8660254037844387076, 1.000000000000000000, 0.8660254037844387076, 1.000000000000000000, 0.8660254037844387076, 1.000000000000000000, 0.8660254037844387076, 1.000000000000000000, 0.8660254037844387076, 1.000000000000000000, 0.8660254037844387076, 1.000000000000000000, 0.8660254037844387076, 1.000000000000000000, 0.8660254037844387076, 1.000000000000000000, 0.8660254037844387076, 1.000000000000000000, 0.8660254037844387076, 1.000000000000000000, 0.8660254037844387076, 1.000000000000000000, 0.8660254037844387076, 1.000000000000000000, 0.8660254037844387076, 1.000000000000000000, 0.8660254037844387076, 1.000000000000000000, 0.8660254037844387076, 1.000000000000000000, 0.8660254037844387076, 1.000000000000000000, 0.8660254037844387076, 1.000000000000000000, 0.8660254037844387076, 1.000000000000000000, 0.8660254037844387076, 1.000000000000000000, 0.8660254037844387076, 1.000000000000000000, 0.8660254037844387076, 1.000000000000000000, 0.8660254037844387076, 1.000000000000000000, 0.8660254037844387076, 1.000000000000000000, 0.8660254037844387076, 1.000000000000000000, 0.8660254037844387076, 1.000000000000000000, 0.8660254037844387076, 1.000000000000000000, 0.8660254037844387076, 1.000000000000000000, 0.8660254037844387076, 1.000000000000000000, 0.8660254037844387076, 1.000000000000000000, 0.8660254037844387076, 1.000000000000000000, 0.8660254037844387076, 1.000000000000000000, 0.8660254037844387076, 1.000000000000000000, 0.8660254037844387076, 1.000000000000000000, 0.8660254037844387076, 1.000000000000000000, 0.8660254037844387076, 1.000000000000000000, 0.8660254037844387076, 1.000000000000000000, 0.8660254037844387076, 1.000000000000000000, 0.8660254037844387076, 1.000000000000000000, 0.8660254037844387076, 1.000000000000000000, 0.8660254037844387076, 1.000000000000000000, 0.8660254037844387076, 1.000000000000000000, 0.8660254037844387076, 1.000000000000000000, 0.8660254037844387076, 1.000000000000000000, 0.8660254037844387076, 1.000000000000000000, 0.8660254037844387076, 1.000000000000000000, 0.8660254037844387076, 1.000000000000000000, 0.8660254037844387076, 1.000000000000000000, 0.8660254037844387076, 1.000000000000000000, 0.8660254037844387076, 1.000000000000000000, 0.8660254037844387076, 1.000000000000000000, 0.8660254037844387076, 1.000000000000000000, 0.8660254037844387076, 1.000000000000000000, 0.8660254037844387076, 1.000000000000000000, 0.8660254037844387076, 1.000000000000000000, 0.8660254037844387076, 1.000000000000000000, 0.8660254037844387076, 1.000000000000000000, 0.8660254037844387076, 1.000000000000000000, 0.8660254037844387076, 1.000000000000000000, 0.8660254037844387076, 1.000000000000000000, 0.8660254037844387076, 1.000000000000000000, 0.8660254037844387076, 1.000000000000000000, 0.8660254037844387076, 1.000000000000000000, 0.8660254037844387076, 1.000000000000000000, 0.8660254037844387076, 1.000000000000000000, 0.8660254037844387076, 1.000000000000000000, 0.8660254037844387076, 1.000000000000000000, 0.8660254037844387076, 1.000000000000000000, 0.8660254037844387076, 1.000000000000000000, 0.8660254037844387076, 1.000000000000000000, 0.8660254037844387076, 1.000000000000000000, 0.8660254037844387076, 1.000000000000000000, 0.8660254037844387076, 1.000000000000000000, 0.8660254037844387076, 1.000000000000000000, 0.8660254037844387076, 1.000000000000000000, 0.8660254037844387076, 1.000000000000000000, 0.8660254037844387076, 1.000000000000000000, 0.8660254037844387076, 1.000000000000000000, 0.8660254037844387076, 1.000000000000000000, 0.8660254037844387076, 1.000000000000000000, 0.8660254037844387076, 1.000000000000000000, 0.8660254037844387076, 1.000000000000000000, 0.8660254037844387076, 1.000000000000000000, 0.8660254037844387076, 1.000000000000000000, 0.8660254037844387076, 1.000000000000000000, 0.8660254037844387076, 1.000000000000000000, 0.8660254037844387076, 1.000000000000000000, 0.8660254037844387076, 1.000000000000000000) ) ) 
 REPRESENTATION_ITEM ( '' )  SURFACE ( )  );
#211799 = CARTESIAN_POINT ( 'NONE',  ( 8.211434591371064684, 12.73175745657494851, -0.7998128361456352531 ) ) ;
#211800 = CARTESIAN_POINT ( 'NONE',  ( 4.387213907293201487, 0.09840592021137170575, 2.068135374880715638 ) ) ;
#211802 = CARTESIAN_POINT ( 'NONE',  ( 2.008865009297224447, 1.601992838228694316, -1.451600824242594845 ) ) ;
#211801 = CARTESIAN_POINT ( 'NONE',  ( -2.117044542028253318, 5.621635732341564662, -0.7998128361456281477 ) ) ;
#211803 = CARTESIAN_POINT ( 'NONE',  ( 4.458633810090739225, -1.957822973221786444, -0.9849130632908836835 ) ) ;
#211804 = CARTESIAN_POINT ( 'NONE',  ( 9.103410076571945453, 12.70806329172093818, 1.199719254218450271 ) ) ;
#211805 = CARTESIAN_POINT ( 'NONE',  ( -0.006158830626143650504, 7.078243236992579845, 2.121324627965421872 ) ) ;
#211806 = CARTESIAN_POINT ( 'NONE',  ( 5.387385936583818591, 7.378645907471495846, -1.599625672291283607 ) ) ;
#211807 = CARTESIAN_POINT ( 'NONE',  ( 1.364683531250000303, 15.31770833367473017, -0.7879004041258355073 ) ) ;
#211808 = CARTESIAN_POINT ( 'NONE',  ( -5.991777542596674166, 5.955104985976372944, 0.000000000000000000 ) ) ;
#211809 = B_SPLINE_CURVE_WITH_KNOTS ( 'NONE', 3,
 ( #213996, #211889, #62454, #47301 ),
 .UNSPECIFIED., .F., .F.,
 ( 4, 4 ),
 ( 5.438330430075821877E-18, 0.0005229773533087089940 ),
 .UNSPECIFIED. ) ;
#211810 = CARTESIAN_POINT ( 'NONE',  ( -0.01695367945527340853, -2.016028864686558730, -0.04667425414178058563 ) ) ;
#211811 = EDGE_CURVE ( 'NONE', #160528, #22347, #185990, .T. ) ;
#211812 = CARTESIAN_POINT ( 'NONE',  ( -7.687109909268394325, 11.91211929421440097, 0.000000000000000000 ) ) ;
#211813 = CARTESIAN_POINT ( 'NONE',  ( 5.207906454484914072, 0.6546344234062730916, -1.964071172066352400 ) ) ;
#211814 = CARTESIAN_POINT ( 'NONE',  ( 3.615773638797363798, -1.897832126884700932, 0.3302691188315133863 ) ) ;
#211815 = CARTESIAN_POINT ( 'NONE',  ( 5.413701396201449079, -1.343708383727526101, -1.636158592728423455 ) ) ;
#211816 = CARTESIAN_POINT ( 'NONE',  ( 6.148786358997489820, 7.132337826040578754, -1.199719254218446718 ) ) ;
#211817 = DIRECTION ( 'NONE',  ( 0.000000000000000000, 0.000000000000000000, 1.000000000000000000 ) ) ;
#211818 = CARTESIAN_POINT ( 'NONE',  ( 4.539879430399799354, 1.283355579558099091, 1.494016145327778045 ) ) ;
#211819 = CARTESIAN_POINT ( 'NONE',  ( 6.017577161850602430, -1.268579900078286471, -1.909058160655076053 ) ) ;
#211820 = CARTESIAN_POINT ( 'NONE',  ( 3.598116246361187542, -1.823677485248562435, -0.08826725125678223927 ) ) ;
#211821 = CARTESIAN_POINT ( 'NONE',  ( 7.688882512725796481, 8.142986817701137525, 0.000000000000000000 ) ) ;
#211822 = CARTESIAN_POINT ( 'NONE',  ( 5.951666246274807115, 6.045958163516475636, 0.7216878364870317197 ) ) ;
#211823 = CARTESIAN_POINT ( 'NONE',  ( -5.257529707049291900, 9.355811434857983500, 0.7998128361456291469 ) ) ;
#211824 = CARTESIAN_POINT ( 'NONE',  ( 5.448397627845284141, 7.449826213943242514, 1.599625672291268286 ) ) ;
#211825 = ORIENTED_EDGE ( 'NONE', *, *, #28177, .T. ) ;
#211827 = CARTESIAN_POINT ( 'NONE',  ( 5.150644359860614863, 1.984129689857921486, 0.3399971717471597654 ) ) ;
#211826 = CARTESIAN_POINT ( 'NONE',  ( 1.030510548812729965, -1.664561007783531332, 0.7873658874757857307 ) ) ;
#211828 = CARTESIAN_POINT ( 'NONE',  ( 5.783868576693856234, 1.881360230585613413, -1.320557073901595047 ) ) ;
#211829 = CARTESIAN_POINT ( 'NONE',  ( 5.471523917629521172, -0.2915489554583711174, 1.939870717765689534 ) ) ;
#211830 = CARTESIAN_POINT ( 'NONE',  ( -7.393273838153706201, 7.519907654134449615, 0.7998128361456341429 ) ) ;
#211831 = CARTESIAN_POINT ( 'NONE',  ( -3.601662362724658895, 7.353689856487406473, -0.7998128361456281477 ) ) ;
#211832 =( NAMED_UNIT ( * ) SI_UNIT ( $, .STERADIAN. ) SOLID_ANGLE_UNIT ( ) );
#211833 = CARTESIAN_POINT ( 'NONE',  ( -3.623772196602547346, 7.449761006003425834, 0.000000000000000000 ) ) ;
#211835 = CARTESIAN_POINT ( 'NONE',  ( 0.5494049127674709432, 0.5909524230637287490, -1.774924738581270089 ) ) ;
#211834 = CARTESIAN_POINT ( 'NONE',  ( 1.892240118738715005, -0.5608018070641508368, -2.014042591102585877 ) ) ;
#211836 = FACE_OUTER_BOUND ( 'NONE', #97270, .T. ) ;
#211837 = CARTESIAN_POINT ( 'NONE',  ( -0.1102773484824301209, 0.2280386113255315761, -2.237141580442712829 ) ) ;
#211838 = CARTESIAN_POINT ( 'NONE',  ( 0.4502399561126956273, -1.468881883692290113, -0.9332017962183251081 ) ) ;
#211839 = CARTESIAN_POINT ( 'NONE',  ( 7.461064606222022277, 7.598996883547496139, 1.040834085586084257E-14 ) ) ;
#211841 = CARTESIAN_POINT ( 'NONE',  ( 1.224999999999976996, 1.666666667349515851, 0.7072540797572517413 ) ) ;
#211840 = FACE_OUTER_BOUND ( 'NONE', #62470, .T. ) ;
#211842 = CARTESIAN_POINT ( 'NONE',  ( 2.244387868473923575, 0.3767020243423558901, 1.683057829810198136 ) ) ;
#211843 = CARTESIAN_POINT ( 'NONE',  ( 2.103317784989285677, -0.4765762082987561321, 2.138964651187735821 ) ) ;
#211844 = CARTESIAN_POINT ( 'NONE',  ( -0.1347034368660744441, -0.1421164721313403212, -1.704521202080215847 ) ) ;
#211845 = CARTESIAN_POINT ( 'NONE',  ( 3.826972293661185187, 2.095320012007126476, 0.6930106488920934060 ) ) ;
#211846 = CARTESIAN_POINT ( 'NONE',  ( -9.979907920417568690, 3.147823346236176878, -6.101210848797135711 ) ) ;
#211847 = AXIS2_PLACEMENT_3D ( 'NONE', #37499, #73182, #74280 ) ;
#211848 = CARTESIAN_POINT ( 'NONE',  ( 1.797964266608031547, -1.570508639683061647, -1.499219477302183412 ) ) ;
#211849 = DIRECTION ( 'NONE',  ( -3.491481338843133750E-15, -0.000000000000000000, -1.000000000000000000 ) ) ;
#211850 = CARTESIAN_POINT ( 'NONE',  ( 2.501287867402203879, -0.2026288386562236921, 2.107594835487134777 ) ) ;
#211851 = MECHANICAL_DESIGN_GEOMETRIC_PRESENTATION_REPRESENTATION (  '', ( #80294 ), #197927 ) ;
#211852 = CARTESIAN_POINT ( 'NONE',  ( 5.463572716182826028, 5.476515711742510284, 0.7216878364870371598 ) ) ;
#211853 = ORIENTED_EDGE ( 'NONE', *, *, #136835, .F. ) ;
#211855 = CARTESIAN_POINT ( 'NONE',  ( -0.6823417656250246877, -0.6364583329919113464, 1.181850606188755259 ) ) ;
#211854 = CARTESIAN_POINT ( 'NONE',  ( 2.208868952076637804, 2.049428429192188705, 1.027153634429162743 ) ) ;
#211856 = CARTESIAN_POINT ( 'NONE',  ( -11.84101807917483740, 12.48978499739122405, -1.444039656437080099 ) ) ;
#211857 = CARTESIAN_POINT ( 'NONE',  ( 5.005985031943777308, 6.863401842066294556, -1.599625672291256295 ) ) ;
#211858 = CARTESIAN_POINT ( 'NONE',  ( 5.936230101866142306, -1.231883464771424075, -1.848230934346828391 ) ) ;
#211859 = CARTESIAN_POINT ( 'NONE',  ( -5.883875478650828050, 9.808345791827219884, 0.7216878364870458196 ) ) ;
#211860 = CARTESIAN_POINT ( 'NONE',  ( 5.233084105194869551, 6.167981546557892436, -1.082531754730548412 ) ) ;
#211861 = CARTESIAN_POINT ( 'NONE',  ( -7.687109908824056426, 8.070642436490613747, 0.7216878364870438212 ) ) ;
#211862 = CARTESIAN_POINT ( 'NONE',  ( 4.095971805104276164, 7.792734516014745871, 0.7216878364870257245 ) ) ;
#211863 = ORIENTED_EDGE ( 'NONE', *, *, #189986, .F. ) ;
#211864 = CARTESIAN_POINT ( 'NONE',  ( 3.885388821667290493, -0.6351983117205138862, -1.913803978180687482 ) ) ;
#211866 = CARTESIAN_POINT ( 'NONE',  ( 2.219651360329556233, 0.3568934070868194919, -2.031323280462021152 ) ) ;
#211865 = CARTESIAN_POINT ( 'NONE',  ( 4.611744806942754238, 8.532119374741881757, -0.7998128361456231517 ) ) ;
#211867 = CARTESIAN_POINT ( 'NONE',  ( 0.000000000000000000, 0.000000000000000000, 0.000000000000000000 ) ) ;
#211868 = CARTESIAN_POINT ( 'NONE',  ( 4.651856102820254968, 7.480896982382013505, -1.082531754730548412 ) ) ;
#211869 = EDGE_LOOP ( 'NONE', ( #43076, #173564, #67789, #85405 ) ) ;
#211870 = CARTESIAN_POINT ( 'NONE',  ( 1.364683531249990311, 4.863541667008084879, 0.7879004041258500513 ) ) ;
#211872 = CARTESIAN_POINT ( 'NONE',  ( 4.822331674454460426, 2.096538211656114647, 0.6379635903819569354 ) ) ;
#211871 = B_SPLINE_CURVE_WITH_KNOTS ( 'NONE', 3,
 ( #195311, #162820, #46942, #180125, #84746, #89037 ),
 .UNSPECIFIED., .F., .F.,
 ( 4, 2, 4 ),
 ( 0.001889712630306643456, 0.002203932548491402497, 0.002518152466676161320 ),
 .UNSPECIFIED. ) ;
#211873 = CARTESIAN_POINT ( 'NONE',  ( 2.180314765559120183, 1.560501322096979449, 1.277041908422072991 ) ) ;
#211874 = CARTESIAN_POINT ( 'NONE',  ( 2.014959344526063845, -1.785600367564584179, 0.4486904387498573676 ) ) ;
#211875 = CARTESIAN_POINT ( 'NONE',  ( 6.988338112840064120, 10.24047933403371502, 1.199719254218460707 ) ) ;
#211876 = CARTESIAN_POINT ( 'NONE',  ( 2.312500000000001776, 1.451031289061216478, 1.451031289061020857 ) ) ;
#211877 = CARTESIAN_POINT ( 'NONE',  ( 5.368107995252269227, 0.9013511576922846880, 1.587453057759043551 ) ) ;
#211878 = CARTESIAN_POINT ( 'NONE',  ( 5.608046130584797950, -0.04667949407829303371, 2.016033753796213635 ) ) ;
#211879 = CARTESIAN_POINT ( 'NONE',  ( -6.692921386640485082, 10.96015871772258521, -0.7998128361456291469 ) ) ;
#211881 = CARTESIAN_POINT ( 'NONE',  ( -6.791708605802965870, 6.888357893050385705, -0.7998128361456362523 ) ) ;
#211880 = CARTESIAN_POINT ( 'NONE',  ( 5.190393989392352303, -2.244764952986468831, -0.2824595779603657486 ) ) ;
#211882 = CARTESIAN_POINT ( 'NONE',  ( 0.8210893850928849824, 1.946682464879319729, 0.8042085006434143146 ) ) ;
#211883 = CARTESIAN_POINT ( 'NONE',  ( -7.208094944320834863, 8.438474185576302133, -1.199719254218452047 ) ) ;
#211884 = CARTESIAN_POINT ( 'NONE',  ( 9.725276259704228821, 10.24057714594344048, 0.7998128361456462443 ) ) ;
#211885 = CARTESIAN_POINT ( 'NONE',  ( 4.601997573603133773, 4.922373501976976762, -0.8019421930630143969 ) ) ;
#211886 = DIRECTION ( 'NONE',  ( -0.5855528813474317751, -0.5275537511866671414, 0.6154793763844541576 ) ) ;
#211887 = CARTESIAN_POINT ( 'NONE',  ( -6.364663046611467756, 9.512858423433634414, 1.199719254218452047 ) ) ;
#211888 = UNCERTAINTY_MEASURE_WITH_UNIT (LENGTH_MEASURE( 1.000000000000000082E-05 ), #161440, 'distance_accuracy_value', 'NONE');
#211889 = CARTESIAN_POINT ( 'NONE',  ( 3.548584350011782185, 7.336486228343999549, 0.1164461989974732298 ) ) ;
#211890 = CARTESIAN_POINT ( 'NONE',  ( 7.713663051532233972, 7.963971413067895355, -0.7998128361456341429 ) ) ;
#211891 = CARTESIAN_POINT ( 'NONE',  ( 4.708705726121224622, 6.822254573549790813, -1.234111767277449534 ) ) ;
#211892 = CARTESIAN_POINT ( 'NONE',  ( -8.012505595996376684, 12.29174759539704986, 0.000000000000000000 ) ) ;
#211894 = CARTESIAN_POINT ( 'NONE',  ( 2.303257990033405367, -0.3847559998488152000, -2.187706203110438175 ) ) ;
#211893 = CARTESIAN_POINT ( 'NONE',  ( 1.881254504445781794, -1.940830296247602949, -0.8548571619346673200 ) ) ;
#211895 = AXIS2_PLACEMENT_3D ( 'NONE', #129850, #163339, #49574 ) ;
#211896 = CARTESIAN_POINT ( 'NONE',  ( -5.608322021959554426, 5.603804175593484871, 0.4115828475494631156 ) ) ;
#211897 = CARTESIAN_POINT ( 'NONE',  ( -4.911796789900812144, 8.952456364851418158, 0.7998128361456291469 ) ) ;
#211898 = CARTESIAN_POINT ( 'NONE',  ( 4.801558957534076022, 8.753569217098425170, 0.7998128361456462443 ) ) ;
#211899 = CARTESIAN_POINT ( 'NONE',  ( 2.910546574502240968, 0.6583626327048962557, 1.848246418561696913 ) ) ;
#211900 = CARTESIAN_POINT ( 'NONE',  ( 6.257251587906815793, 7.258880593101466161, 1.199719254218462483 ) ) ;
#211901 = CARTESIAN_POINT ( 'NONE',  ( -4.145011909418054863, 7.447386798385191575, 0.7030492056920457644 ) ) ;
#211902 = CARTESIAN_POINT ( 'NONE',  ( 2.347533153460546806, 5.890539112345938300, 0.000000000000000000 ) ) ;
#211903 = CARTESIAN_POINT ( 'NONE',  ( -4.014622883422322985, 7.697827440719083647, -0.7216878364870458196 ) ) ;
#211904 = CARTESIAN_POINT ( 'NONE',  ( -7.388830529767770550, 7.722649827591604677, 1.040834085586084257E-14 ) ) ;
#211905 = CARTESIAN_POINT ( 'NONE',  ( 2.074623746436579985, 0.9110886696130392481, 1.915067268644244702 ) ) ;
#211906 = CARTESIAN_POINT ( 'NONE',  ( -4.936050443827081580, 7.916420063510339666, 1.199719254218452935 ) ) ;
#211907 = CARTESIAN_POINT ( 'NONE',  ( 4.135729569369491543, -1.488772398488470872, -1.567562023322838671 ) ) ;
#211908 = CARTESIAN_POINT ( 'NONE',  ( 2.893917256732419396, -0.5369380550670297403, -1.761199466696103499 ) ) ;
#211909 = CARTESIAN_POINT ( 'NONE',  ( -4.916288619803077964, 6.680904680207828683, 1.249144131323683515 ) ) ;
#211910 = CARTESIAN_POINT ( 'NONE',  ( 1.364683531249986537, 0.4260416670080872659, 0.7879004041258500513 ) ) ;
#211911 = CARTESIAN_POINT ( 'NONE',  ( 5.999919492459485859, -0.6329648550039753685, -1.621342527780894827 ) ) ;
#211912 = DIRECTION ( 'NONE',  ( 0.000000000000000000, -1.000000000000000000, 0.000000000000000000 ) ) ;
#211913 = CARTESIAN_POINT ( 'NONE',  ( 3.063779527008304360, 6.518233848244248563, 0.7216878364870317197 ) ) ;
#211914 = EDGE_CURVE ( 'NONE', #85368, #92250, #9180, .T. ) ;
#211916 = CARTESIAN_POINT ( 'NONE',  ( 3.256853613824191029, -1.637998819981079990, 1.410756932016984377 ) ) ;
#211915 = PRODUCT_RELATED_PRODUCT_CATEGORY ( 'part', '', ( #80054 ) ) ;
#211917 = CIRCLE ( 'NONE', #173932, 11.99999999999999112 ) ;
#211918 = CARTESIAN_POINT ( 'NONE',  ( 4.956407584168041502, 1.492027487219639514, 1.356091576722208369 ) ) ;
#211919 = CARTESIAN_POINT ( 'NONE',  ( -8.283668667825340393, 12.60810451253083997, 0.7216878364870458196 ) ) ;
#211921 = AXIS2_PLACEMENT_3D ( 'NONE', #203158, #139266, #205296 ) ;
#211920 = CARTESIAN_POINT ( 'NONE',  ( 2.096749907087645415, -0.5762017740289016032, -2.083436276955972222 ) ) ;
#211922 = CARTESIAN_POINT ( 'NONE',  ( 2.864479682042244679, -1.362014001507254379, 1.425398218059505728 ) ) ;
#211923 = DIRECTION ( 'NONE',  ( 0.000000000000000000, 1.000000000000000000, 0.000000000000000000 ) ) ;
#211924 = CARTESIAN_POINT ( 'NONE',  ( 4.159667821157567502, 0.9185609468507827113, 1.711114809252372915 ) ) ;
#211927 = ORIENTED_EDGE ( 'NONE', *, *, #148167, .T. ) ;
#211926 = CARTESIAN_POINT ( 'NONE',  ( 1.419999999999989049, 6.200000000000045475, -2.899999999999995470 ) ) ;
#211925 = CARTESIAN_POINT ( 'NONE',  ( -8.229436053370685400, 10.62409470039771442, 1.443375672974090751 ) ) ;
#211928 = CARTESIAN_POINT ( 'NONE',  ( -8.106849506328558164, 8.422688943663599659, 0.000000000000000000 ) ) ;
#211929 = CARTESIAN_POINT ( 'NONE',  ( 3.627688620108284745, 6.389997935838436227, 1.199719254218452047 ) ) ;
#211931 = ORIENTED_EDGE ( 'NONE', *, *, #147046, .F. ) ;
#211930 = CARTESIAN_POINT ( 'NONE',  ( -5.004894982100124068, 5.868074229652107121, 1.199719254218452935 ) ) ;
#211932 = CARTESIAN_POINT ( 'NONE',  ( -7.158341917891067219, 11.29522330427417565, 0.000000000000000000 ) ) ;
#211933 = CARTESIAN_POINT ( 'NONE',  ( 1.694636308673210801, -2.196210861363355082, -0.2157497520150277459 ) ) ;
#211934 = CARTESIAN_POINT ( 'NONE',  ( 3.285556943750000070, -2.034374999522043481, 0.000000000000000000 ) ) ;
#211935 = CARTESIAN_POINT ( 'NONE',  ( 5.717619619964247946, 0.3862620380215216476, -1.923179868201368548 ) ) ;
#211936 = CARTESIAN_POINT ( 'NONE',  ( -1.364683531249997417, 5.321875000341417916, 1.214306433183764966E-14 ) ) ;
#211937 = CARTESIAN_POINT ( 'NONE',  ( 1.499999999999989120, 4.577083334016148974, -0.8660254037844323793 ) ) ;
#211938 = CARTESIAN_POINT ( 'NONE',  ( 5.071574956294766068, 6.743279210435389359, -1.418366213760638317 ) ) ;
#211939 = CARTESIAN_POINT ( 'NONE',  ( -5.204170427930421283E-15, -5.907420853759282053, 10.91970695577496997 ) ) ;
#211940 = CARTESIAN_POINT ( 'NONE',  ( 3.802549092506895878, 1.579937072410386278, 0.9450539169142122553 ) ) ;
#211941 = ORIENTED_EDGE ( 'NONE', *, *, #83989, .T. ) ;
#211942 = CARTESIAN_POINT ( 'NONE',  ( 1.224999999999974332, 2.687500000682768508, -4.163336342344337027E-14 ) ) ;
#211943 = CARTESIAN_POINT ( 'NONE',  ( -6.333630315878337136, 10.54098580183340772, 0.000000000000000000 ) ) ;
#211944 = CARTESIAN_POINT ( 'NONE',  ( 6.082307721193076944, 1.091511717630256673, 1.817998432235830908 ) ) ;
#211945 = CARTESIAN_POINT ( 'NONE',  ( 11.91939557091538582, 6.691048939571908605, 0.9932293525215405428 ) ) ;
#211946 = CARTESIAN_POINT ( 'NONE',  ( 4.961394147597008697, 7.875711374583454827, -1.199719254218452047 ) ) ;
#211947 = AXIS2_PLACEMENT_3D ( 'NONE', #210476, #114136, #29616 ) ;
#211948 = CARTESIAN_POINT ( 'NONE',  ( 6.450472299244985663, 0.6421947732520795205, 1.958257120725328315 ) ) ;
#211951 = CARTESIAN_POINT ( 'NONE',  ( 4.071694929070113211, -1.056692140236010102, 1.507659738195665788 ) ) ;
#211950 = CARTESIAN_POINT ( 'NONE',  ( 1.890827768869116632, 0.1781016032055370568, 1.852494144255438346 ) ) ;
#211949 = CARTESIAN_POINT ( 'NONE',  ( -10.42580506876874047, 5.089579995674308854, 5.943607252937018082 ) ) ;
#211952 = CARTESIAN_POINT ( 'NONE',  ( 7.422199028477372451, 10.74665040227725044, -1.199719254218441611 ) ) ;
#211953 = CARTESIAN_POINT ( 'NONE',  ( -6.149505192250180663, 9.332117270003974951, -1.199719254218452047 ) ) ;
#211954 = CARTESIAN_POINT ( 'NONE',  ( 0.000000000000000000, 0.000000000000000000, -0.09999999999999592548 ) ) ;
#211955 = CARTESIAN_POINT ( 'NONE',  ( 2.807470779205251343, 1.864772411128329477, 1.179945617918669143 ) ) ;
#211956 = CARTESIAN_POINT ( 'NONE',  ( 5.940765808339826037, 0.4328084161881738945, 2.220481174026817772 ) ) ;
#211957 = CARTESIAN_POINT ( 'NONE',  ( -5.260200412422196159, 9.080724881227137502, -0.7216878364870207285 ) ) ;
#211958 = CARTESIAN_POINT ( 'NONE',  ( 6.047087830114247886, 0.1867083960328217995, 1.801967238635309165 ) ) ;
#211959 = CARTESIAN_POINT ( 'NONE',  ( 4.874201634824506080, -1.902012294098894829, -0.2279625308443770371 ) ) ;
#211960 = CARTESIAN_POINT ( 'NONE',  ( -0.7500000000000006661, 3.139583334016149418, -1.299038105676652011 ) ) ;
#211961 = CARTESIAN_POINT ( 'NONE',  ( 6.051601594667258333, 0.5412791183288803154, -1.790613848972313571 ) ) ;
#211962 = CARTESIAN_POINT ( 'NONE',  ( 5.863677653134839574, -0.4517109595482105555, 1.805248464757176041 ) ) ;
#211963 = CARTESIAN_POINT ( 'NONE',  ( -0.4019237886466933696, 13.05133545031537246, 1.500000000000005995 ) ) ;
#211964 = CARTESIAN_POINT ( 'NONE',  ( 0.09234973940512071489, -0.4041859633337717694, -1.833079292876439670 ) ) ;
#211965 = CARTESIAN_POINT ( 'NONE',  ( 1.587125413319636635, 1.679225032509903404, 1.116207499648947943 ) ) ;
#211967 = CARTESIAN_POINT ( 'NONE',  ( 2.772209899791327370, 1.127123820452385017, 1.778883819610539208 ) ) ;
#211966 = CARTESIAN_POINT ( 'NONE',  ( -8.992082194361570302, 11.51384853155376220, 1.599625672291269396 ) ) ;
#211968 = CARTESIAN_POINT ( 'NONE',  ( 9.582915646760733708, 10.07448976417602893, 0.7998128361456462443 ) ) ;
#211970 = CARTESIAN_POINT ( 'NONE',  ( -8.748035429315585532, 11.22912730566677553, -1.599625672291263179 ) ) ;
#211969 = CARTESIAN_POINT ( 'NONE',  ( 11.04536101718726293, 13.40000000000000036, -1.100000000000002087 ) ) ;
#211971 = DIRECTION ( 'NONE',  ( -0.8656921114426504582, -0.5005768354468328463, 3.719247132494280721E-15 ) ) ;
#211972 = CARTESIAN_POINT ( 'NONE',  ( 3.181903496825384092, 1.969597418195143446, -0.4466673548119536319 ) ) ;
#211973 = CARTESIAN_POINT ( 'NONE',  ( -1.201851678989727383E-14, 3.446875000341421469, -1.575800808251660134 ) ) ;
#211974 = CARTESIAN_POINT ( 'NONE',  ( 2.737856954955798727, 5.281584649835344258, 1.199719254218452047 ) ) ;
#211975 = CARTESIAN_POINT ( 'NONE',  ( 3.796290242343594468, -2.158924006851222988, -0.1102321833298808978 ) ) ;
#211976 = CARTESIAN_POINT ( 'NONE',  ( 5.691390622686558487, 9.861982503101517139, 0.7998128361456341429 ) ) ;
#211978 = CARTESIAN_POINT ( 'NONE',  ( 0.000000000000000000, -6.776263578034402713E-18, -3.474999999999992095 ) ) ;
#211977 = CARTESIAN_POINT ( 'NONE',  ( 6.343235766347262938, 8.493804042195527870, -1.599625672291281386 ) ) ;
#211979 =( BOUNDED_SURFACE ( )  B_SPLINE_SURFACE ( 3, 2, ( 
 ( #96547, #147409, #213435 ),
 ( #64016, #114955, #129110 ),
 ( #60814, #79197, #44588 ),
 ( #110702, #46722, #131214 ),
 ( #197202, #32578, #30462 ),
 ( #47796, #95486, #15243 ),
 ( #48841, #130164, #180956 ),
 ( #61886, #178851, #162594 ) ),
 .UNSPECIFIED., .F., .F., .T. ) 
 B_SPLINE_SURFACE_WITH_KNOTS ( ( 4, 2, 2, 4 ),
 ( 3, 3 ),
 ( 2.385244779468109755E-18, 0.0004821367237705008143, 0.0009642734475409992434, 0.001928546895081996101 ),
 ( 0.000000000000000000, 1.000000000000000000 ),
 .UNSPECIFIED. ) 
 GEOMETRIC_REPRESENTATION_ITEM ( )  RATIONAL_B_SPLINE_SURFACE ( (
 ( 1.000000000000000000, 0.8509629433086528527, 1.000000000000000000),
 ( 1.000000000000000000, 0.8509293920024736391, 1.000000000000000000),
 ( 1.000000000000000000, 0.8507640800581817153, 1.000000000000000000),
 ( 1.000000000000000000, 0.8504069559990277138, 1.000000000000000000),
 ( 1.000000000000000000, 0.8502555126865255497, 1.000000000000000000),
 ( 1.000000000000000000, 0.8490919837716710550, 1.000000000000000000),
 ( 1.000000000000000000, 0.8474110456169804406, 1.000000000000000000),
 ( 1.000000000000000000, 0.8462382765735556589, 1.000000000000000000) ) ) 
 REPRESENTATION_ITEM ( '' )  SURFACE ( )  );
#211980 = CARTESIAN_POINT ( 'NONE',  ( 8.202319746143333035, 12.51319743723517952, -0.7216878364870328300 ) ) ;
#211982 = CARTESIAN_POINT ( 'NONE',  ( 8.610948272048309704, 14.96724361927355496, -8.359267069145829510 ) ) ;
#211981 = CARTESIAN_POINT ( 'NONE',  ( 0.8190779338598102033, -1.572544420714114821, 1.497277704674306431 ) ) ;
#211983 = CARTESIAN_POINT ( 'NONE',  ( -6.643132081016132062, 8.773406732650713025, 1.443375672974078761 ) ) ;
#211984 = CARTESIAN_POINT ( 'NONE',  ( -0.6823417656250212460, 0.8010416670080899859, 1.181850606188755259 ) ) ;
#211985 = CARTESIAN_POINT ( 'NONE',  ( 2.489988787850425656, -2.185901284972164405, -0.1580625509675498419 ) ) ;
#211986 = DIRECTION ( 'NONE',  ( 0.000000000000000000, 8.546850786086437571E-32, 1.000000000000000000 ) ) ;
#211987 = CARTESIAN_POINT ( 'NONE',  ( 2.518781164845237175, 1.478067295746248400, -1.713045486838754794 ) ) ;
#211988 = CARTESIAN_POINT ( 'NONE',  ( -7.857113714319432063, 9.125386407249497012, 1.199719254218462483 ) ) ;
#211989 = CARTESIAN_POINT ( 'NONE',  ( -4.907688418022547516, 4.827984030555475314, 1.214306433183764966E-14 ) ) ;
#211990 = CARTESIAN_POINT ( 'NONE',  ( -1.364683531250012516, 3.342708333674756727, 0.7879004041258379498 ) ) ;
#211991 = CARTESIAN_POINT ( 'NONE',  ( 5.748548729368831545, 7.266256959964179529, 1.200940202139972435 ) ) ;
#211992 = CARTESIAN_POINT ( 'NONE',  ( 1.499999999999997113, 10.39583333333332860, -0.8660254037844378194 ) ) ;
#211993 = CARTESIAN_POINT ( 'NONE',  ( 5.506019780925567986, 8.477421273504887722, -1.082531754730548412 ) ) ;
#211994 = CARTESIAN_POINT ( 'NONE',  ( 3.426767255637660270, 0.04027588734063606429, 1.769438255327019593 ) ) ;
#211995 = STYLED_ITEM ( 'NONE', ( #123004 ), #66139 ) ;
#211996 = CARTESIAN_POINT ( 'NONE',  ( 5.983472182158235952, 2.041168445429199618, -0.8392293214988936212 ) ) ;
#211997 = VECTOR ( 'NONE', #54793, 1000.000000000000000 ) ;
#211998 = CARTESIAN_POINT ( 'NONE',  ( -1.402160292154681736E-14, 9.171875000341396245, 1.575800808251682339 ) ) ;
#211999 = CARTESIAN_POINT ( 'NONE',  ( -5.957882158562513908, 5.915560371269843465, -0.7998128361456362523 ) ) ;
#212000 = CARTESIAN_POINT ( 'NONE',  ( 0.000000000000000000, -1.000000000000000888, 0.000000000000000000 ) ) ;
#212002 = ORIENTED_EDGE ( 'NONE', *, *, #175718, .F. ) ;
#212001 = CARTESIAN_POINT ( 'NONE',  ( 4.904484127313208042, -1.798792703336571375, -0.2141664767603863595 ) ) ;
#212003 = CARTESIAN_POINT ( 'NONE',  ( 3.906994808788874174, 1.604092888448312326, 0.9621832354540850174 ) ) ;
#212004 = CARTESIAN_POINT ( 'NONE',  ( 3.028250241984064228, 1.103615759228196325, 1.751372171329562688 ) ) ;
#212005 = CARTESIAN_POINT ( 'NONE',  ( -7.607533590599451223, 9.008448956188397361, 1.082531754730549078 ) ) ;
#212006 = CARTESIAN_POINT ( 'NONE',  ( -11.01135777277262129, 10.89999999999998259, 1.399999999999998579 ) ) ;
#212007 = DIRECTION ( 'NONE',  ( 0.6507913734559640506, -0.7592566023653004592, 0.000000000000000000 ) ) ;
#212008 = CARTESIAN_POINT ( 'NONE',  ( -5.712738193804302256, 6.079813188454783024, 0.6294087663294201107 ) ) ;
#212009 = CARTESIAN_POINT ( 'NONE',  ( -0.6823417656249969321, 3.780208333674754506, -1.181850606188749264 ) ) ;
#212010 = CARTESIAN_POINT ( 'NONE',  ( 2.875390130891414042, -0.1950805366632331617, 1.952157403750237163 ) ) ;
#212011 = CARTESIAN_POINT ( 'NONE',  ( 1.141953626738337890, -0.04666616626641807708, -2.015725262716171695 ) ) ;
#212012 = CARTESIAN_POINT ( 'NONE',  ( -4.502189528189771472, 7.410248995266807803, -1.199719254218453823 ) ) ;
#212013 = CARTESIAN_POINT ( 'NONE',  ( 7.151035956204054855, 10.43029348462504124, 1.199719254218460707 ) ) ;
#212014 = CARTESIAN_POINT ( 'NONE',  ( 6.274684828636788225, -1.871173557121402542, -0.6205748305461754599 ) ) ;
#212015 = CARTESIAN_POINT ( 'NONE',  ( 1.364683531249988535, 3.155208333674756283, -0.7879004041258239610 ) ) ;
#212016 = CARTESIAN_POINT ( 'NONE',  ( 2.004154220962415689, -0.8570942286123193199, 1.821751609655430260 ) ) ;
#212018 = CARTESIAN_POINT ( 'NONE',  ( 2.109133483290903222, 0.003435389629122351501, 2.117403154539731602 ) ) ;
#212017 = CARTESIAN_POINT ( 'NONE',  ( -7.375272376154096143, 8.667201196010339004, -1.082531754730544860 ) ) ;
#212020 = EDGE_CURVE ( 'NONE', #136449, #45344, #168899, .T. ) ;
#212019 = CARTESIAN_POINT ( 'NONE',  ( 8.206244894449710614, 14.14858862657662009, -8.756074973582041565 ) ) ;
#212021 = CARTESIAN_POINT ( 'NONE',  ( 3.508316276398337319, 2.070544812355082254, 0.002818362966339192730 ) ) ;
#212022 = CARTESIAN_POINT ( 'NONE',  ( 5.422335090822693715, 5.290755458906732933, 0.000000000000000000 ) ) ;
#212024 = CARTESIAN_POINT ( 'NONE',  ( 2.703961570921634028, 5.242040035128820108, -1.199719254218446718 ) ) ;
#212023 = CARTESIAN_POINT ( 'NONE',  ( 6.386679164125504293, 1.819714881846513199, -1.029135884875460372 ) ) ;
#212026 = EDGE_LOOP ( 'NONE', ( #16964, #26099 ) ) ;
#212025 = CARTESIAN_POINT ( 'NONE',  ( 4.207882836062684540, -1.820678405428953095, 0.1343838851760314757 ) ) ;
#212027 = CARTESIAN_POINT ( 'NONE',  ( 8.353795204314554468, 12.89784483834236184, -0.7998128361456352531 ) ) ;
#212028 = CARTESIAN_POINT ( 'NONE',  ( -0.02244404828157393894, 7.629137130509076492, -2.789100637983292774 ) ) ;
#212030 = CIRCLE ( 'NONE', #21848, 1.500000000000000222 ) ;
#212029 = CARTESIAN_POINT ( 'NONE',  ( 12.54948750854022954, 7.400697955233512815, 0.9574523190714994136 ) ) ;
#212031 = CARTESIAN_POINT ( 'NONE',  ( -10.30047605039691128, 4.688744718740807116, 5.507884344589919934 ) ) ;
#212032 = CARTESIAN_POINT ( 'NONE',  ( 1.364683531249996529, 11.27604166700806410, 0.7879004041258403923 ) ) ;
#212033 = CARTESIAN_POINT ( 'NONE',  ( 5.461546741811521777, -1.510119879425949385, -1.173092037529008369 ) ) ;
#212034 = CARTESIAN_POINT ( 'NONE',  ( -10.47097470845587175, 11.11055866948701443, 1.040834085586084257E-14 ) ) ;
#212035 = CARTESIAN_POINT ( 'NONE',  ( 6.421758314367153275, 10.64380180007036891, -0.7998128361456291469 ) ) ;
#212036 = CARTESIAN_POINT ( 'NONE',  ( -1.360316468749995789, 0.9218750003414100114, -6.938893903907228378E-15 ) ) ;
#212037 = CARTESIAN_POINT ( 'NONE',  ( 9.499633399276474321, -8.038540703696423151, -0.09463244300327215697 ) ) ;
#212038 = CARTESIAN_POINT ( 'NONE',  ( 0.4328342922346357646, -1.301571265828086688, -1.302605208699902928 ) ) ;
#212039 = ORIENTED_EDGE ( 'NONE', *, *, #213502, .T. ) ;
#212040 = FACE_OUTER_BOUND ( 'NONE', #2865, .T. ) ;
#212041 = CARTESIAN_POINT ( 'NONE',  ( 4.200366636497298245, -0.5845007089231197828, -1.776970133648393624 ) ) ;
#212042 = CARTESIAN_POINT ( 'NONE',  ( -0.7684286640458091178, -3.130108765795259984, -3.305065527396989111 ) ) ;
#212043 = CARTESIAN_POINT ( 'NONE',  ( 6.156284269057003655, 9.340026192945279249, -1.199719254218452047 ) ) ;
#212044 = CARTESIAN_POINT ( 'NONE',  ( 0.08011315928756995719, 14.48196125337680229, 11.99973258290717659 ) ) ;
#212045 = CIRCLE ( 'NONE', #201691, 0.09999999999999982514 ) ;
#212046 =( BOUNDED_SURFACE ( )  B_SPLINE_SURFACE ( 1, 2, ( 
 ( #103522, #2785, #132854, #101380, #183696, #150151, #115563, #116628, #166383, #134976, #182622, #167455, #136028, #1721, #199933, #197811, #34245, #149067, #51580, #152272, #85129, #165317, #148020, #100317, #99269, #151215, #102448, #117705, #168514, #200984, #69917, #118759, #53702, #81934, #184744, #202041, #20114, #119834, #67778, #133927, #185813, #37445, #65655, #131802, #49444, #33187, #181559, #155469, #7054, #107856, #41745, #72056, #171713, #57964, #22229, #120915, #173882, #154406, #121988, #153334, #4908, #204175, #75287, #25459, #169581, #156549, #138167, #39582, #104598, #186888, #54767, #140321, #88342, #55832, #38520, #91566, #90485, #189031, #42818, #21164, #73127, #170644, #205260, #187954, #40669, #139229, #137098, #5985, #105684, #157619, #87268, #70985, #106773, #141402, #23310, #206339, #9216, #203124, #56901, #89420, #123075, #172801, #24372, #8144, #74227, #124130, #207411, #190091, #59030, #125188, #191149, #177059, #143532, #80627, #61170, #93696, #129463, #176005, #145670, #44945, #195447, #127331, #43879, #161889, #111053, #160810, #46009, #108923, #60099, #28676, #211667, #94763, #109993, #193300, #144599, #210614, #12401, #62241, #78482, #96901, #209528, #27597, #13476, #113194, #159738, #179199, #11336, #192216, #142456, #77417, #126257, #128400, #194367, #146719, #112130, #158676, #95832, #178133, #196507, #29748, #174945, #92635, #79552, #30823, #162952, #10273, #14530, #63303, #47076, #212735, #64372, #130518, #26527, #76349, #208464, #116373, #32935, #65404, #36114, #85949, #115318, #18791, #84874, #16657, #33990, #181308, #150963, #100065, #388, #166128, #2528, #51318, #68603, #134726, #182361, #50253, #83802, #17714, #132601, #213781, #1463, #99009, #165065, #183440, #164018, #149895, #200732, #101115, #3592, #67528, #135776, #117445, #97960, #152024, #69669, #131551, #133671, #199675, #82743, #35044, #167202, #48149, #15592, #19864, #81678, #147765, #148816, #52383, #118511, #114262, #184495, #66460, #102197, #168263, #180259, #197553, #198607, #31883, #49197, #38264, #155221 ),
 ( #105426, #87009, #23051, #5723, #6802, #171463, #169330, #153080, #186638, #206084, #119579, #37192, #138986, #173632, #170385, #24128, #73967, #185563, #89169, #103268, #54515, #53441, #203933, #88083, #72878, #205007, #140062, #90230, #156295, #7879, #157365, #55581, #21973, #25203, #154156, #104341, #57718, #120659, #123877, #137913, #189842, #71802, #136842, #40414, #121736, #39330, #56654, #201799, #4657, #187702, #41489, #122817, #202867, #188775, #106517, #172543, #107601, #91308, #8959, #75034, #20914, #70729, #174695, #191958, #158422, #76097, #44692, #178954, #125999, #190898, #128149, #110800, #14274, #142200, #141148, #124935, #209272, #211419, #63051, #42562, #129216, #11083, #10021, #160551, #208215, #195192, #79303, #60917, #58781, #127076, #43625, #59847, #46828, #109740, #143281, #29494, #175751, #92386, #145419, #27342, #93444, #108664, #26269, #159483, #112941, #30568, #207158, #194109, #77159, #193038, #176803, #28420, #94513, #111877, #12159, #78230, #144352, #96648, #61993, #210354, #45758, #177881, #95586, #161635, #13229, #162702, #99818, #49999, #47904, #31631, #65159, #84624, #212482, #130268, #17469, #52133, #48946, #117191, #166958, #64125, #116122, #196257, #147515, #146465, #82487, #181062, #198359, #83553, #18548, #183191, #34797, #100871, #35872, #148574, #115066, #118261, #32680, #131315, #150716, #213536, #2276, #16407, #68352, #98759, #15344, #133418, #143, #132356, #149635, #80369, #97708, #66209, #134485, #182110, #81436, #164815, #33739, #165883, #1216, #67279, #199424, #200487, #51068, #197307, #184245, #101947, #168013, #114014, #180009, #163766, #204747, #22798, #56398, #40152, #153904, #21722, #55331, #203683, #104088, #185312, #187453, #70479, #86761, #154967, #135525, #121482, #172287, #72630, #189588, #5474, #107341, #88913, #69418, #57464, #41234, #103017, #39081, #71554, #202618, #6552, #137662, #123624, #201549, #205832, #53195, #119326, #136594, #138729, #105166, #19617, #122559, #54268, #171205, #188520, #87833, #36934, #120404, #170137, #106265, #186380, #23875 ) ),
 .UNSPECIFIED., .F., .F., .T. ) 
 B_SPLINE_SURFACE_WITH_KNOTS ( ( 2, 2 ),
 ( 3, 2, 2, 2, 2, 2, 2, 2, 2, 2, 2, 2, 2, 2, 2, 2, 2, 2, 2, 2, 2, 2, 2, 2, 2, 2, 2, 2, 2, 2, 2, 2, 2, 2, 2, 2, 2, 2, 2, 2, 2, 2, 2, 2, 2, 2, 2, 2, 2, 2, 2, 2, 2, 2, 2, 2, 2, 2, 2, 2, 2, 2, 2, 2, 2, 2, 2, 2, 2, 2, 2, 2, 2, 2, 2, 2, 2, 2, 2, 2, 2, 2, 2, 2, 2, 2, 2, 2, 2, 2, 2, 2, 2, 2, 2, 2, 2, 2, 2, 2, 2, 2, 2, 2, 2, 2, 2, 2, 2, 2, 2, 2, 2, 2, 2, 2, 2, 2, 2, 2, 3 ),
 ( 0.000000000000000000, 1.000000000000000000 ),
 ( 0.000000000000000000, 0.008333333333333333218, 0.01666666666666666644, 0.02500000000000000139, 0.03333333333333333287, 0.04166666666666666435, 0.05000000000000000278, 0.05833333333333333426, 0.06666666666666666574, 0.07499999999999999722, 0.08333333333333332871, 0.09166666666666666019, 0.1000000000000000056, 0.1083333333333333370, 0.1166666666666666685, 0.1250000000000000000, 0.1333333333333333315, 0.1416666666666666630, 0.1499999999999999944, 0.1583333333333333259, 0.1666666666666666574, 0.1749999999999999889, 0.1833333333333333204, 0.1916666666666666796, 0.2000000000000000111, 0.2083333333333333426, 0.2166666666666666741, 0.2250000000000000056, 0.2333333333333333370, 0.2416666666666666685, 0.2500000000000000000, 0.2583333333333333592, 0.2666666666666666630, 0.2750000000000000222, 0.2833333333333333259, 0.2916666666666666852, 0.2999999999999999889, 0.3083333333333333481, 0.3166666666666666519, 0.3250000000000000111, 0.3333333333333333148, 0.3416666666666666741, 0.3499999999999999778, 0.3583333333333333370, 0.3666666666666666408, 0.3750000000000000000, 0.3833333333333333592, 0.3916666666666666630, 0.4000000000000000222, 0.4083333333333333259, 0.4166666666666666852, 0.4249999999999999889, 0.4333333333333333481, 0.4416666666666666519, 0.4500000000000000111, 0.4583333333333333148, 0.4666666666666666741, 0.4749999999999999778, 0.4833333333333333370, 0.4916666666666666408, 0.5000000000000000000, 0.5083333333333333037, 0.5166666666666667185, 0.5250000000000000222, 0.5333333333333333259, 0.5416666666666666297, 0.5500000000000000444, 0.5583333333333333481, 0.5666666666666666519, 0.5749999999999999556, 0.5833333333333333703, 0.5916666666666666741, 0.5999999999999999778, 0.6083333333333332815, 0.6166666666666666963, 0.6250000000000000000, 0.6333333333333333037, 0.6416666666666667185, 0.6500000000000000222, 0.6583333333333333259, 0.6666666666666666297, 0.6750000000000000444, 0.6833333333333333481, 0.6916666666666666519, 0.6999999999999999556, 0.7083333333333333703, 0.7166666666666666741, 0.7249999999999999778, 0.7333333333333332815, 0.7416666666666666963, 0.7500000000000000000, 0.7583333333333333037, 0.7666666666666667185, 0.7750000000000000222, 0.7833333333333333259, 0.7916666666666666297, 0.8000000000000000444, 0.8083333333333333481, 0.8166666666666666519, 0.8249999999999999556, 0.8333333333333333703, 0.8416666666666666741, 0.8499999999999999778, 0.8583333333333332815, 0.8666666666666666963, 0.8750000000000000000, 0.8833333333333333037, 0.8916666666666667185, 0.9000000000000000222, 0.9083333333333333259, 0.9166666666666666297, 0.9250000000000000444, 0.9333333333333333481, 0.9416666666666666519, 0.9499999999999999556, 0.9583333333333333703, 0.9666666666666666741, 0.9749999999999999778, 0.9833333333333332815, 0.9916666666666666963, 1.000000000000000000 ),
 .UNSPECIFIED. ) 
 GEOMETRIC_REPRESENTATION_ITEM ( )  RATIONAL_B_SPLINE_SURFACE ( (
 ( 1.000000000000000000, 0.8660254037844387076, 1.000000000000000000, 0.8660254037844387076, 1.000000000000000000, 0.8660254037844387076, 1.000000000000000000, 0.8660254037844387076, 1.000000000000000000, 0.8660254037844387076, 1.000000000000000000, 0.8660254037844387076, 1.000000000000000000, 0.8660254037844387076, 1.000000000000000000, 0.8660254037844387076, 1.000000000000000000, 0.8660254037844387076, 1.000000000000000000, 0.8660254037844387076, 1.000000000000000000, 0.8660254037844387076, 1.000000000000000000, 0.8660254037844387076, 1.000000000000000000, 0.8660254037844387076, 1.000000000000000000, 0.8660254037844387076, 1.000000000000000000, 0.8660254037844387076, 1.000000000000000000, 0.8660254037844387076, 1.000000000000000000, 0.8660254037844387076, 1.000000000000000000, 0.8660254037844387076, 1.000000000000000000, 0.8660254037844387076, 1.000000000000000000, 0.8660254037844387076, 1.000000000000000000, 0.8660254037844387076, 1.000000000000000000, 0.8660254037844387076, 1.000000000000000000, 0.8660254037844387076, 1.000000000000000000, 0.8660254037844387076, 1.000000000000000000, 0.8660254037844387076, 1.000000000000000000, 0.8660254037844387076, 1.000000000000000000, 0.8660254037844387076, 1.000000000000000000, 0.8660254037844387076, 1.000000000000000000, 0.8660254037844387076, 1.000000000000000000, 0.8660254037844387076, 1.000000000000000000, 0.8660254037844387076, 1.000000000000000000, 0.8660254037844387076, 1.000000000000000000, 0.8660254037844387076, 1.000000000000000000, 0.8660254037844387076, 1.000000000000000000, 0.8660254037844387076, 1.000000000000000000, 0.8660254037844387076, 1.000000000000000000, 0.8660254037844387076, 1.000000000000000000, 0.8660254037844387076, 1.000000000000000000, 0.8660254037844387076, 1.000000000000000000, 0.8660254037844387076, 1.000000000000000000, 0.8660254037844387076, 1.000000000000000000, 0.8660254037844387076, 1.000000000000000000, 0.8660254037844387076, 1.000000000000000000, 0.8660254037844387076, 1.000000000000000000, 0.8660254037844387076, 1.000000000000000000, 0.8660254037844387076, 1.000000000000000000, 0.8660254037844387076, 1.000000000000000000, 0.8660254037844387076, 1.000000000000000000, 0.8660254037844387076, 1.000000000000000000, 0.8660254037844387076, 1.000000000000000000, 0.8660254037844387076, 1.000000000000000000, 0.8660254037844387076, 1.000000000000000000, 0.8660254037844387076, 1.000000000000000000, 0.8660254037844387076, 1.000000000000000000, 0.8660254037844387076, 1.000000000000000000, 0.8660254037844387076, 1.000000000000000000, 0.8660254037844387076, 1.000000000000000000, 0.8660254037844387076, 1.000000000000000000, 0.8660254037844387076, 1.000000000000000000, 0.8660254037844387076, 1.000000000000000000, 0.8660254037844387076, 1.000000000000000000, 0.8660254037844387076, 1.000000000000000000, 0.8660254037844387076, 1.000000000000000000, 0.8660254037844387076, 1.000000000000000000, 0.8660254037844387076, 1.000000000000000000, 0.8660254037844387076, 1.000000000000000000, 0.8660254037844387076, 1.000000000000000000, 0.8660254037844387076, 1.000000000000000000, 0.8660254037844387076, 1.000000000000000000, 0.8660254037844387076, 1.000000000000000000, 0.8660254037844387076, 1.000000000000000000, 0.8660254037844387076, 1.000000000000000000, 0.8660254037844387076, 1.000000000000000000, 0.8660254037844387076, 1.000000000000000000, 0.8660254037844387076, 1.000000000000000000, 0.8660254037844387076, 1.000000000000000000, 0.8660254037844387076, 1.000000000000000000, 0.8660254037844387076, 1.000000000000000000, 0.8660254037844387076, 1.000000000000000000, 0.8660254037844387076, 1.000000000000000000, 0.8660254037844387076, 1.000000000000000000, 0.8660254037844387076, 1.000000000000000000, 0.8660254037844387076, 1.000000000000000000, 0.8660254037844387076, 1.000000000000000000, 0.8660254037844387076, 1.000000000000000000, 0.8660254037844387076, 1.000000000000000000, 0.8660254037844387076, 1.000000000000000000, 0.8660254037844387076, 1.000000000000000000, 0.8660254037844387076, 1.000000000000000000, 0.8660254037844387076, 1.000000000000000000, 0.8660254037844387076, 1.000000000000000000, 0.8660254037844387076, 1.000000000000000000, 0.8660254037844387076, 1.000000000000000000, 0.8660254037844387076, 1.000000000000000000, 0.8660254037844387076, 1.000000000000000000, 0.8660254037844387076, 1.000000000000000000, 0.8660254037844387076, 1.000000000000000000, 0.8660254037844387076, 1.000000000000000000, 0.8660254037844387076, 1.000000000000000000, 0.8660254037844387076, 1.000000000000000000, 0.8660254037844387076, 1.000000000000000000, 0.8660254037844387076, 1.000000000000000000, 0.8660254037844387076, 1.000000000000000000, 0.8660254037844387076, 1.000000000000000000, 0.8660254037844387076, 1.000000000000000000, 0.8660254037844387076, 1.000000000000000000, 0.8660254037844387076, 1.000000000000000000, 0.8660254037844387076, 1.000000000000000000, 0.8660254037844387076, 1.000000000000000000, 0.8660254037844387076, 1.000000000000000000, 0.8660254037844387076, 1.000000000000000000, 0.8660254037844387076, 1.000000000000000000, 0.8660254037844387076, 1.000000000000000000, 0.8660254037844387076, 1.000000000000000000, 0.8660254037844387076, 1.000000000000000000, 0.8660254037844387076, 1.000000000000000000, 0.8660254037844387076, 1.000000000000000000, 0.8660254037844387076, 1.000000000000000000, 0.8660254037844387076, 1.000000000000000000, 0.8660254037844387076, 1.000000000000000000),
 ( 1.000000000000000000, 0.8660254037844387076, 1.000000000000000000, 0.8660254037844387076, 1.000000000000000000, 0.8660254037844387076, 1.000000000000000000, 0.8660254037844387076, 1.000000000000000000, 0.8660254037844387076, 1.000000000000000000, 0.8660254037844387076, 1.000000000000000000, 0.8660254037844387076, 1.000000000000000000, 0.8660254037844387076, 1.000000000000000000, 0.8660254037844387076, 1.000000000000000000, 0.8660254037844387076, 1.000000000000000000, 0.8660254037844387076, 1.000000000000000000, 0.8660254037844387076, 1.000000000000000000, 0.8660254037844387076, 1.000000000000000000, 0.8660254037844387076, 1.000000000000000000, 0.8660254037844387076, 1.000000000000000000, 0.8660254037844387076, 1.000000000000000000, 0.8660254037844387076, 1.000000000000000000, 0.8660254037844387076, 1.000000000000000000, 0.8660254037844387076, 1.000000000000000000, 0.8660254037844387076, 1.000000000000000000, 0.8660254037844387076, 1.000000000000000000, 0.8660254037844387076, 1.000000000000000000, 0.8660254037844387076, 1.000000000000000000, 0.8660254037844387076, 1.000000000000000000, 0.8660254037844387076, 1.000000000000000000, 0.8660254037844387076, 1.000000000000000000, 0.8660254037844387076, 1.000000000000000000, 0.8660254037844387076, 1.000000000000000000, 0.8660254037844387076, 1.000000000000000000, 0.8660254037844387076, 1.000000000000000000, 0.8660254037844387076, 1.000000000000000000, 0.8660254037844387076, 1.000000000000000000, 0.8660254037844387076, 1.000000000000000000, 0.8660254037844387076, 1.000000000000000000, 0.8660254037844387076, 1.000000000000000000, 0.8660254037844387076, 1.000000000000000000, 0.8660254037844387076, 1.000000000000000000, 0.8660254037844387076, 1.000000000000000000, 0.8660254037844387076, 1.000000000000000000, 0.8660254037844387076, 1.000000000000000000, 0.8660254037844387076, 1.000000000000000000, 0.8660254037844387076, 1.000000000000000000, 0.8660254037844387076, 1.000000000000000000, 0.8660254037844387076, 1.000000000000000000, 0.8660254037844387076, 1.000000000000000000, 0.8660254037844387076, 1.000000000000000000, 0.8660254037844387076, 1.000000000000000000, 0.8660254037844387076, 1.000000000000000000, 0.8660254037844387076, 1.000000000000000000, 0.8660254037844387076, 1.000000000000000000, 0.8660254037844387076, 1.000000000000000000, 0.8660254037844387076, 1.000000000000000000, 0.8660254037844387076, 1.000000000000000000, 0.8660254037844387076, 1.000000000000000000, 0.8660254037844387076, 1.000000000000000000, 0.8660254037844387076, 1.000000000000000000, 0.8660254037844387076, 1.000000000000000000, 0.8660254037844387076, 1.000000000000000000, 0.8660254037844387076, 1.000000000000000000, 0.8660254037844387076, 1.000000000000000000, 0.8660254037844387076, 1.000000000000000000, 0.8660254037844387076, 1.000000000000000000, 0.8660254037844387076, 1.000000000000000000, 0.8660254037844387076, 1.000000000000000000, 0.8660254037844387076, 1.000000000000000000, 0.8660254037844387076, 1.000000000000000000, 0.8660254037844387076, 1.000000000000000000, 0.8660254037844387076, 1.000000000000000000, 0.8660254037844387076, 1.000000000000000000, 0.8660254037844387076, 1.000000000000000000, 0.8660254037844387076, 1.000000000000000000, 0.8660254037844387076, 1.000000000000000000, 0.8660254037844387076, 1.000000000000000000, 0.8660254037844387076, 1.000000000000000000, 0.8660254037844387076, 1.000000000000000000, 0.8660254037844387076, 1.000000000000000000, 0.8660254037844387076, 1.000000000000000000, 0.8660254037844387076, 1.000000000000000000, 0.8660254037844387076, 1.000000000000000000, 0.8660254037844387076, 1.000000000000000000, 0.8660254037844387076, 1.000000000000000000, 0.8660254037844387076, 1.000000000000000000, 0.8660254037844387076, 1.000000000000000000, 0.8660254037844387076, 1.000000000000000000, 0.8660254037844387076, 1.000000000000000000, 0.8660254037844387076, 1.000000000000000000, 0.8660254037844387076, 1.000000000000000000, 0.8660254037844387076, 1.000000000000000000, 0.8660254037844387076, 1.000000000000000000, 0.8660254037844387076, 1.000000000000000000, 0.8660254037844387076, 1.000000000000000000, 0.8660254037844387076, 1.000000000000000000, 0.8660254037844387076, 1.000000000000000000, 0.8660254037844387076, 1.000000000000000000, 0.8660254037844387076, 1.000000000000000000, 0.8660254037844387076, 1.000000000000000000, 0.8660254037844387076, 1.000000000000000000, 0.8660254037844387076, 1.000000000000000000, 0.8660254037844387076, 1.000000000000000000, 0.8660254037844387076, 1.000000000000000000, 0.8660254037844387076, 1.000000000000000000, 0.8660254037844387076, 1.000000000000000000, 0.8660254037844387076, 1.000000000000000000, 0.8660254037844387076, 1.000000000000000000, 0.8660254037844387076, 1.000000000000000000, 0.8660254037844387076, 1.000000000000000000, 0.8660254037844387076, 1.000000000000000000, 0.8660254037844387076, 1.000000000000000000, 0.8660254037844387076, 1.000000000000000000, 0.8660254037844387076, 1.000000000000000000, 0.8660254037844387076, 1.000000000000000000, 0.8660254037844387076, 1.000000000000000000, 0.8660254037844387076, 1.000000000000000000, 0.8660254037844387076, 1.000000000000000000, 0.8660254037844387076, 1.000000000000000000, 0.8660254037844387076, 1.000000000000000000, 0.8660254037844387076, 1.000000000000000000, 0.8660254037844387076, 1.000000000000000000, 0.8660254037844387076, 1.000000000000000000, 0.8660254037844387076, 1.000000000000000000) ) ) 
 REPRESENTATION_ITEM ( '' )  SURFACE ( )  );
#212047 = CIRCLE ( 'NONE', #201692, 2.000000000000000000 ) ;
#212048 = CARTESIAN_POINT ( 'NONE',  ( -5.536209915801717507, 7.449110030843877794, 1.248366777010925910 ) ) ;
#212049 = EDGE_CURVE ( 'NONE', #177991, #147438, #151122, .T. ) ;
#212050 = CARTESIAN_POINT ( 'NONE',  ( -6.155038550924159857, 8.203964280876741455, 1.443375672974078761 ) ) ;
#212051 = CARTESIAN_POINT ( 'NONE',  ( 3.822509244049070887, 6.547012320444182798, -1.199719254218452047 ) ) ;
#212052 = CARTESIAN_POINT ( 'NONE',  ( 1.094512790084944287, 1.939365640515663181, 0.3419967617025142514 ) ) ;
#212053 = CARTESIAN_POINT ( 'NONE',  ( 2.056267757160272325, -1.238304521155994209, 1.591332585091954854 ) ) ;
#212054 = CARTESIAN_POINT ( 'NONE',  ( -7.808606406466886973, 11.19745900993164511, 1.199719254218453823 ) ) ;
#212055 = CARTESIAN_POINT ( 'NONE',  ( 5.448397627845284141, 7.449826213943242514, 1.599625672291268286 ) ) ;
#212056 = CARTESIAN_POINT ( 'NONE',  ( 2.150558370509841666, -1.692889690492072718, 1.391600924549152296 ) ) ;
#212057 =( NAMED_UNIT ( * ) PLANE_ANGLE_UNIT ( ) SI_UNIT ( $, .RADIAN. ) );
#212058 = CARTESIAN_POINT ( 'NONE',  ( -9.459838494033043332, 12.05956421450382088, 1.599625672291281386 ) ) ;
#212059 = CARTESIAN_POINT ( 'NONE',  ( 6.825078400183588023, 6.037369320589220045, 2.550557596425677254 ) ) ;
#212060 = DIRECTION ( 'NONE',  ( -5.578564026256490882E-16, -1.000000000000000000, -9.066213480720158442E-32 ) ) ;
#212061 = CARTESIAN_POINT ( 'NONE',  ( -0.5773502691896470473, -2.500000000000002220, 0.9999999999999991118 ) ) ;
#212062 = CARTESIAN_POINT ( 'NONE',  ( 7.560643217915098191, 11.97250085420964716, -0.7998128361456291469 ) ) ;
#212063 = VECTOR ( 'NONE', #131022, 1000.000000000000114 ) ;
#212064 = CARTESIAN_POINT ( 'NONE',  ( 7.334597915313080918, 9.580116872663850813, 1.040834085586084257E-14 ) ) ;
#212065 = CARTESIAN_POINT ( 'NONE',  ( 6.536439455564164724, 7.758839131980592718, 1.082531754730549967 ) ) ;
#212066 = ORIENTED_EDGE ( 'NONE', *, *, #104440, .F. ) ;
#212068 = CARTESIAN_POINT ( 'NONE',  ( 1.365886254406587064, 0.5821385057369383720, -1.927099543440218499 ) ) ;
#212067 = CARTESIAN_POINT ( 'NONE',  ( 4.933073973922719624, -1.305863698873997780, -1.298312775753200699 ) ) ;
#212069 = CARTESIAN_POINT ( 'NONE',  ( 3.216491754421717530, -1.877423419238280822, -1.325616196499669108 ) ) ;
#212070 = CARTESIAN_POINT ( 'NONE',  ( 2.447915292705178825, -0.8007319036262178225, 1.680036726287994719 ) ) ;
#212071 = CARTESIAN_POINT ( 'NONE',  ( 3.285556943750000070, -2.034374999522043481, 0.000000000000000000 ) ) ;
#212072 = CYLINDRICAL_SURFACE ( 'NONE', #60605, 0.3999999999999997446 ) ;
#212073 = CARTESIAN_POINT ( 'NONE',  ( 6.029550621839829816, -0.2273517531893587407, 1.898748578088353733 ) ) ;
#212074 = CARTESIAN_POINT ( 'NONE',  ( -7.486073373039941359, 11.88550270185529278, -0.7998128361456291469 ) ) ;
#212075 = CARTESIAN_POINT ( 'NONE',  ( -6.482206841109545259, 6.735198534148810090, 0.7216878364870257245 ) ) ;
#212077 = CARTESIAN_POINT ( 'NONE',  ( 3.713615009860570915, -1.843089489661839053, 0.3189824552965599969 ) ) ;
#212076 = CARTESIAN_POINT ( 'NONE',  ( 5.196857871947656804, 1.709930586799845553, 1.202785367055765775 ) ) ;
#212078 = CARTESIAN_POINT ( 'NONE',  ( 6.751597309925441159, 9.860318714012938912, -1.082531754730537088 ) ) ;
#212079 = CARTESIAN_POINT ( 'NONE',  ( 6.321814700078944860, 1.054209175812788502, -1.509406368332133930 ) ) ;
#212080 = CIRCLE ( 'NONE', #125770, 2.000000000000006217 ) ;
#212081 = CARTESIAN_POINT ( 'NONE',  ( 3.765413976293345844, 5.416068943807445635, 1.599625672291267398 ) ) ;
#212082 = CARTESIAN_POINT ( 'NONE',  ( 0.3532572990641478228, -7.666862990898835051, -10.99465531782955985 ) ) ;
#212083 = CARTESIAN_POINT ( 'NONE',  ( 5.145002536317147879, -1.476695180717332967, 0.8911356905443221788 ) ) ;
#212084 = CARTESIAN_POINT ( 'NONE',  ( -6.413170354464012846, 7.440785820751486312, 1.199719254218450271 ) ) ;
#212085 = CARTESIAN_POINT ( 'NONE',  ( 0.5978079470381278959, -0.2563149341858957930, 1.714925299717950491 ) ) ;
#212086 = DIRECTION ( 'NONE',  ( 0.000000000000000000, 1.000000000000000000, 0.000000000000000000 ) ) ;
#212087 = CARTESIAN_POINT ( 'NONE',  ( 1.908029163539569417, 3.237038651130959455, 0.4603255239806047228 ) ) ;
#212088 = DIRECTION ( 'NONE',  ( 0.000000000000000000, -1.000000000000000000, 0.000000000000000000 ) ) ;
#212089 = CARTESIAN_POINT ( 'NONE',  ( 4.610331778354775700, 2.170709972759849116, -0.04705437256473897489 ) ) ;
#212090 = CARTESIAN_POINT ( 'NONE',  ( 3.879382553896340013, 1.718498013671100777, -0.6167319420108534622 ) ) ;
#212091 = CARTESIAN_POINT ( 'NONE',  ( 1.410910527293834260, -1.549868713165471590, 1.202602906592651788 ) ) ;
#212092 = CARTESIAN_POINT ( 'NONE',  ( 0.4041146219485808877, -1.136702437883057470, -1.786057295064005013 ) ) ;
#212094 = CARTESIAN_POINT ( 'NONE',  ( -1.364683531249997417, 4.071875000341417028, 1.214306433183764966E-14 ) ) ;
#212093 = CARTESIAN_POINT ( 'NONE',  ( 6.497627784488766878, -2.291974509058695375, 0.05125074467529803363 ) ) ;
#212095 = CARTESIAN_POINT ( 'NONE',  ( 3.697672731465083462, 7.367968498737613281, 2.499999999999998668 ) ) ;
#212096 = CARTESIAN_POINT ( 'NONE',  ( 8.269583629331492602, 11.73526576994040482, 1.199719254218450271 ) ) ;
#212097 = CARTESIAN_POINT ( 'NONE',  ( 2.473420802178166067, -1.846219560914775570, -1.042883725575906029 ) ) ;
#212098 = CARTESIAN_POINT ( 'NONE',  ( -4.446711195602255806, 5.250546485366484717, -1.082531754730544860 ) ) ;
#212099 = CARTESIAN_POINT ( 'NONE',  ( 5.597249624757115960, 5.760645890509660916, 0.6703580308099268414 ) ) ;
#212100 = CARTESIAN_POINT ( 'NONE',  ( -5.395781948114519722, 5.397426482329451325, 0.000000000000000000 ) ) ;
#212101 = CARTESIAN_POINT ( 'NONE',  ( 0.3388458784313007066, -2.007247006727829852, -0.5063607812752639603 ) ) ;
#212103 = CARTESIAN_POINT ( 'NONE',  ( -0.7500000000000006661, 13.98958333401613352, -1.299038105676657340 ) ) ;
#212102 = CARTESIAN_POINT ( 'NONE',  ( 6.983263157960383438, 0.5812290088160886325, 2.006563525967783868 ) ) ;
#212105 = ORIENTED_EDGE ( 'NONE', *, *, #14127, .F. ) ;
#212104 = CARTESIAN_POINT ( 'NONE',  ( 2.034109888970101920, -2.153751770765993001, 0.5431444268512666262 ) ) ;
#212106 = CARTESIAN_POINT ( 'NONE',  ( 0.4405775615070831042, -1.946229768708742647, -1.222969628347547966 ) ) ;
#212108 = CARTESIAN_POINT ( 'NONE',  ( 5.700070374860989553, 0.8410407859656986451, -1.883500665774339833 ) ) ;
#212107 = CARTESIAN_POINT ( 'NONE',  ( 3.171717870593107058, 5.787755718078879674, -1.199719254218446718 ) ) ;
#212110 = CARTESIAN_POINT ( 'NONE',  ( 1.737500000000001155, -1.283333333333334325, 3.009438278150922130 ) ) ;
#212109 = CARTESIAN_POINT ( 'NONE',  ( 4.908934136599710563, 7.884784371745123366, 1.199719254218451159 ) ) ;
#212111 = CARTESIAN_POINT ( 'NONE',  ( 6.222266154028957885, 6.224008365980749247, 0.7998128361456352531 ) ) ;
#212112 = CARTESIAN_POINT ( 'NONE',  ( -1.642778471875000035, -2.705208332855375986, -2.845375778867859751 ) ) ;
#212113 = CARTESIAN_POINT ( 'NONE',  ( 0.2329586101569346424, 2.887341434808698981, -2.334705299551639079 ) ) ;
#212114 = CARTESIAN_POINT ( 'NONE',  ( 5.302248432823610358, 1.390444127666954355, -1.207098008268410183 ) ) ;
#212115 = CARTESIAN_POINT ( 'NONE',  ( 4.493637847925535667, 7.329995691633395261, -1.199719254218452047 ) ) ;
#212116 = CARTESIAN_POINT ( 'NONE',  ( 1.746655555778130253, -1.459509165399446529, 0.9187280511932097715 ) ) ;
#212117 = CARTESIAN_POINT ( 'NONE',  ( 0.9543149826918421175, -1.275552737861269437, 1.561884623745241951 ) ) ;
#212118 = CARTESIAN_POINT ( 'NONE',  ( 1.934640009471942035, -1.849324232932574530, -1.365145410983016117 ) ) ;
#212119 = CARTESIAN_POINT ( 'NONE',  ( 0.6823417656249917140, 3.655208333674754506, 1.181850606188765695 ) ) ;
#212120 = CARTESIAN_POINT ( 'NONE',  ( 1.985968398796404299, 1.559226912063184534, 1.639530705753606821 ) ) ;
#212121 = CARTESIAN_POINT ( 'NONE',  ( 4.354198888085320185, 2.105621147513780045, -0.05115374888297812700 ) ) ;
#212122 = CARTESIAN_POINT ( 'NONE',  ( -4.065465959251405081, 5.836405933916976707, -1.599625672291271394 ) ) ;
#212123 = CARTESIAN_POINT ( 'NONE',  ( 2.354462415756667593, -1.371198970962312691, 1.118854571612490245 ) ) ;
#212124 = CARTESIAN_POINT ( 'NONE',  ( 5.612185521052973414, 8.634967976948757951, -1.199719254218440723 ) ) ;
#212126 = CARTESIAN_POINT ( 'NONE',  ( 5.776963781812925802, 2.119385065811297597, -0.8740618393795733798 ) ) ;
#212125 = CARTESIAN_POINT ( 'NONE',  ( 4.814553946184248368, 7.670711132973337065, -1.082531754730548412 ) ) ;
#212127 = CARTESIAN_POINT ( 'NONE',  ( -5.436983294280064882, 6.301900917203534291, 1.199719254218450271 ) ) ;
#212129 = UNCERTAINTY_MEASURE_WITH_UNIT (LENGTH_MEASURE( 1.000000000000000082E-05 ), #52892, 'distance_accuracy_value', 'NONE');
#212128 = B_SPLINE_CURVE_WITH_KNOTS ( 'NONE', 3,
 ( #88614, #153606, #121185, #189293, #36634, #188217 ),
 .UNSPECIFIED., .F., .F.,
 ( 4, 2, 4 ),
 ( 0.000000000000000000, 0.0003155923098472858596, 0.0006311846196945720446 ),
 .UNSPECIFIED. ) ;
#212130 = CARTESIAN_POINT ( 'NONE',  ( 0.7499999999999902300, 2.483333333333351156, 1.299038105676669330 ) ) ;
#212131 = CARTESIAN_POINT ( 'NONE',  ( 6.258078541936050065, 0.8512804341574469191, -2.052012918514530160 ) ) ;
#212132 = CARTESIAN_POINT ( 'NONE',  ( 4.628971764384363752, -2.004251508290517680, 0.8866568735110615940 ) ) ;
#212133 = CARTESIAN_POINT ( 'NONE',  ( -5.108724954250998707, 4.854600622914589714, -0.7998128361456221525 ) ) ;
#212134 = DIRECTION ( 'NONE',  ( -0.05872483221476459958, 0.000000000000000000, 0.9982742078614211811 ) ) ;
#212135 = CARTESIAN_POINT ( 'NONE',  ( 1.500000000000007105, 10.64264068711930733, 1.214306433183764966E-14 ) ) ;
#212136 = AXIS2_PLACEMENT_3D ( 'NONE', #128641, #162128, #93945 ) ;
#212137 = CARTESIAN_POINT ( 'NONE',  ( 1.364683531249988535, 3.863541667008087543, 0.7879004041258500513 ) ) ;
#212138 = CARTESIAN_POINT ( 'NONE',  ( -1.364683531250000748, 9.109375000341396245, 0.000000000000000000 ) ) ;
#212139 = CARTESIAN_POINT ( 'NONE',  ( -5.450014563013544588, 5.460697866378308341, 0.7216878364870317197 ) ) ;
#212140 = CARTESIAN_POINT ( 'NONE',  ( 5.748313822965784858, 1.043546352714582071, -1.845953426139717246 ) ) ;
#212141 = CARTESIAN_POINT ( 'NONE',  ( -4.638297949650955765, 8.425448351319163365, 0.7216878364870267237 ) ) ;
#212142 = ORIENTED_EDGE ( 'NONE', *, *, #206552, .F. ) ;
#212144 = CARTESIAN_POINT ( 'NONE',  ( 4.367922837034013739, 7.038290343739964428, 1.270857420505863367 ) ) ;
#212143 = CARTESIAN_POINT ( 'NONE',  ( -5.655159470675923394, 5.770309935309573923, 0.000000000000000000 ) ) ;
#212145 = CARTESIAN_POINT ( 'NONE',  ( 2.855963913973019963, 6.483708332943829866, 0.000000000000000000 ) ) ;
#212146 = CARTESIAN_POINT ( 'NONE',  ( 5.688959394570705541, 1.398425918548395153, 1.197878823674280779 ) ) ;
#212147 = CARTESIAN_POINT ( 'NONE',  ( 8.790438134619869004, 13.29428800202395955, -8.101059483297389008 ) ) ;
#212148 = CARTESIAN_POINT ( 'NONE',  ( 0.3110919644345279678, 6.477502264753364436, -3.270003019671252176 ) ) ;
#212149 = CARTESIAN_POINT ( 'NONE',  ( 0.6823417656249917140, 3.655208333674754506, 1.181850606188765695 ) ) ;
#212150 = CARTESIAN_POINT ( 'NONE',  ( 2.735604107484723269, 1.727544688213778601, 0.2106955661135938018 ) ) ;
#212151 = LINE ( 'NONE', #162372, #85745 ) ;
#212152 = CARTESIAN_POINT ( 'NONE',  ( 0.7500000000000006661, 10.94791666734946212, -1.299038105676657340 ) ) ;
#212153 = CARTESIAN_POINT ( 'NONE',  ( -1.402160292154681736E-14, 0.009375000341421267647, -1.575800808251665908 ) ) ;
#212154 = CARTESIAN_POINT ( 'NONE',  ( -1.499999999999961364, 7.000000000000000000, 10.64483442802188762 ) ) ;
#212155 = EDGE_CURVE ( 'NONE', #149263, #67541, #77608, .T. ) ;
#212156 = CARTESIAN_POINT ( 'NONE',  ( 6.579002408576895000, -0.1006694238701970334, -2.159482418181729813 ) ) ;
#212157 = CARTESIAN_POINT ( 'NONE',  ( -9.622536337397040285, 12.24937836509514710, 1.599625672291281386 ) ) ;
#212158 = TOROIDAL_SURFACE ( 'NONE', #28976, 1.749999999999999778, 0.5000000000000007772 ) ;
#212159 = CARTESIAN_POINT ( 'NONE',  ( -7.022760381754429737, 7.295567988242705582, 1.040834085586084257E-14 ) ) ;
#212160 = CARTESIAN_POINT ( 'NONE',  ( 5.471600609837615536, 2.084441204114939161, -0.5725544205837928002 ) ) ;
#212162 = ORIENTED_EDGE ( 'NONE', *, *, #97896, .F. ) ;
#212161 = CARTESIAN_POINT ( 'NONE',  ( -2.986538976760251263, 6.706322249520737522, -0.7998128361456481317 ) ) ;
#212163 = CARTESIAN_POINT ( 'NONE',  ( -1.364683531249997417, 3.759375000341423689, 1.214306433183764966E-14 ) ) ;
#212165 = EDGE_CURVE ( 'NONE', #6089, #108115, #84236, .T. ) ;
#212164 = CARTESIAN_POINT ( 'NONE',  ( 5.817641553194794035, -1.923906765362886961, 0.4292884390787749527 ) ) ;
#212166 = CARTESIAN_POINT ( 'NONE',  ( 4.745267847829638619, -1.681796892959321665, -0.4208994435666196798 ) ) ;
#212168 = CARTESIAN_POINT ( 'NONE',  ( 2.138457411672203712, 0.4836887423533155483, 2.137355272389021899 ) ) ;
#212167 = CARTESIAN_POINT ( 'NONE',  ( -1.360316468750009555, -0.1093749996585596795, -2.081668171172168513E-14 ) ) ;
#212169 = CARTESIAN_POINT ( 'NONE',  ( 3.610674682972123684, -0.9327887667434494601, -2.110822472020437601 ) ) ;
#212170 = CARTESIAN_POINT ( 'NONE',  ( 5.501267734246070518, 1.682208477397129975, 1.190076826167464352 ) ) ;
#212171 = CARTESIAN_POINT ( 'NONE',  ( 1.447104159573095572, 0.5638456037007446575, -1.858296221435972617 ) ) ;
#212172 = CARTESIAN_POINT ( 'NONE',  ( -6.114364089638801403, 8.156510742710487705, 1.443375672974078761 ) ) ;
#212173 = CARTESIAN_POINT ( 'NONE',  ( -3.467853430045390706, 7.267855778353407459, 0.7998128361456352531 ) ) ;
#212174 = CARTESIAN_POINT ( 'NONE',  ( -15.75000000000000000, 13.39999999999998259, 3.199999999999997957 ) ) ;
#212175 = CARTESIAN_POINT ( 'NONE',  ( 3.762070191281779774, 0.7111978290502696254, -1.997938288694045550 ) ) ;
#212176 = CARTESIAN_POINT ( 'NONE',  ( 2.110000207431836472, 0.002812218110825881467, 2.016597019944998959 ) ) ;
#212177 = CARTESIAN_POINT ( 'NONE',  ( -4.894130264408858899, 8.653643041878236630, -0.7216878364870207285 ) ) ;
#212178 = CARTESIAN_POINT ( 'NONE',  ( 4.964015014492747291, 2.183396446337606989, -0.3195234977587738667 ) ) ;
#212179 = CARTESIAN_POINT ( 'NONE',  ( -6.116136693540540570, 10.14959355252369910, 0.000000000000000000 ) ) ;
#212180 = CARTESIAN_POINT ( 'NONE',  ( -1.734723475976807094E-15, 2.999999999999988898, -6.938893903907228378E-15 ) ) ;
#212181 = CARTESIAN_POINT ( 'NONE',  ( 11.94105721237523277, 12.57259609010266921, -1.187919463087249827 ) ) ;
#212182 = CARTESIAN_POINT ( 'NONE',  ( -7.598418745816086783, 7.829519723065708092, 0.000000000000000000 ) ) ;
#212184 = CARTESIAN_POINT ( 'NONE',  ( 6.825078400183544503, 6.034152930826206962, 2.739236550662868197 ) ) ;
#212183 = CARTESIAN_POINT ( 'NONE',  ( -5.672142842012183550, 7.433492730264275927, 1.337035701138490351 ) ) ;
#212185 = CARTESIAN_POINT ( 'NONE',  ( 0.000000000000000000, 0.000000000000000000, 0.000000000000000000 ) ) ;
#212186 = VERTEX_POINT ( 'NONE', #202228 ) ;
#212187 = CARTESIAN_POINT ( 'NONE',  ( 3.959881651031765593, 2.045548025627259126, -0.2503382637644557263 ) ) ;
#212188 = CARTESIAN_POINT ( 'NONE',  ( 0.6801582343749987825, 2.557291667008069869, -1.178068619123886718 ) ) ;
#212189 = CARTESIAN_POINT ( 'NONE',  ( -3.680781672293562123E-15, -7.473374494045017080, 9.500331257164628340 ) ) ;
#212190 = CARTESIAN_POINT ( 'NONE',  ( -4.055860508782465068, 7.883587693554856557, 1.040834085586084257E-14 ) ) ;
#212191 = CARTESIAN_POINT ( 'NONE',  ( -6.168033539574333979, 6.160736982450306876, 0.7998128361456281477 ) ) ;
#212192 = CARTESIAN_POINT ( 'NONE',  ( 3.387372106552827944, 0.04729818973902254198, -2.019286085025721267 ) ) ;
#212193 = CARTESIAN_POINT ( 'NONE',  ( -1.500000000000001332, 1.400000000000019229, 0.000000000000000000 ) ) ;
#212194 = CARTESIAN_POINT ( 'NONE',  ( 2.184835310096557404, 5.700724961754617404, 1.040834085586084257E-14 ) ) ;
#212195 = CARTESIAN_POINT ( 'NONE',  ( 5.957918438201454059, 9.038323046955323292, -1.199719254218440723 ) ) ;
#212196 = CARTESIAN_POINT ( 'NONE',  ( 3.344654342685839499, 0.4992920947068257842, 1.999368073990233308 ) ) ;
#212197 = CARTESIAN_POINT ( 'NONE',  ( 3.024064729735044921, -1.777011313454954999, 0.9530116517338580451 ) ) ;
#212198 = DIRECTION ( 'NONE',  ( 0.000000000000000000, 0.000000000000000000, 1.000000000000000000 ) ) ;
#212199 = CARTESIAN_POINT ( 'NONE',  ( 5.840865249388943248, 5.708764300575555062, 0.7998128361456341429 ) ) ;
#212201 = ORIENTED_EDGE ( 'NONE', *, *, #23600, .T. ) ;
#212200 = CARTESIAN_POINT ( 'NONE',  ( -0.4886806171078718619, 7.337544960129616989, -1.941936010599534468 ) ) ;
#212202 = CARTESIAN_POINT ( 'NONE',  ( 1.376629057770164311, 1.701771572936720212, -0.7031625657484343872 ) ) ;
#212203 = ADVANCED_FACE ( 'NONE', ( #35480 ), #115728, .T. ) ;
#212204 = CARTESIAN_POINT ( 'NONE',  ( 6.674453038267287752, -1.361800985140369402, 1.737325302230605883 ) ) ;
#212205 = CARTESIAN_POINT ( 'NONE',  ( 4.875038752565570732, 7.845239757038595663, -1.199719254218452047 ) ) ;
#212206 = CARTESIAN_POINT ( 'NONE',  ( 2.811983876933337179, -2.138515761559431461, 0.3140893029918228607 ) ) ;
#212207 = CARTESIAN_POINT ( 'NONE',  ( -3.389175213736311587, 4.977123720824209840, 1.443375672974064550 ) ) ;
#212208 = CARTESIAN_POINT ( 'NONE',  ( 4.118443911689470660, 2.077242944681048975, 0.4093182092978660536 ) ) ;
#212209 = CARTESIAN_POINT ( 'NONE',  ( 5.378281411895256880, 4.339595938922573559, -2.499999999999995115 ) ) ;
#212210 = CONICAL_SURFACE ( 'NONE', #118902, 6.540947088288920241, 0.7853981633974536081 ) ;
#212211 = CARTESIAN_POINT ( 'NONE',  ( 0.9361565222895779081, 1.842281575443193375, 0.3236747858033904302 ) ) ;
#212212 = CARTESIAN_POINT ( 'NONE',  ( 4.364113771024707766, 0.9285358673545366370, 1.739096546318192882 ) ) ;
#212213 = CARTESIAN_POINT ( 'NONE',  ( 4.944546133779973651, -1.457238331152037825, 1.394083050251286870 ) ) ;
#212216 = EDGE_CURVE ( 'NONE', #78562, #185232, #18113, .T. ) ;
#212215 = LINE ( 'NONE', #101682, #29588 ) ;
#212214 = CARTESIAN_POINT ( 'NONE',  ( 1.364683531249990311, 3.384375000341416140, 1.214306433183764966E-14 ) ) ;
#212218 = CARTESIAN_POINT ( 'NONE',  ( 6.721333371289576419, -0.1616129481825591130, 2.070667135302119544 ) ) ;
#212217 = CARTESIAN_POINT ( 'NONE',  ( -6.901263884555985051, 8.010228272525461435, 1.199719254218450271 ) ) ;
#212219 = CIRCLE ( 'NONE', #181160, 0.07999999999999998779 ) ;
#212220 = CARTESIAN_POINT ( 'NONE',  ( 6.566853775770633561, 1.536883091774071453, -1.387433097640700774 ) ) ;
#212221 = CARTESIAN_POINT ( 'NONE',  ( 4.794779880727245036, 8.745660294157122649, -0.7998128361456281477 ) ) ;
#212222 = CARTESIAN_POINT ( 'NONE',  ( -6.684333426737305572, 7.757142738403693727, -1.199719254218446718 ) ) ;
#212224 = CARTESIAN_POINT ( 'NONE',  ( -1.537272393291634565, 8.756440202903029046, 2.479668406359612831 ) ) ;
#212223 = B_SPLINE_CURVE_WITH_KNOTS ( 'NONE', 3,
 ( #22573, #55101, #186145, #169903, #23649, #70248 ),
 .UNSPECIFIED., .F., .F.,
 ( 4, 2, 4 ),
 ( 0.000000000000000000, 0.0003172254002810707399, 0.0006344508005621414797 ),
 .UNSPECIFIED. ) ;
#212225 = CARTESIAN_POINT ( 'NONE',  ( 4.979350729014382360, 1.839849877434216241, -0.7087157093622028503 ) ) ;
#212226 = CARTESIAN_POINT ( 'NONE',  ( -0.2104748580754166598, -0.006608320950483163522, -2.103482951484026753 ) ) ;
#212227 = EDGE_CURVE ( 'NONE', #123208, #128754, #94376, .T. ) ;
#212228 = CARTESIAN_POINT ( 'NONE',  ( 0.7499999999999885647, -0.2354166659838466402, 1.299038105676657340 ) ) ;
#212229 = CARTESIAN_POINT ( 'NONE',  ( 5.092513741553108986, -2.289745732339975692, -0.2867506301261530388 ) ) ;
#212230 = CARTESIAN_POINT ( 'NONE',  ( 2.413000123442359701, -1.597275988187638607, 1.305004441579124208 ) ) ;
#212231 = CARTESIAN_POINT ( 'NONE',  ( 6.453317930424781856, 10.47269531889685545, -0.7216878364870267237 ) ) ;
#212233 = CARTESIAN_POINT ( 'NONE',  ( 6.150558962454855561, 7.204682206732687000, 1.199719254218452047 ) ) ;
#212232 = AXIS2_PLACEMENT_3D ( 'NONE', #13313, #180094, #81522 ) ;
#212234 = CARTESIAN_POINT ( 'NONE',  ( 5.585032934186686226, 5.480569609498057382, 0.000000000000000000 ) ) ;
#212235 = CARTESIAN_POINT ( 'NONE',  ( 0.6823417656249882723, 1.738541667008083991, -1.181850606188749264 ) ) ;
#212236 = CARTESIAN_POINT ( 'NONE',  ( 4.740510986633625024, 5.559626234941203116, -1.199719254218450271 ) ) ;
#212237 = CARTESIAN_POINT ( 'NONE',  ( 7.904040366642699489, 8.323727970612377902, 0.7216878364870458196 ) ) ;
#212238 = CARTESIAN_POINT ( 'NONE',  ( 4.070888617658403597, 1.538033944094893579, -1.532718761138168517 ) ) ;
#212239 = CARTESIAN_POINT ( 'NONE',  ( -1.297773248481477681, -0.8887487162373152172, -3.026232207781772932 ) ) ;
#212241 = CARTESIAN_POINT ( 'NONE',  ( 2.999365392321148516, -1.839032331094083927, 0.09308366406014097205 ) ) ;
#212240 = CARTESIAN_POINT ( 'NONE',  ( -3.416291520963659512, 5.969128626890772615, 1.082531754730560403 ) ) ;
#212242 = CARTESIAN_POINT ( 'NONE',  ( -1.001543065824772872E-14, 4.821875000341419693, 1.575800808251672791 ) ) ;
#212243 = CARTESIAN_POINT ( 'NONE',  ( 5.724229345562060089, 2.111793275502030554, 0.5857118945327836057 ) ) ;
#212244 = CARTESIAN_POINT ( 'NONE',  ( 9.858406733136194415E-16, 1.000000000000000888, -8.050000000000000711 ) ) ;
#212245 = CARTESIAN_POINT ( 'NONE',  ( 6.157125652023562878, -1.936745554134344349, -1.169425401991762259 ) ) ;
#212246 = CARTESIAN_POINT ( 'NONE',  ( -5.391520587109122076, 6.494678753518896563, -1.342800935913717852 ) ) ;
#212247 = CARTESIAN_POINT ( 'NONE',  ( 4.941988244637107286, 8.095350367992509177, 1.064974588601754757 ) ) ;
#212248 = CARTESIAN_POINT ( 'NONE',  ( -4.448483798615272100, 8.203998508444197313, 0.000000000000000000 ) ) ;
#212249 = CARTESIAN_POINT ( 'NONE',  ( -7.004500933659075557, -6.920331743269713343, -7.004500933659044470 ) ) ;
#212250 = CARTESIAN_POINT ( 'NONE',  ( 6.098865926757823352, 1.445600302716108843, -1.020594415802724919 ) ) ;
#212251 = CARTESIAN_POINT ( 'NONE',  ( 4.652993947568984545, 0.3464272572618365964, 1.982917695270119518 ) ) ;
#212252 = CARTESIAN_POINT ( 'NONE',  ( 5.900823170445728572, 7.907379670318584353, 1.599625672291267398 ) ) ;
#212253 = CARTESIAN_POINT ( 'NONE',  ( 3.504997884693922483, 1.661208405451128245, -1.294291292614203170 ) ) ;
#212254 = CARTESIAN_POINT ( 'NONE',  ( 2.372541684819210683, -0.3298082299327957378, -1.886833909188085912 ) ) ;
#212255 = CARTESIAN_POINT ( 'NONE',  ( 4.630273154266905777, 5.360739087188218122, 1.199719254218464037 ) ) ;
#212256 = CARTESIAN_POINT ( 'NONE',  ( 2.857809274136946520, -0.6206004443085939570, 1.869272957157315007 ) ) ;
#212257 = CARTESIAN_POINT ( 'NONE',  ( 1.182252951876180180, -1.824241171369020531, -0.4133900166373091767 ) ) ;
#212258 = CARTESIAN_POINT ( 'NONE',  ( 1.767943819387544968, -1.947426213878332035, 0.2369139692007388165 ) ) ;
#212261 = ORIENTED_EDGE ( 'NONE', *, *, #169187, .T. ) ;
#212260 = CARTESIAN_POINT ( 'NONE',  ( 0.8086807686161383568, -0.4671638426185490967, -1.854305266343849734 ) ) ;
#212259 = CARTESIAN_POINT ( 'NONE',  ( 4.142953665201137170, -1.499297852604332348, 0.8526725997853346062 ) ) ;
#212263 = CARTESIAN_POINT ( 'NONE',  ( 6.155038550924155416, 6.283225852274053835, 0.7216878364870317197 ) ) ;
#212262 = CARTESIAN_POINT ( 'NONE',  ( 1.752831059180045115, 0.6944836804415283060, 2.094827981560241970 ) ) ;
#212264 = CARTESIAN_POINT ( 'NONE',  ( -1.201851678989727383E-14, 1.384375000341419693, 1.575800808251672791 ) ) ;
#212265 = CARTESIAN_POINT ( 'NONE',  ( 11.44779963594988637, 12.70000000000000107, -3.600000000000000977 ) ) ;
#212266 = DIRECTION ( 'NONE',  ( -0.000000000000000000, -1.000000000000000000, -0.000000000000000000 ) ) ;
#212267 = CARTESIAN_POINT ( 'NONE',  ( 2.310781476690497271, 5.467761476598782977, -0.5169845646830224517 ) ) ;
#212268 = CARTESIAN_POINT ( 'NONE',  ( 6.368043163206878354, -2.055323469740528264, 0.2474699835256082281 ) ) ;
#212269 = CARTESIAN_POINT ( 'NONE',  ( 0.8716356842100521085, -0.3054578492302991721, 2.047597563663336118 ) ) ;
#212270 = CARTESIAN_POINT ( 'NONE',  ( -0.7500000000000215383, 2.191666666666689078, 1.299038105676671107 ) ) ;
#212271 = CARTESIAN_POINT ( 'NONE',  ( 6.479907352327590964, 9.647310113435821677, 1.199719254218462483 ) ) ;
#212272 = CARTESIAN_POINT ( 'NONE',  ( -7.666245793523398078, 11.03137162816423356, 1.199719254218453823 ) ) ;
#212273 = CARTESIAN_POINT ( 'NONE',  ( 5.903649544107831382, 5.852288987739402870, -0.7998128361456481317 ) ) ;
#212274 = CARTESIAN_POINT ( 'NONE',  ( 5.567072742743464531, -1.671543079161823542, 1.304629437388994395 ) ) ;
#212275 = CARTESIAN_POINT ( 'NONE',  ( 3.088225128862704949, 6.824956093640315302, 0.7998128361456281477 ) ) ;
#212276 = CARTESIAN_POINT ( 'NONE',  ( -1.364683531250012516, 2.530208333674753174, 0.7879004041258379498 ) ) ;
#212277 = EDGE_LOOP ( 'NONE', ( #197663, #29224 ) ) ;
#212278 = CARTESIAN_POINT ( 'NONE',  ( 1.499999999999987121, 2.295833333333350268, -0.8660254037844262731 ) ) ;
#212280 = CARTESIAN_POINT ( 'NONE',  ( 2.361091307074211887, 5.906356958228550447, 0.7998128361456462443 ) ) ;
#212279 = CARTESIAN_POINT ( 'NONE',  ( 6.602011099637477010, 0.7519813002578833450, -1.812223124677159181 ) ) ;
#212281 = CARTESIAN_POINT ( 'NONE',  ( 3.989611116449209405, 1.913510565032714883, 0.6351021849077125303 ) ) ;
#212282 = CARTESIAN_POINT ( 'NONE',  ( 3.485460621946351534, -0.5511008185722067187, 1.834767741543178676 ) ) ;
#212283 = CYLINDRICAL_SURFACE ( 'NONE', #114154, 1.250000000000000000 ) ;
#212284 = CARTESIAN_POINT ( 'NONE',  ( 1.171705676731093604, 1.309414992938146893, 1.757219779060022580 ) ) ;
#212285 = CARTESIAN_POINT ( 'NONE',  ( -1.919771823249095455, 3.227545531266399870, 0.3999999999999835909 ) ) ;
#212286 = CARTESIAN_POINT ( 'NONE',  ( 1.499999999999987121, 1.327083334016149641, -0.8660254037844253849 ) ) ;
#212287 = CARTESIAN_POINT ( 'NONE',  ( 5.677995041854309477, 1.982684118255732875, -0.3484467016405675688 ) ) ;
#212288 = APPLICATION_CONTEXT ( 'automotive_design' ) ;
#212289 = CARTESIAN_POINT ( 'NONE',  ( -7.217017841176048165, 7.314275657660511243, 1.040834085586084257E-14 ) ) ;
#212291 = CARTESIAN_POINT ( 'NONE',  ( 5.993796379919574591, -2.101200072677239739, 0.2596931833054038630 ) ) ;
#212290 = CARTESIAN_POINT ( 'NONE',  ( -3.795919822146283540, 6.412028311603867436, -1.082531754730549967 ) ) ;
#212293 = EDGE_CURVE ( 'NONE', #9995, #187611, #124003, .T. ) ;
#212292 = CARTESIAN_POINT ( 'NONE',  ( -0.6823417656250003738, 8.713541667008065872, 1.181850606188754593 ) ) ;
#212295 = CARTESIAN_POINT ( 'NONE',  ( -6.084577077482911101, 10.32070003369722144, 0.000000000000000000 ) ) ;
#212294 = CARTESIAN_POINT ( 'NONE',  ( 1.909825778081200909, -0.9882315549833411428, -1.842464674945838654 ) ) ;
#212297 = VERTEX_POINT ( 'NONE', #207583 ) ;
#212296 = CARTESIAN_POINT ( 'NONE',  ( 0.8501349688851227437, 0.4944664728778884744, 1.652377535151504206 ) ) ;
#212298 = CARTESIAN_POINT ( 'NONE',  ( 6.799577732453452761, 7.891594428405881878, -1.199719254218446718 ) ) ;
#212299 = CYLINDRICAL_SURFACE ( 'NONE', #186476, 1.500000000000000222 ) ;
#212300 = FILL_AREA_STYLE_COLOUR ( '', #164480 ) ;
#212302 = CARTESIAN_POINT ( 'NONE',  ( 8.636180661780656465, 11.09863007687603087, -1.443375672974052559 ) ) ;
#212301 = CARTESIAN_POINT ( 'NONE',  ( 5.608269097547198712, 9.694731047113750222, -0.7998128361456281477 ) ) ;
#212303 = ORIENTED_EDGE ( 'NONE', *, *, #11240, .F. ) ;
#212304 = CARTESIAN_POINT ( 'NONE',  ( 9.000007961041747606, 1.000000000000000888, 7.937244906211794238 ) ) ;
#212306 = CARTESIAN_POINT ( 'NONE',  ( 1.892921280605066370, -0.08938092231483388272, -1.809401395368259280 ) ) ;
#212305 = CARTESIAN_POINT ( 'NONE',  ( 4.342354338126830804, 8.288106837781779035, -0.7998128361456381397 ) ) ;
#212307 = CARTESIAN_POINT ( 'NONE',  ( -6.449928391799210736, 8.548002428564306143, -1.599625672291263179 ) ) ;
#212308 = CARTESIAN_POINT ( 'NONE',  ( 4.843287188579786573, 6.673587691474970107, -1.599625672291256295 ) ) ;
#212309 = CARTESIAN_POINT ( 'NONE',  ( 4.538947565524982686, 8.517465603079630299, 0.000000000000000000 ) ) ;
#212310 = CARTESIAN_POINT ( 'NONE',  ( 6.539320575229251808, 2.472926584938171413, 2.181659282373017650 ) ) ;
#212311 = DIRECTION ( 'NONE',  ( 1.000000000000000000, -0.000000000000000000, -0.000000000000000000 ) ) ;
#212312 = CARTESIAN_POINT ( 'NONE',  ( 4.084722907606431974, 7.479936734012107458, 0.5927516458891276541 ) ) ;
#212313 = CARTESIAN_POINT ( 'NONE',  ( 9.408995418203963013, 12.00024729270324286, 1.443375672974076540 ) ) ;
#212314 = CARTESIAN_POINT ( 'NONE',  ( 3.332308176975990577, -1.110599006344037853, 1.493168399320473627 ) ) ;
#212315 = CARTESIAN_POINT ( 'NONE',  ( 0.01699859406821546334, -1.751214827781864436, 0.7768474416505846136 ) ) ;
#212316 = CARTESIAN_POINT ( 'NONE',  ( 6.668979838189343035, -1.761623494860217631, -0.7799453142821392015 ) ) ;
#212317 = CARTESIAN_POINT ( 'NONE',  ( 11.41381675112453387, 10.89999999999998259, 3.704697986577180746 ) ) ;
#212318 = CARTESIAN_POINT ( 'NONE',  ( 0.000000000000000000, 4.500000000000003553, 0.000000000000000000 ) ) ;
#212319 = CARTESIAN_POINT ( 'NONE',  ( 4.614363445337835934, 8.349151705029461468, -0.2795175495247017583 ) ) ;
#212320 = FILL_AREA_STYLE_COLOUR ( '', #15689 ) ;
#212321 = CARTESIAN_POINT ( 'NONE',  ( -3.850152436600983386, 4.554561266531622188, 1.082531754730560403 ) ) ;
#212322 = CARTESIAN_POINT ( 'NONE',  ( 9.097157885089661278, 9.715698408800516717, 1.040834085586084257E-14 ) ) ;
#212323 = CARTESIAN_POINT ( 'NONE',  ( 4.838697515689712958, -1.909247481386136647, -0.4825833779809485802 ) ) ;
#212324 = CARTESIAN_POINT ( 'NONE',  ( -3.903858165731105778, 6.641919395739846799, 1.199719254218464037 ) ) ;
#212325 = CARTESIAN_POINT ( 'NONE',  ( 0.000000000000000000, 0.9330127018934565308, 10.99999999999752553 ) ) ;
#212326 = CARTESIAN_POINT ( 'NONE',  ( 6.938893903907228378E-15, 10.64264068711930733, 1.214306433183764966E-14 ) ) ;
#212327 = CARTESIAN_POINT ( 'NONE',  ( 6.527279143455773536, -1.428284688129980440, -1.662137905815167294 ) ) ;
#212328 = DIRECTION ( 'NONE',  ( 1.000000000000000000, 0.000000000000000000, -0.000000000000000000 ) ) ;
#212329 = CARTESIAN_POINT ( 'NONE',  ( 5.333004766823168374, 0.1418691241366967226, 1.921211455432366044 ) ) ;
#212330 = CARTESIAN_POINT ( 'NONE',  ( -5.506582945444718824, 9.576097202994168001, 0.7998128361456481317 ) ) ;
#212331 = ADVANCED_FACE ( 'NONE', ( #169756 ), #73310, .F. ) ;
#212332 = CARTESIAN_POINT ( 'NONE',  ( 0.5514207423844892375, 0.5776932562693118944, -1.731835939664846613 ) ) ;
#212333 = CARTESIAN_POINT ( 'NONE',  ( 1.893488989520499377, 1.919108310403025763, -1.089527612406354873 ) ) ;
#212334 = CARTESIAN_POINT ( 'NONE',  ( -6.100232733750003078, 7.025055339219893114, 0.9836300112023097508 ) ) ;
#212335 = CARTESIAN_POINT ( 'NONE',  ( 0.3340484552533556362, -1.024938778295768849, -1.614363347046356756 ) ) ;
#212336 = EDGE_LOOP ( 'NONE', ( #11194, #93857, #212754, #132188 ) ) ;
#212337 = ORIENTED_EDGE ( 'NONE', *, *, #178838, .F. ) ;
#212338 = CARTESIAN_POINT ( 'NONE',  ( 0.9066264771708797410, 0.5685364763899096729, 1.885722953041415906 ) ) ;
#212339 = CARTESIAN_POINT ( 'NONE',  ( 1.575622484978753679, -1.037422314974449478, 1.641571771860099727 ) ) ;
#212340 = CARTESIAN_POINT ( 'NONE',  ( 0.5267199648841465187, 1.994564833640038781, -0.2930222482238133419 ) ) ;
#212342 = CARTESIAN_POINT ( 'NONE',  ( 5.717585430250381684, 0.3647202891138579539, -1.824662122815931875 ) ) ;
#212341 = CARTESIAN_POINT ( 'NONE',  ( -4.444040490229335560, 8.406740681901359480, 0.7998128361456352531 ) ) ;
#212343 = CARTESIAN_POINT ( 'NONE',  ( 4.701645408888975197, 8.707279753670952971, 0.000000000000000000 ) ) ;
#212344 = LINE ( 'NONE', #82351, #84733 ) ;
#212345 = CARTESIAN_POINT ( 'NONE',  ( 1.499999999999820810, 7.388542872122566330, -4.154462424328214887 ) ) ;
#212346 = CARTESIAN_POINT ( 'NONE',  ( -6.663996196316808174, 7.733415969579778171, -1.199719254218446718 ) ) ;
#212347 = CARTESIAN_POINT ( 'NONE',  ( -6.129167961829681488, 9.308390501180058507, -1.199719254218452047 ) ) ;
#212348 = CARTESIAN_POINT ( 'NONE',  ( 1.206853476500208133, 1.935082376036290075, 1.028754739392373496 ) ) ;
#212349 = CARTESIAN_POINT ( 'NONE',  ( 3.877268743828276243, 4.586196958296845594, 1.082531754730560403 ) ) ;
#212350 = ORIENTED_EDGE ( 'NONE', *, *, #51590, .F. ) ;
#212351 = CARTESIAN_POINT ( 'NONE',  ( 0.3544712801348727238, 3.975028838742718840, -0.9637995819944527032 ) ) ;
#212352 = SURFACE_STYLE_FILL_AREA ( #94385 ) ;
#212353 = CARTESIAN_POINT ( 'NONE',  ( 1.558932953716257730, -1.564965500463588732, -0.9399777662534372080 ) ) ;
#212354 = CARTESIAN_POINT ( 'NONE',  ( -2.300079615812729905, 5.835176651756807331, -0.7998128361456281477 ) ) ;
#212355 = CARTESIAN_POINT ( 'NONE',  ( -0.09935801671627322862, 2.598252772099167274, -1.999773316424213965 ) ) ;
#212356 = CARTESIAN_POINT ( 'NONE',  ( 6.509000000000021657, 1.267728212239338959, 2.115804336118334295 ) ) ;
#212357 = CARTESIAN_POINT ( 'NONE',  ( 10.53876547652418338, 11.18964789890005918, 0.7998128361456462443 ) ) ;
#212358 = CARTESIAN_POINT ( 'NONE',  ( 0.2758378062712996681, 1.107980625233648597, 1.575821400459100463 ) ) ;
#212359 = CARTESIAN_POINT ( 'NONE',  ( 4.258614474744500278, -0.6113484564182982695, -1.864166799412938724 ) ) ;
#212360 = CARTESIAN_POINT ( 'NONE',  ( -8.178592977541617515, 10.56477777859713463, 1.599625672291295375 ) ) ;
#212361 = CARTESIAN_POINT ( 'NONE',  ( 4.964256800898067645, 8.943383367689749619, 0.7998128361456462443 ) ) ;
#212362 = CARTESIAN_POINT ( 'NONE',  ( 4.036819321710017228, -1.906298169312226953, 1.081085072550565407 ) ) ;
#212363 = COLOUR_RGB ( '', 0.31764706, 0.68627451, 0.89019608) ;
#212364 = CARTESIAN_POINT ( 'NONE',  ( 6.609000000000012420, 2.052634316153336691, 2.306727925381938604 ) ) ;
#212365 = CARTESIAN_POINT ( 'NONE',  ( 3.713788242813487184, 0.5077267127921447631, -2.006887321594638784 ) ) ;
#212367 = CARTESIAN_POINT ( 'NONE',  ( -0.6823417656250003738, 1.280208333674752508, -1.181850606188749264 ) ) ;
#212366 = FACE_OUTER_BOUND ( 'NONE', #30607, .T. ) ;
#212369 = ORIENTED_EDGE ( 'NONE', *, *, #2823, .F. ) ;
#212368 = AXIS2_PLACEMENT_3D ( 'NONE', #196571, #112193, #80693 ) ;
#212370 = CARTESIAN_POINT ( 'NONE',  ( 4.131641605347593504, 0.6128431504758731219, 2.215418681923121191 ) ) ;
#212371 = CARTESIAN_POINT ( 'NONE',  ( 6.914295153289432783, 10.05013286460426691, -1.082531754730537976 ) ) ;
#212373 = CARTESIAN_POINT ( 'NONE',  ( -9.512045263456270661, -8.176568542494905500, 0.4655551865852137206 ) ) ;
#212372 = CARTESIAN_POINT ( 'NONE',  ( 6.861835142292147083, 7.178098218861903135, 0.7216878364870328300 ) ) ;
#212374 = CARTESIAN_POINT ( 'NONE',  ( 6.720655732516653380, 6.038084619979597001, 2.521169617733058477 ) ) ;
#212375 = B_SPLINE_CURVE_WITH_KNOTS ( 'NONE', 3,
 ( #26073, #190700, #158236, #9826 ),
 .UNSPECIFIED., .F., .F.,
 ( 4, 4 ),
 ( 0.0005671806269306270149, 0.0008743016172331019402 ),
 .UNSPECIFIED. ) ;
#212376 = CARTESIAN_POINT ( 'NONE',  ( -6.050681693448748177, 10.28115541899069463, 0.7998128361456291469 ) ) ;
#212377 = CARTESIAN_POINT ( 'NONE',  ( 4.206929537583108392, -0.3307808895044571651, 1.913420690662092305 ) ) ;
#212378 = ORIENTED_EDGE ( 'NONE', *, *, #213932, .T. ) ;
#212379 = CARTESIAN_POINT ( 'NONE',  ( 10.50720586046655391, 11.36075438007358507, 0.7216878364870438212 ) ) ;
#212380 = CARTESIAN_POINT ( 'NONE',  ( 4.711142613322857109, 1.586760866459841379, -1.067142987418716604 ) ) ;
#212381 = CARTESIAN_POINT ( 'NONE',  ( 11.92619526913699879, 19.00000000000000000, 1.328859060402684644 ) ) ;
#212382 = CARTESIAN_POINT ( 'NONE',  ( 5.702095886272589453, -1.724958192454665085, 0.004281591079305368218 ) ) ;
#212383 = CARTESIAN_POINT ( 'NONE',  ( 4.821500071095637274, -1.429446227384461032, -1.422610148874188463 ) ) ;
#212384 = CARTESIAN_POINT ( 'NONE',  ( 4.799617249347348569, 1.585997580420713593, -1.664126067976256840 ) ) ;
#212385 = CARTESIAN_POINT ( 'NONE',  ( -0.4019237886466802689, 9.698664549684631098, -1.500000000000002887 ) ) ;
#212386 = CARTESIAN_POINT ( 'NONE',  ( 1.207977004800918852, -0.5332226995428279714, 2.141375170867452660 ) ) ;
#212388 = CARTESIAN_POINT ( 'NONE',  ( -4.990809943606286048, 5.955604701363006015, -1.082531754730549967 ) ) ;
#212387 = CARTESIAN_POINT ( 'NONE',  ( -3.846355548915592504, 7.490793684076796133, -0.1425745578392398905 ) ) ;
#212389 = CARTESIAN_POINT ( 'NONE',  ( 6.239478240350173621, -1.283343308616216705, -1.218829697195593642 ) ) ;
#212391 = CARTESIAN_POINT ( 'NONE',  ( 2.467065147740226116, 0.1108469335737295169, -2.289696780367215467 ) ) ;
#212390 = CARTESIAN_POINT ( 'NONE',  ( 5.027041095616958444, 9.086908054853605421, 0.000000000000000000 ) ) ;
#212392 = CARTESIAN_POINT ( 'NONE',  ( 1.358879374581365429, 1.715036991836488056, -0.2946001921160408821 ) ) ;
#212393 = CYLINDRICAL_SURFACE ( 'NONE', #14158, 1.250000000000000000 ) ;
#212394 = CARTESIAN_POINT ( 'NONE',  ( 0.9304778391672563487, 0.8475688526466665929, 1.512457944649912012 ) ) ;
#212395 = CARTESIAN_POINT ( 'NONE',  ( 1.360316468749980023, 0.7968750003414099004, -3.122502256758252770E-14 ) ) ;
#212396 = CARTESIAN_POINT ( 'NONE',  ( 5.553597010146855695, 5.912075037831448832, 0.6282849591137803502 ) ) ;
#212397 =( BOUNDED_CURVE ( )  B_SPLINE_CURVE ( 2, ( #180283, #96924, #145692, #44967, #97983, #165090, #197577, #162974, #64395 ),
 .UNSPECIFIED., .F., .T. ) 
 B_SPLINE_CURVE_WITH_KNOTS ( ( 3, 2, 2, 2, 3 ),
 ( 0.6093749999999997780, 0.6145833333333333703, 0.6250000000000000000, 0.6354166666666666297, 0.6406250000000002220 ),
 .UNSPECIFIED. ) 
 CURVE ( )  GEOMETRIC_REPRESENTATION_ITEM ( )  RATIONAL_B_SPLINE_CURVE ( ( 0.9330127018922194093, 0.9330127018922165227, 1.000000000000000000, 0.8660254037844387076, 1.000000000000000000, 0.8660254037844387076, 1.000000000000000000, 0.9330127018922165227, 0.9330127018922194093 ) ) 
 REPRESENTATION_ITEM ( '' )  );
#212398 = CARTESIAN_POINT ( 'NONE',  ( 0.9772844579341716242, 2.006041157791297991, 0.8309993691856133458 ) ) ;
#212399 = CARTESIAN_POINT ( 'NONE',  ( 2.694546298722868549, 1.457235452327232395, -1.394086077981852911 ) ) ;
#212400 = CARTESIAN_POINT ( 'NONE',  ( -0.7500000000000006661, 2.139583334016155636, -1.299038105676652011 ) ) ;
#212401 = CARTESIAN_POINT ( 'NONE',  ( 6.533821582689818719, -1.260454884444404122, -1.457021811732343686 ) ) ;
#212402 = CARTESIAN_POINT ( 'NONE',  ( 1.364683531250000303, 13.50520833367472839, -0.7879004041258355073 ) ) ;
#212403 = CARTESIAN_POINT ( 'NONE',  ( 2.619623270456972630, 1.879045213996872965, 1.184562869268386054 ) ) ;
#212404 = ORIENTED_EDGE ( 'NONE', *, *, #203566, .T. ) ;
#212405 = DIRECTION ( 'NONE',  ( 0.000000000000000000, -0.000000000000000000, 1.000000000000000000 ) ) ;
#212406 = FILL_AREA_STYLE ('',( #109678 ) ) ;
#212407 = CARTESIAN_POINT ( 'NONE',  ( 9.562578416340237197, 10.05076299535211781, 0.7998128361456462443 ) ) ;
#212408 = PRESENTATION_STYLE_ASSIGNMENT (( #131246 ) ) ;
#212409 = EDGE_CURVE ( 'NONE', #132613, #1738, #120590, .T. ) ;
#212410 = CARTESIAN_POINT ( 'NONE',  ( 5.636210787324313465, 0.3477544615747550361, 1.705165986005853229 ) ) ;
#212411 = CARTESIAN_POINT ( 'NONE',  ( 3.226955236329264398, -1.811681696138227160, -0.7532884077038405346 ) ) ;
#212413 = CARTESIAN_POINT ( 'NONE',  ( -6.399085315970142851, 8.488685506763726352, -1.443375672974059665 ) ) ;
#212412 = CARTESIAN_POINT ( 'NONE',  ( 4.708759422647839976, 4.387974169377582001, -0.7998128361456211532 ) ) ;
#212414 = EDGE_CURVE ( 'NONE', #11502, #145411, #203505, .T. ) ;
#212415 = CARTESIAN_POINT ( 'NONE',  ( 6.777182134110200096, 7.629137130509069387, 2.789055895399249696 ) ) ;
#212416 = CARTESIAN_POINT ( 'NONE',  ( 4.112777665030871610, 1.603588310063062794, -1.596181346845012117 ) ) ;
#212417 = CARTESIAN_POINT ( 'NONE',  ( 0.5376419320063254847, 1.925266156408891316, -0.7407299734314594097 ) ) ;
#212418 = CARTESIAN_POINT ( 'NONE',  ( -7.528855374290365887, 7.678086112960552434, -0.7998128361456291469 ) ) ;
#212419 = VECTOR ( 'NONE', #184231, 1000.000000000000000 ) ;
#212420 = CARTESIAN_POINT ( 'NONE',  ( 2.079355054740182229, -0.1115493103639639688, -2.259872350005930119 ) ) ;
#212421 = VERTEX_POINT ( 'NONE', #23494 ) ;
#212422 = CARTESIAN_POINT ( 'NONE',  ( -1.201851678989727383E-14, 0.7437500006828187127, 1.732050807568877637 ) ) ;
#212423 = CARTESIAN_POINT ( 'NONE',  ( 3.075316773429651818, 1.777364689479765003, -0.5833007003755164011 ) ) ;
#212424 = CARTESIAN_POINT ( 'NONE',  ( 1.951430075251599838, -1.585913025431864742, -0.7019457847057923860 ) ) ;
#212425 = CARTESIAN_POINT ( 'NONE',  ( 5.917560222199001352, -1.216239291071326001, -1.822900893127032962 ) ) ;
#212426 = CARTESIAN_POINT ( 'NONE',  ( 0.08333923026508995024, -0.1592477204843331384, -2.171661519566956855 ) ) ;
#212427 = CARTESIAN_POINT ( 'NONE',  ( 4.364260218091946975, 1.016419123106377276, 1.907829002176253175 ) ) ;
#212428 = CARTESIAN_POINT ( 'NONE',  ( 4.312401332534675724, 1.776009277829879718, 0.7858599780834804038 ) ) ;
#212429 = CARTESIAN_POINT ( 'NONE',  ( -2.277406616971334508, 5.600798786534425311, 1.040834085586084257E-14 ) ) ;
#212430 = EDGE_CURVE ( 'NONE', #170100, #125304, #140793, .T. ) ;
#212431 = CYLINDRICAL_SURFACE ( 'NONE', #149946, 0.09999999999999982514 ) ;
#212432 = CARTESIAN_POINT ( 'NONE',  ( 2.000000000000001332, -1.212302805901314492E-13, -2.052068128417949389 ) ) ;
#212433 = CARTESIAN_POINT ( 'NONE',  ( 4.863282293121215183, 6.691362709583676072, 1.250037515303052738 ) ) ;
#212434 = DIRECTION ( 'NONE',  ( -0.000000000000000000, 1.000000000000000000, -0.000000000000000000 ) ) ;
#212435 = CARTESIAN_POINT ( 'NONE',  ( 11.86145016429273191, 12.69999999999999929, 1.099999999999996758 ) ) ;
#212436 = CARTESIAN_POINT ( 'NONE',  ( -2.353626204688216217E-14, 2.828125000341407347, -1.570758158831798257 ) ) ;
#212437 = CARTESIAN_POINT ( 'NONE',  ( 5.555314621531947772, -1.277044735018734833, 1.560499014526220307 ) ) ;
#212438 = CARTESIAN_POINT ( 'NONE',  ( -9.938290294017125603, 11.55342575023019691, -1.199719254218441611 ) ) ;
#212439 = CARTESIAN_POINT ( 'NONE',  ( 7.527801604085637699, 9.805521176231838609, 1.599625672291281386 ) ) ;
#212440 = CARTESIAN_POINT ( 'NONE',  ( 5.029711800989886683, 4.970344644017389513, 1.040834085586084257E-14 ) ) ;
#212442 = CARTESIAN_POINT ( 'NONE',  ( -6.796618584846395805, -7.026643280347676601, 6.776593369754376539 ) ) ;
#212441 = CARTESIAN_POINT ( 'NONE',  ( 3.791466046568803705, 1.323482414808102137, 1.257835202898072380 ) ) ;
#212443 = CARTESIAN_POINT ( 'NONE',  ( 1.811274280335458453, -3.469446951953614189E-15, 0.2936757779752607878 ) ) ;
#212444 = ORIENTED_EDGE ( 'NONE', *, *, #194283, .T. ) ;
#212445 = CARTESIAN_POINT ( 'NONE',  ( -4.109529958273628658, 7.808552361378938045, 0.7216878364870338292 ) ) ;
#212446 = CARTESIAN_POINT ( 'NONE',  ( -1.642778471875000035, -4.105208332855374564, -2.845375778867859751 ) ) ;
#212447 = CARTESIAN_POINT ( 'NONE',  ( -9.643927338022246332, 10.14567007064778004, -0.7998128361456291469 ) ) ;
#212448 = CARTESIAN_POINT ( 'NONE',  ( 0.1760434994887878080, 1.997199259934297366, -0.3004917578056826022 ) ) ;
#212449 = CARTESIAN_POINT ( 'NONE',  ( 0.6277789859737945566, -0.3070864893036719945, 2.098006834332386994 ) ) ;
#212450 = VERTEX_POINT ( 'NONE', #56015 ) ;
#212451 = CARTESIAN_POINT ( 'NONE',  ( -4.111865726694519552, 8.019203457777400956, 0.000000000000000000 ) ) ;
#212452 = CARTESIAN_POINT ( 'NONE',  ( 3.032219910950674890, 6.689340329417765574, 0.7998128361456321445 ) ) ;
#212453 = CARTESIAN_POINT ( 'NONE',  ( 6.825078400183568483, -0.002763825414428457399, 2.044262525762724270 ) ) ;
#212454 = CARTESIAN_POINT ( 'NONE',  ( 5.854138739207011888, 0.1455364397412381439, -2.011204036175239018 ) ) ;
#212455 = ORIENTED_EDGE ( 'NONE', *, *, #18034, .F. ) ;
#212456 = CARTESIAN_POINT ( 'NONE',  ( -8.622095623286845978, 12.14652976288826913, 1.199719254218462483 ) ) ;
#212457 = CARTESIAN_POINT ( 'NONE',  ( 7.614839552730775729, 8.913009562054615031, 1.199719254218452047 ) ) ;
#212458 =( BOUNDED_CURVE ( )  B_SPLINE_CURVE ( 2, ( #147518, #65162, #182113, #12162, #30571 ),
 .UNSPECIFIED., .F., .T. ) 
 B_SPLINE_CURVE_WITH_KNOTS ( ( 3, 2, 3 ),
 ( 0.2465812307583980512, 0.2500000000000000000, 0.2539810465305627485 ),
 .UNSPECIFIED. ) 
 CURVE ( )  GEOMETRIC_REPRESENTATION_ITEM ( )  RATIONAL_B_SPLINE_CURVE ( ( 0.9351709383301824996, 0.9450366125562636999, 1.000000000000000000, 0.9359969078262996289, 0.9331456447830145384 ) ) 
 REPRESENTATION_ITEM ( '' )  );
#212461 = ORIENTED_EDGE ( 'NONE', *, *, #87337, .T. ) ;
#212460 = CARTESIAN_POINT ( 'NONE',  ( 0.07680821025391781909, 4.096870002413341538, -2.365840309731046975 ) ) ;
#212459 = CARTESIAN_POINT ( 'NONE',  ( -6.303615075710993665, 6.318915441276411471, -0.7998128361456362523 ) ) ;
#212462 = CARTESIAN_POINT ( 'NONE',  ( 5.652821694808577213, 7.451312062667313718, 1.328372732707931103 ) ) ;
#212463 = B_SPLINE_CURVE_WITH_KNOTS ( 'NONE', 3,
 ( #7653, #188550, #90010, #174465, #106295, #23905, #54296, #120434, #186409, #38046 ),
 .UNSPECIFIED., .F., .F.,
 ( 4, 2, 2, 2, 4 ),
 ( 0.0002061898317416328299, 0.0005587239135660436798, 0.0009112579953904544755, 0.001263792077214865271, 0.001616326159039276067 ),
 .UNSPECIFIED. ) ;
#212464 = CARTESIAN_POINT ( 'NONE',  ( 5.817732461567613811, -1.591073081590412830, 1.238133459405404757 ) ) ;
#212465 = CARTESIAN_POINT ( 'NONE',  ( 4.452959842461719830, 0.4008590389125502029, -1.796806262838637647 ) ) ;
#212466 = CARTESIAN_POINT ( 'NONE',  ( 0.07700591528351626025, 0.2537022344677486996, -1.946355950789683043 ) ) ;
#212467 = CARTESIAN_POINT ( 'NONE',  ( 3.264621958926614109, 1.037573782609865436, 2.061359394274730583 ) ) ;
#212468 = CARTESIAN_POINT ( 'NONE',  ( 6.540882763950133238, 6.595727744222092959, 0.000000000000000000 ) ) ;
#212469 = CARTESIAN_POINT ( 'NONE',  ( 6.186834690482100108, -0.3103498281695793448, -2.139073744226393181 ) ) ;
#212470 = CARTESIAN_POINT ( 'NONE',  ( 8.132193210098487057, 8.381980254736715708, 1.040834085586084257E-14 ) ) ;
#212471 = CARTESIAN_POINT ( 'NONE',  ( 1.417416744832197484, -1.080314125112752155, -1.613661906057413331 ) ) ;
#212472 = CARTESIAN_POINT ( 'NONE',  ( -4.731959306369413198, 5.479372931307791461, -1.199719254218446718 ) ) ;
#212473 = VERTEX_POINT ( 'NONE', #138342 ) ;
#212474 = CARTESIAN_POINT ( 'NONE',  ( 4.780793123113402210, -2.255322609370190357, 0.4421783396322577775 ) ) ;
#212475 = DIRECTION ( 'NONE',  ( -0.000000000000000000, -1.000000000000000000, -0.000000000000000000 ) ) ;
#212476 = CARTESIAN_POINT ( 'NONE',  ( -5.490125858891038213, 5.369844688319787451, -0.7998128361456362523 ) ) ;
#212477 = CLOSED_SHELL ( 'NONE', ( #141608, #21309, #166700, #23096, #93822, #112396, #107230, #51380, #27090, #196751, #25658, #24122, #65866, #40884, #125225, #140427, #118259, #162144, #48968, #58788, #140141, #213677, #9776, #26863, #21863, #93777, #109063, #36562, #207090, #101902, #33748, #32, #73321, #86398, #14431, #119076, #34794, #88204, #131899, #125142, #89993, #92234, #48825, #158043, #155738, #211410, #62399, #179760, #189139, #82814, #107080, #204992, #147918, #109112, #24668, #117650, #53541, #176804, #90848, #213872, #115175, #45090, #152515, #174652, #154198, #52177, #142856, #179193, #10817, #206532, #48386, #24021, #20972, #109780, #8500, #155916, #184846, #15215, #18415, #161237, #196562, #71855, #110157, #131853, #114753, #97734, #62572, #195909, #142295, #179066, #73870 ) ) ;
#212478 = CARTESIAN_POINT ( 'NONE',  ( 4.381629165553334815, 1.221847395770376377, 1.416585496670008659 ) ) ;
#212479 = B_SPLINE_CURVE_WITH_KNOTS ( 'NONE', 3,
 ( #133868, #88282, #35242, #104538, #204119, #203063 ),
 .UNSPECIFIED., .F., .F.,
 ( 4, 2, 4 ),
 ( 0.001259240562161248120, 0.001573673787268790349, 0.001888107012376332794 ),
 .UNSPECIFIED. ) ;
#212483 = EDGE_CURVE ( 'NONE', #132154, #202848, #89606, .T. ) ;
#212482 = CARTESIAN_POINT ( 'NONE',  ( -4.599959256786493533, 8.588645909551377855, 0.000000000000000000 ) ) ;
#212481 = CARTESIAN_POINT ( 'NONE',  ( -1.402160292154681736E-14, 0.6187500006828180465, -1.732050807568863648 ) ) ;
#212480 = CARTESIAN_POINT ( 'NONE',  ( 1.353610510645312237, -1.387278792934818705, -1.316581319992945920 ) ) ;
#212484 = CARTESIAN_POINT ( 'NONE',  ( 3.176612885197922953, -1.314426786483071208, 1.772596291930063739 ) ) ;
#212485 = CARTESIAN_POINT ( 'NONE',  ( -1.445103857048106510, 8.688264192037884470, -2.625611233228244412 ) ) ;
#212486 = CARTESIAN_POINT ( 'NONE',  ( 4.216749469050096621, 4.878294787768598262, -1.199719254218452047 ) ) ;
#212487 = CARTESIAN_POINT ( 'NONE',  ( 5.031484404002867450, 8.884165881396448583, 0.7216878364870317197 ) ) ;
#212488 = CARTESIAN_POINT ( 'NONE',  ( -2.839543107058306592, 5.400218493954923815, -1.199719254218446718 ) ) ;
#212489 = CARTESIAN_POINT ( 'NONE',  ( -7.227905289416814760, 7.605180057173966723, -0.7216878364870338292 ) ) ;
#212490 = CARTESIAN_POINT ( 'NONE',  ( 1.194530107633525517, -0.4747795734156860514, -1.913232634659914444 ) ) ;
#212491 = EDGE_CURVE ( 'NONE', #166496, #25291, #76346, .T. ) ;
#212492 = CARTESIAN_POINT ( 'NONE',  ( 1.026927485578407406, 1.372003256358475864, -1.855264817478113226 ) ) ;
#212493 = CARTESIAN_POINT ( 'NONE',  ( 0.9417639971489067952, 1.314929008279978495, 1.456166070238865018 ) ) ;
#212494 = CARTESIAN_POINT ( 'NONE',  ( 5.647355161340581020, 1.821535332892617820, -0.9675206831420575249 ) ) ;
#212495 = CARTESIAN_POINT ( 'NONE',  ( 5.504247177468190699, 5.523969249908757817, 0.7216878364870317197 ) ) ;
#212496 = CARTESIAN_POINT ( 'NONE',  ( 5.499767588998890844, 6.445425604367387429, 1.199719254218451159 ) ) ;
#212497 = ORIENTED_EDGE ( 'NONE', *, *, #34131, .F. ) ;
#212498 = CARTESIAN_POINT ( 'NONE',  ( -10.47097470845587175, 11.11055866948701443, 1.040834085586084257E-14 ) ) ;
#212499 = CARTESIAN_POINT ( 'NONE',  ( 0.000000000000000000, 8.920000000000001705, 0.000000000000000000 ) ) ;
#212500 = CARTESIAN_POINT ( 'NONE',  ( 4.514501963226220660, 4.369266499959774563, -0.7216878364870197293 ) ) ;
#212501 = CARTESIAN_POINT ( 'NONE',  ( 0.3741910912563637948, -2.129432730031981080, 0.4223156635175562279 ) ) ;
#212503 = CARTESIAN_POINT ( 'NONE',  ( 4.369470645354133431, 8.319742529546998000, 0.7998128361456271485 ) ) ;
#212502 = CARTESIAN_POINT ( 'NONE',  ( -11.94105721237523454, 11.02740784401788865, 1.187919463087248273 ) ) ;
#212504 = COLOUR_RGB ( '', 0.40784314, 0.44705882, 0.49803922) ;
#212505 = CARTESIAN_POINT ( 'NONE',  ( -9.540655113774946017, 3.481540744127369802, 7.145788969735951568 ) ) ;
#212506 = FACE_OUTER_BOUND ( 'NONE', #144462, .T. ) ;
#212507 = CARTESIAN_POINT ( 'NONE',  ( 2.934663490303309974, 0.2251962677765201870, 1.856852477824536329 ) ) ;
#212508 = CARTESIAN_POINT ( 'NONE',  ( 6.221977808853903724, -1.195094089922192016, -1.800988070004491792 ) ) ;
#212509 = CARTESIAN_POINT ( 'NONE',  ( -5.593616938499215152, 6.351546440420595019, 1.211061620805883532 ) ) ;
#212510 = CARTESIAN_POINT ( 'NONE',  ( 0.07735805125225460321, 2.008365972388022946, -2.502973720202539276 ) ) ;
#212511 = CARTESIAN_POINT ( 'NONE',  ( 0.6823417656249864960, -1.073958332991911568, -1.181850606188749264 ) ) ;
#212512 = CARTESIAN_POINT ( 'NONE',  ( 2.367698891403247519, 0.5082884949165042965, -1.843433491391050838 ) ) ;
#212513 = CARTESIAN_POINT ( 'NONE',  ( 3.836565602288672938, 0.2594712388852594143, 1.750573784680304890 ) ) ;
#212514 = CARTESIAN_POINT ( 'NONE',  ( 0.8559432719405724033, 0.7744784914341161786, -1.748599447100062321 ) ) ;
#212515 = CARTESIAN_POINT ( 'NONE',  ( -4.880045225915050189, 7.780804299287790826, 1.199719254218464037 ) ) ;
#212517 = CARTESIAN_POINT ( 'NONE',  ( 5.905858165902563073, -1.068448527453051966, -1.589740232873719128 ) ) ;
#212516 = CARTESIAN_POINT ( 'NONE',  ( 3.261441746617202764, -3.200405687979760216, 0.6342848732913847210 ) ) ;
#212518 = CARTESIAN_POINT ( 'NONE',  ( 6.531706384513794816, 1.885137803977337656, -0.5704747015483744299 ) ) ;
#212519 = CARTESIAN_POINT ( 'NONE',  ( -1.499999999999997780, 4.400000000000021672, 1.214306433183764966E-14 ) ) ;
#212520 = CARTESIAN_POINT ( 'NONE',  ( 2.619513681940002670, 1.793805257907291395, 1.130712135851599465 ) ) ;
#212521 = CARTESIAN_POINT ( 'NONE',  ( 4.496171506534161644, 8.048216686630889072, -2.444650791391918876 ) ) ;
#212522 = CARTESIAN_POINT ( 'NONE',  ( 4.908994958506140982, 1.627828031611065152, 0.9215782234750914403 ) ) ;
#212524 = VERTEX_POINT ( 'NONE', #123246 ) ;
#212523 = CARTESIAN_POINT ( 'NONE',  ( 0.4690313652776016418, 0.1822212253758948297, -1.816563760317004395 ) ) ;
#212526 = CARTESIAN_POINT ( 'NONE',  ( -6.056815632531343141, 6.015240258500212711, 0.3115616189311651296 ) ) ;
#212525 = CARTESIAN_POINT ( 'NONE',  ( 4.090592613104036879, -2.182713160620152859, -0.3248913242878055385 ) ) ;
#212527 = CARTESIAN_POINT ( 'NONE',  ( 1.364683531249986537, -1.136458332991912235, 0.7879004041258500513 ) ) ;
#212528 = CARTESIAN_POINT ( 'NONE',  ( 1.961455461422195068, 1.713676499688887800, 1.147740006246004585 ) ) ;
#212529 = CARTESIAN_POINT ( 'NONE',  ( 6.745345117998789775, 7.828323044875442172, 1.199719254218462483 ) ) ;
#212531 = CARTESIAN_POINT ( 'NONE',  ( -6.855619230004478482, 11.14997286831390788, -0.7998128361456291469 ) ) ;
#212530 = VECTOR ( 'NONE', #157246, 1000.000000000000000 ) ;
#212532 = FILL_AREA_STYLE ('',( #197353 ) ) ;
#212533 = CARTESIAN_POINT ( 'NONE',  ( 9.728138913005292210, 11.30824913904973705, -1.199719254218440723 ) ) ;
#212534 = CARTESIAN_POINT ( 'NONE',  ( 11.89204169242350950, 11.29999999999999893, -0.8046421800350563869 ) ) ;
#212535 = DIRECTION ( 'NONE',  ( -1.207943261119674327E-30, -2.168404344971008079E-15, -1.000000000000000000 ) ) ;
#212536 = CARTESIAN_POINT ( 'NONE',  ( -4.933501523973760072E-10, 15.51845925587262798, -12.00000000000000178 ) ) ;
#212537 = ORIENTED_EDGE ( 'NONE', *, *, #188786, .F. ) ;
#212538 = CARTESIAN_POINT ( 'NONE',  ( 4.264170421968140445, -2.065031762457261610, 0.1491743435546449281 ) ) ;
#212540 = CARTESIAN_POINT ( 'NONE',  ( 1.364683531249986537, -0.7822916663252464931, -0.7879004041258309554 ) ) ;
#212539 = CIRCLE ( 'NONE', #5009, 0.08000000000000030698 ) ;
#212541 = CARTESIAN_POINT ( 'NONE',  ( 1.476082264964494906, 1.286352913914396545, 1.737049067733025032 ) ) ;
#212542 = CARTESIAN_POINT ( 'NONE',  ( -5.479780979625591186, 7.495630219063617261, -1.250153324542001343 ) ) ;
#212543 = CARTESIAN_POINT ( 'NONE',  ( 1.770181643375926317, 2.014124636562672155, -0.1506882416659905133 ) ) ;
#212544 = CYLINDRICAL_SURFACE ( 'NONE', #25240, 3.150000000000000799 ) ;
#212545 = ORIENTED_EDGE ( 'NONE', *, *, #37910, .T. ) ;
#212547 = CARTESIAN_POINT ( 'NONE',  ( 6.643132081016105417, 10.69414516125339887, 0.7216878364870438212 ) ) ;
#212546 = CARTESIAN_POINT ( 'NONE',  ( -3.474999999999998312, -3.470833333333334103, 2.006292185433951047 ) ) ;
#212548 = CARTESIAN_POINT ( 'NONE',  ( 0.04160626335162659339, 14.52071188304540073, 11.99061301703373417 ) ) ;
#212549 = CARTESIAN_POINT ( 'NONE',  ( -4.787437638956939523, 5.718337012605431369, -1.082531754730549967 ) ) ;
#212550 = CARTESIAN_POINT ( 'NONE',  ( 0.3390778084843976137, -1.706115258973059490, -1.074657883261991076 ) ) ;
#212551 = CARTESIAN_POINT ( 'NONE',  ( 5.126606437771586755, 0.1607948393855564151, 2.185736094377451089 ) ) ;
#212552 = PRESENTATION_LAYER_ASSIGNMENT (  '', '', ( #98457 ) ) ;
#212553 = ADVANCED_FACE ( 'NONE', ( #139413 ), #189210, .F. ) ;
#212554 = CARTESIAN_POINT ( 'NONE',  ( 1.499999999999989120, 4.785416667349486453, 0.8660254037844524744 ) ) ;
#212555 = CARTESIAN_POINT ( 'NONE',  ( 4.517770118113122457, -0.5046507728132009207, 1.844564425022446885 ) ) ;
#212556 = CARTESIAN_POINT ( 'NONE',  ( -3.632695093457760649, 6.325562478087638496, -1.199719254218452047 ) ) ;
#212557 = CARTESIAN_POINT ( 'NONE',  ( 5.409340101728155936, 8.294351971116089572, -1.082531754730543971 ) ) ;
#212559 = CARTESIAN_POINT ( 'NONE',  ( 2.601185598297011570, -0.1948207814224910128, 2.006963067508853005 ) ) ;
#212558 = CARTESIAN_POINT ( 'NONE',  ( 10.96785329849812562, -5.223431457505089526, -0.4373225248172959434 ) ) ;
#212560 = CARTESIAN_POINT ( 'NONE',  ( 1.364683531249997417, 12.54687500034139980, 2.602085213965210642E-15 ) ) ;
#212562 = CARTESIAN_POINT ( 'NONE',  ( -3.654804927335652209, 6.421633627603656080, 1.199719254218452935 ) ) ;
#212561 = CARTESIAN_POINT ( 'NONE',  ( 0.08209332325101456607, -1.073118421065310413, 2.025687816139466246 ) ) ;
#212563 = CARTESIAN_POINT ( 'NONE',  ( 4.998908393266289885, 1.432429904705156520, -0.9603719661937599739 ) ) ;
#212564 = PLANE ( 'NONE',  #178269 ) ;
#212565 = CARTESIAN_POINT ( 'NONE',  ( 3.063252641683779753, 5.661212951017999373, 1.199719254218450271 ) ) ;
#212566 = CARTESIAN_POINT ( 'NONE',  ( -1.499999999999981126, 3.910416667349481123, -0.8660254037844499209 ) ) ;
#212567 = CARTESIAN_POINT ( 'NONE',  ( -1.451998047843676476, 7.315968950353781253, 4.301760722578348073 ) ) ;
#212568 = PRESENTATION_STYLE_ASSIGNMENT (( #52216 ) ) ;
#212569 = ORIENTED_EDGE ( 'NONE', *, *, #169514, .F. ) ;
#212570 = CARTESIAN_POINT ( 'NONE',  ( 5.285751626526108637, 1.744147384919532140, -0.4889748023358466145 ) ) ;
#212571 = PRESENTATION_LAYER_ASSIGNMENT (  '', '', ( #5044 ) ) ;
#212572 = ORIENTED_EDGE ( 'NONE', *, *, #87068, .F. ) ;
#212573 = CARTESIAN_POINT ( 'NONE',  ( 4.016958651398847557, 7.908478536599129249, -0.7998128361456362523 ) ) ;
#212574 = CARTESIAN_POINT ( 'NONE',  ( -2.535011536075347571, 5.133042487381361596, -0.9999999999999956701 ) ) ;
#212575 = CARTESIAN_POINT ( 'NONE',  ( 5.813115421323210796, 1.476946679544950847, -1.048544953227096288 ) ) ;
#212576 = CARTESIAN_POINT ( 'NONE',  ( 5.004368096775565711, 8.852530189631227842, -0.7216878364870458196 ) ) ;
#212577 = CARTESIAN_POINT ( 'NONE',  ( 7.836475020641954004, -5.360178282914183967, -7.719547554928811728 ) ) ;
#212578 = CARTESIAN_POINT ( 'NONE',  ( 3.257961296797746265, 0.9855263100190698733, 1.957416934251283935 ) ) ;
#212579 = ORIENTED_EDGE ( 'NONE', *, *, #16602, .F. ) ;
#212581 = CARTESIAN_POINT ( 'NONE',  ( 7.730120138085914583, 12.17022392774227768, 0.7998128361456462443 ) ) ;
#212580 = CARTESIAN_POINT ( 'NONE',  ( 6.514093505496237668, 1.855963486094978965, -0.1381079127797563977 ) ) ;
#212582 = CARTESIAN_POINT ( 'NONE',  ( 3.954619794068328087, -1.788705220947036878, -0.6861305607534126105 ) ) ;
#212583 = FACE_OUTER_BOUND ( 'NONE', #75580, .T. ) ;
#212584 = CARTESIAN_POINT ( 'NONE',  ( -0.7500000000000179856, 12.04166666666666607, 1.299038105676658228 ) ) ;
#212585 = CARTESIAN_POINT ( 'NONE',  ( -1.402160292154681736E-14, -0.05312499965857903073, -1.575800808251665908 ) ) ;
#212586 = CARTESIAN_POINT ( 'NONE',  ( 3.850152436600926542, 7.435668909435648288, -0.7216878364870197293 ) ) ;
#212587 = CARTESIAN_POINT ( 'NONE',  ( -9.815740026613967828, 10.55404424057886636, -0.7216878364870267237 ) ) ;
#212588 = CARTESIAN_POINT ( 'NONE',  ( 1.868271315571629509, 1.111147431007172726, 1.854118885846419262 ) ) ;
#212589 = CARTESIAN_POINT ( 'NONE',  ( -4.098307573080856692, 8.003385611894792362, 0.7998128361456352531 ) ) ;
#212590 = VECTOR ( 'NONE', #57002, 1000.000000000000000 ) ;
#212591 = CARTESIAN_POINT ( 'NONE',  ( 5.876533236880477240, 5.820653295974182129, 0.7998128361456352531 ) ) ;
#212592 = CARTESIAN_POINT ( 'NONE',  ( 1.834698128333624112, 0.1755570873784827179, 1.817110820650599923 ) ) ;
#212593 = CARTESIAN_POINT ( 'NONE',  ( -4.925689880466507908, 4.641059703499347044, -0.7998128361456221525 ) ) ;
#212594 = CARTESIAN_POINT ( 'NONE',  ( 3.645350208285046634, -1.381898811119431691, -1.193016960613018096 ) ) ;
#212595 = CARTESIAN_POINT ( 'NONE',  ( 9.228631970132603612, 13.18394157654138965, -9.019657609914000673 ) ) ;
#212596 = VERTEX_POINT ( 'NONE', #71163 ) ;
#212597 = CARTESIAN_POINT ( 'NONE',  ( 3.613681597605075346, 0.4810616251548325284, -1.909752186315590405 ) ) ;
#212598 = EDGE_LOOP ( 'NONE', ( #119935, #160106, #15457, #100334, #32277, #155610, #78568, #154798, #120500, #64210, #55474, #110635, #58055, #158105, #9233, #91420, #42577, #44030, #166157, #1837, #186503, #187126, #199438, #209321, #33260, #31195, #118621, #108244, #172525, #169951, #176085, #126799, #22874, #79665, #87382, #92334, #175832, #94998, #177351, #191827, #171173, #109395, #15320, #103172 ) ) ;
#212599 = CARTESIAN_POINT ( 'NONE',  ( 4.581548892214976298, -0.9124856661332171326, 1.714327114426909882 ) ) ;
#212600 = ORIENTED_EDGE ( 'NONE', *, *, #195600, .T. ) ;
#212601 = CARTESIAN_POINT ( 'NONE',  ( -5.966470118465691641, 9.118576350588734059, -1.199719254218452047 ) ) ;
#212603 = CARTESIAN_POINT ( 'NONE',  ( 4.816704082729271086, -0.7169179515637627009, -1.995842421597990413 ) ) ;
#212602 = CARTESIAN_POINT ( 'NONE',  ( 6.180537922983273091, 8.303989891604203422, -1.599625672291281386 ) ) ;
#212604 = CARTESIAN_POINT ( 'NONE',  ( 4.370663978927085580, 5.060324124126027279, 7.500000000000000000 ) ) ;
#212605 = CARTESIAN_POINT ( 'NONE',  ( 5.555833580239399438, 6.383300830698137140, -1.210397860111110946 ) ) ;
#212606 = CARTESIAN_POINT ( 'NONE',  ( -9.491250020638663187, -6.775781654326522130, 0.2167848519283762654 ) ) ;
#212607 = EDGE_LOOP ( 'NONE', ( #109165, #92920, #193573, #156234 ) ) ;
#212608 = CARTESIAN_POINT ( 'NONE',  ( 5.890091390494168522, 5.836471141856793388, 0.000000000000000000 ) ) ;
#212609 = CARTESIAN_POINT ( 'NONE',  ( 4.178388974671240597, 0.9510918172684652561, 1.774266679505158262 ) ) ;
#212610 = CARTESIAN_POINT ( 'NONE',  ( 3.125598124496329360E-16, 2.519999999999999130, 2.000000000000000000 ) ) ;
#212611 = CARTESIAN_POINT ( 'NONE',  ( 5.197797600609998625, -0.6536857159176562293, 1.704833070275885598 ) ) ;
#212612 = CARTESIAN_POINT ( 'NONE',  ( 0.3091450132529197092, -1.663722454078466306, 1.232067777400827069 ) ) ;
#212613 = CARTESIAN_POINT ( 'NONE',  ( -7.321039761699444703, 10.52466824108257804, 1.082531754730549967 ) ) ;
#212614 = CARTESIAN_POINT ( 'NONE',  ( -6.317530715954224441, 6.956803165068716766, 0.9171252194158643345 ) ) ;
#212615 = CARTESIAN_POINT ( 'NONE',  ( -1.225000000000035172, 1.562500000682809365, -4.510281037539698445E-14 ) ) ;
#212616 = CARTESIAN_POINT ( 'NONE',  ( 5.752782329262380756, -1.473788443143897675, 1.151991621687727507 ) ) ;
#212617 = CARTESIAN_POINT ( 'NONE',  ( 6.449928391799196525, 8.548002428564306143, -1.599625672291262513 ) ) ;
#212618 = CARTESIAN_POINT ( 'NONE',  ( -5.111587607552082524, 5.922272616020886282, 1.199719254218450271 ) ) ;
#212619 = CARTESIAN_POINT ( 'NONE',  ( -1.364683531250000748, 10.42187500034139802, 0.000000000000000000 ) ) ;
#212620 = CARTESIAN_POINT ( 'NONE',  ( -5.738125327081750271, 7.717565519727259904, 1.599625672291269396 ) ) ;
#212622 = CARTESIAN_POINT ( 'NONE',  ( -7.608060475923978494, 8.905100639113307182, 1.199719254218452047 ) ) ;
#212621 = DIRECTION ( 'NONE',  ( 0.000000000000000000, 0.000000000000000000, -1.000000000000000000 ) ) ;
#212623 = EDGE_CURVE ( 'NONE', #189774, #109299, #106956, .T. ) ;
#212624 = CARTESIAN_POINT ( 'NONE',  ( -6.715366157470410435, 6.729015360003925750, -0.7998128361456291469 ) ) ;
#212625 = CARTESIAN_POINT ( 'NONE',  ( 1.288034235163344254, -1.310400469390052836, -1.602789277989056238 ) ) ;
#212626 = CARTESIAN_POINT ( 'NONE',  ( 2.864987086846816577, -0.1587241086147250513, -2.111353475082369702 ) ) ;
#212627 = CARTESIAN_POINT ( 'NONE',  ( 7.540305987494599016, 11.94877408538573427, -0.7998128361456291469 ) ) ;
#212628 = DIRECTION ( 'NONE',  ( -1.276756478318932585E-15, 1.000000000000000000, -1.665334536937738262E-16 ) ) ;
#212629 = CARTESIAN_POINT ( 'NONE',  ( 0.4616802850961505555, -0.5308588990461468038, 1.896450293990773472 ) ) ;
#212630 = CARTESIAN_POINT ( 'NONE',  ( 4.350666953118342839, 7.402852620340107492, 1.136566098749042242 ) ) ;
#212631 = CARTESIAN_POINT ( 'NONE',  ( 5.531363484695522637, 5.555604941673978558, -0.7216878364870207285 ) ) ;
#212633 = DIRECTION ( 'NONE',  ( 0.000000000000000000, 0.000000000000000000, 1.000000000000000000 ) ) ;
#212632 = CARTESIAN_POINT ( 'NONE',  ( 1.001543065824772753E-15, -2.712499999999999911, 4.012584370867899430 ) ) ;
#212634 = CARTESIAN_POINT ( 'NONE',  ( 2.414399183035727425, 1.495821068830467615, -1.737032439462746325 ) ) ;
#212635 = CARTESIAN_POINT ( 'NONE',  ( 0.5744775230259161480, -1.718042477583326066, -0.6180270036199516648 ) ) ;
#212636 = CARTESIAN_POINT ( 'NONE',  ( 2.355592738034977263, -1.419685808644566949, -1.281520755053264571 ) ) ;
#212637 = VERTEX_POINT ( 'NONE', #8319 ) ;
#212638 = CARTESIAN_POINT ( 'NONE',  ( 7.741342523278705201, 9.094283034322399928, 1.082531754730558626 ) ) ;
#212639 = CARTESIAN_POINT ( 'NONE',  ( 2.179941694947628683, 1.973542599225884153, -0.3968540688959447116 ) ) ;
#212640 = CARTESIAN_POINT ( 'NONE',  ( 0.7605091544688712402, -0.6555486260201286441, -1.849146037077718852 ) ) ;
#212641 = CARTESIAN_POINT ( 'NONE',  ( -10.14557902172788495, 10.73093036830436553, 1.040834085586084257E-14 ) ) ;
#212642 = CARTESIAN_POINT ( 'NONE',  ( -6.744291347794091784, 9.955758108146730123, -1.199719254218440723 ) ) ;
#212643 = CARTESIAN_POINT ( 'NONE',  ( -4.812781342726871969, 6.637997537979888563, 1.443375672974064550 ) ) ;
#212645 = CARTESIAN_POINT ( 'NONE',  ( 2.096244624822783731, -0.4688358662975153357, -1.706545078221621603 ) ) ;
#212644 = CARTESIAN_POINT ( 'NONE',  ( 3.416043810090535260, 1.326132273491455349, -1.616208110139333742 ) ) ;
#212646 = CARTESIAN_POINT ( 'NONE',  ( -11.02381569330256283, 2.441452740530747789, 3.988656969163915100 ) ) ;
#212648 = CARTESIAN_POINT ( 'NONE',  ( 4.839906306838932970, 2.285852466752227752, 0.1720476854494106811 ) ) ;
#212647 = CARTESIAN_POINT ( 'NONE',  ( -10.91970695577495931, 0.000000000000000000, 0.000000000000000000 ) ) ;
#212649 = CARTESIAN_POINT ( 'NONE',  ( 4.224340698251967119, 0.08847545473529906668, 1.738206131172301161 ) ) ;
#212650 = CARTESIAN_POINT ( 'NONE',  ( 9.887974103068218668, 10.43039129653476493, 0.7998128361456462443 ) ) ;
#212651 = CARTESIAN_POINT ( 'NONE',  ( 4.000000000000012434, 5.999999999999998224, -1.214306433183764966E-14 ) ) ;
#212652 = CARTESIAN_POINT ( 'NONE',  ( 4.481622980438174864, 1.585354267084694957, 0.7024943803609559057 ) ) ;
#212653 = CARTESIAN_POINT ( 'NONE',  ( 4.791568617006563002, -1.986896891843348723, 0.8757425373496147136 ) ) ;
#212654 = CARTESIAN_POINT ( 'NONE',  ( 4.142179624174931796, 4.791296635414242111, 1.199719254218464037 ) ) ;
#212655 = CARTESIAN_POINT ( 'NONE',  ( 5.313685493615880162, -1.282986534165726944, -1.555701818360885280 ) ) ;
#212656 = CARTESIAN_POINT ( 'NONE',  ( 6.750000000000005329, 1.157781160899305384, 2.098894642203967376 ) ) ;
#212657 = CARTESIAN_POINT ( 'NONE',  ( -3.443980807556779045, 6.324176108538676289, 1.003164557157047332 ) ) ;
#212658 = CARTESIAN_POINT ( 'NONE',  ( 3.645458630373909159, -1.458056112162182893, -1.259071146193297075 ) ) ;
#212659 = CARTESIAN_POINT ( 'NONE',  ( -1.402160292154681736E-14, 10.09375000068279604, 1.732050807568881190 ) ) ;
#212660 = CARTESIAN_POINT ( 'NONE',  ( 5.678047454291774265, 2.188620968312010362, -0.3794988778502098592 ) ) ;
#212661 = ORIENTED_EDGE ( 'NONE', *, *, #26463, .T. ) ;
#212662 = CARTESIAN_POINT ( 'NONE',  ( 6.983263157960327483, 4.697935251208478213, 2.408834092705824936 ) ) ;
#212663 = CARTESIAN_POINT ( 'NONE',  ( 0.7499999999999902300, 3.483333333333352044, 1.299038105676669330 ) ) ;
#212664 = CARTESIAN_POINT ( 'NONE',  ( 5.015626762051672571, 7.938982758113895422, 1.199719254218462483 ) ) ;
#212665 = CARTESIAN_POINT ( 'NONE',  ( 2.016565898353571473, -2.220703888365501921, 0.05821906423880519182 ) ) ;
#212666 = CARTESIAN_POINT ( 'NONE',  ( -1.737500000000000266, -1.064583332377418090, -3.009438278150923907 ) ) ;
#212667 = CARTESIAN_POINT ( 'NONE',  ( 6.805829924380105034, 9.923590097543378619, 1.082531754730558626 ) ) ;
#212668 = CARTESIAN_POINT ( 'NONE',  ( 0.1400748609344511231, 7.098713645440544617, 2.115199198882494080 ) ) ;
#212669 = AXIS2_PLACEMENT_3D ( 'NONE', #200107, #202233, #135153 ) ;
#212670 = CARTESIAN_POINT ( 'NONE',  ( 3.379725431556547477, 7.165039780116438273, -1.734723475976807094E-15 ) ) ;
#212671 = CARTESIAN_POINT ( 'NONE',  ( -3.187575512988701565, 6.732938841879847480, 0.000000000000000000 ) ) ;
#212673 = CARTESIAN_POINT ( 'NONE',  ( 5.477030937198195559, 1.904485971043594628, 0.7926545740569268528 ) ) ;
#212672 = CARTESIAN_POINT ( 'NONE',  ( 10.22692794340986921, 10.82583744360002243, 0.000000000000000000 ) ) ;
#212674 = CARTESIAN_POINT ( 'NONE',  ( -3.418627288940168096, 7.140148937072163804, -0.7998128361456281477 ) ) ;
#212675 = MECHANICAL_DESIGN_GEOMETRIC_PRESENTATION_REPRESENTATION (  '', ( #81279 ), #191955 ) ;
#212676 = CARTESIAN_POINT ( 'NONE',  ( 0.7499999999999920064, 4.764583334016150751, 1.299038105676669330 ) ) ;
#212677 = CARTESIAN_POINT ( 'NONE',  ( 1.364683531249986537, -0.1364583329919154264, 0.7879004041258500513 ) ) ;
#212678 = CARTESIAN_POINT ( 'NONE',  ( 0.4207181242068900873, -0.09552205520973154618, 1.767312625620009126 ) ) ;
#212679 = CARTESIAN_POINT ( 'NONE',  ( 5.361839092321889488, -0.05056905708066515570, -1.733610765856267388 ) ) ;
#212680 = CARTESIAN_POINT ( 'NONE',  ( 5.020954538418783031, -1.650374644951870806, 0.5528329121840831473 ) ) ;
#212681 = CARTESIAN_POINT ( 'NONE',  ( 3.171717870593107058, 5.787755718078879674, -1.199719254218446718 ) ) ;
#212682 = CARTESIAN_POINT ( 'NONE',  ( 3.140441720415044546, 0.5589363893779492054, 2.223061277538174174 ) ) ;
#212683 = CARTESIAN_POINT ( 'NONE',  ( 0.6823417656249917140, 5.655208333674749177, 1.181850606188765695 ) ) ;
#212684 = CARTESIAN_POINT ( 'NONE',  ( 1.253568445147245525, 0.7445567558202557112, 1.684058134371092752 ) ) ;
#212685 = ADVANCED_FACE ( 'NONE', ( #110167 ), #143712, .T. ) ;
#212686 = CARTESIAN_POINT ( 'NONE',  ( 0.000000000000000000, 5.499999999999998224, 0.000000000000000000 ) ) ;
#212687 = PRESENTATION_STYLE_ASSIGNMENT (( #159690 ) ) ;
#212688 = CARTESIAN_POINT ( 'NONE',  ( 1.905030480050071251, 1.515927946353814892, 1.016894063925778635 ) ) ;
#212689 = CARTESIAN_POINT ( 'NONE',  ( 3.252577435111691617, 1.966644794889659043, -0.4445022851852917234 ) ) ;
#212690 = CARTESIAN_POINT ( 'NONE',  ( 1.078377591563362436, -2.138745004354754897, -0.4770250503970187572 ) ) ;
#212691 = CARTESIAN_POINT ( 'NONE',  ( 9.503631714379071838, 15.23661009679124057, -8.229227087069268975 ) ) ;
#212692 = CARTESIAN_POINT ( 'NONE',  ( 4.313572747864121482, -0.3622951029728087580, 2.074398424781583206 ) ) ;
#212693 = CARTESIAN_POINT ( 'NONE',  ( -5.716734326456539783, 9.821273814174633188, -0.7998128361456231517 ) ) ;
#212694 = CARTESIAN_POINT ( 'NONE',  ( 8.250525573328690854, 13.32549038962357635, 8.564080365641034476 ) ) ;
#212695 = CIRCLE ( 'NONE', #101526, 11.92000000000000171 ) ;
#212696 = CARTESIAN_POINT ( 'NONE',  ( 1.908725956546155178, 0.6474277305483535638, 1.966616875269424192 ) ) ;
#212697 = CARTESIAN_POINT ( 'NONE',  ( 5.854423403002611437, 5.724582146458163656, 1.040834085586084257E-14 ) ) ;
#212698 = CARTESIAN_POINT ( 'NONE',  ( -1.360316468750006225, 2.640625000341401130, 3.469446951953614189E-15 ) ) ;
#212699 = CARTESIAN_POINT ( 'NONE',  ( 3.826904873358004888, 1.498484187726952799, -1.500593194838243605 ) ) ;
#212700 = CARTESIAN_POINT ( 'NONE',  ( 0.2758378062712996681, 1.107980625233648597, 1.575821400459100463 ) ) ;
#212701 = ORIENTED_EDGE ( 'NONE', *, *, #71135, .T. ) ;
#212702 = CARTESIAN_POINT ( 'NONE',  ( -4.444040490229335560, 8.406740681901359480, 0.7998128361456352531 ) ) ;
#212703 = CARTESIAN_POINT ( 'NONE',  ( 8.940712233207955606, 12.51824914112961729, 1.199719254218450271 ) ) ;
#212704 = CARTESIAN_POINT ( 'NONE',  ( 6.834718834620487016, 7.146462526578263308, 0.000000000000000000 ) ) ;
#212705 = CARTESIAN_POINT ( 'NONE',  ( -3.475000000000000533, -3.456249999044084920, 0.000000000000000000 ) ) ;
#212706 = CARTESIAN_POINT ( 'NONE',  ( -4.446184310277715213, 7.274633231044262516, -1.199719254218452047 ) ) ;
#212707 = CARTESIAN_POINT ( 'NONE',  ( 2.724872815078176913, 1.459976238909798996, -1.395942890215768895 ) ) ;
#212708 = CARTESIAN_POINT ( 'NONE',  ( 1.606614413041591360, -0.7575671727712609549, -1.965171518483445068 ) ) ;
#212709 = CARTESIAN_POINT ( 'NONE',  ( -6.629010762438975135, 6.698543742459062145, -0.7998128361456362523 ) ) ;
#212710 = CARTESIAN_POINT ( 'NONE',  ( 9.562578416340237197, 10.05076299535211781, 0.7998128361456462443 ) ) ;
#212711 = CARTESIAN_POINT ( 'NONE',  ( 5.541811466629937399, 1.248470921604339923, 1.380218479220591155 ) ) ;
#212712 = CARTESIAN_POINT ( 'NONE',  ( 9.250740883225924804, 9.686952540052077509, 1.040834085586084257E-14 ) ) ;
#212713 = EDGE_CURVE ( 'NONE', #108406, #152119, #182180, .T. ) ;
#212714 = CARTESIAN_POINT ( 'NONE',  ( 4.175484721775176489, 3.976419294354625933, -0.06592222766770190756 ) ) ;
#212715 = CARTESIAN_POINT ( 'NONE',  ( -9.490344339885973923, 12.09515436799890331, -1.443375672974059665 ) ) ;
#212716 = CARTESIAN_POINT ( 'NONE',  ( -7.100719765255177229, 9.307259030929609267, -1.599625672291263179 ) ) ;
#212717 = CARTESIAN_POINT ( 'NONE',  ( 6.649297902391459125, -1.653525193404258742, -1.229868563883255828 ) ) ;
#212718 = TOROIDAL_SURFACE ( 'NONE', #164335, -0.1799999999926198968, 0.5000000000000013323 ) ;
#212720 = CARTESIAN_POINT ( 'NONE',  ( -4.043597078347817231, 7.757176853022865082, 0.5683662157932849457 ) ) ;
#212719 = CARTESIAN_POINT ( 'NONE',  ( -6.069210040772897052, 7.109775131437022999, -1.199719254218453823 ) ) ;
#212721 = CARTESIAN_POINT ( 'NONE',  ( 1.364683531249986537, 0.8635416670080893198, 0.7879004041258500513 ) ) ;
#212722 = CARTESIAN_POINT ( 'NONE',  ( 2.512703819571511232, 1.733401479428131609, 0.04661458952265155886 ) ) ;
#212723 = CARTESIAN_POINT ( 'NONE',  ( 1.587455592251562297, -1.731706956562387711, -0.1728515053983879501 ) ) ;
#212725 = CARTESIAN_POINT ( 'NONE',  ( 7.782016984564065432, 8.181367358187307204, 0.7216878364870458196 ) ) ;
#212724 = CARTESIAN_POINT ( 'NONE',  ( 0.4468379896771547122, 2.301730118641607703, 0.1654463548556948105 ) ) ;
#212726 = CARTESIAN_POINT ( 'NONE',  ( -10.91672646594461327, 4.673612064222224305, 4.467269497407427181 ) ) ;
#212727 = CARTESIAN_POINT ( 'NONE',  ( 2.706383518077785322, -0.7856088873096721548, -1.905365358233277240 ) ) ;
#212728 = CARTESIAN_POINT ( 'NONE',  ( 5.087333953625774008, 6.958308917361963886, 1.599625672291267398 ) ) ;
#212729 = CARTESIAN_POINT ( 'NONE',  ( 1.247422469434919412, -1.966343046301596509, -0.4444367004674750210 ) ) ;
#212730 = CARTESIAN_POINT ( 'NONE',  ( 6.825078400183582694, 7.052246674313852992, 2.642498189888539795 ) ) ;
#212731 = CARTESIAN_POINT ( 'NONE',  ( -5.285699784481336927, 7.260012063351913625, 1.599625672291263179 ) ) ;
#212732 = CARTESIAN_POINT ( 'NONE',  ( 0.7078139640715176428, -1.962176506181498636, 0.1910761354673266577 ) ) ;
#212733 =( GEOMETRIC_REPRESENTATION_CONTEXT ( 3 ) GLOBAL_UNCERTAINTY_ASSIGNED_CONTEXT ( ( #14992 ) ) GLOBAL_UNIT_ASSIGNED_CONTEXT ( ( #112474, #12751, #195792 ) ) REPRESENTATION_CONTEXT ( 'NONE', 'WORKASPACE' ) );
#212736 = EDGE_CURVE ( 'NONE', #157195, #74610, #58352, .T. ) ;
#212735 = CARTESIAN_POINT ( 'NONE',  ( -5.153507786970262572, 9.026526494858359229, -0.7216878364870338292 ) ) ;
#212734 = CARTESIAN_POINT ( 'NONE',  ( 4.904515063324526025, -1.898637117948184017, -0.2282459111111398431 ) ) ;
#212737 = CARTESIAN_POINT ( 'NONE',  ( -6.089020385868856522, 9.157588645938716354, -1.082531754730549967 ) ) ;
#212738 = CARTESIAN_POINT ( 'NONE',  ( 6.339319342841494453, 9.553567112360518365, -1.199719254218452047 ) ) ;
#212739 = AXIS2_PLACEMENT_3D ( 'NONE', #175357, #176410, #64773 ) ;
#212740 = CARTESIAN_POINT ( 'NONE',  ( -7.930593509350902792, 8.217056947189661287, -0.7998128361456362523 ) ) ;
#212741 = CARTESIAN_POINT ( 'NONE',  ( 0.6451828087791033894, 0.1507176824743546029, 2.014122433718650296 ) ) ;
#212742 = CARTESIAN_POINT ( 'NONE',  ( 11.33772463945037146, 12.69999999999998153, 3.599999999999999201 ) ) ;
#212743 = EDGE_CURVE ( 'NONE', #46648, #137788, #110369, .T. ) ;
#212744 = CARTESIAN_POINT ( 'NONE',  ( 5.034332918631054810, 1.191367258472323831, -1.976142064534849307 ) ) ;
#212745 = CARTESIAN_POINT ( 'NONE',  ( 5.600043156098196917, 0.7966083592686534764, -1.793046234938546757 ) ) ;
#212746 = CARTESIAN_POINT ( 'NONE',  ( 1.569116724355507975, 1.727593668635756918, 0.9295332132536607839 ) ) ;
#212747 = CARTESIAN_POINT ( 'NONE',  ( 8.550388431712704573, 13.12720360364021133, 0.000000000000000000 ) ) ;
#212748 = CARTESIAN_POINT ( 'NONE',  ( -9.393959922490113357, 14.54118366885366775, 7.466876303508932722 ) ) ;
#212749 = VERTEX_POINT ( 'NONE', #94936 ) ;
#212750 = CARTESIAN_POINT ( 'NONE',  ( -0.1177638760072839408, -2.117013592363240271, -0.04492315971119444085 ) ) ;
#212752 = CARTESIAN_POINT ( 'NONE',  ( -8.369460898337653276, 8.658792557682392754, 0.7998128361456462443 ) ) ;
#212751 = CARTESIAN_POINT ( 'NONE',  ( -4.355193658487827690, 6.104145239700998538, -1.599625672291256295 ) ) ;
#212753 = CARTESIAN_POINT ( 'NONE',  ( 0.9371597039556851527, 0.7481776565299682602, -1.682445429299509909 ) ) ;
#212754 = ORIENTED_EDGE ( 'NONE', *, *, #1482, .F. ) ;
#212755 = CARTESIAN_POINT ( 'NONE',  ( 4.768535058008659178, -0.9225228719554872114, -1.965435229472652479 ) ) ;
#212756 = CARTESIAN_POINT ( 'NONE',  ( 11.52671564374114155, 8.445739998960311468, -3.359000350707669558 ) ) ;
#212757 = CARTESIAN_POINT ( 'NONE',  ( 1.723052270212792836, 1.567896913533245229, -1.427966198690698851 ) ) ;
#212758 = CARTESIAN_POINT ( 'NONE',  ( -1.500000000000011324, 3.702083334016152971, 0.8660254037844403729 ) ) ;
#212759 = CARTESIAN_POINT ( 'NONE',  ( 8.646349277213076334, 11.11049346154719508, 1.599625672291281386 ) ) ;
#212760 = CARTESIAN_POINT ( 'NONE',  ( -1.849151978240317185, 2.492296139600388205, -2.488099065827154899 ) ) ;
#212761 = CARTESIAN_POINT ( 'NONE',  ( 3.075518034276482293, 1.957894989606956182, -0.6432953703794060951 ) ) ;
#212763 = CARTESIAN_POINT ( 'NONE',  ( -0.07694640568740516995, -1.131669979810394633, -1.452919414246391261 ) ) ;
#212762 = CARTESIAN_POINT ( 'NONE',  ( -7.181014916732457287, 11.52960116949655678, -0.7998128361456291469 ) ) ;
#212764 = CARTESIAN_POINT ( 'NONE',  ( -1.201851678989727383E-14, 2.946875000341419248, -1.575800808251660134 ) ) ;
#212765 = DIRECTION ( 'NONE',  ( 0.2150645590070887347, -0.8781765503997437383, 0.4272624273056235267 ) ) ;
#212766 = CARTESIAN_POINT ( 'NONE',  ( 1.412038856124948838, 4.223545038993179901, -0.5099368981155084635 ) ) ;
#212767 = CARTESIAN_POINT ( 'NONE',  ( 0.04788047853313340263, -1.708876078042343316, -1.396090968258607790 ) ) ;
#212768 = CARTESIAN_POINT ( 'NONE',  ( 2.038691496156146865, 2.237626877524625524, 0.3332970034419027727 ) ) ;
#212769 = CARTESIAN_POINT ( 'NONE',  ( -9.978437869977959451, 10.74385839117019614, -0.7216878364870267237 ) ) ;
#212770 = CARTESIAN_POINT ( 'NONE',  ( 2.021461901335448896, -0.3940331753463456321, 1.768040416340182608 ) ) ;
#212771 = CARTESIAN_POINT ( 'NONE',  ( 1.499098398830187362, -0.2305585200724231121, 1.901688874922660588 ) ) ;
#212772 = CARTESIAN_POINT ( 'NONE',  ( 2.805202726412972858, -1.722705984639979704, 1.148039668612794051 ) ) ;
#212773 = CARTESIAN_POINT ( 'NONE',  ( -1.364683531250012516, 2.092708333674750953, 0.7879004041258379498 ) ) ;
#212774 = CARTESIAN_POINT ( 'NONE',  ( 2.026188796938654946, 1.136581424768828397, -1.610674104117129302 ) ) ;
#212775 = CARTESIAN_POINT ( 'NONE',  ( 5.303319688262892129, 1.576177044413902717, 1.107479782286522996 ) ) ;
#212776 = CARTESIAN_POINT ( 'NONE',  ( 3.115926070338378207, -0.9207206926411042325, -1.628290677324291780 ) ) ;
#212778 = CARTESIAN_POINT ( 'NONE',  ( 6.132331002353889282, 6.987295666328819266, -0.9434213173033257904 ) ) ;
#212777 = CARTESIAN_POINT ( 'NONE',  ( 1.085104692462773412, -2.252536170888468359, -0.5009029511823160918 ) ) ;
#212779 = CARTESIAN_POINT ( 'NONE',  ( 2.734617598447198539, -1.779929554887052401, -0.5434082684390993956 ) ) ;
#212780 = CARTESIAN_POINT ( 'NONE',  ( 1.364683531249988535, 2.863541667008082658, 0.7879004041258500513 ) ) ;
#212781 = CARTESIAN_POINT ( 'NONE',  ( 5.477030937198195559, 1.904485971043594628, 0.7926545740569268528 ) ) ;
#212782 = CARTESIAN_POINT ( 'NONE',  ( -4.089755892816631544, 7.923132308261379819, -0.7998128361456281477 ) ) ;
#212783 = CARTESIAN_POINT ( 'NONE',  ( -1.354875605471922873, 3.776832748260927630, 0.6436714776511484049 ) ) ;
#212784 = CARTESIAN_POINT ( 'NONE',  ( 6.088920695360399371, -0.3053041885118645271, -2.083579958893892137 ) ) ;
#212785 = CARTESIAN_POINT ( 'NONE',  ( -0.6823417656250003738, 2.280208333674753174, -1.181850606188749264 ) ) ;
#212786 = CARTESIAN_POINT ( 'NONE',  ( 6.169229141836319208, 0.1658205177522271423, -2.155315574850395155 ) ) ;
#212787 = CARTESIAN_POINT ( 'NONE',  ( 0.3976880421775743635, -0.6195963491163231085, -1.733980255833282191 ) ) ;
#212788 = CARTESIAN_POINT ( 'NONE',  ( 5.883464967995201356, 0.1463045851861736191, -2.014419601194089804 ) ) ;
#212789 = DIRECTION ( 'NONE',  ( -3.451266460341926649E-31, -5.200010849845536803E-32, 1.000000000000000000 ) ) ;
#212790 = CARTESIAN_POINT ( 'NONE',  ( -5.761852096127856981, 5.824508321678349532, 0.000000000000000000 ) ) ;
#212793 = CARTESIAN_POINT ( 'NONE',  ( 4.202664430556247055, 6.886563688082179446, 1.082531754730558626 ) ) ;
#212792 = CARTESIAN_POINT ( 'NONE',  ( 3.285556943750000514, -1.013541666188710888, 1.896917185911906500 ) ) ;
#212791 = CARTESIAN_POINT ( 'NONE',  ( -1.790573066372362465, 14.55177515835072199, -11.85444247180616095 ) ) ;
#212794 = CARTESIAN_POINT ( 'NONE',  ( -5.829079699232685208, 5.765290835385048496, 0.000000000000000000 ) ) ;
#212795 = CARTESIAN_POINT ( 'NONE',  ( 3.344935638061694139, -1.780668040901035143, -0.9463001528628791625 ) ) ;
#212796 = CARTESIAN_POINT ( 'NONE',  ( -6.204827856548512877, 10.39071626594860476, -0.7998128361456291469 ) ) ;
#212798 = CARTESIAN_POINT ( 'NONE',  ( -10.99126615174920474, -5.166862915010145052, 0.4382560683119315903 ) ) ;
#212797 = CARTESIAN_POINT ( 'NONE',  ( -8.948018195339354719, 12.42280974699582607, 1.082531754730560403 ) ) ;
#212799 = CARTESIAN_POINT ( 'NONE',  ( 1.364683531249992088, 5.384375000341417916, 1.214306433183764966E-14 ) ) ;
#212801 = CARTESIAN_POINT ( 'NONE',  ( -1.364683531250014514, 9.838541667008064096, -0.7879004041258335089 ) ) ;
#212800 = CARTESIAN_POINT ( 'NONE',  ( 5.946190753372003535, 2.158995856162956084, 0.1107517376499680406 ) ) ;
#212802 = DIRECTION ( 'NONE',  ( 0.000000000000000000, 1.000000000000000000, 0.000000000000000000 ) ) ;
#212803 = CARTESIAN_POINT ( 'NONE',  ( -12.00016495910608860, 8.079444814310500433, -0.2607765302759474380 ) ) ;
#212804 = CIRCLE ( 'NONE', #157488, 10.91999999999999105 ) ;
#212806 = CARTESIAN_POINT ( 'NONE',  ( 5.079703922733037835, -0.7231256174668048153, 1.882480835741196845 ) ) ;
#212805 = CARTESIAN_POINT ( 'NONE',  ( -6.683806541412776525, 7.860491055478785682, -1.082531754730543083 ) ) ;
#212807 = CARTESIAN_POINT ( 'NONE',  ( 1.364683531249986537, -0.07395833299191513499, 0.7879004041258500513 ) ) ;
#212808 = CARTESIAN_POINT ( 'NONE',  ( 1.611479353654057034, -1.712177798104688620, 0.2083697849032482008 ) ) ;
#212809 = CARTESIAN_POINT ( 'NONE',  ( 3.739016502318667445, 7.584212696005614873, 0.7998128361456271485 ) ) ;
#212811 = CARTESIAN_POINT ( 'NONE',  ( 7.530627977747744062, 7.750430493652658015, -0.7998128361456341429 ) ) ;
#212810 = CARTESIAN_POINT ( 'NONE',  ( 7.483737605063422116, 7.833374748769873719, -0.7216878364870257245 ) ) ;
#212812 = CARTESIAN_POINT ( 'NONE',  ( -11.94312002716720045, 8.978941879399096493, 0.6089553112034360449 ) ) ;
#212813 = CARTESIAN_POINT ( 'NONE',  ( 6.907498162232361238, -0.4094499450241483318, 1.831839262316947270 ) ) ;
#212814 = CARTESIAN_POINT ( 'NONE',  ( 0.4518146667342719525, -1.425121331298753402, -1.422066715514385349 ) ) ;
#212815 = CARTESIAN_POINT ( 'NONE',  ( -15.75000000000000000, 13.79999999999999893, -1.800000000000001155 ) ) ;
#212816 = CARTESIAN_POINT ( 'NONE',  ( 4.338245966248566177, 4.163634503485842409, 1.214306433183764966E-14 ) ) ;
#212817 = CARTESIAN_POINT ( 'NONE',  ( 3.417197246517459597, 1.994164043739574232, 0.9453733912969732867 ) ) ;
#212818 = CARTESIAN_POINT ( 'NONE',  ( 5.137628997053973912, 2.028260002996465250, -0.7749071676581267276 ) ) ;
#212819 = ORIENTED_EDGE ( 'NONE', *, *, #166683, .F. ) ;
#212820 = CARTESIAN_POINT ( 'NONE',  ( 5.259637247458703868, 5.100941308315409373, 0.000000000000000000 ) ) ;
#212821 = CARTESIAN_POINT ( 'NONE',  ( 8.392133896734655707, 11.77427806529038357, 1.082531754730546636 ) ) ;
#212823 = CARTESIAN_POINT ( 'NONE',  ( 1.405875298092047698, -1.122519365368032984, -1.674874950958963549 ) ) ;
#212822 = CARTESIAN_POINT ( 'NONE',  ( 2.912858673564645784, -0.6176872867308530468, -2.028511212565413224 ) ) ;
#212825 = ORIENTED_EDGE ( 'NONE', *, *, #189834, .T. ) ;
#212824 = CARTESIAN_POINT ( 'NONE',  ( 1.845701740803426194, -1.185437281251604746, -1.369922693571566485 ) ) ;
#212826 = CARTESIAN_POINT ( 'NONE',  ( 6.574778147984297938, 6.635272358928617997, -0.7998128361456481317 ) ) ;
#212827 = PRESENTATION_LAYER_ASSIGNMENT (  '', '', ( #64121 ) ) ;
#212828 = CARTESIAN_POINT ( 'NONE',  ( 7.284808609244363353, 7.393364887073558656, 0.7998128361456341429 ) ) ;
#212830 = CARTESIAN_POINT ( 'NONE',  ( 0.9365811914238668656, -1.507994439141499221, 1.181323522483549437 ) ) ;
#212829 = CARTESIAN_POINT ( 'NONE',  ( -4.939248034080176097, 4.656877549381960080, 1.214306433183764966E-14 ) ) ;
#212831 = DIRECTION ( 'NONE',  ( 0.000000000000000000, 0.000000000000000000, -1.000000000000000000 ) ) ;
#212832 = CARTESIAN_POINT ( 'NONE',  ( 4.905139262582265403, 4.827437033166341429, 0.6004564335717228474 ) ) ;
#212833 = STYLED_ITEM ( 'NONE', ( #162275 ), #190216 ) ;
#212834 = CARTESIAN_POINT ( 'NONE',  ( 4.622967192135525316, 8.337286124226029216, -0.7216878364870207285 ) ) ;
#212835 = CARTESIAN_POINT ( 'NONE',  ( -1.364683531250000748, 0.3218750003414205807, 0.000000000000000000 ) ) ;
#212836 = CARTESIAN_POINT ( 'NONE',  ( 6.115105756127376502, 6.015623637602188545, 0.1580619937117197227 ) ) ;
#212837 = CARTESIAN_POINT ( 'NONE',  ( -9.809487834687324437, 11.40315621434539395, 1.199719254218462483 ) ) ;
#212838 = CARTESIAN_POINT ( 'NONE',  ( 4.733611406029458735, 0.6279933214467496860, -1.916352419866963697 ) ) ;
#212839 = CARTESIAN_POINT ( 'NONE',  ( 5.805597153138060129, -0.5296426447994294628, 2.095691122003799478 ) ) ;
#212840 = CARTESIAN_POINT ( 'NONE',  ( -6.292392690518223475, 6.513748691792265788, -0.7216878364870338292 ) ) ;
#212841 = CARTESIAN_POINT ( 'NONE',  ( 4.909461021924240498, 7.781436054670031410, 1.082531754730549078 ) ) ;
#212842 = CARTESIAN_POINT ( 'NONE',  ( 1.424255164902767934, -2.103954720533041556, 0.2648648325892372646 ) ) ;
#212843 = DIRECTION ( 'NONE',  ( 3.122502256758252154E-17, 2.602085213965210950E-17, 1.000000000000000000 ) ) ;
#212844 = CARTESIAN_POINT ( 'NONE',  ( 3.110573765929941725, 1.430363465515383625, -1.356829130874689815 ) ) ;
#212845 = ORIENTED_EDGE ( 'NONE', *, *, #60871, .T. ) ;
#212846 = CARTESIAN_POINT ( 'NONE',  ( 0.7499999999999902300, 4.566666666666691299, -1.299038105676658228 ) ) ;
#212847 = CARTESIAN_POINT ( 'NONE',  ( 6.812958078942359386, -1.523254609455872322, 1.248309864861799401 ) ) ;
#212848 = CARTESIAN_POINT ( 'NONE',  ( 1.288897009404812666, 1.470358960358808309, 1.268651691623223110 ) ) ;
#212849 = VERTEX_POINT ( 'NONE', #195619 ) ;
#212850 = CARTESIAN_POINT ( 'NONE',  ( 6.875078400183573635, 7.629137130509068498, 2.744348168701661095 ) ) ;
#212852 = CARTESIAN_POINT ( 'NONE',  ( 6.003228155800906407, 10.22579295840155744, 0.000000000000000000 ) ) ;
#212851 = CARTESIAN_POINT ( 'NONE',  ( -6.834718835064852449, 8.106831741398025315, 1.082531754730549078 ) ) ;
#212854 = CARTESIAN_POINT ( 'NONE',  ( 6.714312387265682247, 8.856450423275211037, 1.599625672291281386 ) ) ;
#212853 = CARTESIAN_POINT ( 'NONE',  ( 2.923863239626739663, 1.160869195616637706, -1.738502609096896467 ) ) ;
#212855 = CARTESIAN_POINT ( 'NONE',  ( 4.041739190205284160, 7.729463131965888856, 0.000000000000000000 ) ) ;
#212857 = ORIENTED_EDGE ( 'NONE', *, *, #73552, .T. ) ;
#212856 = CARTESIAN_POINT ( 'NONE',  ( 6.621744163077868173, -0.4141588628726756149, 1.873750786029332316 ) ) ;
#212858 = CARTESIAN_POINT ( 'NONE',  ( 4.371826309796801979, 2.140994599346605742, -0.5347268394074317088 ) ) ;
#212859 = EDGE_CURVE ( 'NONE', #138011, #30458, #96418, .T. ) ;
#212860 = CARTESIAN_POINT ( 'NONE',  ( 3.276612781706738087, -1.315965827422488132, 1.771305981150771647 ) ) ;
#212861 = CARTESIAN_POINT ( 'NONE',  ( -11.89317557362571698, 12.33724156162407226, 1.599935658896036283 ) ) ;
#212862 = CARTESIAN_POINT ( 'NONE',  ( 1.523922206041250949, -1.897707704667614959, 0.2351830868887184178 ) ) ;
#212863 = DIRECTION ( 'NONE',  ( 0.000000000000000000, 1.000000000000000000, 0.000000000000000000 ) ) ;
#212864 = CARTESIAN_POINT ( 'NONE',  ( 9.317477881089539338, 11.89347683273640932, 1.599625672291279388 ) ) ;
#212865 = CARTESIAN_POINT ( 'NONE',  ( 4.035645461687249913, 1.950487776689105335, -0.6946759356915441774 ) ) ;
#212866 = AXIS2_PLACEMENT_3D ( 'NONE', #51960, #119143, #53009 ) ;
#212868 = CARTESIAN_POINT ( 'NONE',  ( 1.340939272977889951, 0.4221563536682856332, 2.119910705745978508 ) ) ;
#212867 = LINE ( 'NONE', #178270, #66307 ) ;
#212869 = CARTESIAN_POINT ( 'NONE',  ( 3.386445149735781257, -0.4294187885149694517, -2.148908265708626697 ) ) ;
#212870 = CARTESIAN_POINT ( 'NONE',  ( 8.374132434735052755, 12.92157160716627295, -0.7998128361456352531 ) ) ;
#212871 = EDGE_CURVE ( 'NONE', #180616, #97371, #68685, .T. ) ;
#212872 =( NAMED_UNIT ( * ) PLANE_ANGLE_UNIT ( ) SI_UNIT ( $, .RADIAN. ) );
#212873 = CARTESIAN_POINT ( 'NONE',  ( -0.1081551476993485722, 7.159877756659424719, 1.998460492244615638 ) ) ;
#212874 = CARTESIAN_POINT ( 'NONE',  ( 4.538947565524982686, 8.517465603079630299, 0.000000000000000000 ) ) ;
#212875 = CARTESIAN_POINT ( 'NONE',  ( 1.364683531249997417, 14.29687500034140157, 2.602085213965210642E-15 ) ) ;
#212876 = CARTESIAN_POINT ( 'NONE',  ( -5.490125858891038213, 5.369844688319787451, -0.7998128361456362523 ) ) ;
#212878 = ADVANCED_FACE ( 'NONE', ( #211840 ), #79719, .F. ) ;
#212877 = PRODUCT_DEFINITION_CONTEXT ( 'detailed design', #110207, 'design' ) ;
#212879 = CARTESIAN_POINT ( 'NONE',  ( 0.6510177983308338412, 0.9963039324867200008, 1.753029211773032392 ) ) ;
#212881 = CARTESIAN_POINT ( 'NONE',  ( -9.110716038703348119, 12.61262389758715408, 1.082531754730560403 ) ) ;
#212880 = CIRCLE ( 'NONE', #60756, 0.07999999999999998779 ) ;
#212882 = CARTESIAN_POINT ( 'NONE',  ( 4.909070852169226562, -1.665950775781706028, 1.228889460859562854 ) ) ;
#212883 = CARTESIAN_POINT ( 'NONE',  ( 3.703666587441448943, -0.5581696590808477021, 1.843871709287647764 ) ) ;
#212884 = CARTESIAN_POINT ( 'NONE',  ( 5.747700551816460113, 2.085811977426319519, -0.3625847027708250514 ) ) ;
#212885 = CARTESIAN_POINT ( 'NONE',  ( 6.094553744542824170, 7.069066442510145265, 1.199719254218462483 ) ) ;
#212886 = CARTESIAN_POINT ( 'NONE',  ( -1.364683531250010740, 5.530208333674750953, 0.7879004041258379498 ) ) ;
#212887 = CARTESIAN_POINT ( 'NONE',  ( 3.889471302351163562, -1.821405649934451532, 0.7496272025103620784 ) ) ;
#212888 = CARTESIAN_POINT ( 'NONE',  ( 5.648434673080700463, -1.810194131346474222, 1.406188067625735449 ) ) ;
#212889 = CARTESIAN_POINT ( 'NONE',  ( 4.002439121739418404, -0.5745171773131328985, -1.733004836422600725 ) ) ;
#212890 = AXIS2_PLACEMENT_3D ( 'NONE', #11508, #83706, #98914 ) ;
#212891 = CARTESIAN_POINT ( 'NONE',  ( 6.617788377246179188, 8.814115421577600529, -1.443375672974078761 ) ) ;
#212892 = CARTESIAN_POINT ( 'NONE',  ( 4.812781342726858647, 6.637997537979888563, 1.443375672974062551 ) ) ;
#212893 = CARTESIAN_POINT ( 'NONE',  ( -6.200875153403786477, 8.327716660428123419, -1.599625672291271394 ) ) ;
#212894 = CARTESIAN_POINT ( 'NONE',  ( 4.681308178468477799, 8.683552984847038303, 0.000000000000000000 ) ) ;
#212895 = ORIENTED_EDGE ( 'NONE', *, *, #71271, .F. ) ;
#212896 = CARTESIAN_POINT ( 'NONE',  ( 5.677995041854309477, 1.982684118255732875, -0.3484467016405675688 ) ) ;
#212897 = CARTESIAN_POINT ( 'NONE',  ( 5.959697520924294167, -2.181652697926935502, -0.7244182876006750593 ) ) ;
#212898 = CARTESIAN_POINT ( 'NONE',  ( 4.645332984504850771, 1.754159843842403976, -0.8783796436172899291 ) ) ;
#212899 = CARTESIAN_POINT ( 'NONE',  ( -6.124532705071231931, 8.168374127381657246, -1.599625672291263179 ) ) ;
#212900 = CARTESIAN_POINT ( 'NONE',  ( -4.029797971759847997, 5.724516938518342535, -1.599625672291256295 ) ) ;
#212901 = FILL_AREA_STYLE_COLOUR ( '', #181897 ) ;
#212902 = CARTESIAN_POINT ( 'NONE',  ( -6.448838341955544173, 7.552674816150118708, 1.199719254218452047 ) ) ;
#212904 = CARTESIAN_POINT ( 'NONE',  ( 0.08069323953814251660, -0.1329233695197447052, -1.840450602299897431 ) ) ;
#212903 = CARTESIAN_POINT ( 'NONE',  ( 0.8200051061889235271, 1.242435332701301132, -1.681397122352365603 ) ) ;
#212905 = CARTESIAN_POINT ( 'NONE',  ( -0.006158830626153827259, 7.078243236992583398, 2.121324627965421872 ) ) ;
#212906 = CARTESIAN_POINT ( 'NONE',  ( 6.580031058444741454, -1.904989947508778814, -0.3762313139713204801 ) ) ;
#212907 = CARTESIAN_POINT ( 'NONE',  ( -0.2102771530458094895, 1.993718876163485421, -2.617492801249762913 ) ) ;
#212908 = CARTESIAN_POINT ( 'NONE',  ( 0.6963323360776455528, 1.421588922443246084, 1.003805163531448441 ) ) ;
#212909 = CARTESIAN_POINT ( 'NONE',  ( 6.636879889089462026, 7.701780277814560982, -1.199719254218446718 ) ) ;
#212910 = CARTESIAN_POINT ( 'NONE',  ( 1.556029036868112669, 0.5000000000000007772, -1.827231139298829410 ) ) ;
#212911 = CARTESIAN_POINT ( 'NONE',  ( 1.699380632523245449, -0.5835770076011400631, 1.623301926564212794 ) ) ;
#212912 = CARTESIAN_POINT ( 'NONE',  ( 1.452940684028160234, -1.882004992133184285, -1.122693704575933316 ) ) ;
#212913 = CARTESIAN_POINT ( 'NONE',  ( 4.565167970240332274, -1.970479184476851886, -0.9938812724585781577 ) ) ;
#212914 = CARTESIAN_POINT ( 'NONE',  ( 1.499139249613313574, 0.4210003976099167544, 2.129699363925404487 ) ) ;
#212915 = CARTESIAN_POINT ( 'NONE',  ( 0.3283667639546791195, 1.746078182827022429, 0.5332771064449209897 ) ) ;
#212916 = CARTESIAN_POINT ( 'NONE',  ( 2.677094534585529928, 1.813448998079300489, -1.092781719356890946 ) ) ;
#212917 = CARTESIAN_POINT ( 'NONE',  ( 4.487385655998878065, 6.258369236797239665, 1.443375672974062551 ) ) ;
#212918 = ORIENTED_EDGE ( 'NONE', *, *, #205156, .F. ) ;
#212920 = CARTESIAN_POINT ( 'NONE',  ( -0.6823417656250003738, -0.2197916663252488800, -1.181850606188749264 ) ) ;
#212919 = CARTESIAN_POINT ( 'NONE',  ( 2.982263410219893274, -2.258884913406122408, -0.3895283529634691599 ) ) ;
#212921 = CARTESIAN_POINT ( 'NONE',  ( 4.207107738942202246, 3.802713871720993399, 1.214306433183764966E-14 ) ) ;
#212922 = CARTESIAN_POINT ( 'NONE',  ( 3.506755287428983792, 7.242964935309132990, 1.040834085586084257E-14 ) ) ;
#212923 = CARTESIAN_POINT ( 'NONE',  ( 4.793709693897413082, 2.072883653632663137, -0.7987435787581667057 ) ) ;
#212924 = CARTESIAN_POINT ( 'NONE',  ( -7.890482213473404727, 8.307910125248191946, 0.7216878364870578100 ) ) ;
#212925 = CARTESIAN_POINT ( 'NONE',  ( 3.524756749872944628, 7.056040608253000279, -0.7216878364870267237 ) ) ;
#212926 = CARTESIAN_POINT ( 'NONE',  ( -7.822691444960716112, 8.228820895316715678, -0.7216878364870267237 ) ) ;
#212927 = CARTESIAN_POINT ( 'NONE',  ( 5.885648082108200896, 6.039213315313952002, 0.7216878364870328300 ) ) ;
#212928 = ORIENTED_EDGE ( 'NONE', *, *, #30893, .T. ) ;
#212929 = CARTESIAN_POINT ( 'NONE',  ( 3.235000160576475992, 2.016597019841442240, -0.002811030766311505089 ) ) ;
#212931 = CARTESIAN_POINT ( 'NONE',  ( 1.727463565662648026, 0.1559948080240464718, -2.056756566214789306 ) ) ;
#212930 = CARTESIAN_POINT ( 'NONE',  ( 7.396136491454752715, 8.587579647240744407, 1.199719254218462483 ) ) ;
#212932 = DIRECTION ( 'NONE',  ( 1.000000000000000000, 0.000000000000000000, 0.000000000000000000 ) ) ;
#212933 = CARTESIAN_POINT ( 'NONE',  ( 5.112833325684902341, 7.058334528089426740, -1.443375672974078761 ) ) ;
#212934 = CARTESIAN_POINT ( 'NONE',  ( 0.1100172516615156165, 7.047065462482140497, 3.945011421259203566 ) ) ;
#212935 = CARTESIAN_POINT ( 'NONE',  ( -1.364683531250010295, 3.780208333674750953, 0.7879004041258379498 ) ) ;
#212936 = CARTESIAN_POINT ( 'NONE',  ( 5.033237522093748417, -1.548190877955179179, -1.551241237171486098 ) ) ;
#212937 = CARTESIAN_POINT ( 'NONE',  ( 1.986954140179174155, -2.015912935764123670, 0.05229865529512293942 ) ) ;
#212938 = CARTESIAN_POINT ( 'NONE',  ( 1.100829259350871281, -0.4471758257712907247, 1.786007343351428966 ) ) ;
#212939 = ADVANCED_FACE ( 'NONE', ( #113369 ), #158849, .T. ) ;
#212940 = CARTESIAN_POINT ( 'NONE',  ( 8.294891053462476904, 8.571794405328034827, 1.040834085586084257E-14 ) ) ;
#212941 = CARTESIAN_POINT ( 'NONE',  ( 5.702125722003772879, -1.825762228975034596, 0.002264948092654816680 ) ) ;
#212942 = CARTESIAN_POINT ( 'NONE',  ( 5.660779783930850684, 1.203351582566011047, 1.617819807990819481 ) ) ;
#212943 = CARTESIAN_POINT ( 'NONE',  ( -8.552495972122143186, 8.872333477097637200, 0.7998128361456462443 ) ) ;
#212945 = CARTESIAN_POINT ( 'NONE',  ( -4.769436176957319695, 8.786368983084006601, 0.7998128361456281477 ) ) ;
#212944 = CARTESIAN_POINT ( 'NONE',  ( 4.909165057579100377, 1.966063467186284663, 1.119528758242648525 ) ) ;
#212946 = CARTESIAN_POINT ( 'NONE',  ( 0.8386649464857205416, 2.075244960028700181, 0.3580382472886770584 ) ) ;
#212947 = CARTESIAN_POINT ( 'NONE',  ( -6.261886844665283114, 8.398896966899865646, 1.599625672291269396 ) ) ;
#212948 = CARTESIAN_POINT ( 'NONE',  ( 4.510256325466165173, 2.069976601481211542, -0.04757507122059301263 ) ) ;
#212949 = CARTESIAN_POINT ( 'NONE',  ( 9.402743226277308963, 10.92862083786708816, -1.199719254218446718 ) ) ;
#212950 = CARTESIAN_POINT ( 'NONE',  ( -3.145840728001146669, 6.444277940974754593, 0.6115128566374624652 ) ) ;
#212951 = CARTESIAN_POINT ( 'NONE',  ( 13.76511073782748262, 20.33492760793704690, 12.33038967882342085 ) ) ;
#212952 = CARTESIAN_POINT ( 'NONE',  ( -7.153898609505128015, 11.49796547773133604, 0.7998128361456481317 ) ) ;
#212953 = CARTESIAN_POINT ( 'NONE',  ( 7.334597915313080918, 9.580116872663850813, 1.040834085586084257E-14 ) ) ;
#212954 = CARTESIAN_POINT ( 'NONE',  ( 4.968100067739229075, 6.607231601306259527, -1.242533411653036879 ) ) ;
#212955 = CARTESIAN_POINT ( 'NONE',  ( -9.164948653157990677, 11.71552606681625619, -1.443375672974059665 ) ) ;
#212956 = CARTESIAN_POINT ( 'NONE',  ( 2.109928881651984778, 1.720655366031418332, 1.405045424887063410 ) ) ;
#212957 = DIRECTION ( 'NONE',  ( -0.000000000000000000, -1.000000000000000000, -0.000000000000000000 ) ) ;
#212958 = CARTESIAN_POINT ( 'NONE',  ( -5.586841817283045408, 8.675676665875643678, 1.199719254218454489 ) ) ;
#212959 = CARTESIAN_POINT ( 'NONE',  ( 4.937140493670735708, 8.911747675924535983, -0.7998128361456281477 ) ) ;
#212960 = CARTESIAN_POINT ( 'NONE',  ( 3.754310534785664899, -1.959519245081872585, -0.09869234604030494018 ) ) ;
#212961 = CARTESIAN_POINT ( 'NONE',  ( 5.124091990960999432, 8.065525525174782828, -1.199719254218452047 ) ) ;
#212962 = CARTESIAN_POINT ( 'NONE',  ( -4.053570677780473197, 7.570253647979210854, -0.4034679714342986889 ) ) ;
#212963 = CARTESIAN_POINT ( 'NONE',  ( 5.020596955762157698, 4.751784624677624080, 1.040834085586084257E-14 ) ) ;
#212964 = CARTESIAN_POINT ( 'NONE',  ( -6.292392690518223475, 6.513748691792265788, -0.7216878364870338292 ) ) ;
#212965 = CARTESIAN_POINT ( 'NONE',  ( -7.714226216495749355, 8.102278128774251797, 1.040834085586084257E-14 ) ) ;
#212966 = CARTESIAN_POINT ( 'NONE',  ( 2.672263739372262137, 2.109986773948614225, -0.2121620573234672125 ) ) ;
#212967 = CARTESIAN_POINT ( 'NONE',  ( -6.017840079619296567, 8.114175741012878973, -1.599625672291271394 ) ) ;
#212968 = CARTESIAN_POINT ( 'NONE',  ( 4.223607183596161718, -2.069420184152844566, 0.6248923283326962563 ) ) ;
#212969 = CARTESIAN_POINT ( 'NONE',  ( 2.524749765808989466, -1.717266272480859834, 0.6646640004178903105 ) ) ;
#212970 = CARTESIAN_POINT ( 'NONE',  ( -4.616994038156231106, 6.938643078242441753, 1.201688966319388374 ) ) ;
#212971 = CARTESIAN_POINT ( 'NONE',  ( 1.364683531249986537, 0.4677083336747514530, -0.7879004041258309554 ) ) ;
#212972 = CARTESIAN_POINT ( 'NONE',  ( 6.017484387666114820, -0.9725936433230500944, -1.442976214814440716 ) ) ;
#212973 = CARTESIAN_POINT ( 'NONE',  ( 11.02381569330252908, 2.441452740530748233, -3.988656969163989707 ) ) ;
#212974 = CARTESIAN_POINT ( 'NONE',  ( 5.070386261830877928, 5.978167395966564435, -1.082531754730548412 ) ) ;
#212975 = CARTESIAN_POINT ( 'NONE',  ( 11.00595142344305444, 9.990095813384931134, -1.443824005414910072 ) ) ;
#212976 = CARTESIAN_POINT ( 'NONE',  ( 2.922914210685311431, 2.035003303901411265, 0.7295308445595325431 ) ) ;
#212977 = TOROIDAL_SURFACE ( 'NONE', #133559, 11.29999999999999893, 0.2000000000000000111 ) ;
#212978 = CARTESIAN_POINT ( 'NONE',  ( 4.921249881687197458, 0.7690040753521177885, 1.863882819927860535 ) ) ;
#212979 = CARTESIAN_POINT ( 'NONE',  ( -9.625925875578284163, 10.33259439770390564, 1.040834085586084257E-14 ) ) ;
#212980 = CARTESIAN_POINT ( 'NONE',  ( 2.799875798528407511, -0.6792266858460673795, 2.052276964324008635 ) ) ;
#212981 =( BOUNDED_CURVE ( )  B_SPLINE_CURVE ( 2, ( #203313, #47795, #179904, #31527, #97601 ),
 .UNSPECIFIED., .F., .T. ) 
 B_SPLINE_CURVE_WITH_KNOTS ( ( 3, 2, 3 ),
 ( 0.9910714285714286031, 0.9940476190476190688, 1.000000000000000000 ),
 .UNSPECIFIED. ) 
 CURVE ( )  GEOMETRIC_REPRESENTATION_ITEM ( )  RATIONAL_B_SPLINE_CURVE ( ( 0.9330127018922194093, 0.9330127018922194093, 1.000000000000000000, 0.8660254037844387076, 1.000000000000000000 ) ) 
 REPRESENTATION_ITEM ( '' )  );
#212982 = CARTESIAN_POINT ( 'NONE',  ( 2.653541938639871756, 0.5291849669812850321, -1.898919477364902741 ) ) ;
#212983 = CARTESIAN_POINT ( 'NONE',  ( 10.38813158755803556, 2.629643693813619620, 6.007251501586638121 ) ) ;
#212984 = CARTESIAN_POINT ( 'NONE',  ( 4.036618323093550842, -1.688041843851136425, 0.9601762628524412868 ) ) ;
#212988 = ORIENTED_EDGE ( 'NONE', *, *, #211516, .F. ) ;
#212987 = ADVANCED_FACE ( 'NONE', ( #93875 ), #96004, .T. ) ;
#212986 = LINE ( 'NONE', #142716, #153433 ) ;
#212985 = CARTESIAN_POINT ( 'NONE',  ( -10.26315909542058336, 11.07603315418659840, -0.7216878364870267237 ) ) ;
#212989 = CARTESIAN_POINT ( 'NONE',  ( -5.759181390754928742, 9.941071732514568993, 0.000000000000000000 ) ) ;
#212990 = CARTESIAN_POINT ( 'NONE',  ( 3.898851692381625877, 6.706354853490643642, -1.199719254218452047 ) ) ;
#212992 = ORIENTED_EDGE ( 'NONE', *, *, #212743, .F. ) ;
#212991 = CARTESIAN_POINT ( 'NONE',  ( -6.642568916052639771, 6.714361588341672515, 0.000000000000000000 ) ) ;
#212993 = CARTESIAN_POINT ( 'NONE',  ( -8.473482818416670170, 10.90881592628469932, -1.443375672974058777 ) ) ;
#212994 = ADVANCED_FACE ( 'NONE', ( #61348 ), #75670, .F. ) ;
#212995 = CARTESIAN_POINT ( 'NONE',  ( 0.9212656856641410208, 2.039593612490635532, 0.8430313063367624871 ) ) ;
#212996 = CARTESIAN_POINT ( 'NONE',  ( -3.285556943750000514, -1.538541666188708357, -1.896917185911906500 ) ) ;
#212997 = CARTESIAN_POINT ( 'NONE',  ( 4.856279117655732058, -1.961245242753749674, -0.05215834203427943683 ) ) ;
#212998 = CARTESIAN_POINT ( 'NONE',  ( 1.364683531249988535, 4.717708333674756283, -0.7879004041258300672 ) ) ;
#212999 = CARTESIAN_POINT ( 'NONE',  ( -1.499999999999997780, 3.181250000682818602, 1.214306433183764966E-14 ) ) ;
#213000 = CARTESIAN_POINT ( 'NONE',  ( 0.1747926744264677867, 0.7439089246787933263, -1.939883394317852616 ) ) ;
#213001 = CARTESIAN_POINT ( 'NONE',  ( 4.382634408885896171, 1.643497958660003144, -0.8300281608688080404 ) ) ;
#213002 = ORIENTED_EDGE ( 'NONE', *, *, #197493, .T. ) ;
#213003 = CARTESIAN_POINT ( 'NONE',  ( -4.557020949502716471E-14, 1.625000000682779611, 1.414508159514571428 ) ) ;
#213004 = EDGE_CURVE ( 'NONE', #90309, #107434, #196738, .T. ) ;
#213005 = CARTESIAN_POINT ( 'NONE',  ( -8.345207244411405156, 9.694828859023472134, 1.199719254218462483 ) ) ;
#213006 = CARTESIAN_POINT ( 'NONE',  ( 1.500000000000032641, 7.750000000000000000, 9.886859966642587594 ) ) ;
#213007 = CARTESIAN_POINT ( 'NONE',  ( 4.957343421279006179, -1.817532610912236724, 1.092287347377165485 ) ) ;
#213008 = CARTESIAN_POINT ( 'NONE',  ( -5.531188331362556276, 5.962015196429335973, -0.9252058187971325953 ) ) ;
#213009 = CARTESIAN_POINT ( 'NONE',  ( 4.774442650306744085, 8.721933525333202653, -0.7998128361456281477 ) ) ;
#213010 = CARTESIAN_POINT ( 'NONE',  ( 6.415316853601439995, -0.2566941480561866773, 2.044681889290477894 ) ) ;
#213013 = CARTESIAN_POINT ( 'NONE',  ( 3.315785976855676775, 1.165629053876730659, -1.425327459889616177 ) ) ;
#213012 = CARTESIAN_POINT ( 'NONE',  ( 0.2911520677349140884, -1.704046917483082346, 0.7485983125269514149 ) ) ;
#213011 = CARTESIAN_POINT ( 'NONE',  ( -0.4350687514514811616, -5.166862915010145052, -10.91132967064556425 ) ) ;
#213014 = CARTESIAN_POINT ( 'NONE',  ( 8.609591239877852686, 10.00327685373437347, -1.199719254218445830 ) ) ;
#213015 = CARTESIAN_POINT ( 'NONE',  ( -11.06389876992414578, 3.829536045110820464, 3.713591040152699030 ) ) ;
#213016 = CARTESIAN_POINT ( 'NONE',  ( -7.279802135894939852, 7.457800344824362604, -0.7998128361456362523 ) ) ;
#213017 = DIRECTION ( 'NONE',  ( -0.9829311923673912377, -0.1839735607939864959, 0.000000000000000000 ) ) ;
#213018 = CIRCLE ( 'NONE', #161099, 0.08000000000000040412 ) ;
#213019 = CARTESIAN_POINT ( 'NONE',  ( 3.703933201646680828, -0.6411959742554216302, 2.111683309420588905 ) ) ;
#213020 = CARTESIAN_POINT ( 'NONE',  ( 4.534621088391048715, 2.217606307645642261, 0.4472613530076152699 ) ) ;
#213021 = CARTESIAN_POINT ( 'NONE',  ( -5.572037945536512105, 9.444535336527177805, 0.000000000000000000 ) ) ;
#213022 = CARTESIAN_POINT ( 'NONE',  ( 5.484552789610383172, -1.142847587564936207, 1.405643779654427661 ) ) ;
#213023 = CARTESIAN_POINT ( 'NONE',  ( 5.155460239800898847, 1.844409812803897264, -0.5174689040137578910 ) ) ;
#213024 = CARTESIAN_POINT ( 'NONE',  ( -1.364683531250012516, 5.051041667008085767, -0.7879004041258300672 ) ) ;
#213025 = CARTESIAN_POINT ( 'NONE',  ( 5.805500895539822181, -0.4530025297027094888, 1.814837910242727226 ) ) ;
#213026 = CARTESIAN_POINT ( 'NONE',  ( 5.898848723475273559, 0.3636257040535681995, 1.824992291636283293 ) ) ;
#213027 = CARTESIAN_POINT ( 'NONE',  ( -0.0001326642102265163461, 15.43055640418811514, 11.92506554388277706 ) ) ;
#213029 = EDGE_CURVE ( 'NONE', #7182, #204270, #41216, .T. ) ;
#213028 = CIRCLE ( 'NONE', #112782, 11.49999999999998934 ) ;
#213030 = CARTESIAN_POINT ( 'NONE',  ( 6.543818844511720023, 0.6727183027174578056, -1.637219817372371100 ) ) ;
#213031 = B_SPLINE_CURVE_WITH_KNOTS ( 'NONE', 3,
 ( #56720, #139051, #92453, #90294, #27412, #192030 ),
 .UNSPECIFIED., .F., .F.,
 ( 4, 2, 4 ),
 ( 0.000000000000000000, 0.0003072753182893358343, 0.0006145506365786716687 ),
 .UNSPECIFIED. ) ;
#213032 = AXIS2_PLACEMENT_3D ( 'NONE', #48520, #163330, #14910 ) ;
#213033 = CARTESIAN_POINT ( 'NONE',  ( 1.551970632248239612, 1.040795554343958429, 1.727062486439542965 ) ) ;
#213034 = B_SPLINE_CURVE_WITH_KNOTS ( 'NONE', 3,
 ( #186104, #152549, #206625, #173088, #156836, #174167, #38804, #137387, #203403, #104886 ),
 .UNSPECIFIED., .F., .F.,
 ( 4, 3, 3, 4 ),
 ( 0.000000000000000000, 4.390531002228115621E-05, 8.388738317900957750E-05, 0.0001586609058613872871 ),
 .UNSPECIFIED. ) ;
#213036 = CARTESIAN_POINT ( 'NONE',  ( 2.438226732591573409, 0.9919046538873840246, -1.857854779501419307 ) ) ;
#213035 = CARTESIAN_POINT ( 'NONE',  ( -9.989660255170729641, 10.54902514065433827, -0.7998128361456291469 ) ) ;
#213037 = CARTESIAN_POINT ( 'NONE',  ( 7.736899214892750010, 12.17813285068358020, 1.040834085586084257E-14 ) ) ;
#213039 = CARTESIAN_POINT ( 'NONE',  ( -7.818248136574758256, 12.27303992597924420, 0.000000000000000000 ) ) ;
#213038 = CARTESIAN_POINT ( 'NONE',  ( -1.500000000000015099, -1.079166666666641961, 0.8660254037844403729 ) ) ;
#213040 = CARTESIAN_POINT ( 'NONE',  ( 1.916276942859599597, -2.019257470013501088, 0.05376132052286108215 ) ) ;
#213041 = CARTESIAN_POINT ( 'NONE',  ( -0.6823417656250212460, 3.051041667008084879, 1.181850606188767472 ) ) ;
#213042 = AXIS2_PLACEMENT_3D ( 'NONE', #111036, #92618, #25439 ) ;
#213043 = CARTESIAN_POINT ( 'NONE',  ( 3.171717870593107058, 5.787755718078879674, -1.199719254218446718 ) ) ;
#213044 = CARTESIAN_POINT ( 'NONE',  ( 2.935029080331118756, 0.2613785356864756770, 2.145644965459513109 ) ) ;
#213045 = CARTESIAN_POINT ( 'NONE',  ( 6.610000000000028741, 1.211438232176115237, 2.390254139237833808 ) ) ;
#213047 = DIRECTION ( 'NONE',  ( 5.578564026256490882E-16, 1.000000000000000000, 9.066213480720158442E-32 ) ) ;
#213046 = CARTESIAN_POINT ( 'NONE',  ( 5.969332771766739931, 10.18624834369502885, -0.7998128361456481317 ) ) ;
#213048 = CARTESIAN_POINT ( 'NONE',  ( 10.03267048398825168, 10.80712977418221676, 0.000000000000000000 ) ) ;
#213049 = CARTESIAN_POINT ( 'NONE',  ( 8.400184771233881520, 15.16344228256336812, -8.571051625424484399 ) ) ;
#213050 = CARTESIAN_POINT ( 'NONE',  ( -7.049876689426106680, 9.247942109129029475, -1.443375672974059665 ) ) ;
#213051 = CARTESIAN_POINT ( 'NONE',  ( 0.6823417656249882723, 0.6760416670080898749, -1.181850606188749264 ) ) ;
#213052 = CARTESIAN_POINT ( 'NONE',  ( 0.4510473619779230003, -1.854578567552306767, -1.167393260480112493 ) ) ;
#213053 = CARTESIAN_POINT ( 'NONE',  ( 0.006768871532346439589, 8.210909518262138107, 2.038649385027043959 ) ) ;
#213054 = CARTESIAN_POINT ( 'NONE',  ( 2.624197652063056996, -1.302182479666073700, -1.850046142848650321 ) ) ;
#213055 = CARTESIAN_POINT ( 'NONE',  ( -6.835281999583978418, 11.12624609948998966, -0.7998128361456291469 ) ) ;
#213056 = CARTESIAN_POINT ( 'NONE',  ( -3.104453987404957260, 6.565687385373657925, -0.7216878364870257245 ) ) ;
#213057 = CARTESIAN_POINT ( 'NONE',  ( 1.364683531249990311, 2.946875000341416140, 1.214306433183764966E-14 ) ) ;
#213058 = CARTESIAN_POINT ( 'NONE',  ( 4.759808938472720463, 8.174556087920027636, -0.7576060450402433144 ) ) ;
#213059 = CARTESIAN_POINT ( 'NONE',  ( 1.499999999999997113, 11.39583333333333393, -0.8660254037844378194 ) ) ;
#213060 = CARTESIAN_POINT ( 'NONE',  ( 6.034787771858531435, 10.05468647722803865, 0.000000000000000000 ) ) ;
#213061 = CARTESIAN_POINT ( 'NONE',  ( 3.444378845967084324, 0.4270997545614327318, 1.717301222563255791 ) ) ;
#213062 =( BOUNDED_SURFACE ( )  B_SPLINE_SURFACE ( 3, 2, ( 
 ( #87839, #73712, #22805 ),
 ( #188527, #139810, #202624 ),
 ( #170143, #53201, #186386 ),
 ( #55336, #38023, #120411 ),
 ( #171211, #157116, #119332 ),
 ( #20677, #185319, #41240 ),
 ( #122565, #6558, #8705 ),
 ( #153910, #105174, #169078 ) ),
 .UNSPECIFIED., .F., .F., .T. ) 
 B_SPLINE_SURFACE_WITH_KNOTS ( ( 4, 2, 2, 4 ),
 ( 3, 3 ),
 ( 0.000000000000000000, 0.0004924884914732730132, 0.0007387327372099095199, 0.0009849769829465460265 ),
 ( 0.000000000000000000, 1.000000000000000000 ),
 .UNSPECIFIED. ) 
 GEOMETRIC_REPRESENTATION_ITEM ( )  RATIONAL_B_SPLINE_SURFACE ( (
 ( 1.000000000000000000, 0.7045118851637662827, 1.000000000000000000),
 ( 1.000000000000000000, 0.7593505504062139089, 1.000000000000000000),
 ( 1.000000000000000000, 0.8104906253036173736, 1.000000000000000000),
 ( 1.000000000000000000, 0.8722646935499589471, 1.000000000000000000),
 ( 1.000000000000000000, 0.8905178607894793652, 1.000000000000000000),
 ( 1.000000000000000000, 0.9170530604353642756, 1.000000000000000000),
 ( 1.000000000000000000, 0.9248184710077380632, 1.000000000000000000),
 ( 1.000000000000000000, 0.9238795325112880708, 1.000000000000000000) ) ) 
 REPRESENTATION_ITEM ( '' )  SURFACE ( )  );
#213063 = CARTESIAN_POINT ( 'NONE',  ( 6.124089168553260798, -1.220954261165616783, -1.838047742986161026 ) ) ;
#213064 = CARTESIAN_POINT ( 'NONE',  ( -1.364683531250010295, 9.380208333674735499, 0.7879004041258445001 ) ) ;
#213065 = EDGE_LOOP ( 'NONE', ( #14096, #159604, #193739, #156379 ) ) ;
#213066 = CARTESIAN_POINT ( 'NONE',  ( -7.096767062110449942, 7.244259425409119046, -0.7998128361456362523 ) ) ;
#213067 = CARTESIAN_POINT ( 'NONE',  ( 5.413685477598253470, -1.281375732037979942, -1.556898226837098331 ) ) ;
#213068 = ORIENTED_EDGE ( 'NONE', *, *, #209086, .T. ) ;
#213069 = CARTESIAN_POINT ( 'NONE',  ( 2.887410755087606695, 1.321643875934110479, 1.324118206929347563 ) ) ;
#213070 = CARTESIAN_POINT ( 'NONE',  ( 3.309495622959734096, -1.689761761210720525, -1.195817184978978265 ) ) ;
#213071 = CARTESIAN_POINT ( 'NONE',  ( -3.022498986271275001, 2.800000000000024691, 2.500000000000011102 ) ) ;
#213072 = PRESENTATION_STYLE_ASSIGNMENT (( #164346 ) ) ;
#213073 = DIRECTION ( 'NONE',  ( -0.000000000000000000, 1.000000000000000000, -0.000000000000000000 ) ) ;
#213074 = CARTESIAN_POINT ( 'NONE',  ( -9.481348452320373710, -9.006862915010128035, 0.5950054837411764552 ) ) ;
#213075 = CARTESIAN_POINT ( 'NONE',  ( -1.364683531249997417, 4.571875000341417028, 1.214306433183764966E-14 ) ) ;
#213076 = CARTESIAN_POINT ( 'NONE',  ( 1.142663480069527671, 1.843847066288730074, 0.5072560978593986247 ) ) ;
#213077 = CARTESIAN_POINT ( 'NONE',  ( 2.330453122711079850, -1.209328770571056921, 1.544706564130463811 ) ) ;
#213078 = CARTESIAN_POINT ( 'NONE',  ( 0.9661724576192336489, 1.646585359754201061, 1.163093122096101162 ) ) ;
#213079 = CARTESIAN_POINT ( 'NONE',  ( -4.960304097753355457, 6.880383762169266504, 1.599625672291263179 ) ) ;
#213081 = CARTESIAN_POINT ( 'NONE',  ( -1.274519002043997595, 3.715789678311091748, -0.4828173461639007069 ) ) ;
#213080 = CARTESIAN_POINT ( 'NONE',  ( 7.235247531187115833, 11.59287255302699648, -0.7998128361456291469 ) ) ;
#213082 = CARTESIAN_POINT ( 'NONE',  ( 6.784453690597813669, -1.932871751835860241, -0.3867854297147227394 ) ) ;
#213083 = CARTESIAN_POINT ( 'NONE',  ( 0.6823417656249899377, 2.842708333674753618, 1.181850606188765695 ) ) ;
#213084 = CARTESIAN_POINT ( 'NONE',  ( 1.758066197707741640, 0.7666020408202559588, -1.861725765494412599 ) ) ;
#213085 = AXIS2_PLACEMENT_3D ( 'NONE', #101199, #205090, #173711 ) ;
#213087 = CARTESIAN_POINT ( 'NONE',  ( 2.003655485592752861, -2.052825532818176590, 0.5177380972332337183 ) ) ;
#213086 = CARTESIAN_POINT ( 'NONE',  ( -6.805829924380121909, 8.963220883242035697, 1.443375672974078761 ) ) ;
#213088 = CARTESIAN_POINT ( 'NONE',  ( -7.285838599102589797E-14, 7.078193277237590841, -2.121339347286493648 ) ) ;
#213089 = CARTESIAN_POINT ( 'NONE',  ( 3.895033709675084221, 0.3008086390649654662, 2.048262060622765279 ) ) ;
#213090 = CARTESIAN_POINT ( 'NONE',  ( 5.761288931164342486, 5.686201605971993978, -0.7998128361456481317 ) ) ;
#213092 = CARTESIAN_POINT ( 'NONE',  ( 4.864678189204997949, 4.569879397027603929, 0.7998128361456341429 ) ) ;
#213091 = CARTESIAN_POINT ( 'NONE',  ( 5.929650942584956397, 1.031255971971676955, -1.818501217082470145 ) ) ;
#213094 = ORIENTED_EDGE ( 'NONE', *, *, #174269, .F. ) ;
#213093 = CARTESIAN_POINT ( 'NONE',  ( 4.541915102786819425, 0.7800907816924649296, -1.650662693317282770 ) ) ;
#213095 = CARTESIAN_POINT ( 'NONE',  ( 9.673906298550626559, 11.24497775551929557, 1.199719254218452047 ) ) ;
#213096 = CARTESIAN_POINT ( 'NONE',  ( 6.890000000000007674, 7.629137130509070275, 2.600000000000001421 ) ) ;
#213097 = CARTESIAN_POINT ( 'NONE',  ( 10.16976112282614508, 11.75387517088144484, 7.514388995082887490 ) ) ;
#213098 = CARTESIAN_POINT ( 'NONE',  ( 6.387735258934439386, 1.517164627179751646, 1.602757196154185770 ) ) ;
#213099 = CARTESIAN_POINT ( 'NONE',  ( 1.364683531249996529, 10.52604166700806765, 0.7879004041258403923 ) ) ;
#213100 = ORIENTED_EDGE ( 'NONE', *, *, #158732, .F. ) ;
#213101 = CARTESIAN_POINT ( 'NONE',  ( 5.373660369522260005, 0.3689257714810100786, -1.876182517032434216 ) ) ;
#213102 = CARTESIAN_POINT ( 'NONE',  ( -4.322352044658376968, 3.937165561723182883, 0.7998128361456341429 ) ) ;
#213103 = CARTESIAN_POINT ( 'NONE',  ( 8.118635056484817980, 8.366162408854107113, 0.7998128361456481317 ) ) ;
#213104 = CARTESIAN_POINT ( 'NONE',  ( -1.360316468750028651, 1.692708333674762144, 0.7853790794158620470 ) ) ;
#213105 = CARTESIAN_POINT ( 'NONE',  ( 3.321384445223597659, 6.818772919495430074, -0.7216878364870267237 ) ) ;
#213106 = CARTESIAN_POINT ( 'NONE',  ( -3.449547071718232605, 5.999999999999998224, -2.024999999999999911 ) ) ;
#213107 = DIRECTION ( 'NONE',  ( 5.176899690512889973E-31, -0.6000000000000069722, -0.7999999999999948264 ) ) ;
#213108 = CARTESIAN_POINT ( 'NONE',  ( 0.7844012160764175512, 1.623964078452419857, -0.8677550623670119423 ) ) ;
#213109 = VERTEX_POINT ( 'NONE', #212910 ) ;
#213110 = EDGE_CURVE ( 'NONE', #124865, #188409, #70888, .T. ) ;
#213111 = CARTESIAN_POINT ( 'NONE',  ( -7.774674742793745708, 8.035151719539642912, 0.7998128361456341429 ) ) ;
#213112 = CARTESIAN_POINT ( 'NONE',  ( 4.446469999505775483, 0.4968273501132040026, 1.803309644091706021 ) ) ;
#213113 = CARTESIAN_POINT ( 'NONE',  ( -11.04536101718726293, 13.50462094045401962, 1.099999999999999201 ) ) ;
#213114 = CARTESIAN_POINT ( 'NONE',  ( 4.650083499807233345, 5.295740330745369207, -1.000000000000000888 ) ) ;
#213115 = CIRCLE ( 'NONE', #171704, 0.08000000000000005718 ) ;
#213116 = DIRECTION ( 'NONE',  ( 3.330669073875478989E-16, -3.540251991789410786E-16, -1.000000000000000000 ) ) ;
#213117 = CARTESIAN_POINT ( 'NONE',  ( -7.104109303880803417, 8.350844278358124484, 1.082531754730549967 ) ) ;
#213118 = CIRCLE ( 'NONE', #26367, 0.8299999999999999600 ) ;
#213119 = CARTESIAN_POINT ( 'NONE',  ( 4.202137545231717120, 6.989912005157271402, 1.199719254218462483 ) ) ;
#213120 = CARTESIAN_POINT ( 'NONE',  ( 1.129674139269299049, 1.899472608897791348, -0.5201393403096374879 ) ) ;
#213121 = CARTESIAN_POINT ( 'NONE',  ( 1.915638884950950027, -1.319244919589783516, -1.525031147761625405 ) ) ;
#213122 = CARTESIAN_POINT ( 'NONE',  ( -7.862839020921525091, 11.26073039346208660, -1.199719254218446718 ) ) ;
#213123 = CARTESIAN_POINT ( 'NONE',  ( 5.529746549527311039, 7.544733289238903851, -1.599625672291281386 ) ) ;
#213124 = FACE_OUTER_BOUND ( 'NONE', #203545, .T. ) ;
#213125 = CARTESIAN_POINT ( 'NONE',  ( 2.256057974219495499, 0.9384471748680022207, 1.980482673072603284 ) ) ;
#213126 = CARTESIAN_POINT ( 'NONE',  ( 9.574107819074903603, 3.767510227260138844, -7.159700062698973078 ) ) ;
#213127 = CARTESIAN_POINT ( 'NONE',  ( -9.982881178363895103, 10.54111621771303753, 1.040834085586084257E-14 ) ) ;
#213128 = CARTESIAN_POINT ( 'NONE',  ( 1.500000000000035971, 7.750000000000000000, 10.86128356754324109 ) ) ;
#213129 = CARTESIAN_POINT ( 'NONE',  ( 4.148431816101584957, 6.823292304551739740, -1.082531754730548412 ) ) ;
#213130 = CARTESIAN_POINT ( 'NONE',  ( 5.261973015879598314, 5.311592404713873172, -0.7216878364870458196 ) ) ;
#213131 = CARTESIAN_POINT ( 'NONE',  ( 9.420217803396747414, 9.884675613584706255, 0.7998128361456462443 ) ) ;
#213132 = ADVANCED_FACE ( 'NONE', ( #10446 ), #142630, .F. ) ;
#213133 = CARTESIAN_POINT ( 'NONE',  ( -4.970620135051034616, 8.062850052469723749, -1.111334424012894617 ) ) ;
#213134 = CARTESIAN_POINT ( 'NONE',  ( 6.861835142292143530, 8.138467433163244280, 1.082531754730549967 ) ) ;
#213135 = EDGE_LOOP ( 'NONE', ( #35051, #136850, #7664, #28139 ) ) ;
#213136 = ORIENTED_EDGE ( 'NONE', *, *, #56646, .T. ) ;
#213138 = CARTESIAN_POINT ( 'NONE',  ( 1.875641098811844154, 0.3420332329174725072, -1.983669356598726674 ) ) ;
#213137 = CARTESIAN_POINT ( 'NONE',  ( 5.249485218566787736, 1.838879873951341004, -0.09611505855997715120 ) ) ;
#213139 = CARTESIAN_POINT ( 'NONE',  ( 3.198860821731682513, -1.541234334381531568, -1.705209785003541700 ) ) ;
#213141 = CARTESIAN_POINT ( 'NONE',  ( 1.568971434307638857, 1.638126988201485279, 0.8830449202173286105 ) ) ;
#213140 = CARTESIAN_POINT ( 'NONE',  ( -0.4019237886467001974, 10.05133545031537246, 1.500000000000001998 ) ) ;
#213142 = CARTESIAN_POINT ( 'NONE',  ( -1.642778471874998480, -1.801041666188708090, 2.845375778867863303 ) ) ;
#213143 = PRESENTATION_STYLE_ASSIGNMENT (( #131953 ) ) ;
#213144 = CARTESIAN_POINT ( 'NONE',  ( 5.765855477156511810, 0.5488314196105298359, -1.831976909803390896 ) ) ;
#213145 = CARTESIAN_POINT ( 'NONE',  ( -8.483651433849100698, 10.92067931095586886, 1.599625672291269396 ) ) ;
#213146 = CARTESIAN_POINT ( 'NONE',  ( -5.424670859243583720, 8.382514198209223721, 1.082531754730550855 ) ) ;
#213148 = CARTESIAN_POINT ( 'NONE',  ( 3.871829239884491791, 1.038646522470688671, 1.555605274479121114 ) ) ;
#213147 = CARTESIAN_POINT ( 'NONE',  ( 4.651946873442760477, 0.8016356570225026124, 1.931162265472508910 ) ) ;
#213149 = CARTESIAN_POINT ( 'NONE',  ( 6.480434237652115570, 10.50433101066207442, 0.7216878364870438212 ) ) ;
#213150 = CARTESIAN_POINT ( 'NONE',  ( 5.513187957602974976, -1.795010045117376496, 0.4093405989887277663 ) ) ;
#213151 = CARTESIAN_POINT ( 'NONE',  ( 2.900554798319789906, 5.471398800426671372, 1.199719254218452047 ) ) ;
#213152 = CARTESIAN_POINT ( 'NONE',  ( 0.2721095781817989834, -7.697284395437333337, -10.99684423689256008 ) ) ;
#213153 = CARTESIAN_POINT ( 'NONE',  ( 4.687984124052484880, -0.8092498044112338418, 1.523260386444349468 ) ) ;
#213154 = CARTESIAN_POINT ( 'NONE',  ( -5.052384799386910430, 9.046199365926717917, 1.214306433183764966E-14 ) ) ;
#213155 = CARTESIAN_POINT ( 'NONE',  ( -1.304512053934558738E-16, 4.099999999999999645, 2.350000000000007194 ) ) ;
#213156 = CIRCLE ( 'NONE', #150892, 12.00000000000000178 ) ;
#213157 = CARTESIAN_POINT ( 'NONE',  ( 9.579592329539993401, -9.999999999999994671, -0.07839159645131119070 ) ) ;
#213158 = CARTESIAN_POINT ( 'NONE',  ( 4.680651438812245324, 1.340593046976858771, -1.707629433300766664 ) ) ;
#213159 = CARTESIAN_POINT ( 'NONE',  ( 3.141029808440584326, -1.609794727316344209, 0.8612202190056221784 ) ) ;
#213160 = CARTESIAN_POINT ( 'NONE',  ( 0.7253527386562284018, 0.1980078388067410822, -1.951770168129369543 ) ) ;
#213161 = CARTESIAN_POINT ( 'NONE',  ( 5.454358448847595575, -1.341013495729547644, 1.638584853213326031 ) ) ;
#213163 = CARTESIAN_POINT ( 'NONE',  ( -1.001543065824772872E-14, 4.634375000341418804, 1.575800808251672791 ) ) ;
#213162 = CARTESIAN_POINT ( 'NONE',  ( 5.759400667030329934, 2.259083744078540956, -0.3884743064591251738 ) ) ;
#213164 = DIRECTION ( 'NONE',  ( -5.578564026256490882E-16, -1.000000000000000000, -9.066213480720158442E-32 ) ) ;
#213165 = CARTESIAN_POINT ( 'NONE',  ( 7.730120138085914583, 12.17022392774227768, 0.7998128361456462443 ) ) ;
#213166 = AXIS2_PLACEMENT_3D ( 'NONE', #105904, #155682, #188164 ) ;
#213167 = CARTESIAN_POINT ( 'NONE',  ( 1.875790325896836919, 0.3594715711359474652, -2.089634487563592824 ) ) ;
#213168 = CARTESIAN_POINT ( 'NONE',  ( -4.202664430556263930, 5.926194473780837413, 1.443375672974064550 ) ) ;
#213169 = CARTESIAN_POINT ( 'NONE',  ( 4.204437033569277560, 7.919277282557212416, 0.000000000000000000 ) ) ;
#213170 = CARTESIAN_POINT ( 'NONE',  ( -3.429849674132936066, 6.945315686556313040, -0.7216878364870257245 ) ) ;
#213171 = CARTESIAN_POINT ( 'NONE',  ( 6.368071955308375998, -2.155667716570781156, 0.2575352064990812928 ) ) ;
#213173 = CARTESIAN_POINT ( 'NONE',  ( 0.7500000000000006661, 12.19791666734946389, -1.299038105676657340 ) ) ;
#213172 = CARTESIAN_POINT ( 'NONE',  ( 6.983263157960368339, 1.271300847835453940, 2.069154070428773196 ) ) ;
#213175 = VERTEX_POINT ( 'NONE', #65572 ) ;
#213174 = CARTESIAN_POINT ( 'NONE',  ( 2.122025409673257812, -0.4832278914180427876, 2.167962204723080433 ) ) ;
#213176 = CARTESIAN_POINT ( 'NONE',  ( 6.504528880466823537, -1.955196382115764964, 0.4926337920100053447 ) ) ;
#213178 = CARTESIAN_POINT ( 'NONE',  ( 5.981316409642544407, -0.05633626937831189702, 2.061977559458886056 ) ) ;
#213177 = CARTESIAN_POINT ( 'NONE',  ( 3.822509244049070887, 6.547012320444182798, -1.199719254218452047 ) ) ;
#213180 = CARTESIAN_POINT ( 'NONE',  ( -1.737499999999997824, -2.391666666666667052, 3.009438278150925683 ) ) ;
#213179 = CARTESIAN_POINT ( 'NONE',  ( 5.529746549527311039, 7.544733289238903851, -1.599625672291281386 ) ) ;
#213181 = CARTESIAN_POINT ( 'NONE',  ( 6.886615681098613884, 6.999082814228660077, 0.000000000000000000 ) ) ;
#213182 = CARTESIAN_POINT ( 'NONE',  ( 3.285556943749998737, -2.792708332855373676, -1.896917185911906500 ) ) ;
#213183 = CARTESIAN_POINT ( 'NONE',  ( 0.2333540202161610289, 7.629137130509112907, -2.645727818377396900 ) ) ;
#213184 = CARTESIAN_POINT ( 'NONE',  ( 5.478019777291557979, -1.797689181224306321, -0.3974485807837144224 ) ) ;
#213185 = AXIS2_PLACEMENT_3D ( 'NONE', #212850, #12522, #110108 ) ;
#213186 = ADVANCED_FACE ( 'NONE', ( #131719 ), #98485, .F. ) ;
#213187 = CARTESIAN_POINT ( 'NONE',  ( 6.030679399980265920, 5.930214142932100252, -0.7998128361456281477 ) ) ;
#213188 = CARTESIAN_POINT ( 'NONE',  ( -0.4500000000000163869, 3.949999999999995293, -0.5000000000000229816 ) ) ;
#213189 = CARTESIAN_POINT ( 'NONE',  ( 1.606044756371062920, -0.6162743471601249690, -1.611104689205801188 ) ) ;
#213190 = CARTESIAN_POINT ( 'NONE',  ( 0.5324358445358172709, 0.5899921999869184308, 1.928256190492839028 ) ) ;
#213191 = CARTESIAN_POINT ( 'NONE',  ( 2.374040334453372925, -0.3969776081079456898, -2.264039395722910353 ) ) ;
#213192 = CARTESIAN_POINT ( 'NONE',  ( 1.364683531249988535, 4.467708333674754506, -0.7879004041258300672 ) ) ;
#213193 = CARTESIAN_POINT ( 'NONE',  ( 2.495744459589462227, 1.747532462024743882, 1.436835450399133407 ) ) ;
#213194 = CARTESIAN_POINT ( 'NONE',  ( 4.020224483524700076, -1.082363273655801095, -1.806513482918799429 ) ) ;
#213195 = CARTESIAN_POINT ( 'NONE',  ( -3.122120512896910505, 6.864500708346841229, 0.7998128361456352531 ) ) ;
#213196 = CARTESIAN_POINT ( 'NONE',  ( 2.389615768203833479, -0.7611923103308501082, 1.597832513397597021 ) ) ;
#213197 = CARTESIAN_POINT ( 'NONE',  ( 5.425234023762710578, 9.481190127698507553, -0.7998128361456291469 ) ) ;
#213198 = CARTESIAN_POINT ( 'NONE',  ( 4.651856102820254968, 7.480896982382013505, -1.082531754730548412 ) ) ;
#213199 = CARTESIAN_POINT ( 'NONE',  ( -4.876128802409253282, 8.840567369452784874, 0.7998128361456481317 ) ) ;
#213200 = CARTESIAN_POINT ( 'NONE',  ( -0.7500000000000006661, 2.358333333333358262, -1.299038105676652011 ) ) ;
#213201 = CARTESIAN_POINT ( 'NONE',  ( 6.363560548480147183, -1.783403785914154049, -1.324293268510617017 ) ) ;
#213202 = CARTESIAN_POINT ( 'NONE',  ( 3.293114190187882429, 1.727671002657789057, 1.348082825637614279 ) ) ;
#213203 = CARTESIAN_POINT ( 'NONE',  ( -4.111146893441842920, 5.819424013814012753, 1.599625672291267398 ) ) ;
#213204 = CARTESIAN_POINT ( 'NONE',  ( 0.05606965051298876818, 7.151966587341790138, -1.999903488157537046 ) ) ;
#213205 = CARTESIAN_POINT ( 'NONE',  ( -3.410126044457033156, -0.03745499569612897872, 0.000000000000000000 ) ) ;
#213206 = CARTESIAN_POINT ( 'NONE',  ( 1.364683531249990311, 3.134375000341423245, 1.214306433183764966E-14 ) ) ;
#213207 = CARTESIAN_POINT ( 'NONE',  ( -1.402160292154681736E-14, 8.421875000341403350, 1.575800808251682339 ) ) ;
#213208 = CARTESIAN_POINT ( 'NONE',  ( -4.284013352238262407, 6.021101549076499637, -1.443375672974053447 ) ) ;
#213209 = CARTESIAN_POINT ( 'NONE',  ( 6.258074605086497932, 0.8102346573028992305, -1.959903593942226685 ) ) ;
#213210 = CARTESIAN_POINT ( 'NONE',  ( -6.319508997745553636, 6.545384383557486530, 0.7216878364870257245 ) ) ;
#213211 = ORIENTED_EDGE ( 'NONE', *, *, #184288, .T. ) ;
#213213 = CARTESIAN_POINT ( 'NONE',  ( -4.826339496784927796, 5.693446170079573321, 1.082531754730560403 ) ) ;
#213212 = CARTESIAN_POINT ( 'NONE',  ( -3.689227196694341515, 7.318199139536432973, -0.7216878364870458196 ) ) ;
#213214 = CARTESIAN_POINT ( 'NONE',  ( 5.494078562035752178, 7.432844293840273231, -1.599625672291262513 ) ) ;
#213215 = CARTESIAN_POINT ( 'NONE',  ( 6.392148736875968851, -0.4980823202534768179, -1.772533436741857260 ) ) ;
#213216 = CARTESIAN_POINT ( 'NONE',  ( 0.2082862676862618501, 7.047992132487147288, -4.030656176649458189 ) ) ;
#213217 = CARTESIAN_POINT ( 'NONE',  ( -0.6823417656249969321, 4.280208333674755394, -1.181850606188749264 ) ) ;
#213218 = CARTESIAN_POINT ( 'NONE',  ( 2.243362625160577384, 1.740107689937436808, 0.04144568419049177860 ) ) ;
#213219 = CARTESIAN_POINT ( 'NONE',  ( -2.486770427477412948, 2.630042260599927850, 11.73951962969540297 ) ) ;
#213220 = CARTESIAN_POINT ( 'NONE',  ( 0.6429252097494702056, -0.2364460082661112295, -1.947484529462916836 ) ) ;
#213221 = CARTESIAN_POINT ( 'NONE',  ( -0.6823417656250003738, -0.4697916663252491021, -1.181850606188749264 ) ) ;
#213222 = DIRECTION ( 'NONE',  ( 0.000000000000000000, 0.000000000000000000, 1.000000000000000000 ) ) ;
#213223 = CARTESIAN_POINT ( 'NONE',  ( 6.368072262247213899, 1.106822706796772193, 1.856716078747308263 ) ) ;
#213224 = CARTESIAN_POINT ( 'NONE',  ( -10.08065090696061716, 11.71951313199760136, -1.199719254218441611 ) ) ;
#213225 = CARTESIAN_POINT ( 'NONE',  ( -6.846504384776765484, 8.050305206070113684, -1.082531754730543083 ) ) ;
#213226 = CARTESIAN_POINT ( 'NONE',  ( 5.577088068215094729, -0.04877400797019536272, -2.161318155665878038 ) ) ;
#213228 = ORIENTED_EDGE ( 'NONE', *, *, #161705, .T. ) ;
#213227 = CARTESIAN_POINT ( 'NONE',  ( -3.471769853551161411, 6.208092708188416076, 1.199719254218452935 ) ) ;
#213229 = CARTESIAN_POINT ( 'NONE',  ( -1.364683531250010295, 4.280208333674753618, 0.7879004041258379498 ) ) ;
#213230 = CARTESIAN_POINT ( 'NONE',  ( 5.659438124648599633, 0.3871718161991606344, -1.932801920045317257 ) ) ;
#213231 = CARTESIAN_POINT ( 'NONE',  ( 5.448516766998877436, 1.166291874360864345, 1.283151444216067638 ) ) ;
#213233 = CARTESIAN_POINT ( 'NONE',  ( 1.945129482973105839, -1.762486321751283835, -1.302348873264857820 ) ) ;
#213232 = CARTESIAN_POINT ( 'NONE',  ( 1.360316468749994012, -0.9843749996586090845, -5.204170427930421283E-15 ) ) ;
#213234 = CARTESIAN_POINT ( 'NONE',  ( 3.628207509315328760, -1.372338424813070556, -1.855037849730954091 ) ) ;
#213235 = CARTESIAN_POINT ( 'NONE',  ( 5.237599208242285087, -1.454345255708370255, -1.460303020606460445 ) ) ;
#213236 = CARTESIAN_POINT ( 'NONE',  ( 0.8318532965871343610, 1.913089267318631270, 0.3326846900589939815 ) ) ;
#213238 = EDGE_CURVE ( 'NONE', #123093, #207594, #72240, .T. ) ;
#213237 = CARTESIAN_POINT ( 'NONE',  ( -6.358410854684793279, 7.480862754296137673, -1.082531754730543083 ) ) ;
#213239 = PRODUCT_DEFINITION_SHAPE ( 'NONE', 'NONE',  #160678 ) ;
#213240 = CARTESIAN_POINT ( 'NONE',  ( -4.492547798081878874, 6.334668079219206049, 1.599625672291263179 ) ) ;
#213241 = CARTESIAN_POINT ( 'NONE',  ( -5.604008600195527379, 5.714843533513091600, -0.1954433161525123697 ) ) ;
#213242 = CARTESIAN_POINT ( 'NONE',  ( 4.517907016363444939, -0.5628432189327194912, 2.044499502628312371 ) ) ;
#213243 = CARTESIAN_POINT ( 'NONE',  ( 2.619767714365705658, 0.2496074646863334634, 2.000857082853441327 ) ) ;
#213244 = CARTESIAN_POINT ( 'NONE',  ( -5.924549939047510705, 6.974691686052601369, 1.082531754730549967 ) ) ;
#213245 = CARTESIAN_POINT ( 'NONE',  ( 4.753059971535213535, -1.774748228059085164, 1.311344899593884561 ) ) ;
#213247 =( BOUNDED_CURVE ( )  B_SPLINE_CURVE ( 2, ( #197173, #179874, #29359, #31499, #196127, #112805, #47765, #83415, #178818 ),
 .UNSPECIFIED., .F., .T. ) 
 B_SPLINE_CURVE_WITH_KNOTS ( ( 3, 2, 2, 2, 3 ),
 ( 0.5803571428571429047, 0.5833333333333333703, 0.5892857142857143016, 0.5952380952380952328, 0.5982142857142856984 ),
 .UNSPECIFIED. ) 
 CURVE ( )  GEOMETRIC_REPRESENTATION_ITEM ( )  RATIONAL_B_SPLINE_CURVE ( ( 0.9330127018922194093, 0.9330127018922206306, 1.000000000000000000, 0.8660254037844387076, 1.000000000000000000, 0.8660254037844387076, 1.000000000000000000, 0.9330127018922194093, 0.9330127018922194093 ) ) 
 REPRESENTATION_ITEM ( '' )  );
#213246 = CARTESIAN_POINT ( 'NONE',  ( -2.658506526196446007, -3.058169421092554963, 2.222368686088465939 ) ) ;
#213248 = CARTESIAN_POINT ( 'NONE',  ( 1.195384358724066508E-16, -4.140708350189171938, 1.000000000000004441 ) ) ;
#213249 = CARTESIAN_POINT ( 'NONE',  ( -7.370792787684826486, 8.628288336167626582, -1.199719254218452047 ) ) ;
#213252 = CIRCLE ( 'NONE', #178812, 0.07999999999999980738 ) ;
#213251 = CARTESIAN_POINT ( 'NONE',  ( -10.98598255107576627, -7.721050908199745599, 0.1917610387292554008 ) ) ;
#213250 = CARTESIAN_POINT ( 'NONE',  ( -4.912146588114373991, 8.123387011080156483, 1.048141424314027237 ) ) ;
#213253 = PRESENTATION_STYLE_ASSIGNMENT (( #147227 ) ) ;
#213254 = ORIENTED_EDGE ( 'NONE', *, *, #101161, .F. ) ;
#213255 = CARTESIAN_POINT ( 'NONE',  ( 4.662995224183227982, -1.840047010505897029, -0.9283316357228312832 ) ) ;
#213256 = CARTESIAN_POINT ( 'NONE',  ( 4.041065261760094174, 7.751399574583047070, -0.4490336992654907489 ) ) ;
#213257 = EDGE_CURVE ( 'NONE', #25034, #156131, #120711, .T. ) ;
#213258 = UNCERTAINTY_MEASURE_WITH_UNIT (LENGTH_MEASURE( 1.000000000000000082E-05 ), #16782, 'distance_accuracy_value', 'NONE');
#213259 = CARTESIAN_POINT ( 'NONE',  ( 0.1329588055935395918, 0.006246367379872773060, -1.846049620084759590 ) ) ;
#213260 = CARTESIAN_POINT ( 'NONE',  ( -5.576481253922474401, 5.400316305864651056, -0.7998128361456221525 ) ) ;
#213261 = CARTESIAN_POINT ( 'NONE',  ( 2.983074145627107931, -1.866958838928289399, -0.7709177042417614256 ) ) ;
#213262 = CARTESIAN_POINT ( 'NONE',  ( -1.500000000000015099, -0.6208333333333116988, -0.8660254037844383745 ) ) ;
#213263 = CARTESIAN_POINT ( 'NONE',  ( 10.22248463502393001, 11.02857961705718282, 0.7216878364870438212 ) ) ;
#213264 = CARTESIAN_POINT ( 'NONE',  ( 5.608269097547198712, 9.694731047113750222, -0.7998128361456281477 ) ) ;
#213265 = CARTESIAN_POINT ( 'NONE',  ( 2.676696200465655373, -1.971695749941338560, -0.5996849476793424394 ) ) ;
#213266 = CARTESIAN_POINT ( 'NONE',  ( -6.663994888585885512, -7.154544010627095219, 6.770610912236877610 ) ) ;
#213267 = CARTESIAN_POINT ( 'NONE',  ( 6.166260936116925606, 6.088392601758203071, 0.7998128361456341429 ) ) ;
#213268 = CARTESIAN_POINT ( 'NONE',  ( 1.657894046870052485, -1.302874822933766774, 1.301145727299134025 ) ) ;
#213269 = CARTESIAN_POINT ( 'NONE',  ( 0.4523713176287887383, 0.7179250195528188438, -2.193251166140824715 ) ) ;
#213270 = CARTESIAN_POINT ( 'NONE',  ( 5.363132282657546490, 8.414682208812571673, -1.199719254218452047 ) ) ;
#213271 = CARTESIAN_POINT ( 'NONE',  ( 2.847126979364768218, -1.798887516807456954, 1.198237791991546564 ) ) ;
#213272 = CARTESIAN_POINT ( 'NONE',  ( -3.470524135418306511, 5.072030796119872953, -1.443375672974053447 ) ) ;
#213273 = CARTESIAN_POINT ( 'NONE',  ( 1.358611653602972646, -1.916354379050893009, -0.6279873632355145174 ) ) ;
#213274 = CARTESIAN_POINT ( 'NONE',  ( 2.425563141628499064, 0.9819131520533967983, 2.078181775667542475 ) ) ;
#213275 = CIRCLE ( 'NONE', #137244, 0.08000000000000020983 ) ;
#213276 = CARTESIAN_POINT ( 'NONE',  ( 11.04536101718726293, 0.000000000000000000, -1.100000000000002087 ) ) ;
#213277 = CARTESIAN_POINT ( 'NONE',  ( 0.2857447052702493662, -0.8859512962964136706, 1.647562673099879138 ) ) ;
#213278 = EDGE_CURVE ( 'NONE', #90309, #186972, #4816, .T. ) ;
#213279 = CARTESIAN_POINT ( 'NONE',  ( 4.785985848584410896, -0.9303070431277806751, 1.738173387191404684 ) ) ;
#213280 =( GEOMETRIC_REPRESENTATION_CONTEXT ( 3 ) GLOBAL_UNCERTAINTY_ASSIGNED_CONTEXT ( ( #68019 ) ) GLOBAL_UNIT_ASSIGNED_CONTEXT ( ( #72500, #138600, #50942 ) ) REPRESENTATION_CONTEXT ( 'NONE', 'WORKASPACE' ) );
#213281 = CARTESIAN_POINT ( 'NONE',  ( 4.821500071095637274, -1.429446227384461032, -1.422610148874188463 ) ) ;
#213283 = CARTESIAN_POINT ( 'NONE',  ( 10.50720586046655391, 11.36075438007358507, 0.7216878364870438212 ) ) ;
#213282 = CARTESIAN_POINT ( 'NONE',  ( 1.364683531249988535, 3.905208333674751842, -0.7879004041258239610 ) ) ;
#213285 = CARTESIAN_POINT ( 'NONE',  ( 6.076811011874215573, -1.999271364452784638, -0.6623750905550094270 ) ) ;
#213284 = CARTESIAN_POINT ( 'NONE',  ( -7.250913225210214641, 7.353820272367037170, 0.7998128361456341429 ) ) ;
#213286 = CARTESIAN_POINT ( 'NONE',  ( 6.180147188013234150, -1.146869210499700920, -1.723488058659912392 ) ) ;
#213287 = CARTESIAN_POINT ( 'NONE',  ( 5.656776405399742025, 7.622658444431597680, -1.599625672291262513 ) ) ;
#213288 = CARTESIAN_POINT ( 'NONE',  ( -6.925517538482230506, 6.974191971184389160, 0.7998128361456341429 ) ) ;
#213289 = CARTESIAN_POINT ( 'NONE',  ( 6.539320575229247368, 1.272291865413360812, 2.120198356887960767 ) ) ;
#213290 = CARTESIAN_POINT ( 'NONE',  ( 6.451426753955883164, -1.802380967894920527, 0.9117540809469369956 ) ) ;
#213291 = CARTESIAN_POINT ( 'NONE',  ( -1.402160292154681736E-14, 0.8687500006828192678, -1.732050807568863648 ) ) ;
#213292 = CARTESIAN_POINT ( 'NONE',  ( 4.108297157686680912, -2.301651690510425841, 0.1678553853470560464 ) ) ;
#213293 = CARTESIAN_POINT ( 'NONE',  ( 1.868110439076278384, -2.047461887716729656, 0.2484499435305431159 ) ) ;
#213294 = CARTESIAN_POINT ( 'NONE',  ( 6.616015773788773480, 10.66250946948817813, -0.7216878364870267237 ) ) ;
#213295 = CARTESIAN_POINT ( 'NONE',  ( 5.345657705538078730, 9.458627433094950021, 0.7998128361456331437 ) ) ;
#213296 = CARTESIAN_POINT ( 'NONE',  ( 6.225128807330042591, 7.291680359087043151, -1.199719254218452047 ) ) ;
#213297 = CARTESIAN_POINT ( 'NONE',  ( -0.6823417656250003738, 0.7802083336747520637, -1.181850606188749264 ) ) ;
#213298 = CARTESIAN_POINT ( 'NONE',  ( 2.905190055078214595, 6.611415174225076186, 0.7998128361456271485 ) ) ;
#213299 = CARTESIAN_POINT ( 'NONE',  ( 7.578644679914718019, 7.944099669429731669, 0.7216878364870317197 ) ) ;
#213301 = DIRECTION ( 'NONE',  ( -0.000000000000000000, 1.000000000000000000, -0.000000000000000000 ) ) ;
#213300 = CARTESIAN_POINT ( 'NONE',  ( 4.316952289276101418, -1.611618797226920252, 1.455085969030824211 ) ) ;
#213302 = FACE_OUTER_BOUND ( 'NONE', #62210, .T. ) ;
#213304 = CARTESIAN_POINT ( 'NONE',  ( 3.403688466941825475, -0.7492148395099357261, -1.682118234477212537 ) ) ;
#213303 = CARTESIAN_POINT ( 'NONE',  ( -3.795919822146277767, 7.372397525905215687, -0.7216878364870267237 ) ) ;
#213305 = CARTESIAN_POINT ( 'NONE',  ( 0.6823417656249917140, 4.092708333674755394, 1.181850606188765695 ) ) ;
#213306 = CARTESIAN_POINT ( 'NONE',  ( 5.179302069984247581, 1.471482994053765925, 1.624232740060495228 ) ) ;
#213307 = CARTESIAN_POINT ( 'NONE',  ( 7.873621124554150974, 14.32272913405169668, 9.058612350049280337 ) ) ;
#213308 = CARTESIAN_POINT ( 'NONE',  ( 5.858358025671378755, 0.9108227554960802719, 2.071263147418811013 ) ) ;
#213309 = CARTESIAN_POINT ( 'NONE',  ( -5.747250929305832479, 6.247137566976777912, -1.064685594968674209 ) ) ;
#213310 = CARTESIAN_POINT ( 'NONE',  ( 4.598366155629488361, 8.485928551783258555, 0.1149073004905968448 ) ) ;
#213311 = CARTESIAN_POINT ( 'NONE',  ( -6.251718229232857915, 7.426664367927358512, -1.082531754730549967 ) ) ;
#213312 = CARTESIAN_POINT ( 'NONE',  ( 4.095971805104285934, 6.832365301713403838, 1.082531754730549078 ) ) ;
#213313 = CARTESIAN_POINT ( 'NONE',  ( 6.837169251635001999, -1.579311124772398767, 0.7986344709578310219 ) ) ;
#213314 = CIRCLE ( 'NONE', #36914, 0.08000000000000020983 ) ;
#213315 = CARTESIAN_POINT ( 'NONE',  ( 3.879544890376307453, 0.2443292893146010170, -1.998135132051428231 ) ) ;
#213316 = CARTESIAN_POINT ( 'NONE',  ( 6.825640269476072497, 10.05066518344239412, 1.199719254218460707 ) ) ;
#213317 = CARTESIAN_POINT ( 'NONE',  ( 3.469845758843297823, 2.055011051013386769, -0.4596899858253248872 ) ) ;
#213318 = CARTESIAN_POINT ( 'NONE',  ( 1.897908843228306663, -0.9047085692259320133, -1.688519222619834892 ) ) ;
#213319 = CARTESIAN_POINT ( 'NONE',  ( 3.147464216666835402, 6.823792019419957278, -0.7998128361456291469 ) ) ;
#213320 = CARTESIAN_POINT ( 'NONE',  ( 3.191813391966125124, -1.320872291013975630, -1.461159636213595459 ) ) ;
#213321 = CARTESIAN_POINT ( 'NONE',  ( 4.886975862609196142, -1.903224527948672584, -0.6766701927056159027 ) ) ;
#213322 = CARTESIAN_POINT ( 'NONE',  ( 0.4615142869485132637, 1.850934062480696252, -0.2700578556205368574 ) ) ;
#213323 = CARTESIAN_POINT ( 'NONE',  ( 0.8362905744919849615, -1.092891352686057527, 1.629061181365853539 ) ) ;
#213325 = ORIENTED_EDGE ( 'NONE', *, *, #74394, .T. ) ;
#213324 = CARTESIAN_POINT ( 'NONE',  ( 0.4922593472763935329, -1.060406550076501642, 1.591262010887870115 ) ) ;
#213326 = CARTESIAN_POINT ( 'NONE',  ( 4.528060117284229413, 7.266191989264828344, 1.082531754730558626 ) ) ;
#213327 = CARTESIAN_POINT ( 'NONE',  ( -1.364683531250000748, 0.07187500034142035865, 0.000000000000000000 ) ) ;
#213328 = FACE_OUTER_BOUND ( 'NONE', #134844, .T. ) ;
#213329 = CARTESIAN_POINT ( 'NONE',  ( -9.606148981167596190, -6.583980363595129504, 0.4355862708379978354 ) ) ;
#213330 = CARTESIAN_POINT ( 'NONE',  ( 1.082579992370054311, 1.234693400583252609, -1.661741702728709802 ) ) ;
#213331 = CARTESIAN_POINT ( 'NONE',  ( -1.402160292154681736E-14, 2.087500000000021227, -1.732050807568863648 ) ) ;
#213332 = CARTESIAN_POINT ( 'NONE',  ( 6.775324078527185989, 8.927630729746953264, -1.599625672291262513 ) ) ;
#213333 = CARTESIAN_POINT ( 'NONE',  ( -7.934546212495630968, 10.28005655271014795, -1.599625672291263179 ) ) ;
#213334 = CARTESIAN_POINT ( 'NONE',  ( 4.206772801990143584, 8.129928378955675328, 0.7998128361456271485 ) ) ;
#213335 = CARTESIAN_POINT ( 'NONE',  ( 5.268275487455277073, 2.118052368503114291, -0.1043780312826799589 ) ) ;
#213336 = CARTESIAN_POINT ( 'NONE',  ( 3.237364818613055473, 6.998952398349030268, -1.734723475976807094E-15 ) ) ;
#213337 = CARTESIAN_POINT ( 'NONE',  ( -1.364683531250012516, 0.7802083336747528408, 0.7879004041258379498 ) ) ;
#213338 = ORIENTED_EDGE ( 'NONE', *, *, #42375, .F. ) ;
#213339 = AXIS2_PLACEMENT_3D ( 'NONE', #11279, #93635, #14472 ) ;
#213340 = CARTESIAN_POINT ( 'NONE',  ( -0.7500000000000006661, 2.108333333333357817, -1.299038105676652011 ) ) ;
#213342 = CARTESIAN_POINT ( 'NONE',  ( 3.985207087413062066, 6.736826471035503694, -1.199719254218452047 ) ) ;
#213341 = CARTESIAN_POINT ( 'NONE',  ( 6.250445965835445428, -1.952298026214387194, -0.1936728439068043650 ) ) ;
#213343 = CARTESIAN_POINT ( 'NONE',  ( 4.393907559866160994, 0.09612058942952760032, 2.013924333851605297 ) ) ;
#213344 = CARTESIAN_POINT ( 'NONE',  ( 3.432743858578292784, -1.563009043653120322, 1.107381117132580250 ) ) ;
#213345 = CARTESIAN_POINT ( 'NONE',  ( 11.81907076198602802, 9.842687754035216230, -1.592066415281268243 ) ) ;
#213346 = CARTESIAN_POINT ( 'NONE',  ( 1.066276686178056377, -1.386418637449363889, 1.697306931840412370 ) ) ;
#213347 = CARTESIAN_POINT ( 'NONE',  ( 0.1333692844072559280, 6.947498546895843674, -2.648624074793118233 ) ) ;
#213348 = CARTESIAN_POINT ( 'NONE',  ( 2.934663490303309530, 0.2251962677765201870, 1.856852477824536329 ) ) ;
#213349 = CARTESIAN_POINT ( 'NONE',  ( -1.500000000000015099, -0.5479166659838513587, 0.8660254037844403729 ) ) ;
#213350 = CARTESIAN_POINT ( 'NONE',  ( -6.826694039680798021, 7.923230120171105284, -1.199719254218446718 ) ) ;
#213351 = B_SPLINE_CURVE_WITH_KNOTS ( 'NONE', 3,
 ( #186126, #52935, #151521, #73447, #135280, #106015, #87580, #20424, #55081, #4158 ),
 .UNSPECIFIED., .F., .F.,
 ( 4, 2, 2, 2, 4 ),
 ( 0.001822879634083278844, 0.002175306537177320101, 0.002527733440271360925, 0.002880160343365402182, 0.003232587246459443439 ),
 .UNSPECIFIED. ) ;
#213353 = CARTESIAN_POINT ( 'NONE',  ( 6.116841120987044356, 0.2079722402913257440, 2.107011275531808003 ) ) ;
#213352 = CARTESIAN_POINT ( 'NONE',  ( -4.785665035943912571, 4.685623418130398399, 1.214306433183764966E-14 ) ) ;
#213354 = CARTESIAN_POINT ( 'NONE',  ( -1.402160292154681736E-14, 8.734375000341403350, 1.575800808251682339 ) ) ;
#213356 = CARTESIAN_POINT ( 'NONE',  ( -6.312203035614172286, 9.521931420595302953, -1.199719254218452047 ) ) ;
#213355 = CARTESIAN_POINT ( 'NONE',  ( 2.015285228526709549, -2.027172053905087701, 0.5110949307850811696 ) ) ;
#213358 = ORIENTED_EDGE ( 'NONE', *, *, #130359, .F. ) ;
#213357 = CARTESIAN_POINT ( 'NONE',  ( 0.7973487315477224557, -0.6271472479968034364, 1.606907058918445985 ) ) ;
#213359 = CARTESIAN_POINT ( 'NONE',  ( 7.149227073107712549, 7.235186428247455837, -0.7998128361456281477 ) ) ;
#213360 = CARTESIAN_POINT ( 'NONE',  ( 1.419999999999822515, 7.388542872122566330, 4.154462424328221104 ) ) ;
#213361 = CARTESIAN_POINT ( 'NONE',  ( 0.06712503953320783645, -9.995102581657556939, 9.579544693637551234 ) ) ;
#213362 = CARTESIAN_POINT ( 'NONE',  ( -7.019253602638888090, -7.126685749119995528, -7.019253602638846345 ) ) ;
#213364 = CARTESIAN_POINT ( 'NONE',  ( 8.880227426826634129, 11.38335130276301754, 1.443375672974076540 ) ) ;
#213363 = CARTESIAN_POINT ( 'NONE',  ( 6.819914962873951936, 7.915321197229798322, -1.199719254218446718 ) ) ;
#213365 = CARTESIAN_POINT ( 'NONE',  ( -1.500000000000008216, 9.500000000000001776, 3.469446951953614189E-15 ) ) ;
#213367 = CARTESIAN_POINT ( 'NONE',  ( 2.174188805400371294, 0.7754062184415695391, 1.637274071133995035 ) ) ;
#213366 = CARTESIAN_POINT ( 'NONE',  ( 6.540882763950133238, 6.595727744222092959, 0.000000000000000000 ) ) ;
#213368 = CARTESIAN_POINT ( 'NONE',  ( -5.831978632172702071, 9.955725504176825780, 0.7998128361456481317 ) ) ;
#213369 = CARTESIAN_POINT ( 'NONE',  ( 5.190073875932979419, 4.949507698210251938, 0.7998128361456341429 ) ) ;
#213370 = CARTESIAN_POINT ( 'NONE',  ( 4.877901405866606588, 8.912911750144889567, 0.7998128361456341429 ) ) ;
#213371 = CARTESIAN_POINT ( 'NONE',  ( 6.539320575229257138, 2.987941927008979537, 2.250856951216452906 ) ) ;
#213372 = CARTESIAN_POINT ( 'NONE',  ( 4.017310073039977780, 7.571390042887482963, 0.3083681156060176232 ) ) ;
#213373 = CARTESIAN_POINT ( 'NONE',  ( 9.002250809793993724, 11.52571191622492464, -1.443375672974057666 ) ) ;
#213374 = EDGE_CURVE ( 'NONE', #189774, #44776, #137994, .T. ) ;
#213375 = CARTESIAN_POINT ( 'NONE',  ( 2.787383077106736273, -1.737616373609903286, 0.6669969758191662823 ) ) ;
#213376 = CARTESIAN_POINT ( 'NONE',  ( 0.4388990752801218975, -1.618778001572194647, -1.023919763412997286 ) ) ;
#213377 = CARTESIAN_POINT ( 'NONE',  ( 6.475613818078473471, 1.843275991838376981, -0.5597920731088936730 ) ) ;
#213378 = DIRECTION ( 'NONE',  ( -3.706092522800016599E-15, 0.000000000000000000, -1.000000000000000000 ) ) ;
#213379 = CARTESIAN_POINT ( 'NONE',  ( -1.853667714121317367, 8.957164077253494838, 0.7750000000000013545 ) ) ;
#213380 = CARTESIAN_POINT ( 'NONE',  ( 4.794097012578165007, 8.135614534340449566, -0.8214339667521903809 ) ) ;
#213381 =( LENGTH_UNIT ( ) NAMED_UNIT ( * ) SI_UNIT ( .MILLI., .METRE. ) );
#213382 = FACE_OUTER_BOUND ( 'NONE', #29872, .T. ) ;
#213383 = CARTESIAN_POINT ( 'NONE',  ( 9.747949258545622442, 10.47495501116581984, 0.000000000000000000 ) ) ;
#213384 = CARTESIAN_POINT ( 'NONE',  ( 4.733233314711627671, 0.004152288854553880422, -1.969629310717621040 ) ) ;
#213385 = CARTESIAN_POINT ( 'NONE',  ( 1.313308151137903224, 1.731519532738003297, -1.223779428986125462 ) ) ;
#213386 = CARTESIAN_POINT ( 'NONE',  ( -6.878064000834399394, 6.918829510595249310, -0.7998128361456291469 ) ) ;
#213387 = CARTESIAN_POINT ( 'NONE',  ( -4.161989969270909917, 5.878740935614592544, 1.443375672974064550 ) ) ;
#213388 = DIRECTION ( 'NONE',  ( 1.000000000000000000, 0.000000000000000000, 0.000000000000000000 ) ) ;
#213389 = CARTESIAN_POINT ( 'NONE',  ( 5.894512528888635750, 1.793468170635740710, -1.259063434910556500 ) ) ;
#213390 = DIRECTION ( 'NONE',  ( 0.000000000000000000, 1.000000000000000000, 0.000000000000000000 ) ) ;
#213391 = CARTESIAN_POINT ( 'NONE',  ( 4.260710244665906643, -1.428042822336324846, 1.293124370783913735 ) ) ;
#213392 = CARTESIAN_POINT ( 'NONE',  ( -7.393273838153706201, 7.519907654134449615, 0.7998128361456341429 ) ) ;
#213393 = CARTESIAN_POINT ( 'NONE',  ( -1.394453263437886604E-15, 2.375000000682794266, 1.224999999999975220 ) ) ;
#213394 = CARTESIAN_POINT ( 'NONE',  ( 1.207977004800918852, -0.5332226995428279714, 2.141375170867452660 ) ) ;
#213395 = CARTESIAN_POINT ( 'NONE',  ( -6.109845972839394790, 7.018363806889529322, 0.9744278291697535677 ) ) ;
#213396 = CARTESIAN_POINT ( 'NONE',  ( -0.4294425147611594107, -9.006862915010128035, 9.490288674561789151 ) ) ;
#213397 = ORIENTED_EDGE ( 'NONE', *, *, #92241, .T. ) ;
#213398 = CARTESIAN_POINT ( 'NONE',  ( 3.933273961740298752, 5.682181936820735579, 1.443375672974058777 ) ) ;
#213399 = VERTEX_POINT ( 'NONE', #106687 ) ;
#213400 = CARTESIAN_POINT ( 'NONE',  ( 6.491062224718945117, 0.1893930596480186412, 1.960278089617428554 ) ) ;
#213401 = CARTESIAN_POINT ( 'NONE',  ( 1.663517674946796143, 1.000093669912437644, 1.664638661912527962 ) ) ;
#213402 = CIRCLE ( 'NONE', #165028, 2.600000000000008082 ) ;
#213403 = CARTESIAN_POINT ( 'NONE',  ( 0.1575669172422279607, -0.4392406603518673736, -1.974865693180789750 ) ) ;
#213405 = CARTESIAN_POINT ( 'NONE',  ( 5.137489257405690957, 1.737274493258118113, -0.6675986409061424043 ) ) ;
#213404 = CARTESIAN_POINT ( 'NONE',  ( -5.769876891067536206, 8.889217585290882795, 1.199719254218454489 ) ) ;
#213406 = CARTESIAN_POINT ( 'NONE',  ( 4.850785098639300408, 8.881276058379668825, -0.7998128361456481317 ) ) ;
#213407 = CARTESIAN_POINT ( 'NONE',  ( 6.509000000000012776, 0.5843741663743782233, 2.053293374786519188 ) ) ;
#213408 = CARTESIAN_POINT ( 'NONE',  ( -5.096975683733680818, 8.033889833409558534, -1.199719254218452047 ) ) ;
#213409 = CARTESIAN_POINT ( 'NONE',  ( -6.400331034103001748, 9.624747418832267698, 1.199719254218452935 ) ) ;
#213410 = CARTESIAN_POINT ( 'NONE',  ( 0.9783777488623355278, -2.139296967303818686, -0.4750931833387496694 ) ) ;
#213411 = CARTESIAN_POINT ( 'NONE',  ( 4.039966587192250103, 7.657118751792200584, 0.7216878364870298324 ) ) ;
#213412 = CARTESIAN_POINT ( 'NONE',  ( -0.3670591950586384877, 13.37245467069800497, -1.330911102734550822 ) ) ;
#213413 = CARTESIAN_POINT ( 'NONE',  ( 1.469576158976824144E-15, 19.00000000000000000, 12.00000000000000178 ) ) ;
#213414 = CARTESIAN_POINT ( 'NONE',  ( 2.191784710619415044, -0.7813054520266484726, 1.650194661559079456 ) ) ;
#213415 = CARTESIAN_POINT ( 'NONE',  ( -0.4644214298920709694, 7.369507887686579828, 4.459343850248737695 ) ) ;
#213416 = CARTESIAN_POINT ( 'NONE',  ( 0.1216811705908979330, 2.536982183874235908, -1.996294991408742003 ) ) ;
#213417 = CARTESIAN_POINT ( 'NONE',  ( 6.609000000000064823, 1.245995683336246884, 2.213443714173808807 ) ) ;
#213418 = CARTESIAN_POINT ( 'NONE',  ( 10.56588178375152864, 11.22128359066528169, -0.7998128361456281477 ) ) ;
#213419 = CARTESIAN_POINT ( 'NONE',  ( 6.586557105272873969, -1.791547847876047594, -0.3505316570680468979 ) ) ;
#213420 = CARTESIAN_POINT ( 'NONE',  ( 3.977359813172594905, -0.1486911861427446802, 1.956209631609528099 ) ) ;
#213421 = CARTESIAN_POINT ( 'NONE',  ( -8.528242318195895066, 9.908369778438709474, 1.199719254218462483 ) ) ;
#213422 = CARTESIAN_POINT ( 'NONE',  ( 7.298366762858032430, 7.409182732956175244, 1.040834085586084257E-14 ) ) ;
#213423 = CARTESIAN_POINT ( 'NONE',  ( 4.405938146338868933, -0.9375679901368579872, -1.981035393479456008 ) ) ;
#213424 = PRESENTATION_LAYER_ASSIGNMENT (  '', '', ( #50797 ) ) ;
#213425 = CARTESIAN_POINT ( 'NONE',  ( 6.609000000000011532, 3.695567819995113634, 2.514302272609474809 ) ) ;
#213426 = CARTESIAN_POINT ( 'NONE',  ( 2.922783962489564846, -1.430918204188264875, 1.496350883549990352 ) ) ;
#213428 = CARTESIAN_POINT ( 'NONE',  ( 1.364683531249988757, 1.446875000341421469, 0.000000000000000000 ) ) ;
#213427 = CARTESIAN_POINT ( 'NONE',  ( 5.738512597764636958, 5.917411899002901876, -2.440166504834939243 ) ) ;
#213429 = ORIENTED_EDGE ( 'NONE', *, *, #76187, .T. ) ;
#213430 = CARTESIAN_POINT ( 'NONE',  ( 3.393488084526240733, -0.9333142364225041065, -2.100862151682027612 ) ) ;
#213431 = CARTESIAN_POINT ( 'NONE',  ( 6.941411460516762943, 11.04213777067082702, -0.7216878364870267237 ) ) ;
#213433 = CARTESIAN_POINT ( 'NONE',  ( 0.6124999999999914957, 1.333333333333339255, 1.060881119635932679 ) ) ;
#213432 = CARTESIAN_POINT ( 'NONE',  ( 6.549997609177859559, 6.814287763561861944, 0.000000000000000000 ) ) ;
#213434 = CARTESIAN_POINT ( 'NONE',  ( 6.720655732516688019, 6.039915720534646759, 2.321169117395345705 ) ) ;
#213435 = CARTESIAN_POINT ( 'NONE',  ( -9.604686356149271020, 4.518467169708413778, -7.193747284969076006 ) ) ;
#213436 = CARTESIAN_POINT ( 'NONE',  ( 4.347558855881414885, 1.941490382076584975, -0.04909019101095174475 ) ) ;
#213437 = VERTEX_POINT ( 'NONE', #37357 ) ;
#213438 = CARTESIAN_POINT ( 'NONE',  ( -0.01315889736799453862, -9.583523248313889908, 9.500441148486922671 ) ) ;
#213439 = CARTESIAN_POINT ( 'NONE',  ( 4.605663860560767375, 1.420894170025093439, 1.280184534114735095 ) ) ;
#213440 =( LENGTH_UNIT ( ) NAMED_UNIT ( * ) SI_UNIT ( .MILLI., .METRE. ) );
#213441 = CARTESIAN_POINT ( 'NONE',  ( 5.438411972298594854, 1.699845694858553857, 0.2911611187441583426 ) ) ;
#213442 = CARTESIAN_POINT ( 'NONE',  ( 4.645720405014278853, 1.993893748393640086, -0.3006458143828410479 ) ) ;
#213443 = CARTESIAN_POINT ( 'NONE',  ( 4.571052534358505781, -1.084669189052098082, 2.026668040654127090 ) ) ;
#213444 = CARTESIAN_POINT ( 'NONE',  ( -2.493739017041104677, 8.265916556960542394, 2.456386464945204740 ) ) ;
#213445 = CARTESIAN_POINT ( 'NONE',  ( 0.8915962724085277902, 1.944627461026976034, -1.043433064090833140 ) ) ;
#213447 = CARTESIAN_POINT ( 'NONE',  ( -4.448483799059637533, 7.243629294661272588, 1.082531754730549967 ) ) ;
#213446 = CARTESIAN_POINT ( 'NONE',  ( -9.992522908471816123, 11.61669713376064372, 1.199719254218462483 ) ) ;
#213448 = CARTESIAN_POINT ( 'NONE',  ( 6.397684210179588327, -0.5939413028648796722, 1.667199339893215448 ) ) ;
#213450 = CARTESIAN_POINT ( 'NONE',  ( 2.185838763446645849, -0.9780977115210144346, 2.073240998862643458 ) ) ;
#213449 = CARTESIAN_POINT ( 'NONE',  ( 4.864343252252968597, 8.897093904262280972, 0.000000000000000000 ) ) ;
#213451 = CARTESIAN_POINT ( 'NONE',  ( 1.376469814831126071, 1.609123190100629985, -0.6634216792447115152 ) ) ;
#213452 = CARTESIAN_POINT ( 'NONE',  ( 11.87828357749949681, 11.30310252740378729, -1.708055325888855114 ) ) ;
#213453 = CARTESIAN_POINT ( 'NONE',  ( 1.246934265006810927, -1.689945720101847293, -0.3868003843893202953 ) ) ;
#213454 = CARTESIAN_POINT ( 'NONE',  ( -1.360316468749996677, 0.4010416670080598767, -0.7853790794158941324 ) ) ;
#213455 = DIRECTION ( 'NONE',  ( 0.000000000000000000, 1.000000000000000000, 0.000000000000000000 ) ) ;
#213456 = CARTESIAN_POINT ( 'NONE',  ( 1.188188303608740615, -1.377055334905618933, -1.678633986682298573 ) ) ;
#213457 = CARTESIAN_POINT ( 'NONE',  ( 2.061732777098632230, 1.244387006429502396, 1.586668050434843158 ) ) ;
#213458 = CARTESIAN_POINT ( 'NONE',  ( 1.499999999999985123, -0.1729166659838496101, -0.8660254037844323793 ) ) ;
#213459 = CARTESIAN_POINT ( 'NONE',  ( 5.602155610709171896, -1.926676517935271171, 0.002254597750208849581 ) ) ;
#213460 = CARTESIAN_POINT ( 'NONE',  ( 1.364683531249997417, 12.48437500034139980, 2.602085213965210642E-15 ) ) ;
#213461 = CARTESIAN_POINT ( 'NONE',  ( 2.268119307372215676, 0.5874642799142595351, -2.142291314107084954 ) ) ;
#213462 = ORIENTED_EDGE ( 'NONE', *, *, #67235, .T. ) ;
#213463 = CARTESIAN_POINT ( 'NONE',  ( -9.579764304849156531, -9.999999999999994671, 0.06720017513374074158 ) ) ;
#213464 = CARTESIAN_POINT ( 'NONE',  ( -1.402160292154681736E-14, -0.5374999999999753308, 1.732050807568877637 ) ) ;
#213465 = CARTESIAN_POINT ( 'NONE',  ( 8.215351014876830504, 11.67199438640995801, -1.199719254218446718 ) ) ;
#213466 = CARTESIAN_POINT ( 'NONE',  ( 7.146556367734764770, 9.431011410480991231, 1.443375672974063439 ) ) ;
#213467 =( NAMED_UNIT ( * ) PLANE_ANGLE_UNIT ( ) SI_UNIT ( $, .RADIAN. ) );
#213468 = CARTESIAN_POINT ( 'NONE',  ( 5.302228144868663229, 1.312797389530523162, -1.142775443803839108 ) ) ;
#213469 = CARTESIAN_POINT ( 'NONE',  ( 3.859774877264535053, -0.5717695562157121270, 1.876676618968641019 ) ) ;
#213471 = CARTESIAN_POINT ( 'NONE',  ( -6.236387472606145010, 9.259240570473746601, -1.082531754730538864 ) ) ;
#213470 = CARTESIAN_POINT ( 'NONE',  ( 4.009460741339333723, 5.700790169694431420, -1.599625672291256295 ) ) ;
#213472 = CARTESIAN_POINT ( 'NONE',  ( -1.491588839496432062, 4.432142968562463814, -0.1769418395740521011 ) ) ;
#213473 = CARTESIAN_POINT ( 'NONE',  ( 4.798257751182677389, -2.261729152689537781, -0.06211711723675371333 ) ) ;
#213474 = CARTESIAN_POINT ( 'NONE',  ( 1.486864572717770283, 1.987365476997263292, 0.5519934122387574194 ) ) ;
#213475 = CARTESIAN_POINT ( 'NONE',  ( -7.531718027591449705, 8.745758106066849891, 1.199719254218462483 ) ) ;
#213476 = CARTESIAN_POINT ( 'NONE',  ( -3.104453987404963478, 5.605318171072321221, -1.082531754730549078 ) ) ;
#213477 = CARTESIAN_POINT ( 'NONE',  ( 2.852682258652036840, 0.7612096163719231923, 2.130753183350143409 ) ) ;
#213478 = EDGE_LOOP ( 'NONE', ( #132318, #162335, #186467, #203046 ) ) ;
#213479 = CARTESIAN_POINT ( 'NONE',  ( -1.201851678989727383E-14, 0.9937500006828198229, 1.732050807568877637 ) ) ;
#213480 = CARTESIAN_POINT ( 'NONE',  ( 2.917106759524803472, -0.1871779394605546654, 1.861177454839262113 ) ) ;
#213481 = CARTESIAN_POINT ( 'NONE',  ( 1.300929835083320274, 1.165380355416269609, -1.284392162598305021 ) ) ;
#213482 = CARTESIAN_POINT ( 'NONE',  ( 5.706613541269077494, 1.932210019790636224, 1.034112652976440394 ) ) ;
#213483 = CARTESIAN_POINT ( 'NONE',  ( 0.3763673390903346516, 1.272619870141003418, 1.802674353332263335 ) ) ;
#213484 = CARTESIAN_POINT ( 'NONE',  ( 3.766626874709140704, -1.453462046928340579, 1.600284095077113333 ) ) ;
#213485 = CARTESIAN_POINT ( 'NONE',  ( 4.154194137148957466, -1.438218894771810641, 1.305048227774636915 ) ) ;
#213486 = AXIS2_PLACEMENT_3D ( 'NONE', #192934, #194004, #211317 ) ;
#213487 = CARTESIAN_POINT ( 'NONE',  ( -4.243338890952916387, 4.052909582307567149, -0.7216878364870207285 ) ) ;
#213489 = EDGE_LOOP ( 'NONE', ( #182385, #33330, #182640, #129476, #162042 ) ) ;
#213488 = CARTESIAN_POINT ( 'NONE',  ( 6.749288224047838902, -1.502610544577225760, -1.113804566994440970 ) ) ;
#213490 = CARTESIAN_POINT ( 'NONE',  ( 0.4687500000003047007, 0.7852924748224731077, -1.895863743164100335 ) ) ;
#213491 = CARTESIAN_POINT ( 'NONE',  ( 4.025675347721991315, 7.559696154190033823, -0.3592088497781486534 ) ) ;
#213492 = DIRECTION ( 'NONE',  ( 0.000000000000000000, 0.000000000000000000, 1.000000000000000000 ) ) ;
#213493 = CARTESIAN_POINT ( 'NONE',  ( 1.360316468750001784, 2.286458333674732835, -0.7853790794158941324 ) ) ;
#213494 = CARTESIAN_POINT ( 'NONE',  ( 5.397111353752316987, -0.9091427841607623295, -1.799923777076550824 ) ) ;
#213495 = CARTESIAN_POINT ( 'NONE',  ( -8.696665468161981494, 12.23352791524263239, -1.199719254218446718 ) ) ;
#213496 = CARTESIAN_POINT ( 'NONE',  ( 8.471147050440139381, 8.777426401801974976, -0.7998128361456281477 ) ) ;
#213497 = CARTESIAN_POINT ( 'NONE',  ( 4.041212305325117882, 6.872442235258051646, -1.199719254218448494 ) ) ;
#213498 = CARTESIAN_POINT ( 'NONE',  ( 3.053144290054691901, -1.492835736363471888, -1.050712463094093385 ) ) ;
#213499 = CARTESIAN_POINT ( 'NONE',  ( 2.609770642201841184, -0.3830433331901555993, 0.000000000000000000 ) ) ;
#213500 = ORIENTED_EDGE ( 'NONE', *, *, #110293, .F. ) ;
#213501 = CARTESIAN_POINT ( 'NONE',  ( -3.973948422136968084, 7.650373902552835226, -0.7216878364870458196 ) ) ;
#213502 = EDGE_CURVE ( 'NONE', #8666, #105457, #44613, .T. ) ;
#213503 = UNCERTAINTY_MEASURE_WITH_UNIT (LENGTH_MEASURE( 1.000000000000000082E-05 ), #89871, 'distance_accuracy_value', 'NONE');
#213504 = CARTESIAN_POINT ( 'NONE',  ( -3.285556943750000070, -3.696874999522044458, 0.000000000000000000 ) ) ;
#213505 = CARTESIAN_POINT ( 'NONE',  ( -7.147119532698295252, 11.49005655479003174, 0.000000000000000000 ) ) ;
#213506 = CARTESIAN_POINT ( 'NONE',  ( 6.252604593904901975, 1.998004417694958512, 0.2941112629052196614 ) ) ;
#213507 = CARTESIAN_POINT ( 'NONE',  ( 1.084817099560590803, -1.342388549496125627, 1.641497191572589776 ) ) ;
#213508 = EDGE_LOOP ( 'NONE', ( #31746, #128146, #181104, #49970 ) ) ;
#213509 = CARTESIAN_POINT ( 'NONE',  ( -6.445975688654487001, 6.485002823043819475, -0.7998128361456362523 ) ) ;
#213510 = CARTESIAN_POINT ( 'NONE',  ( 4.813308228051395687, 5.574280006603454574, 1.199719254218462483 ) ) ;
#213511 = CARTESIAN_POINT ( 'NONE',  ( 6.245006310359877411, -1.742422335079217843, 1.100243706638550423 ) ) ;
#213512 = CARTESIAN_POINT ( 'NONE',  ( 5.590470263882489910, -0.4872053753022275724, 1.956560708789633285 ) ) ;
#213513 = VERTEX_POINT ( 'NONE', #23219 ) ;
#213514 = CARTESIAN_POINT ( 'NONE',  ( -8.448702279610222021, 13.00856975952063088, 1.040834085586084257E-14 ) ) ;
#213515 = CARTESIAN_POINT ( 'NONE',  ( 7.320879633048903241E-15, 0.3750000006828252408, 1.224999999999981659 ) ) ;
#213517 = CARTESIAN_POINT ( 'NONE',  ( -0.1290005225502675879, -0.006633637972621592160, -2.173875058097324064 ) ) ;
#213516 = CARTESIAN_POINT ( 'NONE',  ( -4.782994330570982555, 8.802186828966616972, 0.000000000000000000 ) ) ;
#213518 = CARTESIAN_POINT ( 'NONE',  ( 6.578229047358968629, 6.784305542873760864, 0.2988042929856441488 ) ) ;
#213519 = CARTESIAN_POINT ( 'NONE',  ( 4.798203786142633653, -1.844427309015805649, 0.8145022673629878085 ) ) ;
#213520 = CARTESIAN_POINT ( 'NONE',  ( 4.646344025792163990, -1.477054284018078256, 1.098930429567553047 ) ) ;
#213521 = CARTESIAN_POINT ( 'NONE',  ( -0.02319159430949970999, 4.096340798889516854, -2.366022381217198767 ) ) ;
#213522 = CARTESIAN_POINT ( 'NONE',  ( 2.737322364211117520, 0.2836107604972230578, 2.290143083710040717 ) ) ;
#213523 = CARTESIAN_POINT ( 'NONE',  ( 5.006703865196457492, 9.063181286029688977, 0.000000000000000000 ) ) ;
#213524 = CARTESIAN_POINT ( 'NONE',  ( 6.081358973892867503, 1.999796440023202448, -0.8210498935554910727 ) ) ;
#213525 = CARTESIAN_POINT ( 'NONE',  ( 6.259060471003163428, 10.45398764947904624, -0.7998128361456291469 ) ) ;
#213526 = CARTESIAN_POINT ( 'NONE',  ( 0.8021671156859496721, 1.469769370800941166, -1.269469122775281456 ) ) ;
#213527 = CARTESIAN_POINT ( 'NONE',  ( -3.327636637150278798, 5.969660945728899826, -1.199719254218452935 ) ) ;
#213528 = VERTEX_POINT ( 'NONE', #172712 ) ;
#213529 = CARTESIAN_POINT ( 'NONE',  ( 4.288600692895239597, -2.201063653074202708, 0.6618141117178658606 ) ) ;
#213530 = CARTESIAN_POINT ( 'NONE',  ( -1.201851678989727383E-14, 2.946875000341418804, -1.575800808251660134 ) ) ;
#213531 = CARTESIAN_POINT ( 'NONE',  ( -3.494969737272722643, 7.299491470118629088, -0.7998128361456481317 ) ) ;
#213532 = CARTESIAN_POINT ( 'NONE',  ( 3.942156681999692491, 1.861596489644477437, 0.1839347620080991341 ) ) ;
#213533 = EDGE_CURVE ( 'NONE', #199393, #13599, #85838, .T. ) ;
#213536 = CARTESIAN_POINT ( 'NONE',  ( -6.017840079619296567, 8.114175741012878973, -1.599625672291271394 ) ) ;
#213535 = CARTESIAN_POINT ( 'NONE',  ( -1.500000000000001332, 0.4312500006828159926, 0.000000000000000000 ) ) ;
#213534 = CARTESIAN_POINT ( 'NONE',  ( 1.634869402278725348, 1.785593253932623803, 0.6852637533772619749 ) ) ;
#213537 = CARTESIAN_POINT ( 'NONE',  ( 3.123846942790895476, -2.126788776302591888, 0.5888931905130634359 ) ) ;
#213538 = CARTESIAN_POINT ( 'NONE',  ( 6.983263157960401202, 2.460233018525457727, 2.229759568558951965 ) ) ;
#213539 = CARTESIAN_POINT ( 'NONE',  ( 5.151735183068521629, 5.112705256442466428, 1.040834085586084257E-14 ) ) ;
#213540 = CARTESIAN_POINT ( 'NONE',  ( 6.495764994278797388, 8.671754808115688107, 1.443375672974063439 ) ) ;
#213541 = CARTESIAN_POINT ( 'NONE',  ( -3.867100128395853709, 5.534702787927018974, -1.599625672291256295 ) ) ;
#213542 = CARTESIAN_POINT ( 'NONE',  ( -7.404161286394468355, 7.810812053647902431, 0.000000000000000000 ) ) ;
#213543 = CARTESIAN_POINT ( 'NONE',  ( 0.5792891803052163668, 1.841034274367932877, -0.7053527730483382108 ) ) ;
#213544 = CARTESIAN_POINT ( 'NONE',  ( 1.097181765414790400, -0.5634973350938665693, -2.237626367659339088 ) ) ;
#213545 = CARTESIAN_POINT ( 'NONE',  ( 1.240593047436115759, -1.913272810121857237, -0.4332019784048374289 ) ) ;
#213546 = CARTESIAN_POINT ( 'NONE',  ( 5.366109125895877519, -2.053123361074739250, 0.1969011160823062045 ) ) ;
#213547 = CARTESIAN_POINT ( 'NONE',  ( 3.850152436600926542, 7.435668909435648288, -0.7216878364870197293 ) ) ;
#213548 = CARTESIAN_POINT ( 'NONE',  ( 4.692003678781083487, 7.631698837623355658, -1.199719254218450271 ) ) ;
#213549 = ORIENTED_EDGE ( 'NONE', *, *, #98948, .F. ) ;
#213550 = CARTESIAN_POINT ( 'NONE',  ( -1.364683531249997417, 5.321875000341417916, 1.214306433183764966E-14 ) ) ;
#213551 = CARTESIAN_POINT ( 'NONE',  ( 10.89523958697327011, -6.437359833193944780, -0.04208621775141048460 ) ) ;
#213552 = CARTESIAN_POINT ( 'NONE',  ( 3.592547517496925913, 5.214391408544949869, -1.443375672974058777 ) ) ;
#213554 = AXIS2_PLACEMENT_3D ( 'NONE', #23812, #89916, #193779 ) ;
#213553 = CARTESIAN_POINT ( 'NONE',  ( 1.094852686531849084, 2.138608527004157711, 0.3732488551555103173 ) ) ;
#213556 = CARTESIAN_POINT ( 'NONE',  ( 6.603072989126265391, -0.3962418105841297722, 1.804722624154910360 ) ) ;
#213555 = DIRECTION ( 'NONE',  ( 1.224646799147343346E-16, 0.000000000000000000, -1.000000000000000000 ) ) ;
#213557 = CARTESIAN_POINT ( 'NONE',  ( 11.52901446936750141, 11.29425527467587465, -3.330874149801114292 ) ) ;
#213558 = DIRECTION ( 'NONE',  ( 0.04529798058948680123, 1.504112749676217512E-16, 0.9989735196462991018 ) ) ;
#213559 = CARTESIAN_POINT ( 'NONE',  ( 0.8603690976232807319, -1.359099942111790416, 1.285485254608226269 ) ) ;
#213560 = CARTESIAN_POINT ( 'NONE',  ( 5.712251288600169730, -0.9662322189689104279, -1.933677227328117532 ) ) ;
#213561 = CARTESIAN_POINT ( 'NONE',  ( -6.103605818514504122, 6.017332118737867219, 0.3415998263276952551 ) ) ;
#213562 = CARTESIAN_POINT ( 'NONE',  ( 0.07735805125225460321, 4.085280796943619563, -2.643583850410589964 ) ) ;
#213563 = CARTESIAN_POINT ( 'NONE',  ( -0.6823417656250246877, -1.198958332991911790, 1.181850606188755259 ) ) ;
#213564 = CARTESIAN_POINT ( 'NONE',  ( 2.473184984502617478, -1.664690511387197702, -0.9409074295685518896 ) ) ;
#213565 = CARTESIAN_POINT ( 'NONE',  ( 3.168565732603556562, -1.634766719728536266, -0.6786406015907071598 ) ) ;
#213566 = CARTESIAN_POINT ( 'NONE',  ( 0.5570965697654255422, -1.639946202723217450, 0.9833419947904218361 ) ) ;
#213568 = CARTESIAN_POINT ( 'NONE',  ( 5.730082575778132181, 1.913663781862886104, 0.08886097549761286241 ) ) ;
#213567 = CARTESIAN_POINT ( 'NONE',  ( 3.124804640640014064, -3.181435245600519046, -1.183652705699159924 ) ) ;
#213569 = CARTESIAN_POINT ( 'NONE',  ( 1.499999999999987566, -0.9749999999999827693, 0.000000000000000000 ) ) ;
#213570 = CARTESIAN_POINT ( 'NONE',  ( 6.303175665915636827, -1.664687476133955846, 1.052260723566181833 ) ) ;
#213571 = CARTESIAN_POINT ( 'NONE',  ( -1.499999999999997780, 4.900000000000022560, 1.214306433183764966E-14 ) ) ;
#213572 = CARTESIAN_POINT ( 'NONE',  ( 0.8090202166558431163, -0.5209130535433897924, -2.055487714681260236 ) ) ;
#213573 = CARTESIAN_POINT ( 'NONE',  ( 0.06290936665214190426, -8.043994141378489005, -10.94971099608171627 ) ) ;
#213574 = CARTESIAN_POINT ( 'NONE',  ( 4.522238337509359773, 1.150754656758418593, -1.474723989322044959 ) ) ;
#213576 = ORIENTED_EDGE ( 'NONE', *, *, #61445, .F. ) ;
#213575 = CARTESIAN_POINT ( 'NONE',  ( 0.9260630535584664091, 1.089557764695957554, -1.464779044915397455 ) ) ;
#213578 = CARTESIAN_POINT ( 'NONE',  ( 10.38614328979769041, 3.507114751586604129, 5.996442624206595795 ) ) ;
#213577 = CARTESIAN_POINT ( 'NONE',  ( 5.057340365224886725, -1.863002784048470639, -1.182737378625432489 ) ) ;
#213579 = CARTESIAN_POINT ( 'NONE',  ( -1.364683531250012516, 4.551041667008082214, -0.7879004041258300672 ) ) ;
#213580 = CARTESIAN_POINT ( 'NONE',  ( 1.785667050844968351, -1.942997710132963407, 0.6927838567832644845 ) ) ;
#213581 = CARTESIAN_POINT ( 'NONE',  ( 7.122110765880372618, 7.203550736482235095, 0.7998128361456341429 ) ) ;
#213582 = CARTESIAN_POINT ( 'NONE',  ( -6.503107236049161521, 10.73870887536603291, 0.7998128361456481317 ) ) ;
#213583 = CARTESIAN_POINT ( 'NONE',  ( -3.424799127523457276, -0.02060169327834648900, -0.4188067397860005814 ) ) ;
#213584 = LINE ( 'NONE', #82537, #158608 ) ;
#213585 = ORIENTED_EDGE ( 'NONE', *, *, #205767, .F. ) ;
#213586 = CARTESIAN_POINT ( 'NONE',  ( 4.492674960910642667, 2.029786422369950216, 0.4070406814440513665 ) ) ;
#213587 = CARTESIAN_POINT ( 'NONE',  ( -1.364683531250000748, -1.178124999658580752, 0.000000000000000000 ) ) ;
#213588 = CARTESIAN_POINT ( 'NONE',  ( 1.599129061979026822, 1.768144091905754500, -1.243190488262067683 ) ) ;
#213589 = CARTESIAN_POINT ( 'NONE',  ( -5.250728612101474901, 7.694385777474874288, -1.211319784145984846 ) ) ;
#213590 = CARTESIAN_POINT ( 'NONE',  ( 1.928384432292037598, -0.9539229595667864103, -1.780212580967098335 ) ) ;
#213591 = CARTESIAN_POINT ( 'NONE',  ( 4.561484710689858169, 7.006108427806116978, -1.224552438206182980 ) ) ;
#213592 = VERTEX_POINT ( 'NONE', #205172 ) ;
#213594 = CARTESIAN_POINT ( 'NONE',  ( 7.944714827928050838, 9.331550723079971021, 1.082531754730558626 ) ) ;
#213593 = CARTESIAN_POINT ( 'NONE',  ( 1.737500000000001155, -3.033333333333332327, 3.009438278150922130 ) ) ;
#213595 = CARTESIAN_POINT ( 'NONE',  ( 0.02465203476893947088, 14.53755993404379510, 11.97749487451461903 ) ) ;
#213596 = CARTESIAN_POINT ( 'NONE',  ( 0.2687680251878405424, -0.2516378192510167477, -2.000730910237565663 ) ) ;
#213597 = CARTESIAN_POINT ( 'NONE',  ( 5.038714576072483631, -1.879839391954684746, 1.126354835186346603 ) ) ;
#213598 = CARTESIAN_POINT ( 'NONE',  ( -1.500000000000011324, 5.160416667349487341, -0.8660254037844313801 ) ) ;
#213599 = CARTESIAN_POINT ( 'NONE',  ( 3.761887187967042134, 0.6396200178584460216, -1.802413552503052463 ) ) ;
#213600 = CARTESIAN_POINT ( 'NONE',  ( -3.228813138348844536, 6.918699094715619502, 0.7998128361456341429 ) ) ;
#213601 = CARTESIAN_POINT ( 'NONE',  ( 5.463572716182819811, 8.357623354646536384, 1.082531754730558626 ) ) ;
#213603 = CARTESIAN_POINT ( 'NONE',  ( 1.933220473845993492, -1.621196910160098925, -1.198842755339262212 ) ) ;
#213602 = CARTESIAN_POINT ( 'NONE',  ( -10.43941509239824228, 11.28166515066052966, 1.040834085586084257E-14 ) ) ;
#213604 = CARTESIAN_POINT ( 'NONE',  ( -1.364683531250000748, 12.92187500034139980, 0.000000000000000000 ) ) ;
#213606 = CARTESIAN_POINT ( 'NONE',  ( -6.064239847062411926, 10.29697326487330500, 0.000000000000000000 ) ) ;
#213605 = CARTESIAN_POINT ( 'NONE',  ( 0.9082674546003096649, -1.036902680258915854, -2.044550831922228085 ) ) ;
#213607 = CARTESIAN_POINT ( 'NONE',  ( 4.559404828610894356, 0.3762245950137115269, -1.683048502377647804 ) ) ;
#213608 = CARTESIAN_POINT ( 'NONE',  ( 7.472478939787284169, 8.746922180287201698, 1.199719254218452935 ) ) ;
#213609 = CARTESIAN_POINT ( 'NONE',  ( 3.714044015139744914, 6.420469553383295391, 1.199719254218462483 ) ) ;
#213610 = CARTESIAN_POINT ( 'NONE',  ( -0.7499999999999972244, 3.889583334016149863, -1.299038105676652011 ) ) ;
#213611 = CARTESIAN_POINT ( 'NONE',  ( 0.07516593201273635838, 6.947014887512039216, -2.639261810199782232 ) ) ;
#213612 = ORIENTED_EDGE ( 'NONE', *, *, #187293, .T. ) ;
#213613 = CIRCLE ( 'NONE', #147940, 4.021913119055696484 ) ;
#213614 = ORIENTED_EDGE ( 'NONE', *, *, #150248, .F. ) ;
#213615 = CARTESIAN_POINT ( 'NONE',  ( 5.443967095383744237, -1.154075521934978532, -1.396247737120015930 ) ) ;
#213616 = ORIENTED_EDGE ( 'NONE', *, *, #77330, .F. ) ;
#213617 = CARTESIAN_POINT ( 'NONE',  ( 6.052789233858158369, 6.026285292448116948, 0.000000000000000000 ) ) ;
#213618 = DIRECTION ( 'NONE',  ( 0.000000000000000000, 1.000000000000000000, 0.000000000000000000 ) ) ;
#213619 = CARTESIAN_POINT ( 'NONE',  ( 5.777939495331589015, 1.783485896618082878, -0.3162516061415173718 ) ) ;
#213620 = CARTESIAN_POINT ( 'NONE',  ( 4.855228407025239612, 8.678533884922511987, 0.000000000000000000 ) ) ;
#213621 = CARTESIAN_POINT ( 'NONE',  ( -11.86239285000045918, 9.799999999999997158, -1.812080536912752837 ) ) ;
#213622 = CARTESIAN_POINT ( 'NONE',  ( 2.853686581259745836, 2.180823047698337902, -0.2155538573413370296 ) ) ;
#213623 = EDGE_LOOP ( 'NONE', ( #180610, #156940, #196868, #189125 ) ) ;
#213624 = CIRCLE ( 'NONE', #106405, 12.00000000000000178 ) ;
#213625 = EDGE_CURVE ( 'NONE', #213592, #42393, #193328, .T. ) ;
#213627 = CARTESIAN_POINT ( 'NONE',  ( 7.892817981449907982, 12.36003807833360391, 0.7998128361456462443 ) ) ;
#213626 = CARTESIAN_POINT ( 'NONE',  ( 6.373497979817693171, -0.2265250974912805249, 1.847160380126455559 ) ) ;
#213628 = CARTESIAN_POINT ( 'NONE',  ( 3.427252967507479209, -1.452606091845513037, -1.248918174067833009 ) ) ;
#213629 = CARTESIAN_POINT ( 'NONE',  ( -3.245517230425579371E-14, 3.975067388631681187, 1.872309607372774520 ) ) ;
#213630 = PRESENTATION_STYLE_ASSIGNMENT (( #194210 ) ) ;
#213631 = CARTESIAN_POINT ( 'NONE',  ( 1.364683531249988757, -0.6156249996585803075, 0.000000000000000000 ) ) ;
#213632 = CARTESIAN_POINT ( 'NONE',  ( 5.585596099150174965, 7.539614753807099667, -1.443375672974057666 ) ) ;
#213634 = CARTESIAN_POINT ( 'NONE',  ( 5.893796404173470727, -2.101076160772547219, 0.2616963346634570975 ) ) ;
#213633 = CARTESIAN_POINT ( 'NONE',  ( -8.324343129110692630, 12.65555805069709550, 0.7216878364870338292 ) ) ;
#213635 = CARTESIAN_POINT ( 'NONE',  ( 1.112450467520700537, -0.9725818059473788635, -1.930612204972524060 ) ) ;
#213636 = CARTESIAN_POINT ( 'NONE',  ( -5.984998465789844069, 5.947196063035064206, 0.7998128361456281477 ) ) ;
#213637 = EDGE_CURVE ( 'NONE', #41470, #53161, #127709, .T. ) ;
#213638 = CARTESIAN_POINT ( 'NONE',  ( 4.390861645979372341, 6.216034235099629157, -1.599625672291269396 ) ) ;
#213639 = CARTESIAN_POINT ( 'NONE',  ( 1.289775909805501719, -0.8246113042270180049, 1.628811597173693393 ) ) ;
#213640 = CARTESIAN_POINT ( 'NONE',  ( -3.765413976293358278, 5.416068943807445635, 1.599625672291267398 ) ) ;
#213641 = CARTESIAN_POINT ( 'NONE',  ( 3.135583521505393545, -1.224952879796761041, -1.353777129306121818 ) ) ;
#213642 = CARTESIAN_POINT ( 'NONE',  ( 9.318301066091441598, 12.86598888409864472, -8.945124285776126172 ) ) ;
#213643 = VERTEX_POINT ( 'NONE', #188942 ) ;
#213644 = CARTESIAN_POINT ( 'NONE',  ( 2.822656803168353434, -1.360269829074612469, 1.424587346448534353 ) ) ;
#213645 = ORIENTED_EDGE ( 'NONE', *, *, #167257, .F. ) ;
#213646 = CARTESIAN_POINT ( 'NONE',  ( 5.073749223668181152, -1.075672608635285687, 1.616763269924810231 ) ) ;
#213647 = CARTESIAN_POINT ( 'NONE',  ( -4.679499295372141709, 5.488445928469455559, 1.199719254218452935 ) ) ;
#213649 = CARTESIAN_POINT ( 'NONE',  ( 5.291314375706784645, -0.05428322906628547939, -2.120082430678168706 ) ) ;
#213648 = CARTESIAN_POINT ( 'NONE',  ( 5.481239241674765950, 9.616805891921051952, -0.7998128361456481317 ) ) ;
#213650 = CARTESIAN_POINT ( 'NONE',  ( 0.001121896803084446431, -7.189645481337945121, 9.584290747382876674 ) ) ;
#213651 = CARTESIAN_POINT ( 'NONE',  ( 2.877492880751183257, 0.2784179829431778219, -1.891769048003589138 ) ) ;
#213652 = CARTESIAN_POINT ( 'NONE',  ( 5.816641468517390834, 6.206546802344954372, -0.9418049055998338748 ) ) ;
#213653 = CARTESIAN_POINT ( 'NONE',  ( -1.284279953904135407, 3.128360285806111474, -0.7749999999999892530 ) ) ;
#213654 = CARTESIAN_POINT ( 'NONE',  ( 4.472210567661338843, 6.310941310395290493, 1.599625672291261402 ) ) ;
#213655 = CARTESIAN_POINT ( 'NONE',  ( 4.354156267015011572, 0.8588168762691525959, -1.820826276449886150 ) ) ;
#213657 =( BOUNDED_SURFACE ( )  B_SPLINE_SURFACE ( 3, 2, ( 
 ( #204762, #138744, #56414 ),
 ( #40167, #106281, #172302 ),
 ( #23891, #89997, #73722 ),
 ( #205848, #175506, #57481 ),
 ( #41249, #107357, #173379 ),
 ( #24963, #91065, #74799 ),
 ( #124696, #153919, #108431 ),
 ( #174451, #26027, #92137 ),
 ( #141963, #207975, #59602 ),
 ( #125760, #5489, #137678 ),
 ( #10835, #46572, #80113 ),
 ( #61742, #160308, #95339 ),
 ( #110561, #146218, #44443 ),
 ( #211169, #45510, #159234 ) ),
 .UNSPECIFIED., .F., .F., .T. ) 
 B_SPLINE_SURFACE_WITH_KNOTS ( ( 4, 2, 2, 2, 2, 2, 4 ),
 ( 3, 3 ),
 ( 0.01742726680619078455, 0.02012515843099235008, 0.02147410424339313284, 0.02282305005579391213, 0.02417199586819469143, 0.02552094168059547419, 0.02821883330539703971 ),
 ( 0.000000000000000000, 1.000000000000000000 ),
 .UNSPECIFIED. ) 
 GEOMETRIC_REPRESENTATION_ITEM ( )  RATIONAL_B_SPLINE_SURFACE ( (
 ( 1.000000000000000000, 0.8509629433930230302, 1.000000000000000000),
 ( 1.000000000000000000, 0.8507187689822764964, 1.000000000000000000),
 ( 1.000000000000000000, 0.8494327192471640142, 1.000000000000000000),
 ( 1.000000000000000000, 0.8495462935814993566, 1.000000000000000000),
 ( 1.000000000000000000, 0.8498623255111610320, 1.000000000000000000),
 ( 1.000000000000000000, 0.8506092561374887229, 1.000000000000000000),
 ( 1.000000000000000000, 0.8510280321988274999, 1.000000000000000000),
 ( 1.000000000000000000, 0.8508805742456044818, 1.000000000000000000),
 ( 1.000000000000000000, 0.8503832817317976689, 1.000000000000000000),
 ( 1.000000000000000000, 0.8496212719666990099, 1.000000000000000000),
 ( 1.000000000000000000, 0.8493586043581990985, 1.000000000000000000),
 ( 1.000000000000000000, 0.8494730729331905206, 1.000000000000000000),
 ( 1.000000000000000000, 0.8509586478585877689, 1.000000000000000000),
 ( 1.000000000000000000, 0.8509656014577856586, 1.000000000000000000) ) ) 
 REPRESENTATION_ITEM ( '' )  SURFACE ( )  );
#213656 = CARTESIAN_POINT ( 'NONE',  ( -3.975497760493641675, 7.849573349659754840, -7.471960471057975262E-11 ) ) ;
#213658 = CARTESIAN_POINT ( 'NONE',  ( 4.898959864523320107, 1.516061528642864253, -1.016892643307308441 ) ) ;
#213659 = CARTESIAN_POINT ( 'NONE',  ( 0.7310241076574041097, -1.948878508384953356, -0.6990896207654460071 ) ) ;
#213660 = CARTESIAN_POINT ( 'NONE',  ( -8.514157279702027736, 10.95626946445095307, -1.443375672974059665 ) ) ;
#213661 = CARTESIAN_POINT ( 'NONE',  ( -5.922807744518227224, 7.239652023730190677, 1.252291340712426981 ) ) ;
#213662 = CARTESIAN_POINT ( 'NONE',  ( 2.672702088255949078E-15, 1.625000000682787160, 1.224999999999980549 ) ) ;
#213663 = CARTESIAN_POINT ( 'NONE',  ( 5.207814216083940018, -1.861544245658670604, 0.1842191830812092979 ) ) ;
#213664 = CARTESIAN_POINT ( 'NONE',  ( 7.396136491454752715, 8.587579647240744407, 1.199719254218462483 ) ) ;
#213665 = EDGE_CURVE ( 'NONE', #79400, #133821, #61914, .T. ) ;
#213666 = CARTESIAN_POINT ( 'NONE',  ( -4.517891501851816649, 6.293959390292322986, -1.599625672291256517 ) ) ;
#213667 = CARTESIAN_POINT ( 'NONE',  ( -8.012344526598182026E-15, 10.60937500034139624, -1.575800808251669460 ) ) ;
#213668 = CARTESIAN_POINT ( 'NONE',  ( -6.247609857798938293, 6.183299677053865295, -0.7998128361456291469 ) ) ;
#213670 = CARTESIAN_POINT ( 'NONE',  ( -4.963693635934603776, 4.963599794778024155, 0.000000000000000000 ) ) ;
#213669 = CARTESIAN_POINT ( 'NONE',  ( 3.602716132929354664, 5.226254793216122074, 1.599625672291267398 ) ) ;
#213671 = CARTESIAN_POINT ( 'NONE',  ( -6.071018923869249129, 10.30488218781460574, 0.7998128361456291469 ) ) ;
#213672 = CARTESIAN_POINT ( 'NONE',  ( -6.230135280679522936, 7.227244901336242755, 1.199719254218450271 ) ) ;
#213673 = CARTESIAN_POINT ( 'NONE',  ( 1.622023338512183832, 2.040292009219225378, -0.3499636251925800079 ) ) ;
#213674 = CARTESIAN_POINT ( 'NONE',  ( 2.478245404118933237, -2.111759443744887221, -0.1527427581556138059 ) ) ;
#213675 = CARTESIAN_POINT ( 'NONE',  ( 8.320953590485093088, 10.73086516036454618, 1.599625672291281386 ) ) ;
#213677 = ADVANCED_FACE ( 'NONE', ( #97609 ), #114961, .F. ) ;
#213676 = CARTESIAN_POINT ( 'NONE',  ( -11.84668730067608600, 13.40000000000000036, -1.400000000000001910 ) ) ;
#213678 = CARTESIAN_POINT ( 'NONE',  ( 6.948098034395241207, -0.8905871627266357393, 1.867117781285509537 ) ) ;
#213679 = CARTESIAN_POINT ( 'NONE',  ( 4.595133766160131472, 7.156059413716462814, 1.333087067838649720 ) ) ;
#213680 = CARTESIAN_POINT ( 'NONE',  ( 5.558479791922850133, 6.547609847740540445, -1.082531754730542195 ) ) ;
#213682 = DIRECTION ( 'NONE',  ( 0.000000000000000000, 0.000000000000000000, 1.000000000000000000 ) ) ;
#213681 = CARTESIAN_POINT ( 'NONE',  ( -4.370663978927098015, 5.060324124126027279, 1.009771797811723326 ) ) ;
#213683 = CARTESIAN_POINT ( 'NONE',  ( 2.572590238467100665, -2.194022629849821104, -0.6638836622538509813 ) ) ;
#213684 = CARTESIAN_POINT ( 'NONE',  ( 6.609000000000038177, 0.002801690667396730672, 2.000160786441218530 ) ) ;
#213685 = CARTESIAN_POINT ( 'NONE',  ( 2.478646075381494285, -1.315928518397539548, 1.387899491812602859 ) ) ;
#213686 = EDGE_CURVE ( 'NONE', #28237, #154122, #98660, .T. ) ;
#213687 = VERTEX_POINT ( 'NONE', #16304 ) ;
#213688 = CARTESIAN_POINT ( 'NONE',  ( 7.795575137733369075, 9.157554417852841411, -1.082531754730537976 ) ) ;
#213689 = CARTESIAN_POINT ( 'NONE',  ( 0.2463402104127752068, 1.031448792800106595, -1.728751203700854111 ) ) ;
#213690 = CARTESIAN_POINT ( 'NONE',  ( 1.393326438508041942, -1.775833184744341375, 0.8338576968042878956 ) ) ;
#213691 = CARTESIAN_POINT ( 'NONE',  ( -8.784793466650835825, 12.33634391347959713, 1.199719254218462483 ) ) ;
#213692 = CARTESIAN_POINT ( 'NONE',  ( -7.888146445052511169, 8.097259028849730811, 1.040834085586084257E-14 ) ) ;
#213693 = CARTESIAN_POINT ( 'NONE',  ( -11.26761089376506497, 6.406307030788339851, 3.999051048939115560 ) ) ;
#213695 = CARTESIAN_POINT ( 'NONE',  ( 2.289615904538056412, -0.7594197407109636311, 1.598781567136787318 ) ) ;
#213694 = CARTESIAN_POINT ( 'NONE',  ( 4.417973705048302335, 1.286473518301757712, -1.647865739169761978 ) ) ;
#213696 = DIRECTION ( 'NONE',  ( 1.000000000000000000, -5.578564026256503701E-16, 1.972152263052529514E-31 ) ) ;
#213698 = CARTESIAN_POINT ( 'NONE',  ( 5.156304180611417820, -1.663069175626085139, 1.577778581399520652 ) ) ;
#213697 = CARTESIAN_POINT ( 'NONE',  ( -11.82646905334693699, 7.635427781191967078, -2.047549239027206092 ) ) ;
#213699 = CARTESIAN_POINT ( 'NONE',  ( 4.804519235412550771, 1.516407796731779722, 0.8538163389757484900 ) ) ;
#213700 = CARTESIAN_POINT ( 'NONE',  ( 8.028399517586572998, 12.51821653715971472, -0.7998128361456352531 ) ) ;
#213701 = CARTESIAN_POINT ( 'NONE',  ( 7.662794434365301832, -5.790678129197942781, -7.045261094876537733 ) ) ;
#213702 = CARTESIAN_POINT ( 'NONE',  ( 4.499182623014930549, 1.700326773844270667, 0.3381245445180857123 ) ) ;
#213703 = CARTESIAN_POINT ( 'NONE',  ( 5.143125006682406131, -0.2608717942136177248, -2.155377805267975067 ) ) ;
#213704 = CARTESIAN_POINT ( 'NONE',  ( 3.928111819657337911, 5.605883094398769195, 1.599625672291267398 ) ) ;
#213705 = CARTESIAN_POINT ( 'NONE',  ( 5.278529876733943915, -0.4946281652532491524, -1.954780475499573900 ) ) ;
#213706 = CARTESIAN_POINT ( 'NONE',  ( 0.2812500008225146120, 0.7852924545924094835, 1.895863743164083681 ) ) ;
#213707 = AXIS2_PLACEMENT_3D ( 'NONE', #17593, #68481, #84754 ) ;
#213708 = CARTESIAN_POINT ( 'NONE',  ( -1.201851678989727383E-14, 3.618750000682816381, -1.732050807568863648 ) ) ;
#213709 = CARTESIAN_POINT ( 'NONE',  ( 2.362220099979424059, 0.8219310624981416291, 1.742368475122471727 ) ) ;
#213710 = CARTESIAN_POINT ( 'NONE',  ( -6.009258394948636914E-15, 9.968750000682796042, -1.732050807568875195 ) ) ;
#213711 = CARTESIAN_POINT ( 'NONE',  ( 5.308899460236623291, -0.5399372957704140497, -2.154654435841397930 ) ) ;
#213712 = VERTEX_POINT ( 'NONE', #163666 ) ;
#213713 = CARTESIAN_POINT ( 'NONE',  ( 6.883263157960401557, 3.701933627517115966, 2.360572570571787043 ) ) ;
#213714 = CARTESIAN_POINT ( 'NONE',  ( -1.201851678989727383E-14, 2.837500000000024780, -1.732050807568863648 ) ) ;
#213715 = CARTESIAN_POINT ( 'NONE',  ( 6.810273232766058449, 6.839740281182199233, 1.040834085586084257E-14 ) ) ;
#213716 = CARTESIAN_POINT ( 'NONE',  ( 1.858359290357750160, 0.8465214129982703284, -2.053864850685551691 ) ) ;
#213717 = CARTESIAN_POINT ( 'NONE',  ( 0.7499999999999902300, 4.816666666666684193, -1.299038105676658228 ) ) ;
#213718 = CARTESIAN_POINT ( 'NONE',  ( 7.944714827928050838, 9.331550723079971021, 1.082531754730558626 ) ) ;
#213719 = CARTESIAN_POINT ( 'NONE',  ( 0.000000000000000000, 0.000000000000000000, 0.000000000000000000 ) ) ;
#213720 = CARTESIAN_POINT ( 'NONE',  ( 3.067887898442204442, 6.801229324816399746, 0.7998128361456271485 ) ) ;
#213721 = AXIS2_PLACEMENT_3D ( 'NONE', #107742, #44829, #25343 ) ;
#213722 = CARTESIAN_POINT ( 'NONE',  ( -3.363831509966360489, 6.938570838353784076, -0.7216878364870458196 ) ) ;
#213724 = CARTESIAN_POINT ( 'NONE',  ( 4.756332342268011715, -2.062141065897259207, -0.05393103437261077132 ) ) ;
#213723 = CARTESIAN_POINT ( 'NONE',  ( 10.53876547652418338, 11.18964789890005918, 0.7998128361456462443 ) ) ;
#213725 = CARTESIAN_POINT ( 'NONE',  ( -4.925689880466507908, 4.641059703499347044, -0.7998128361456221525 ) ) ;
#213726 = CARTESIAN_POINT ( 'NONE',  ( -1.500000000000011324, 5.452083334016153415, 0.8660254037844403729 ) ) ;
#213727 = CARTESIAN_POINT ( 'NONE',  ( 0.6823417656249882723, -0.9072916663252494907, 1.181850606188755259 ) ) ;
#213728 = CARTESIAN_POINT ( 'NONE',  ( 6.380143124955812262, -1.000617425381218561, 1.580232162242324545 ) ) ;
#213729 = CARTESIAN_POINT ( 'NONE',  ( 5.238767818816652877, 1.731821575490007703, -0.09270464131736801117 ) ) ;
#213730 = CARTESIAN_POINT ( 'NONE',  ( 4.124340800031966126, 0.09048578169197672716, 1.738227929847275588 ) ) ;
#213731 = CARTESIAN_POINT ( 'NONE',  ( 3.147464216666835402, 6.823792019419957278, -0.7998128361456291469 ) ) ;
#213732 = CARTESIAN_POINT ( 'NONE',  ( 1.857357856600039048, 0.3871700131025680447, -2.259295229882941403 ) ) ;
#213733 = CARTESIAN_POINT ( 'NONE',  ( 0.6823417656249899377, 4.738541667008086655, -1.181850606188754593 ) ) ;
#213734 = CARTESIAN_POINT ( 'NONE',  ( 5.337476071801405375, 0.8461711052811745626, -1.912038999733718825 ) ) ;
#213735 = CARTESIAN_POINT ( 'NONE',  ( 1.640310086786896049, -1.556016536173940645, 0.9838780322720328542 ) ) ;
#213736 = CARTESIAN_POINT ( 'NONE',  ( 9.333039360705550180, 4.446953957879813402, -7.472411811099956225 ) ) ;
#213737 = CARTESIAN_POINT ( 'NONE',  ( 2.239018641000252607, -1.631965468365924377, 0.8183158014263000046 ) ) ;
#213738 = CARTESIAN_POINT ( 'NONE',  ( 2.408827471728996361, -1.163269702728772392, -1.646838680093346996 ) ) ;
#213739 = CARTESIAN_POINT ( 'NONE',  ( 1.025618320672251560, -1.392776288830662512, -1.691927514038966907 ) ) ;
#213740 = CARTESIAN_POINT ( 'NONE',  ( 7.320801413324473650, 16.00000000000000000, -10.35317664616355771 ) ) ;
#213741 = CARTESIAN_POINT ( 'NONE',  ( -5.526920175865215334, 9.599823971818089774, 0.7998128361456481317 ) ) ;
#213742 = CARTESIAN_POINT ( 'NONE',  ( 1.820844063133007396, -1.465591517063179028, 1.462601037713284535 ) ) ;
#213743 = CARTESIAN_POINT ( 'NONE',  ( 5.087333953625774008, 6.958308917361963886, 1.599625672291267398 ) ) ;
#213744 = CARTESIAN_POINT ( 'NONE',  ( -0.6801582343750229853, -0.8697916663252605041, -1.178068619123862515 ) ) ;
#213745 = CARTESIAN_POINT ( 'NONE',  ( 3.932379033323248230, -1.091282289853046317, -1.817994770353311473 ) ) ;
#213746 = CARTESIAN_POINT ( 'NONE',  ( 0.6823417656249899377, 1.092708333674752286, 1.181850606188755259 ) ) ;
#213747 = CARTESIAN_POINT ( 'NONE',  ( 0.3109947909220554529, 1.675391530434092280, 0.9509023542121838313 ) ) ;
#213748 = VERTEX_POINT ( 'NONE', #82389 ) ;
#213749 = CARTESIAN_POINT ( 'NONE',  ( -5.794130544993808307, 7.853181283949808744, 1.599625672291263179 ) ) ;
#213750 = ADVANCED_FACE ( 'NONE', ( #48847 ), #141582, .T. ) ;
#213751 = CARTESIAN_POINT ( 'NONE',  ( 10.26082332744404368, 10.86538205830655279, -0.7998128361456281477 ) ) ;
#213752 = CARTESIAN_POINT ( 'NONE',  ( 5.356880090730857802, 8.303424968277756335, 1.082531754730548412 ) ) ;
#213753 = CARTESIAN_POINT ( 'NONE',  ( 3.475000000000000533, -3.602083332377418401, -2.006292185433951047 ) ) ;
#213754 = CARTESIAN_POINT ( 'NONE',  ( -6.715366157470410435, 6.729015360003925750, -0.7998128361456291469 ) ) ;
#213755 = CARTESIAN_POINT ( 'NONE',  ( 3.568621913994294292, 0.7309530501433506577, 1.883054584751037819 ) ) ;
#213756 = CARTESIAN_POINT ( 'NONE',  ( 0.5871190474453058528, -0.2578297629921856293, -2.090033075799145657 ) ) ;
#213757 = CARTESIAN_POINT ( 'NONE',  ( -5.712781623311813384, 7.758274208654143855, -1.599625672291271394 ) ) ;
#213758 = CARTESIAN_POINT ( 'NONE',  ( 7.540305987494599016, 11.94877408538573427, -0.7998128361456291469 ) ) ;
#213759 = CARTESIAN_POINT ( 'NONE',  ( 4.944130858096120740, -0.8794851946119870423, 1.640036094180880477 ) ) ;
#213760 = CARTESIAN_POINT ( 'NONE',  ( 9.023114925094663619, 10.48572115315399245, 1.199719254218453823 ) ) ;
#213761 = DIRECTION ( 'NONE',  ( 0.000000000000000000, 0.000000000000000000, -1.000000000000000000 ) ) ;
#213762 = ORIENTED_EDGE ( 'NONE', *, *, #151857, .T. ) ;
#213764 = CARTESIAN_POINT ( 'NONE',  ( -5.101945877444165944, 4.846691699973280976, 0.000000000000000000 ) ) ;
#213763 = AXIS2_PLACEMENT_3D ( 'NONE', #24638, #58224, #109183 ) ;
#213765 = CARTESIAN_POINT ( 'NONE',  ( -6.235860587281615075, 9.362588887548838557, -1.199719254218440723 ) ) ;
#213766 = CARTESIAN_POINT ( 'NONE',  ( 6.315316842782157991, -0.2547183123318246256, 2.045024454579154938 ) ) ;
#213768 = CARTESIAN_POINT ( 'NONE',  ( -5.193604695876673283, 6.642107527433549485, 1.420026453975403724 ) ) ;
#213767 = CARTESIAN_POINT ( 'NONE',  ( -5.098748287191073203, 8.106234214101666780, 1.199719254218452935 ) ) ;
#213769 = CARTESIAN_POINT ( 'NONE',  ( -0.6823417656250246877, 0.05104166700808931978, 1.181850606188755259 ) ) ;
#213770 = CARTESIAN_POINT ( 'NONE',  ( 2.301686711942134256, -1.551025276819127496, 0.7750448480700108389 ) ) ;
#213771 = CARTESIAN_POINT ( 'NONE',  ( 1.341335103225870240, 1.738211624227633978, 0.08822054626196448868 ) ) ;
#213773 = CARTESIAN_POINT ( 'NONE',  ( 6.643132081016111634, 9.733775946952057723, 1.082531754730558626 ) ) ;
#213772 = CARTESIAN_POINT ( 'NONE',  ( 0.5171989335802311682, 1.588149187230869952, -1.674348222103681172 ) ) ;
#213774 = CARTESIAN_POINT ( 'NONE',  ( -10.92050379694822837, 4.688480456342538183, -4.459762147120462039 ) ) ;
#213775 = CARTESIAN_POINT ( 'NONE',  ( 2.583338899891209017, 1.885494326376845775, -0.8321024974875782521 ) ) ;
#213776 = CARTESIAN_POINT ( 'NONE',  ( 1.511092056569414366, 2.013677475703846476, 0.1017375232199163593 ) ) ;
#213777 = CARTESIAN_POINT ( 'NONE',  ( 6.925078400183537042, 4.686282476709005884, 2.806848198465234479 ) ) ;
#213778 = CARTESIAN_POINT ( 'NONE',  ( -6.296835998904160014, 6.311006518335105397, 0.000000000000000000 ) ) ;
#213779 = CARTESIAN_POINT ( 'NONE',  ( 0.6199196518563926395, -1.052708125740812628, -1.666702442819472774 ) ) ;
#213781 = CARTESIAN_POINT ( 'NONE',  ( -7.458393901293492334, 7.874083437696761223, 0.7216878364870317197 ) ) ;
#213780 = CARTESIAN_POINT ( 'NONE',  ( 4.447458312869024155, -1.746245811230532130, 0.7801085911468002010 ) ) ;
#213782 = CARTESIAN_POINT ( 'NONE',  ( 5.848300530743933301, 2.204158087718602221, 0.1119919437090263481 ) ) ;
#213783 = CARTESIAN_POINT ( 'NONE',  ( -6.251718229232846369, 9.347402796530044355, -1.082531754730549967 ) ) ;
#213784 = CARTESIAN_POINT ( 'NONE',  ( 7.862802741282558294, 8.137967717776607657, 0.000000000000000000 ) ) ;
#213785 = CARTESIAN_POINT ( 'NONE',  ( -4.136646265500964148, 6.879818838842817641, -1.082531754730551743 ) ) ;
#213786 = CARTESIAN_POINT ( 'NONE',  ( 0.3639331001695153001, 0.6315192924679478015, -1.918485960686921565 ) ) ;
#213787 = CARTESIAN_POINT ( 'NONE',  ( -0.7500000000000006661, 12.73958333401613352, -1.299038105676657340 ) ) ;
#213788 = CARTESIAN_POINT ( 'NONE',  ( 4.331326240856082421, 0.1090238329626690705, 2.305124713103424483 ) ) ;
#213789 = CARTESIAN_POINT ( 'NONE',  ( 5.142999638377217408, -0.2383176028181442918, -1.947251298587366231 ) ) ;
#213790 = CARTESIAN_POINT ( 'NONE',  ( 1.938261246079517219, -1.053878627966830184, 1.654468565904606558 ) ) ;
#213791 = CARTESIAN_POINT ( 'NONE',  ( 8.940712233207955606, 12.51824914112961729, 1.199719254218450271 ) ) ;
#213792 = CARTESIAN_POINT ( 'NONE',  ( -9.421011374644489678, 14.56515202819860377, 7.432750069618532685 ) ) ;
#213793 = ORIENTED_EDGE ( 'NONE', *, *, #181594, .T. ) ;
#213794 = CARTESIAN_POINT ( 'NONE',  ( 0.4798920220053382590, -0.7558346266652364864, 1.978032726644059158 ) ) ;
#213796 = CARTESIAN_POINT ( 'NONE',  ( -7.965578943228732278, 9.251929174310385307, -1.199719254218446718 ) ) ;
#213795 = CARTESIAN_POINT ( 'NONE',  ( -5.168682875307782254, 7.053215992657626110, -1.599625672291256295 ) ) ;
#213797 = CARTESIAN_POINT ( 'NONE',  ( 1.060217833243476182, -1.663605802054025418, -0.7890760572396152694 ) ) ;
#213798 = VERTEX_POINT ( 'NONE', #31534 ) ;
#213799 = CARTESIAN_POINT ( 'NONE',  ( 4.170888513267295039, 1.539375584636338390, -1.531221199927160770 ) ) ;
#213800 = CARTESIAN_POINT ( 'NONE',  ( 9.423393029473404070, 13.09419267589542457, -7.355985009210963987 ) ) ;
#213801 = CARTESIAN_POINT ( 'NONE',  ( 2.285534418239891785, 0.09939759515392716793, -2.118372479656557061 ) ) ;
#213802 = CARTESIAN_POINT ( 'NONE',  ( -1.499999999999997780, 2.681250000682818158, 1.214306433183764966E-14 ) ) ;
#213803 = CARTESIAN_POINT ( 'NONE',  ( 7.716561984472250835, 12.15440608185967086, 1.040834085586084257E-14 ) ) ;
#213804 = DIRECTION ( 'NONE',  ( 0.000000000000000000, -1.000000000000000000, 0.000000000000000000 ) ) ;
#213805 = CARTESIAN_POINT ( 'NONE',  ( 6.599791786788117953, 6.770233575417231364, 0.1470628079319712123 ) ) ;
#213806 = AXIS2_PLACEMENT_3D ( 'NONE', #59343, #76653, #175249 ) ;
#213807 = CARTESIAN_POINT ( 'NONE',  ( 2.389980588989379040, -0.8839831138988951675, 1.861718010716238547 ) ) ;
#213809 = CARTESIAN_POINT ( 'NONE',  ( -1.500000000000035971, 7.750000000000000000, -9.886859966642584041 ) ) ;
#213808 = CARTESIAN_POINT ( 'NONE',  ( -7.153898609505128015, 11.49796547773133604, 0.7998128361456481317 ) ) ;
#213810 = STYLED_ITEM ( 'NONE', ( #8916 ), #9062 ) ;
#213811 = CARTESIAN_POINT ( 'NONE',  ( -1.201851678989727383E-14, 2.821875000341418804, 1.575800808251672791 ) ) ;
#213812 = CARTESIAN_POINT ( 'NONE',  ( -0.02264175331115856130, 5.720791440175713838, -2.683188945093956335 ) ) ;
#213813 = CARTESIAN_POINT ( 'NONE',  ( -10.83760191302001097, 4.885617943545219610, -4.963142630924989973 ) ) ;
#213814 = CARTESIAN_POINT ( 'NONE',  ( 5.303337639526568559, 1.684534858470821961, -0.9050978215178404618 ) ) ;
#213815 = B_SPLINE_CURVE_WITH_KNOTS ( 'NONE', 3,
 ( #174588, #91198, #192924, #74930 ),
 .UNSPECIFIED., .F., .F.,
 ( 4, 4 ),
 ( 0.000000000000000000, 0.0002908967400263839909 ),
 .UNSPECIFIED. ) ;
#213816 = CARTESIAN_POINT ( 'NONE',  ( -4.189106276498259618, 6.870745841681152655, 1.082531754730560403 ) ) ;
#213817 = CARTESIAN_POINT ( 'NONE',  ( 1.634417699101225585, 1.115656568974830343, -1.968152581808318757 ) ) ;
#213818 = CARTESIAN_POINT ( 'NONE',  ( -8.012505595996376684, 12.29174759539704986, 0.000000000000000000 ) ) ;
#213819 = CARTESIAN_POINT ( 'NONE',  ( 1.072181177352715453, 0.7354878280073854357, 1.655762779942154372 ) ) ;
#213820 = CARTESIAN_POINT ( 'NONE',  ( 1.657307721912592458, 1.831997054396968361, -0.5600143317019135036 ) ) ;
#213821 = CIRCLE ( 'NONE', #23506, 0.6500000000000000222 ) ;
#213822 = CARTESIAN_POINT ( 'NONE',  ( 3.244645865714153032, -2.039272935636734285, -0.3565889006169955522 ) ) ;
#213823 = CARTESIAN_POINT ( 'NONE',  ( 1.364683531249988535, 1.926041667008086211, 0.7879004041258500513 ) ) ;
#213824 = CARTESIAN_POINT ( 'NONE',  ( 1.129686040349969556, -1.248873030102001902, -1.525460987127578605 ) ) ;
#213825 = CARTESIAN_POINT ( 'NONE',  ( 5.109954983015153829, -1.917020813385891254, 0.1909056391717136592 ) ) ;
#213826 = ADVANCED_FACE ( 'NONE', ( #80268 ), #210255, .F. ) ;
#213828 = CARTESIAN_POINT ( 'NONE',  ( 5.631620320865258655, 7.357208097040313532, -1.234165276361798735 ) ) ;
#213827 = CARTESIAN_POINT ( 'NONE',  ( 0.6632354941851228425, -1.667548007495605944, 1.595465711622134242 ) ) ;
#213829 = CARTESIAN_POINT ( 'NONE',  ( 1.364683531249986537, 2.155208333674751398, -0.7879004041258239610 ) ) ;
#213830 = CARTESIAN_POINT ( 'NONE',  ( 4.861816908638716406, -0.5531579045409695805, 1.987044815706548562 ) ) ;
#213831 = CARTESIAN_POINT ( 'NONE',  ( -6.274726165026268454, 6.214935368819085149, 0.7998128361456341429 ) ) ;
#213832 = CARTESIAN_POINT ( 'NONE',  ( 8.288111976655649471, 8.563885482386732306, -0.7998128361456291469 ) ) ;
#213833 = DIRECTION ( 'NONE',  ( 1.000000000000000000, -0.000000000000000000, -0.000000000000000000 ) ) ;
#213835 = CARTESIAN_POINT ( 'NONE',  ( 1.499999999999990896, 5.775000000000023448, 1.040834085586084257E-14 ) ) ;
#213834 = CARTESIAN_POINT ( 'NONE',  ( 6.493207903183886742, 1.834288230482609583, -1.034473908808232201 ) ) ;
#213836 = CARTESIAN_POINT ( 'NONE',  ( -1.402160292154681736E-14, 2.259375000341416140, -1.575800808251660134 ) ) ;
#213837 = CARTESIAN_POINT ( 'NONE',  ( 4.657600047955182454, 0.4785990281669267876, -2.107782517917502929 ) ) ;
#213838 = CARTESIAN_POINT ( 'NONE',  ( 5.197918162715867929, 1.358090353789550342, 1.495039904793266095 ) ) ;
#213839 = CARTESIAN_POINT ( 'NONE',  ( 1.479373551132449505, 3.300000000000025135, 0.2478989637125245671 ) ) ;
#213840 = CARTESIAN_POINT ( 'NONE',  ( -4.270455198624581783, 7.926022131796578662, 1.040834085586084257E-14 ) ) ;
#213843 = CARTESIAN_POINT ( 'NONE',  ( 3.714570900464269076, 7.277490450609545469, 0.7216878364870298324 ) ) ;
#213842 = CARTESIAN_POINT ( 'NONE',  ( -3.285556943749998737, -1.480208332855375453, 1.896917185911908499 ) ) ;
#213841 = CARTESIAN_POINT ( 'NONE',  ( 6.607619761813720238, 8.802252036906432764, 1.599625672291268286 ) ) ;
#213844 =( BOUNDED_SURFACE ( )  B_SPLINE_SURFACE ( 3, 2, ( 
 ( #42168, #140754, #28025 ),
 ( #190511, #93054, #8568 ),
 ( #156979, #24814, #74648 ),
 ( #11761, #9634, #108285 ) ),
 .UNSPECIFIED., .F., .F., .T. ) 
 B_SPLINE_SURFACE_WITH_KNOTS ( ( 4, 4 ),
 ( 3, 3 ),
 ( 4.363913744254155347E-18, 0.0001288481725834512569 ),
 ( 0.000000000000000000, 1.000000000000000000 ),
 .UNSPECIFIED. ) 
 GEOMETRIC_REPRESENTATION_ITEM ( )  RATIONAL_B_SPLINE_SURFACE ( (
 ( 1.000000000000000000, 0.7779734834199445448, 1.000000000000000000),
 ( 1.000000000000000000, 0.8164436902882270530, 1.000000000000000000),
 ( 1.000000000000000000, 0.8496999780322816997, 1.000000000000000000),
 ( 1.000000000000000000, 0.8739472344167453777, 1.000000000000000000) ) ) 
 REPRESENTATION_ITEM ( '' )  SURFACE ( )  );
#213845 = CARTESIAN_POINT ( 'NONE',  ( -5.978219388983010418, 5.939287140093762574, -0.7998128361456362523 ) ) ;
#213846 = CARTESIAN_POINT ( 'NONE',  ( 3.925017756809038527, -1.752140073516525565, 0.9981236898717813499 ) ) ;
#213847 = CARTESIAN_POINT ( 'NONE',  ( -7.853197290813634268, 10.18514947741448573, 1.599625672291295375 ) ) ;
#213848 = CARTESIAN_POINT ( 'NONE',  ( -2.605138072120212200, 6.191078184115536232, -0.7998128361456281477 ) ) ;
#213849 = CARTESIAN_POINT ( 'NONE',  ( 1.364683531249990311, 5.113541667008084879, 0.7879004041258500513 ) ) ;
#213851 = CARTESIAN_POINT ( 'NONE',  ( 0.6823417656249969321, 8.776041667008065872, -1.181850606188757036 ) ) ;
#213850 = CARTESIAN_POINT ( 'NONE',  ( 4.768538688506021472, -1.414568798902924307, 1.634688457493836289 ) ) ;
#213852 = CARTESIAN_POINT ( 'NONE',  ( -11.51728355775449231, 7.078142246183236175, 3.212931496948879140 ) ) ;
#213854 = CARTESIAN_POINT ( 'NONE',  ( 6.064077406165095496, -1.076301619396256237, 1.704949653848472302 ) ) ;
#213853 = CARTESIAN_POINT ( 'NONE',  ( -6.954969613686107444, 10.09758640173367894, 1.082531754730549967 ) ) ;
#213855 = CARTESIAN_POINT ( 'NONE',  ( 0.6823417656249864960, -0.5114583329919111243, -1.181850606188749264 ) ) ;
#213856 = EDGE_CURVE ( 'NONE', #187130, #170487, #195091, .T. ) ;
#213857 = CARTESIAN_POINT ( 'NONE',  ( 0.5567383370381777663, -1.454440682700371079, -0.9269339563611042054 ) ) ;
#213858 = CARTESIAN_POINT ( 'NONE',  ( 3.874598038455354665, 7.742391154831717692, -0.7998128361456362523 ) ) ;
#213860 = CARTESIAN_POINT ( 'NONE',  ( 7.205232291019763480, 7.370802192470005565, -0.7998128361456341429 ) ) ;
#213859 = CARTESIAN_POINT ( 'NONE',  ( 7.239690840017413365, 10.42976116578691403, -1.082531754730537976 ) ) ;
#213861 = CARTESIAN_POINT ( 'NONE',  ( -11.15508160014129224, 7.312941860064643862, -4.429679592206957395 ) ) ;
#213862 = CARTESIAN_POINT ( 'NONE',  ( 0.1745949693968693039, 0.009193469831081376581, -1.755468632744116686 ) ) ;
#213863 = CARTESIAN_POINT ( 'NONE',  ( 0.8912715949961318440, -0.05164314158133917476, -2.012595864970234238 ) ) ;
#213864 = CARTESIAN_POINT ( 'NONE',  ( 3.575398329460587554, 0.05639400328332971890, -2.206221599391814170 ) ) ;
#213865 = CARTESIAN_POINT ( 'NONE',  ( -5.248414861821563804, 9.137251415518218067, 0.7216878364870267237 ) ) ;
#213866 = ORIENTED_EDGE ( 'NONE', *, *, #61776, .T. ) ;
#213867 = CARTESIAN_POINT ( 'NONE',  ( 8.636180661780656465, 11.09863007687603087, -1.443375672974052559 ) ) ;
#213869 = CARTESIAN_POINT ( 'NONE',  ( 2.126577575561945821, 0.4445254776237593242, 1.966640697269490312 ) ) ;
#213868 = CARTESIAN_POINT ( 'NONE',  ( 2.280079029133400326, 2.079044457705871096, -0.4163345062310334632 ) ) ;
#213871 = ORIENTED_EDGE ( 'NONE', *, *, #190098, .T. ) ;
#213870 = CARTESIAN_POINT ( 'NONE',  ( 2.478518767674630308, -1.246658584539367176, 1.314663817856591699 ) ) ;
#213872 = ADVANCED_FACE ( 'NONE', ( #130169 ), #64023, .F. ) ;
#213873 = CARTESIAN_POINT ( 'NONE',  ( 6.933015448541703485, 9.181880338089085214, 1.599625672291268286 ) ) ;
#213874 = CARTESIAN_POINT ( 'NONE',  ( 7.149227073107712549, 7.235186428247455837, -0.7998128361456281477 ) ) ;
#213876 = CARTESIAN_POINT ( 'NONE',  ( 6.609000000000045283, 0.005669918681758949128, 1.900160851458796651 ) ) ;
#213875 = CARTESIAN_POINT ( 'NONE',  ( -3.255929445576174697, 6.950334786480840243, -0.7998128361456281477 ) ) ;
#213877 = CIRCLE ( 'NONE', #47900, 6.264285714285709794 ) ;
#213878 = CARTESIAN_POINT ( 'NONE',  ( -2.665936209291942305, 0.4260822056534815938, -0.1252292841820018543 ) ) ;
#213879 = CARTESIAN_POINT ( 'NONE',  ( 5.608757509019036469, 5.629766575900002401, 2.420000000000000373 ) ) ;
#213880 = CARTESIAN_POINT ( 'NONE',  ( 6.277061933002788585, 6.425586464699131639, 0.7216878364870317197 ) ) ;
#213881 = CARTESIAN_POINT ( 'NONE',  ( -0.6823417656250003738, -0.2197916663252488800, -1.181850606188749264 ) ) ;
#213882 = LINE ( 'NONE', #178235, #46566 ) ;
#213883 = CARTESIAN_POINT ( 'NONE',  ( -8.296699936558862731, 11.76690146170562201, 1.199719254218453823 ) ) ;
#213884 = CARTESIAN_POINT ( 'NONE',  ( 3.573254463033649131, 0.05508235185803719847, -2.161170636208443963 ) ) ;
#213885 = CARTESIAN_POINT ( 'NONE',  ( -6.943184063974186415, 7.273005294157565359, -0.7216878364870338292 ) ) ;
#213886 = EDGE_CURVE ( 'NONE', #89507, #62493, #24011, .T. ) ;
#213887 = CARTESIAN_POINT ( 'NONE',  ( 4.231553341240963384, 7.950912974840849579, -0.7216878364870357165 ) ) ;
#213888 = CARTESIAN_POINT ( 'NONE',  ( 2.391022662813433453, -2.030629854096975606, -0.6112283555373964061 ) ) ;
#213889 = CARTESIAN_POINT ( 'NONE',  ( 6.581069972421211389, -0.09314021972051109155, -1.823315219958022482 ) ) ;
#213890 = CARTESIAN_POINT ( 'NONE',  ( 2.846899755239293839, -1.641009487379685217, 1.092116875444639090 ) ) ;
#213891 = CARTESIAN_POINT ( 'NONE',  ( 5.519756697582541172, -0.4584384640409416289, 1.856529252577573619 ) ) ;
#213892 = EDGE_LOOP ( 'NONE', ( #140177, #87718, #79362, #177920 ) ) ;
#213893 = SURFACE_STYLE_USAGE ( .BOTH. , #11453 ) ;
#213894 = CARTESIAN_POINT ( 'NONE',  ( 5.951603224533720038, 1.490215702738381331, 1.287855809377226102 ) ) ;
#213895 = CARTESIAN_POINT ( 'NONE',  ( 1.394366005188719893, 1.587816662021741543, -1.117778254020968420 ) ) ;
#213896 = ORIENTED_EDGE ( 'NONE', *, *, #206842, .F. ) ;
#213897 = CARTESIAN_POINT ( 'NONE',  ( -4.510196435976065565, 7.040407170307378060, -1.149263043085164915 ) ) ;
#213899 = CARTESIAN_POINT ( 'NONE',  ( 1.833030277982334422, 2.525853874188491055, -2.500000000000000444 ) ) ;
#213898 = CARTESIAN_POINT ( 'NONE',  ( -6.699137298928187434, 8.909022496873262753, 1.443375672974064550 ) ) ;
#213901 = CARTESIAN_POINT ( 'NONE',  ( 7.806797523370503811, 8.002351953554066810, 1.040834085586084257E-14 ) ) ;
#213900 = CARTESIAN_POINT ( 'NONE',  ( 2.712926231669846810, -0.2040156676378352685, 2.080649193556554533 ) ) ;
#213903 = CARTESIAN_POINT ( 'NONE',  ( 3.716343503477301802, 7.349834830783237294, -1.734723475976807094E-15 ) ) ;
#213902 = CARTESIAN_POINT ( 'NONE',  ( 7.657657833620182153, 7.828355648845348291, -0.7998128361456281477 ) ) ;
#213905 = ORIENTED_EDGE ( 'NONE', *, *, #126844, .F. ) ;
#213904 = CARTESIAN_POINT ( 'NONE',  ( 5.672493831469004100, 0.7790509395085333244, 1.746586765831580124 ) ) ;
#213906 = CARTESIAN_POINT ( 'NONE',  ( 4.301547675229603129, 1.771612934706376707, 1.315755017190944676 ) ) ;
#213907 = CARTESIAN_POINT ( 'NONE',  ( 1.554063478550568256, 0.6399170599369340406, -2.111937735441645980 ) ) ;
#213908 = CARTESIAN_POINT ( 'NONE',  ( -11.00593736619310725, 12.48999492864588134, 1.443925800506593804 ) ) ;
#213909 = CARTESIAN_POINT ( 'NONE',  ( 0.3110002902955294468, 1.589785527739733695, -1.062417771062994287 ) ) ;
#213910 = CARTESIAN_POINT ( 'NONE',  ( -0.4373225248172924462, -7.723431457505077979, 10.96785329849814161 ) ) ;
#213911 = DIRECTION ( 'NONE',  ( 0.000000000000000000, 0.000000000000000000, -1.000000000000000000 ) ) ;
#213912 = CARTESIAN_POINT ( 'NONE',  ( 3.842288295254093100, -1.023014542950370975, 1.799900136785845817 ) ) ;
#213914 = CARTESIAN_POINT ( 'NONE',  ( 2.044033295145482043, 0.8276103948961744949, -1.997198329219296742 ) ) ;
#213913 = CARTESIAN_POINT ( 'NONE',  ( -3.898132859128961236, 4.506575409527250997, -1.199719254218452047 ) ) ;
#213915 = CARTESIAN_POINT ( 'NONE',  ( 3.193114300108112147, 1.729001323093733111, 1.346577201094656395 ) ) ;
#213916 = CARTESIAN_POINT ( 'NONE',  ( 2.324088772396477673E-16, 0.6875000000000069944, -1.225000000000008749 ) ) ;
#213917 = STYLED_ITEM ( 'NONE', ( #115981 ), #155333 ) ;
#213918 = DIRECTION ( 'NONE',  ( -1.000000000000000000, 0.000000000000000000, 0.000000000000000000 ) ) ;
#213919 = CARTESIAN_POINT ( 'NONE',  ( 1.408343819019456176E-15, 0.2000000000000057288, 11.50000000000000000 ) ) ;
#213920 = CARTESIAN_POINT ( 'NONE',  ( -1.364683531250014514, 14.15104166700806765, -0.7879004041258335089 ) ) ;
#213921 = CARTESIAN_POINT ( 'NONE',  ( -4.736594563127865420, 6.619389305106191834, -1.599625672291271394 ) ) ;
#213922 = CARTESIAN_POINT ( 'NONE',  ( 6.557244222609861062, -1.057944526735156821, 1.374202748628235327 ) ) ;
#213923 = CARTESIAN_POINT ( 'NONE',  ( -10.16825202056928390, 10.96530823352674133, 0.7216878364870438212 ) ) ;
#213924 = CARTESIAN_POINT ( 'NONE',  ( 4.153231765667256603, 1.751622898902647663, -1.103220242290925190 ) ) ;
#213925 = CARTESIAN_POINT ( 'NONE',  ( 5.273117041167244778, 1.866726688708058690, -0.9990383793265914525 ) ) ;
#213926 = CARTESIAN_POINT ( 'NONE',  ( 6.531277313481192337, 8.642909503859968368, 1.599625672291281386 ) ) ;
#213928 = EDGE_CURVE ( 'NONE', #9480, #137589, #189864, .T. ) ;
#213927 = CARTESIAN_POINT ( 'NONE',  ( 9.445304453185871196, 4.469082159062184978, 7.402818517570845636 ) ) ;
#213929 = CARTESIAN_POINT ( 'NONE',  ( 3.660960169446208390, 1.555274301336776022, -1.208163239264722133 ) ) ;
#213930 = CARTESIAN_POINT ( 'NONE',  ( 5.859400655334408015, 2.259312458388713196, -0.3864819027975390786 ) ) ;
#213931 = CARTESIAN_POINT ( 'NONE',  ( 2.965264444195826243, 0.2674972279559268973, -1.805858685475017378 ) ) ;
#213932 = EDGE_CURVE ( 'NONE', #71711, #34262, #52905, .T. ) ;
#213933 = CARTESIAN_POINT ( 'NONE',  ( 3.203469434578891661, 6.959407783642502565, -0.7998128361456362523 ) ) ;
#213934 = CARTESIAN_POINT ( 'NONE',  ( 4.650083499362875017, 5.487814173087225633, 1.082531754730560403 ) ) ;
#213935 = CARTESIAN_POINT ( 'NONE',  ( -6.181627972826976958, 9.299317504018391745, 1.199719254218452047 ) ) ;
#213936 = CARTESIAN_POINT ( 'NONE',  ( 6.703580607314123085, 6.785541894813420072, 0.000000000000000000 ) ) ;
#213937 = ORIENTED_EDGE ( 'NONE', *, *, #11640, .T. ) ;
#213938 = CARTESIAN_POINT ( 'NONE',  ( 4.148693527746351251, 1.975194156771160170, 0.3885511358477158894 ) ) ;
#213939 = CARTESIAN_POINT ( 'NONE',  ( 6.100222456320119058, -0.2858642287353658218, 2.280774976835740819 ) ) ;
#213940 = CARTESIAN_POINT ( 'NONE',  ( 4.399235598239510381, -1.708881994454291675, 0.9632455365647660805 ) ) ;
#213941 = CARTESIAN_POINT ( 'NONE',  ( -7.528855374290365887, 7.678086112960552434, -0.7998128361456291469 ) ) ;
#213942 = CARTESIAN_POINT ( 'NONE',  ( -3.924195396151603177, 6.665646164563756138, 1.199719254218464037 ) ) ;
#213943 = CARTESIAN_POINT ( 'NONE',  ( -7.962224162659105708, -5.254973434576998059, 7.552496594302672506 ) ) ;
#213944 = CARTESIAN_POINT ( 'NONE',  ( -5.261446130555064826, 8.296048364692991228, 1.199719254218452935 ) ) ;
#213946 = CARTESIAN_POINT ( 'NONE',  ( 6.280137008050575176, -0.9429096061123897199, 1.497559920798942512 ) ) ;
#213945 = CARTESIAN_POINT ( 'NONE',  ( 0.8551579053767807137, 0.4041549552570160575, -2.051131941465775821 ) ) ;
#213947 = CARTESIAN_POINT ( 'NONE',  ( 2.396645607016957502, 1.759237466006560391, -1.306522788049699679 ) ) ;
#213948 = CARTESIAN_POINT ( 'NONE',  ( 0.9951963871240524506, -1.740626720728695620, -0.001451476259923395245 ) ) ;
#213949 = AXIS2_PLACEMENT_3D ( 'NONE', #48985, #101983, #134520 ) ;
#213950 = CARTESIAN_POINT ( 'NONE',  ( 6.908042961362778733, 8.018137195466769285, 1.199719254218462483 ) ) ;
#213951 = CARTESIAN_POINT ( 'NONE',  ( 0.2333690889706717397, 7.629137130509078268, -2.653349640194931247 ) ) ;
#213952 = CARTESIAN_POINT ( 'NONE',  ( 1.171983892495536805, -1.097183398155553435, 1.330944738974817243 ) ) ;
#213953 = CARTESIAN_POINT ( 'NONE',  ( 1.786939262935317130, 1.904797134731281538, -1.083727916527020607 ) ) ;
#213954 = CARTESIAN_POINT ( 'NONE',  ( 4.090592613104036879, -2.182713160620152859, -0.3248913242878055385 ) ) ;
#213955 = CARTESIAN_POINT ( 'NONE',  ( 1.147616990042895191, 1.915638116573715743, -1.021621585119661058 ) ) ;
#213956 = CARTESIAN_POINT ( 'NONE',  ( 9.499668754385636404, -7.246166700194470067, 0.07933194154488391880 ) ) ;
#213957 = CARTESIAN_POINT ( 'NONE',  ( 2.184896953550282461, 1.697450634274371595, -1.265404921814163641 ) ) ;
#213958 = CARTESIAN_POINT ( 'NONE',  ( 6.727182134110227807, 1.996671600852136352, 2.590479658440256738 ) ) ;
#213959 = VERTEX_POINT ( 'NONE', #165787 ) ;
#213960 = CIRCLE ( 'NONE', #131048, 11.95586206894162906 ) ;
#213962 = CARTESIAN_POINT ( 'NONE',  ( -1.402160292154681736E-14, 0.6343750003414162508, 1.575800808251672791 ) ) ;
#213961 = CARTESIAN_POINT ( 'NONE',  ( 2.753816761298252036, 2.281055701876167685, -0.2276813034018300430 ) ) ;
#213963 = SURFACE_SIDE_STYLE ('',( #45135 ) ) ;
#213964 = CARTESIAN_POINT ( 'NONE',  ( 4.436542580169809291, 6.199052314996659874, 1.599625672291267398 ) ) ;
#213965 = CARTESIAN_POINT ( 'NONE',  ( 4.582826572872266802, -1.451171176318547529, 1.681852496032259614 ) ) ;
#213966 = CARTESIAN_POINT ( 'NONE',  ( -8.676855123066030018, 9.225345186439589895, -0.7216878364870267237 ) ) ;
#213967 = FACE_OUTER_BOUND ( 'NONE', #119925, .T. ) ;
#213968 = CARTESIAN_POINT ( 'NONE',  ( 3.701012746850603996, 7.261672604726938651, 1.040834085586084257E-14 ) ) ;
#213969 = CARTESIAN_POINT ( 'NONE',  ( -7.998947441938374148, 8.434452891790657603, 1.040834085586084257E-14 ) ) ;
#213970 = CARTESIAN_POINT ( 'NONE',  ( 3.418064124421011041, 7.001842221884225559, -0.7216878364870338292 ) ) ;
#213971 = VERTEX_POINT ( 'NONE', #194010 ) ;
#213972 = CARTESIAN_POINT ( 'NONE',  ( 3.252577435111691617, 1.966644794889659043, -0.4445022851852917234 ) ) ;
#213974 = CARTESIAN_POINT ( 'NONE',  ( 1.622013285028017338, 2.032735996446675131, -0.3486163383695956575 ) ) ;
#213973 = CARTESIAN_POINT ( 'NONE',  ( 5.750629710490689384, 9.860818428881154674, -0.7998128361456291469 ) ) ;
#213975 = CARTESIAN_POINT ( 'NONE',  ( -11.91826849282518452, 13.39999999999998437, 1.399999999999998579 ) ) ;
#213976 = CARTESIAN_POINT ( 'NONE',  ( 4.367134876933267407, 8.109091433148536865, 0.000000000000000000 ) ) ;
#213977 = CARTESIAN_POINT ( 'NONE',  ( -10.32992389895503393, 1.000000000000000888, -6.106772653521458594 ) ) ;
#213978 = CARTESIAN_POINT ( 'NONE',  ( 1.364683531249988535, 3.405208333674749621, -0.7879004041258239610 ) ) ;
#213979 = CARTESIAN_POINT ( 'NONE',  ( 3.767680093253112705, 1.217039798425190167, 1.822233383357040104 ) ) ;
#213980 = CARTESIAN_POINT ( 'NONE',  ( 2.795546247670523954, 1.458556481301529706, -1.392545902517070111 ) ) ;
#213981 = CARTESIAN_POINT ( 'NONE',  ( 1.048114208743459619, -1.451426956872736262, 1.132798186660122441 ) ) ;
#213982 = CARTESIAN_POINT ( 'NONE',  ( 6.286176778230493589, 10.48562334124426698, 0.7998128361456462443 ) ) ;
#213983 = CARTESIAN_POINT ( 'NONE',  ( 4.998959831394860664, 1.517082468864182632, -1.015166198912627049 ) ) ;
#213984 = CARTESIAN_POINT ( 'NONE',  ( 5.801407773674092105, 1.352156682446105984, -1.496049708713815374 ) ) ;
#213985 = CARTESIAN_POINT ( 'NONE',  ( -7.202405917357668663, 9.425892875049191488, 1.599625672291295375 ) ) ;
#213987 = CARTESIAN_POINT ( 'NONE',  ( -4.796552484184649856, 8.818004674849227342, -0.7998128361456362523 ) ) ;
#213986 = CARTESIAN_POINT ( 'NONE',  ( 4.135799973978175892, -1.557659423114423847, -1.641163307807387950 ) ) ;
#213988 = CARTESIAN_POINT ( 'NONE',  ( 0.8035136555551088966, 1.722860008830621847, 1.211028463478396988 ) ) ;
#213989 = CARTESIAN_POINT ( 'NONE',  ( -7.761116589180078407, 8.019333873657032541, 0.000000000000000000 ) ) ;
#213990 = CARTESIAN_POINT ( 'NONE',  ( 5.037584538744971141, 1.933038169019934527, -0.7419538039311265321 ) ) ;
#213991 = CARTESIAN_POINT ( 'NONE',  ( 9.673906298550626559, 11.24497775551929557, 1.199719254218452047 ) ) ;
#213992 = CARTESIAN_POINT ( 'NONE',  ( -1.360316468750058627, 2.692708333674814991, 0.7853790794158641564 ) ) ;
#213993 = PRODUCT_CONTEXT ( 'NONE', #104451, 'mechanical' ) ;
#213994 = CARTESIAN_POINT ( 'NONE',  ( -7.492852449846775897, 11.89341162479659531, 0.000000000000000000 ) ) ;
#213995 = UNCERTAINTY_MEASURE_WITH_UNIT (LENGTH_MEASURE( 1.000000000000000082E-05 ), #101529, 'distance_accuracy_value', 'NONE');
#213996 = CARTESIAN_POINT ( 'NONE',  ( 3.570880328030153539, 7.341005539872356600, 0.2896471194287209006 ) ) ;
#213997 = CARTESIAN_POINT ( 'NONE',  ( 7.309781096423290769, 8.557108029695882578, 1.199719254218452935 ) ) ;
#213998 = CARTESIAN_POINT ( 'NONE',  ( 5.253083726123439767, 6.394172465367824465, -1.148862164228587890 ) ) ;
#213999 = CARTESIAN_POINT ( 'NONE',  ( -4.277761160311629673, 4.949475094240346706, 1.199719254218462483 ) ) ;
#214001 = CARTESIAN_POINT ( 'NONE',  ( 1.670502159040608170, 2.215024970770036017, -0.1695594764349258321 ) ) ;
#214000 = CARTESIAN_POINT ( 'NONE',  ( 0.4047333657465709278, -2.105317319661216047, -0.2534319464195868843 ) ) ;
#214002 = CARTESIAN_POINT ( 'NONE',  ( 0.000000000000000000, 18.91999999999999815, 0.000000000000000000 ) ) ;
#214003 = CARTESIAN_POINT ( 'NONE',  ( -6.912678218121246942, 9.158153569265168770, 1.599625672291269396 ) ) ;
#214004 = CARTESIAN_POINT ( 'NONE',  ( 5.126954644262057492, 9.133197518281081173, 0.7998128361456462443 ) ) ;
#214005 = CARTESIAN_POINT ( 'NONE',  ( 3.367582429956605061, -0.3852447139683997657, 1.923494667983568718 ) ) ;
#214006 = CARTESIAN_POINT ( 'NONE',  ( 5.717788096661236885, 7.693838750903348789, 1.599625672291267398 ) ) ;
#214007 = CARTESIAN_POINT ( 'NONE',  ( -4.014638704412293535, 7.626288086010478473, 0.05010440672792437766 ) ) ;
#214008 = CARTESIAN_POINT ( 'NONE',  ( 3.521367211247359741, 5.131347717920458962, -1.599625672291262513 ) ) ;
#214009 = CARTESIAN_POINT ( 'NONE',  ( -4.977251789992602760, 8.820894498384422633, 0.000000000000000000 ) ) ;
#214010 = CARTESIAN_POINT ( 'NONE',  ( -6.480434237652138663, 8.583592582059388576, 1.443375672974078761 ) ) ;
#214012 = CARTESIAN_POINT ( 'NONE',  ( 1.846092968827160119, -1.388944967848893430, -1.602481653760478020 ) ) ;
#214011 = AXIS2_PLACEMENT_3D ( 'NONE', #30996, #159912, #160985 ) ;
#214013 = CARTESIAN_POINT ( 'NONE',  ( -6.394605727500880299, 7.489403432619674561, -1.199719254218452047 ) ) ;
#214014 = CARTESIAN_POINT ( 'NONE',  ( 6.092239754786219486, 0.9682357284593717806, -1.706234036142616928 ) ) ;
#214015 = CARTESIAN_POINT ( 'NONE',  ( 3.485389320157119997, 1.955090977548096687, -0.9225387301767663528 ) ) ;
#214016 = CARTESIAN_POINT ( 'NONE',  ( 3.298233973420101606, 1.449563003725433896, -1.135193286699177628 ) ) ;
#214017 = CARTESIAN_POINT ( 'NONE',  ( -4.099290701344459720, 7.507401141727952698, 0.5799236987427489609 ) ) ;
#214018 = CARTESIAN_POINT ( 'NONE',  ( -1.364683531250014514, -0.6572916663252459379, 0.7879004041258379498 ) ) ;
#214019 = CARTESIAN_POINT ( 'NONE',  ( 4.751753191611454596, 0.6700524488352653796, 1.606376638082593455 ) ) ;
#214020 = CARTESIAN_POINT ( 'NONE',  ( 11.52463353791759992, 9.719999999999998863, -3.346594096177641475 ) ) ;
#214021 = CARTESIAN_POINT ( 'NONE',  ( 3.877268743828266029, 6.506935386899531437, 1.082531754730558626 ) ) ;
#214022 = CARTESIAN_POINT ( 'NONE',  ( 2.430746436576446179, 2.096607243605509208, 0.5259719050795114148 ) ) ;
#214023 = CARTESIAN_POINT ( 'NONE',  ( 4.798203786142633653, -1.844427309015805649, 0.8145022673629878085 ) ) ;
#214024 = CARTESIAN_POINT ( 'NONE',  ( -10.10046125205659173, 10.88621900359527572, -0.7216878364870267237 ) ) ;
#214025 = TOROIDAL_SURFACE ( 'NONE', #99488, 2.400000000000000355, 0.1000000000000000056 ) ;
#214026 = CARTESIAN_POINT ( 'NONE',  ( 1.077287230265553397, -0.05381693868444264311, -2.161191418701657430 ) ) ;
#214027 = CARTESIAN_POINT ( 'NONE',  ( 2.284392081957301812, -1.932574240873608629, -0.3883164474826616419 ) ) ;
#214028 = CARTESIAN_POINT ( 'NONE',  ( 3.192849282005063127, 1.532776493767808113, 1.192484549457759613 ) ) ;
#214031 = ORIENTED_EDGE ( 'NONE', *, *, #154855, .T. ) ;
#214030 = CARTESIAN_POINT ( 'NONE',  ( -10.87339879486171590, 5.131770238416462959, 5.487091846871368084 ) ) ;
#214029 = CARTESIAN_POINT ( 'NONE',  ( -10.15469386651127515, 11.90985960142705657, 1.082531754730558626 ) ) ;
#214032 = CARTESIAN_POINT ( 'NONE',  ( -6.583366107887490770, 9.838288338247510367, 1.199719254218452935 ) ) ;
#214033 = CARTESIAN_POINT ( 'NONE',  ( 4.248501033035879004, 6.049946853332221153, -1.599625672291273171 ) ) ;
#214035 = ORIENTED_EDGE ( 'NONE', *, *, #33740, .T. ) ;
#214034 = CARTESIAN_POINT ( 'NONE',  ( -5.498713818794216834, 8.572860667638675380, -1.199719254218452047 ) ) ;
#214036 = CARTESIAN_POINT ( 'NONE',  ( -9.775065565328603157, 11.46695991671396087, -1.082531754730537976 ) ) ;
#214037 = CARTESIAN_POINT ( 'NONE',  ( 1.431021430919703574, 2.126993092707793132, 0.5877070120439558121 ) ) ;
#214038 = CARTESIAN_POINT ( 'NONE',  ( 1.642778471875001811, -3.842708332855375275, 2.845375778867859751 ) ) ;
#214039 = CARTESIAN_POINT ( 'NONE',  ( 5.313317156408340125, -1.655227327604656740, -1.052681782574490743 ) ) ;
#214040 = CARTESIAN_POINT ( 'NONE',  ( 3.468056730359007744, -1.039945921192251266, 1.844253657775334121 ) ) ;
#214041 = CARTESIAN_POINT ( 'NONE',  ( -1.500000000000013101, 2.452083334016154748, 0.8660254037844403729 ) ) ;
#214042 = CARTESIAN_POINT ( 'NONE',  ( 0.1747926744264677590, 6.948552888299643904, -2.450368216405907962 ) ) ;
#214043 = CARTESIAN_POINT ( 'NONE',  ( 4.312339554033173705, 1.684294245562456993, 0.7440144950455057637 ) ) ;
#214044 = ORIENTED_EDGE ( 'NONE', *, *, #196360, .T. ) ;
#214045 = CARTESIAN_POINT ( 'NONE',  ( -9.481229494658258261, 9.955855920056455588, -0.7998128361456291469 ) ) ;
#214046 = CARTESIAN_POINT ( 'NONE',  ( 0.3999999999999442335, 3.248764396332271875, 0.4641653677812440093 ) ) ;
#214047 = CARTESIAN_POINT ( 'NONE',  ( 5.203433420164765622, 1.869144303625443371, -1.001675624404389620 ) ) ;
#214048 = CARTESIAN_POINT ( 'NONE',  ( 6.257251587906815793, 7.258880593101466161, 1.199719254218462483 ) ) ;
#214049 = ADVANCED_FACE ( 'NONE', ( #45659 ), #172781, .F. ) ;
#214050 = CARTESIAN_POINT ( 'NONE',  ( 6.274695623702050362, -1.955332461540583600, -0.6509123137334557052 ) ) ;
#214053 = CARTESIAN_POINT ( 'NONE',  ( 3.614658571667620279, -0.1319153736358945894, 1.836568937333193485 ) ) ;
#214052 = CARTESIAN_POINT ( 'NONE',  ( 1.328301213181204421, -1.184495032981685014, 1.435421900094263403 ) ) ;
#214051 = DIRECTION ( 'NONE',  ( 1.000000000000000000, -5.578564026256504688E-16, -0.000000000000000000 ) ) ;
#214054 = CARTESIAN_POINT ( 'NONE',  ( 7.958799866421889746, 9.244020251369077457, -1.199719254218441611 ) ) ;
#214055 = CARTESIAN_POINT ( 'NONE',  ( -10.85277107007939001, 3.956598013261175772, 3.932872935640539414 ) ) ;
#214056 = CARTESIAN_POINT ( 'NONE',  ( -6.084577077482911101, 10.32070003369722144, 0.000000000000000000 ) ) ;
#214057 = CARTESIAN_POINT ( 'NONE',  ( 0.3282377607281103393, 2.136164550367433357, 1.224999999999969225 ) ) ;
#214058 = CARTESIAN_POINT ( 'NONE',  ( 3.809358915828209735, 1.892446193107431451, 1.135094405146239049 ) ) ;
#214059 = CARTESIAN_POINT ( 'NONE',  ( 4.833442251172010984, -2.071103420340114187, 0.9108926349224757413 ) ) ;
#214060 = CARTESIAN_POINT ( 'NONE',  ( -5.721177635286839092, 9.618531641235897212, 0.7216878364870458196 ) ) ;
#214061 = CARTESIAN_POINT ( 'NONE',  ( 4.394648900434598104, -1.758782010937329110, -0.4337233627825891613 ) ) ;
#214062 = CARTESIAN_POINT ( 'NONE',  ( 5.876186789644119557, -1.907177742178717716, -0.1804351137127818694 ) ) ;
#214063 = CARTESIAN_POINT ( 'NONE',  ( -1.001543065824772872E-14, 4.884375000341420581, 1.575800808251672791 ) ) ;
#214064 = CARTESIAN_POINT ( 'NONE',  ( 5.700035372616791385, -1.870836310086241294, 0.001406584917262864625 ) ) ;
#214066 = ADVANCED_FACE ( 'NONE', ( #145320 ), #196554, .T. ) ;
#214065 = AXIS2_PLACEMENT_3D ( 'NONE', #74276, #138215, #22278 ) ;
#214067 = CARTESIAN_POINT ( 'NONE',  ( 5.564867526603252124, 1.409050971242819417, -1.215897700512589052 ) ) ;
#214068 = DIRECTION ( 'NONE',  ( 0.000000000000000000, 0.000000000000000000, -1.000000000000000000 ) ) ;
#214069 = CARTESIAN_POINT ( 'NONE',  ( 6.034039731144309471, 0.8686908000094315518, -1.541921269980907949 ) ) ;
#214070 = CARTESIAN_POINT ( 'NONE',  ( 1.007046422456716384, -0.04465021774549028655, 2.016188868504041665 ) ) ;
#214072 = CARTESIAN_POINT ( 'NONE',  ( 2.912826151168836031, 1.525034000978764626, -1.452760968584436707 ) ) ;
#214071 = CARTESIAN_POINT ( 'NONE',  ( -2.914639836813632812, 6.344237543017112735, 0.7216878364870317197 ) ) ;
#214073 = CARTESIAN_POINT ( 'NONE',  ( 9.398826802771546696, 11.98838390803207865, -1.599625672291262513 ) ) ;
#214075 = CARTESIAN_POINT ( 'NONE',  ( -9.501566725078754772, 9.979582688880366703, -0.7998128361456291469 ) ) ;
#214074 = PLANE ( 'NONE',  #76812 ) ;
#214076 = PLANE ( 'NONE',  #79007 ) ;
#214077 = CARTESIAN_POINT ( 'NONE',  ( 1.687766420876281037, 1.931502627210328837, -0.5905180581586618738 ) ) ;
#214078 = CARTESIAN_POINT ( 'NONE',  ( -1.402160292154681736E-14, 1.946875000341422579, -1.575800808251660134 ) ) ;
#214079 = CARTESIAN_POINT ( 'NONE',  ( 5.169736645512481132, 4.925780929386339935, 0.7998128361456341429 ) ) ;
#214080 = CARTESIAN_POINT ( 'NONE',  ( 2.811983876933337179, -2.138515761559431461, 0.3140893029918228607 ) ) ;
#214081 = CARTESIAN_POINT ( 'NONE',  ( 6.890000000000039648, 4.701345932300413644, 2.282685536056531461 ) ) ;
#214083 =( NAMED_UNIT ( * ) PLANE_ANGLE_UNIT ( ) SI_UNIT ( $, .RADIAN. ) );
#214082 = CARTESIAN_POINT ( 'NONE',  ( 3.627688620108284745, 6.389997935838436227, 1.199719254218452047 ) ) ;
#214084 = CARTESIAN_POINT ( 'NONE',  ( 9.531018800282605952, 11.18223869082697597, 1.082531754730548412 ) ) ;
#214085 = CARTESIAN_POINT ( 'NONE',  ( -7.905503641038438722, -6.808400134080595301, 7.455003611050304180 ) ) ;
#214086 = CARTESIAN_POINT ( 'NONE',  ( -6.670248388243482651, 9.765411638717282017, 1.082531754730548412 ) ) ;
#214087 = CARTESIAN_POINT ( 'NONE',  ( -1.364683531250014514, 0.9885416670080898749, -0.7879004041258289570 ) ) ;
#214088 = CARTESIAN_POINT ( 'NONE',  ( 1.505704256594592838, -2.174480876681058827, 0.2726767719730335826 ) ) ;
#214089 = CARTESIAN_POINT ( 'NONE',  ( 0.5050423914800099556, 7.726475908227712353, 1.936073478083413235 ) ) ;
#214090 = CARTESIAN_POINT ( 'NONE',  ( 1.745381597357411385, -1.910777759476259163, 1.211296049258607788 ) ) ;
#214091 = CARTESIAN_POINT ( 'NONE',  ( -9.182950115157607840, 9.607863310639020327, 0.7998128361456462443 ) ) ;
#214092 = CARTESIAN_POINT ( 'NONE',  ( -5.083944415000202888, 5.033616027029415463, 0.7216878364870317197 ) ) ;
#214094 = AXIS2_PLACEMENT_3D ( 'NONE', #34274, #18005, #101412 ) ;
#214093 = CARTESIAN_POINT ( 'NONE',  ( 0.6823417656249917140, 3.405208333674754506, 1.181850606188765695 ) ) ;
#214095 = CARTESIAN_POINT ( 'NONE',  ( 4.600487305768355739, 8.366733224642864286, -0.1591645125929436189 ) ) ;
#214096 = CARTESIAN_POINT ( 'NONE',  ( -0.7500000000000006661, 10.70833333333333393, -1.299038105676657340 ) ) ;
#214097 = CARTESIAN_POINT ( 'NONE',  ( 2.905190055078214595, 6.611415174225076186, 0.7998128361456271485 ) ) ;
#214098 = CARTESIAN_POINT ( 'NONE',  ( 2.952157954411178675, 0.5926004979403748374, 1.667723606733088060 ) ) ;
#214099 = CARTESIAN_POINT ( 'NONE',  ( 0.09494852110062798611, -0.4603312545960658864, -2.062269868324863253 ) ) ;
#214100 = CARTESIAN_POINT ( 'NONE',  ( -0.6823417656250039265, 9.067708333674733723, -1.181850606188755259 ) ) ;
#214101 = VERTEX_POINT ( 'NONE', #153800 ) ;
#214102 = CARTESIAN_POINT ( 'NONE',  ( -7.110325215724114578, 7.260077271291732082, 0.000000000000000000 ) ) ;
#214103 = CARTESIAN_POINT ( 'NONE',  ( 4.974232547167513729, -2.001514726140873890, -0.2440111082952014510 ) ) ;
#214105 = EDGE_LOOP ( 'NONE', ( #18945, #88990, #25941 ) ) ;
#214104 = CARTESIAN_POINT ( 'NONE',  ( 4.869312882171149326, -1.534379415642408651, -0.9627496050425389251 ) ) ;
#214106 = VECTOR ( 'NONE', #135842, 1000.000000000000000 ) ;
#214107 = CARTESIAN_POINT ( 'NONE',  ( 2.834663617355744680, 0.2272019944037397543, 1.856728029318695627 ) ) ;
#214108 = CARTESIAN_POINT ( 'NONE',  ( 3.713788242813487184, 0.5077267127921447631, -2.006887321594638784 ) ) ;
#214109 = CARTESIAN_POINT ( 'NONE',  ( -7.553300976144787349, 8.945177572657957654, -1.082531754730549967 ) ) ;
#214110 = CARTESIAN_POINT ( 'NONE',  ( 2.531394148431935776, -0.1834752923718513118, 1.903540536635806912 ) ) ;
#214111 = CARTESIAN_POINT ( 'NONE',  ( -0.5151702941667783975, 3.543307664981999228, 0.3998358608512623813 ) ) ;
#214112 = CARTESIAN_POINT ( 'NONE',  ( -9.645452764996941042, 5.068254855380425639, -6.574395040668256307 ) ) ;
#214113 = CARTESIAN_POINT ( 'NONE',  ( -11.55950211276791428, 11.37999999999998302, 3.221476510067114329 ) ) ;
#214114 = B_SPLINE_CURVE_WITH_KNOTS ( 'NONE', 3,
 ( #113879, #49862, #10, #1080 ),
 .UNSPECIFIED., .F., .F.,
 ( 4, 4 ),
 ( 0.000000000000000000, 0.0002908967400263839909 ),
 .UNSPECIFIED. ) ;
#214115 = CARTESIAN_POINT ( 'NONE',  ( -1.364683531249997417, 4.821875000341417916, 1.214306433183764966E-14 ) ) ;
#214116 = CARTESIAN_POINT ( 'NONE',  ( 0.8438408207818194340, -1.215224102361469161, -1.476598726422105656 ) ) ;
#214117 = CARTESIAN_POINT ( 'NONE',  ( 3.332423539472821439, -1.170687260143790320, 1.574129132985650825 ) ) ;
#214118 = EDGE_CURVE ( 'NONE', #56290, #213437, #181358, .T. ) ;
#214119 = CARTESIAN_POINT ( 'NONE',  ( -4.176793841461789114, 7.030620694084159794, -1.199719254218455378 ) ) ;
#214120 = CARTESIAN_POINT ( 'NONE',  ( 9.585778300061798873, 11.14216175728232550, -1.199719254218440723 ) ) ;
#214121 = CARTESIAN_POINT ( 'NONE',  ( 6.468046296993485988, 1.011472520757991767, 1.691939633080985272 ) ) ;
#214122 = CARTESIAN_POINT ( 'NONE',  ( -1.201851678989727383E-14, 2.071875000341422801, 1.575800808251672791 ) ) ;
#214123 = CARTESIAN_POINT ( 'NONE',  ( 1.810793108869549917, -0.5408357282137785660, -1.939109541719201912 ) ) ;
#214125 = CARTESIAN_POINT ( 'NONE',  ( 2.478245404118933237, -2.111759443744887221, -0.1527427581556138059 ) ) ;
#214124 = CARTESIAN_POINT ( 'NONE',  ( -7.876924059859742755, 8.292092279365579799, 1.040834085586084257E-14 ) ) ;
#214126 = CARTESIAN_POINT ( 'NONE',  ( 8.900805598352070191, 12.81158145916116453, -8.049589252430559227 ) ) ;
#214127 = CARTESIAN_POINT ( 'NONE',  ( 3.631357695093720750, 0.05367941694835526995, -2.069842578854002468 ) ) ;
#214128 = B_SPLINE_CURVE_WITH_KNOTS ( 'NONE', 3,
 ( #83247, #197010, #131018, #100578, #166651, #149332 ),
 .UNSPECIFIED., .F., .F.,
 ( 4, 2, 4 ),
 ( 2.354250779258689971E-08, 0.0004384930979466261560, 0.0008769626533854597882 ),
 .UNSPECIFIED. ) ;
#214129 = CARTESIAN_POINT ( 'NONE',  ( 3.901714345682657292, 7.774026846596938434, 0.7998128361456271485 ) ) ;
#214131 = CARTESIAN_POINT ( 'NONE',  ( 4.704842999142070603, 5.447737239542574272, -1.199719254218452047 ) ) ;
#214130 = CARTESIAN_POINT ( 'NONE',  ( 6.404249610866886044, 1.549990571320001731, -1.403138301853884773 ) ) ;
#214133 = ORIENTED_EDGE ( 'NONE', *, *, #17125, .F. ) ;
#214132 = CARTESIAN_POINT ( 'NONE',  ( 4.190329584092522097, -1.805708503706305423, -0.2678305112727846771 ) ) ;
#214134 = CARTESIAN_POINT ( 'NONE',  ( 9.541187415715040032, 12.15447128979948310, -1.599625672291262513 ) ) ;
#214135 = FACE_OUTER_BOUND ( 'NONE', #163325, .T. ) ;
#214136 = CARTESIAN_POINT ( 'NONE',  ( 8.892182451728965376, 12.91678122746358248, -7.588089516412551028 ) ) ;
#214137 = CARTESIAN_POINT ( 'NONE',  ( 5.579209114504255496, -0.04897750150410771358, -2.206396493298476980 ) ) ;
#214138 = CARTESIAN_POINT ( 'NONE',  ( -0.6823417656250039265, 10.13020833367472839, -1.181850606188755259 ) ) ;
#214139 = EDGE_CURVE ( 'NONE', #130050, #176746, #155448, .T. ) ;
#214140 = EDGE_LOOP ( 'NONE', ( #4148, #50881, #46769, #118131 ) ) ;
#214141 = CARTESIAN_POINT ( 'NONE',  ( 3.475170734053119048, -1.687717282722025924, -0.8990902037325496643 ) ) ;
#214142 = CARTESIAN_POINT ( 'NONE',  ( -8.448702279610222021, 13.00856975952063088, 1.040834085586084257E-14 ) ) ;
#214143 = CARTESIAN_POINT ( 'NONE',  ( 5.608269097547198712, 9.694731047113750222, -0.7998128361456281477 ) ) ;
#214144 = CARTESIAN_POINT ( 'NONE',  ( -0.6801582343750125492, 2.213541667008059211, 1.178068619123818994 ) ) ;
#214145 = CARTESIAN_POINT ( 'NONE',  ( 3.511198595814921219, 7.040222761851976152, 0.7216878364870317197 ) ) ;
#214146 = CARTESIAN_POINT ( 'NONE',  ( 2.000000000000003553, 6.400000000000022560, 2.449293598294762621E-16 ) ) ;
#214147 = CARTESIAN_POINT ( 'NONE',  ( 8.742474708574045295, 13.54844359601399972, -8.153352885485730894 ) ) ;
#214148 = CARTESIAN_POINT ( 'NONE',  ( 0.1515692981730529243, 0.7036590017722235135, 1.701685288394996665 ) ) ;
#214149 = ORIENTED_EDGE ( 'NONE', *, *, #102547, .F. ) ;
#214150 = CARTESIAN_POINT ( 'NONE',  ( -7.075376061485238566, 9.347967719856493218, 1.599625672291269396 ) ) ;
#214151 = CARTESIAN_POINT ( 'NONE',  ( 4.516781199771729760, 1.709404882366181377, 0.7599583452636837766 ) ) ;
#214152 = CARTESIAN_POINT ( 'NONE',  ( 6.994027139803230320, 9.253060644560830994, -1.599625672291267398 ) ) ;
#214153 = CARTESIAN_POINT ( 'NONE',  ( -1.499999999999997113, 7.438721522839124134, -4.195160983902616714 ) ) ;
#214154 = CARTESIAN_POINT ( 'NONE',  ( -7.714226216495749355, 8.102278128774251797, 1.040834085586084257E-14 ) ) ;
#214155 = CARTESIAN_POINT ( 'NONE',  ( 5.229694566569264680, 7.124396299129368337, 1.599625672291267398 ) ) ;
#214156 = CARTESIAN_POINT ( 'NONE',  ( 1.428490153906246007, -1.253617920133040853, 1.518890472526812419 ) ) ;
#214157 = CARTESIAN_POINT ( 'NONE',  ( 2.407827563459669307, -1.163288551851604513, -1.646826728940099738 ) ) ;
#214158 = CARTESIAN_POINT ( 'NONE',  ( -7.472515219426274946, 11.86968485597268064, 0.000000000000000000 ) ) ;
#214159 = CARTESIAN_POINT ( 'NONE',  ( 5.180097208873055692, 8.201141289397330780, -1.199719254218450271 ) ) ;
#214161 = EDGE_CURVE ( 'NONE', #205391, #41837, #199321, .T. ) ;
#214160 = CARTESIAN_POINT ( 'NONE',  ( 6.773376348128858915, -7.215568602681178945, 6.661184042391304239 ) ) ;
#214162 = CARTESIAN_POINT ( 'NONE',  ( 2.730644157659181559, 0.2691629481662433099, 2.174792594416566249 ) ) ;
#214163 = CARTESIAN_POINT ( 'NONE',  ( 2.335486742378070968, 0.1025264918674481801, -0.4876558207452422189 ) ) ;
#214164 = CARTESIAN_POINT ( 'NONE',  ( -7.947050595904583403, 12.42330946186405249, 0.7998128361456481317 ) ) ;
#214165 = CARTESIAN_POINT ( 'NONE',  ( -0.6823417656250212460, 3.051041667008084879, 1.181850606188767472 ) ) ;
#214166 = DIRECTION ( 'NONE',  ( 0.7613463080411785322, -0.000000000000000000, 0.6483454320283801309 ) ) ;
#214167 = EDGE_CURVE ( 'NONE', #197916, #63041, #51709, .T. ) ;
#214168 = CARTESIAN_POINT ( 'NONE',  ( 4.692530564105613422, 7.528350520548263702, -1.082531754730548412 ) ) ;
#214169 = CARTESIAN_POINT ( 'NONE',  ( 8.718056468787178659, 10.12981962079525289, 1.199719254218462483 ) ) ;
#214170 = CARTESIAN_POINT ( 'NONE',  ( 3.216308754939877446, 4.775446185561722956, -1.599625672291262513 ) ) ;
#214171 = CARTESIAN_POINT ( 'NONE',  ( 5.397554552016204710, 9.311247720745345902, 0.7216878364870317197 ) ) ;
#214172 = VERTEX_POINT ( 'NONE', #134385 ) ;
#214174 = CARTESIAN_POINT ( 'NONE',  ( 1.858066033337543832, 0.7684160352657551929, -1.860855044080988785 ) ) ;
#214173 = CARTESIAN_POINT ( 'NONE',  ( 4.862772069579198941, 0.1752732939881325724, -1.832877676746891726 ) ) ;
#214175 = CARTESIAN_POINT ( 'NONE',  ( 3.673487740190139572, -0.9280425899400122081, -2.102842487114229275 ) ) ;
#214177 = CARTESIAN_POINT ( 'NONE',  ( 1.393147051786493673, -1.685373162331062602, 0.7893452609444310264 ) ) ;
#214176 = CARTESIAN_POINT ( 'NONE',  ( -0.7500000000000179856, 10.04166666666667140, 1.299038105676658228 ) ) ;
#214178 = CARTESIAN_POINT ( 'NONE',  ( -1.642778471874998480, -3.901041666188709289, 2.845375778867863303 ) ) ;
#214179 = CARTESIAN_POINT ( 'NONE',  ( 6.082274476537278041, 0.9889857280602430967, 1.636697341158253272 ) ) ;
#214180 = CARTESIAN_POINT ( 'NONE',  ( -7.648771216403934758, 12.07531685244661723, -0.7998128361456291469 ) ) ;
#214181 = CARTESIAN_POINT ( 'NONE',  ( -6.048345925472225382, 8.149765894507963182, 1.443375672974058777 ) ) ;
#214183 = CARTESIAN_POINT ( 'NONE',  ( 2.096370420935515178, -0.4963513585865795275, -1.803540123670114736 ) ) ;
#214182 = CARTESIAN_POINT ( 'NONE',  ( 3.597287555019304861, -0.6049611382589085151, 2.001324503170316849 ) ) ;
#214184 = CARTESIAN_POINT ( 'NONE',  ( 8.107412671292047790, 8.560995659369956101, 0.7216878364870458196 ) ) ;
#214185 = CARTESIAN_POINT ( 'NONE',  ( -1.001543065824772872E-14, 5.134375000341421469, 1.575800808251672791 ) ) ;
#214186 = CARTESIAN_POINT ( 'NONE',  ( 6.022987620897008121, -1.731432113864934674, 0.6267441317700100933 ) ) ;
#214187 = CIRCLE ( 'NONE', #120944, 12.00000000000000178 ) ;
#214188 = CARTESIAN_POINT ( 'NONE',  ( 3.171717870593107058, 5.787755718078879674, -1.199719254218446718 ) ) ;
#214189 = CARTESIAN_POINT ( 'NONE',  ( 1.224999999999984990, 1.104166666666725360, 0.7072540797572737237 ) ) ;
#214190 = CARTESIAN_POINT ( 'NONE',  ( 4.811038506879902421, 1.503007855926122405, 0.8461308117306536314 ) ) ;
#214191 = CARTESIAN_POINT ( 'NONE',  ( -5.865874016206865882, 9.995270118883347266, 0.000000000000000000 ) ) ;
#214192 = CARTESIAN_POINT ( 'NONE',  ( 0.3868564640647629282, -0.5820622975930835885, -1.633661194748408541 ) ) ;
#214193 = LINE ( 'NONE', #96252, #92433 ) ;
#214194 = CARTESIAN_POINT ( 'NONE',  ( 1.907519672996849103, 3.236073672982398008, 0.4612874649729346022 ) ) ;
#214195 = CARTESIAN_POINT ( 'NONE',  ( 4.399414683135016269, -1.891862197681973834, 1.064912953861403944 ) ) ;
#214196 = CARTESIAN_POINT ( 'NONE',  ( 3.035583632137848653, -1.226507576337819483, -1.352503160878690380 ) ) ;
#214197 = CARTESIAN_POINT ( 'NONE',  ( 0.6023038706522118035, 1.956103482322549825, 0.1501044349687257751 ) ) ;
#214198 = CARTESIAN_POINT ( 'NONE',  ( 5.559793223943660934, 1.263291928365728012, 1.699014672817029892 ) ) ;
#214200 = CARTESIAN_POINT ( 'NONE',  ( -1.364683531250010295, 3.842708333674751398, 0.7879004041258379498 ) ) ;
#214199 = CARTESIAN_POINT ( 'NONE',  ( 6.040627043210095692, -1.938779113641406759, 1.222911669862235096 ) ) ;
#214201 = CARTESIAN_POINT ( 'NONE',  ( 5.300874872818884143, 5.286701561151147644, 0.7216878364870010776 ) ) ;
#214202 = CARTESIAN_POINT ( 'NONE',  ( 7.553864141108259211, 11.96459193126834464, 1.040834085586084257E-14 ) ) ;
#214203 = CARTESIAN_POINT ( 'NONE',  ( 1.928540351845555056, -1.002238520345886785, -1.868699319572619366 ) ) ;
#214204 = CARTESIAN_POINT ( 'NONE',  ( -3.307826292054310890, 5.842585859829892314, -1.082531754730549967 ) ) ;
#214205 = CIRCLE ( 'NONE', #17253, 2.000000000000006217 ) ;
#214206 = CARTESIAN_POINT ( 'NONE',  ( 5.598800414281360993, 5.751655211587324956, 0.6575274206139459787 ) ) ;
#214207 = CARTESIAN_POINT ( 'NONE',  ( -3.701012746406287413, 6.301303389907177532, 1.082531754730560403 ) ) ;
#214208 =( BOUNDED_CURVE ( )  B_SPLINE_CURVE ( 2, ( #94962, #163151, #50448, #48344, #14735, #114455, #130713 ),
 .UNSPECIFIED., .F., .T. ) 
 B_SPLINE_CURVE_WITH_KNOTS ( ( 3, 2, 2, 3 ),
 ( 0.2250000000000001998, 0.2291666666666669350, 0.2333333333333336701, 0.2375000000000004052 ),
 .UNSPECIFIED. ) 
 CURVE ( )  GEOMETRIC_REPRESENTATION_ITEM ( )  RATIONAL_B_SPLINE_CURVE ( ( 0.9999999999999937828, 0.8660254037844449249, 1.000000000000000000, 0.8660254037844387076, 1.000000000000000000, 0.8660254037844252739, 1.000000000000013323 ) ) 
 REPRESENTATION_ITEM ( '' )  );
#214209 = CARTESIAN_POINT ( 'NONE',  ( 6.719587830005472995, 0.3798626643731088937, -2.137457590422507714 ) ) ;
#214211 = CARTESIAN_POINT ( 'NONE',  ( 1.499999999999993117, 12.88541666734946389, 0.8660254037844409281 ) ) ;
#214210 = CARTESIAN_POINT ( 'NONE',  ( 6.883263157960367806, 6.035304072343574688, 2.648703854151325032 ) ) ;
#214213 = ORIENTED_EDGE ( 'NONE', *, *, #101161, .T. ) ;
#214212 = CARTESIAN_POINT ( 'NONE',  ( 1.858359290357750160, 0.8465214129982703284, -2.053864850685551691 ) ) ;
#214214 = CARTESIAN_POINT ( 'NONE',  ( 0.001177798100650446610, -2.252613640939280515, 0.4573402144308849615 ) ) ;
#214216 = CARTESIAN_POINT ( 'NONE',  ( 4.170800697546906299, 1.462118435030785646, -1.455038044888419702 ) ) ;
#214215 = CARTESIAN_POINT ( 'NONE',  ( 4.172158584703322681, 5.890604320285754980, -1.599625672291256295 ) ) ;
#214218 = CARTESIAN_POINT ( 'NONE',  ( 1.737499999999999378, -3.616666666666667140, -3.009438278150925683 ) ) ;
#214217 = CARTESIAN_POINT ( 'NONE',  ( 5.554000203453580475, 6.508696987897830688, -1.199719254218452047 ) ) ;
#214219 = CARTESIAN_POINT ( 'NONE',  ( 6.561219994370630637, 6.619454513046008515, 0.000000000000000000 ) ) ;
#214220 = CARTESIAN_POINT ( 'NONE',  ( 2.960184520039609524, -4.197067588314596698, -1.425549731837409961 ) ) ;
#214221 = FACE_OUTER_BOUND ( 'NONE', #6497, .T. ) ;
#214222 = CARTESIAN_POINT ( 'NONE',  ( 4.546344060013487898, -1.475942220874026489, 1.100600019281534836 ) ) ;
#214224 = EDGE_LOOP ( 'NONE', ( #64246, #64342, #111294, #158789 ) ) ;
#214223 = CARTESIAN_POINT ( 'NONE',  ( 4.761938266897790761, 6.578680616179308771, 1.599625672291267398 ) ) ;
#214225 = CARTESIAN_POINT ( 'NONE',  ( 1.623609269016149437, -0.9540678014761799774, -1.436642212298586907 ) ) ;
#214226 = CARTESIAN_POINT ( 'NONE',  ( -0.08279552664090458758, -1.841734517378278424, 0.8216794407479923734 ) ) ;
#214227 = CARTESIAN_POINT ( 'NONE',  ( 2.198211363809216667, 2.055062875077425577, 1.030007645627160517 ) ) ;
#214228 = CARTESIAN_POINT ( 'NONE',  ( -1.201851678989727383E-14, 3.384375000341421469, 1.575800808251672791 ) ) ;
#214229 = CARTESIAN_POINT ( 'NONE',  ( 1.546537457781042235, 2.259796958156198077, 0.1114739384607699862 ) ) ;
#214230 = CARTESIAN_POINT ( 'NONE',  ( 3.844438321715905715, 2.095922912919225389, 0.2063985846082766473 ) ) ;
#214231 = CARTESIAN_POINT ( 'NONE',  ( -4.604929450496978660, 5.401447776115099408, -1.199719254218453823 ) ) ;
#214232 = CARTESIAN_POINT ( 'NONE',  ( 2.635733503900684838, 0.8381847041133619891, -1.558674532600109686 ) ) ;
#214233 = CARTESIAN_POINT ( 'NONE',  ( 5.587931867126699537, 9.671004278289832001, -0.7998128361456291469 ) ) ;
#214235 = EDGE_CURVE ( 'NONE', #202848, #129569, #10103, .T. ) ;
#214234 = CARTESIAN_POINT ( 'NONE',  ( 5.356880090730872013, 6.382686539675070492, 1.082531754730549078 ) ) ;
#214236 = CARTESIAN_POINT ( 'NONE',  ( -6.413170354464012846, 7.440785820751486312, 1.199719254218450271 ) ) ;
#214237 = CARTESIAN_POINT ( 'NONE',  ( 1.499999999999987121, 1.795833333333355819, -0.8660254037844253849 ) ) ;
#214238 = CARTESIAN_POINT ( 'NONE',  ( 4.711300293261502681, 1.846222065370630050, -1.235088439349934841 ) ) ;
#214239 = CARTESIAN_POINT ( 'NONE',  ( 3.328257738700185264, 2.138080787187321086, 0.4799892483983853042 ) ) ;
#214240 = CARTESIAN_POINT ( 'NONE',  ( -4.388035272317281077, 8.271124917678806199, 0.7998128361456481317 ) ) ;
#214241 = CARTESIAN_POINT ( 'NONE',  ( -4.930325137224961907, 5.781076077297750970, -1.199719254218453823 ) ) ;
#214242 = CARTESIAN_POINT ( 'NONE',  ( 6.551439628692993900, -1.894445571042557619, 0.9528467149547341641 ) ) ;
#214243 = CARTESIAN_POINT ( 'NONE',  ( -1.364683531250010295, 3.780208333674750953, 0.7879004041258379498 ) ) ;
#214244 = CARTESIAN_POINT ( 'NONE',  ( 6.610000000000006537, 2.052567036419289614, 2.306714106643445561 ) ) ;
#214245 = CARTESIAN_POINT ( 'NONE',  ( -5.436456409399874623, 5.444880020495701523, 0.000000000000000000 ) ) ;
#214246 = CARTESIAN_POINT ( 'NONE',  ( 5.449516625918088053, -1.916229881892789866, 0.9086369058012438993 ) ) ;
#214247 = CARTESIAN_POINT ( 'NONE',  ( -7.607533591043815768, 8.048079742405473525, 0.000000000000000000 ) ) ;
#214248 = ORIENTED_EDGE ( 'NONE', *, *, #177361, .F. ) ;
#214250 = CARTESIAN_POINT ( 'NONE',  ( 6.297764839082774735, -0.7330946318361495351, 2.033732118066629457 ) ) ;
#214249 = CARTESIAN_POINT ( 'NONE',  ( -4.312902262922974295, 8.045820050136510915, 0.7216878364870338292 ) ) ;
#214251 = CARTESIAN_POINT ( 'NONE',  ( 5.867981556616276073, 5.740399992340775803, -0.7998128361456281477 ) ) ;
#214252 = CARTESIAN_POINT ( 'NONE',  ( 6.614805131849967879, -0.1256686391097518729, 1.812046779126045726 ) ) ;
#214253 = CARTESIAN_POINT ( 'NONE',  ( 3.602337597214539753E-15, 1.000000000682806034, -1.225000000000015410 ) ) ;
#214254 = CARTESIAN_POINT ( 'NONE',  ( -1.201851678989727383E-14, 3.009375000341419248, -1.575800808251660134 ) ) ;
#214255 = CARTESIAN_POINT ( 'NONE',  ( 1.399541807966601104, -0.6259456572170263300, -1.624154832779246993 ) ) ;
#214256 = CARTESIAN_POINT ( 'NONE',  ( 4.546061579283848353, 4.198160018786257552, -0.7998128361456211532 ) ) ;
#214257 = CARTESIAN_POINT ( 'NONE',  ( 0.2386218892466463737, -1.902018210125755004, -0.4804332253167050149 ) ) ;
#214258 = CARTESIAN_POINT ( 'NONE',  ( -0.6823417656250246877, 0.6135416670080897639, 1.181850606188755259 ) ) ;
#214259 = CARTESIAN_POINT ( 'NONE',  ( -4.294587207893853176, 7.385457912387431101, -1.052126661723006285 ) ) ;
#214260 = CARTESIAN_POINT ( 'NONE',  ( 4.838837662799537753, 0.3661284547709364734, 2.130314178654398205 ) ) ;
#214261 = CARTESIAN_POINT ( 'NONE',  ( -2.948008335967658322, 5.526761261015804116, 1.199719254218462483 ) ) ;
#214262 = CARTESIAN_POINT ( 'NONE',  ( -5.707619481228817904, 8.642344580533519505, -1.082531754730537976 ) ) ;
#214263 = CARTESIAN_POINT ( 'NONE',  ( 4.663041391408608405, -1.929494027986548454, -0.9748474430888448561 ) ) ;
#214265 = ORIENTED_EDGE ( 'NONE', *, *, #157150, .T. ) ;
#214264 = CARTESIAN_POINT ( 'NONE',  ( -6.708500942254057897E-15, -5.907420853759271395, -11.00029519899099029 ) ) ;
#214266 = CARTESIAN_POINT ( 'NONE',  ( 0.6823417656249899377, 3.092708333674754062, 1.181850606188765695 ) ) ;
#214267 = CARTESIAN_POINT ( 'NONE',  ( 5.993430986175369846, 1.491191765471042041, 1.289477300995988118 ) ) ;
#214268 = CARTESIAN_POINT ( 'NONE',  ( 5.483642203991152542, 1.602890455293109584, 0.6615300989148454880 ) ) ;
#214270 = CARTESIAN_POINT ( 'NONE',  ( 2.402122600552298870, -0.8417629408748151798, -2.023652355447076001 ) ) ;
#214269 = CARTESIAN_POINT ( 'NONE',  ( 1.360316468749977581, -0.2135416663252950598, -0.7853790794159261068 ) ) ;
#214271 = CARTESIAN_POINT ( 'NONE',  ( 3.663348518144835086, -2.033753252616496532, -1.090341736564947484 ) ) ;
#214272 = CARTESIAN_POINT ( 'NONE',  ( 4.534483719690214798, 2.020231433191475467, 0.4058933888440272031 ) ) ;
#214273 = CARTESIAN_POINT ( 'NONE',  ( 0.6209105903263291149, -1.844282116485985501, 0.6082893332694323529 ) ) ;
#214274 = CARTESIAN_POINT ( 'NONE',  ( -6.168596704093453731, 10.14052055484361325, 0.7216878364870458196 ) ) ;
#214275 = CARTESIAN_POINT ( 'NONE',  ( -3.332271893908731464, 7.109677319527304640, -0.7998128361456481317 ) ) ;
#214276 = CARTESIAN_POINT ( 'NONE',  ( -5.602498012743508227, 5.726462300312828546, -0.1687859242097844992 ) ) ;
#214277 = CARTESIAN_POINT ( 'NONE',  ( 3.603867943843573673, 1.538443694073919898, 1.459757404076333698 ) ) ;
#214278 = CARTESIAN_POINT ( 'NONE',  ( 1.678041975860264342E-16, 13.49999999999999822, 1.240450515248286534 ) ) ;
#214279 = CARTESIAN_POINT ( 'NONE',  ( 1.090470458312575053, -0.4872005951904456733, 1.956561897242928172 ) ) ;
#214280 = CARTESIAN_POINT ( 'NONE',  ( -6.873620692004104527, 7.121571683533994168, 0.7216878364870317197 ) ) ;
#214281 = CARTESIAN_POINT ( 'NONE',  ( 4.770673279661371780, -1.444480529215144804, 1.668407551275403300 ) ) ;
#214282 = CARTESIAN_POINT ( 'NONE',  ( -5.608135385276092677, 5.599224824533728828, 0.4022279080854191391 ) ) ;
#214283 = CARTESIAN_POINT ( 'NONE',  ( 7.204675194429079505E-15, -1.793749999044084831, -3.475000000000000089 ) ) ;
#214284 = CARTESIAN_POINT ( 'NONE',  ( -1.499999999999996669, 4.910416667349485564, -0.8660254037844395958 ) ) ;
#214285 = DIRECTION ( 'NONE',  ( 5.578564026256490882E-16, 1.000000000000000000, 9.066213480720158442E-32 ) ) ;
#214286 = CARTESIAN_POINT ( 'NONE',  ( -5.897079639132071449, 7.258985838325384243, -1.264812401031592204 ) ) ;
#214287 = CARTESIAN_POINT ( 'NONE',  ( 11.00595142344305444, 12.49009581338493113, -1.443824005414910072 ) ) ;
#214288 = ORIENTED_EDGE ( 'NONE', *, *, #106262, .T. ) ;
#214289 = CARTESIAN_POINT ( 'NONE',  ( 4.821196345351608237, -0.1031141679418267343, 2.058443437638860285 ) ) ;
#214290 = CARTESIAN_POINT ( 'NONE',  ( 0.6801582343749865700, 1.307291667008089853, -1.178068619123883165 ) ) ;
#214291 = CARTESIAN_POINT ( 'NONE',  ( -6.078132937628113908, 5.985576603521232109, 1.040834085586084257E-14 ) ) ;
#214292 = CARTESIAN_POINT ( 'NONE',  ( 3.774085898144818874, 2.004173781823472833, -0.2492677732841129534 ) ) ;
#214293 = CARTESIAN_POINT ( 'NONE',  ( -1.500000000000001332, -0.8499999999999757749, 0.000000000000000000 ) ) ;
#214294 = CARTESIAN_POINT ( 'NONE',  ( 3.708318708537623021, 4.285125567170706695, -1.199719254218446718 ) ) ;
#214295 = CARTESIAN_POINT ( 'NONE',  ( 8.633844893804129228, 8.967240552393299424, -0.7998128361456211532 ) ) ;
#214296 = CARTESIAN_POINT ( 'NONE',  ( 2.641540400197890825, -1.526127808488053628, -1.385168266076434174 ) ) ;
#214297 = CARTESIAN_POINT ( 'NONE',  ( -3.253593677155282471, 6.739683690082376444, 1.040834085586084257E-14 ) ) ;
#214298 = CARTESIAN_POINT ( 'NONE',  ( 4.157546660884947620, 8.002221537674429896, 1.040834085586084257E-14 ) ) ;
#214299 =( BOUNDED_SURFACE ( )  B_SPLINE_SURFACE ( 3, 2, ( 
 ( #112480, #96189, #178489 ),
 ( #13826, #12757, #114613 ),
 ( #179554, #83093, #65755 ),
 ( #80977, #149172, #31175 ) ),
 .UNSPECIFIED., .F., .F., .T. ) 
 B_SPLINE_SURFACE_WITH_KNOTS ( ( 4, 4 ),
 ( 3, 3 ),
 ( 5.985662991022360223E-05, 0.0001887152224066861379 ),
 ( 0.000000000000000000, 1.000000000000000000 ),
 .UNSPECIFIED. ) 
 GEOMETRIC_REPRESENTATION_ITEM ( )  RATIONAL_B_SPLINE_SURFACE ( (
 ( 1.000000000000000000, 0.8739472344186550723, 1.000000000000000000),
 ( 1.000000000000000000, 0.8497613059194148999, 1.000000000000000000),
 ( 1.000000000000000000, 0.8164163343283504792, 1.000000000000000000),
 ( 1.000000000000000000, 0.7779734834199396598, 1.000000000000000000) ) ) 
 REPRESENTATION_ITEM ( '' )  SURFACE ( )  );
#214300 = MECHANICAL_DESIGN_GEOMETRIC_PRESENTATION_REPRESENTATION (  '', ( #41519 ), #203965 ) ;
#214301 = CARTESIAN_POINT ( 'NONE',  ( -0.1411974294642228400, 2.034035580701949897, -2.316051970441324936 ) ) ;
#214302 = CARTESIAN_POINT ( 'NONE',  ( 1.534833434108737515, -1.332603482217321389, -1.270662175854364362 ) ) ;
#214303 = CARTESIAN_POINT ( 'NONE',  ( 6.709632191794143274, -0.4886956906769434061, 2.160084693451309601 ) ) ;
#214304 = CARTESIAN_POINT ( 'NONE',  ( 5.417364897112183719, 8.477953592343014932, 1.199719254218451159 ) ) ;
#214305 = CARTESIAN_POINT ( 'NONE',  ( 1.897963814661303150, -0.7301937759345776824, 2.034636513274298064 ) ) ;
#214306 = CARTESIAN_POINT ( 'NONE',  ( -4.121315508874276112, 4.870918184183829602, -1.082531754730549967 ) ) ;
#214307 = CARTESIAN_POINT ( 'NONE',  ( 1.569546381206438967, 1.394087592100446971, 1.457234012747665508 ) ) ;
#214308 = EDGE_CURVE ( 'NONE', #31644, #203495, #68213, .T. ) ;
#214309 = LINE ( 'NONE', #194911, #187502 ) ;
#214310 = CARTESIAN_POINT ( 'NONE',  ( 0.2154177506630133854, -1.835460468737951878, 0.3602540799089171131 ) ) ;
#214311 = CARTESIAN_POINT ( 'NONE',  ( 4.539890248181537302, 0.8439850759212139675, -1.781816264247655157 ) ) ;
#214312 = CARTESIAN_POINT ( 'NONE',  ( 4.153529959351897283, 1.954779968807466295, -0.4946301968136583849 ) ) ;
#214314 = CARTESIAN_POINT ( 'NONE',  ( 8.202319746143333035, 12.51319743723517952, -0.7216878364870328300 ) ) ;
#214313 = CARTESIAN_POINT ( 'NONE',  ( 0.6823417656249882723, 2.426041667008084435, -1.181850606188749264 ) ) ;
#214316 = CARTESIAN_POINT ( 'NONE',  ( 5.690091061058023314, -0.9480630415420692181, 1.880679904143019776 ) ) ;
#214315 = CARTESIAN_POINT ( 'NONE',  ( -7.714753101375940503, 8.959299025482085455, 1.199719254218462483 ) ) ;
#214317 = CARTESIAN_POINT ( 'NONE',  ( 5.002425025097493538, 2.064580399062130311, 0.1557331365308264881 ) ) ;
#214318 = CARTESIAN_POINT ( 'NONE',  ( 5.494078562035752178, 7.432844293840273231, -1.599625672291262513 ) ) ;
#214319 = CARTESIAN_POINT ( 'NONE',  ( -5.554036483092550824, 9.631459663583308739, -0.7998128361456231517 ) ) ;
#214320 = CARTESIAN_POINT ( 'NONE',  ( 6.539320575229249144, 2.442570667128646900, 2.385998263081292148 ) ) ;
#214321 = CARTESIAN_POINT ( 'NONE',  ( 5.677991919488574624, 1.989193807575660555, -0.3493085226990484959 ) ) ;
#214322 = CARTESIAN_POINT ( 'NONE',  ( -1.500000000000015099, -1.089583332650509773, -0.8660254037844383745 ) ) ;
#214323 = CARTESIAN_POINT ( 'NONE',  ( 3.563348594130168578, -2.034784092110089926, -1.088618498840478566 ) ) ;
#214324 = CARTESIAN_POINT ( 'NONE',  ( 1.375913251025398409, -2.013209319166248346, 0.4479213407221314669 ) ) ;
#214325 = CARTESIAN_POINT ( 'NONE',  ( 8.920901888112002354, 9.510066412326583674, 0.7216878364870438212 ) ) ;
#214326 = ADVANCED_FACE ( 'NONE', ( #106165 ), #173156, .F. ) ;
#214327 = CARTESIAN_POINT ( 'NONE',  ( 5.020262018810099924, 9.078999131912302900, 0.7998128361456331437 ) ) ;
#214328 = CARTESIAN_POINT ( 'NONE',  ( 6.723917837734620484, 6.809268663637336516, 0.000000000000000000 ) ) ;
#214329 = CARTESIAN_POINT ( 'NONE',  ( -1.364683531250014514, 0.5510416670080878765, -0.7879004041258289570 ) ) ;
#214330 = CARTESIAN_POINT ( 'NONE',  ( 6.378184920586140727, 6.405913593630768510, 0.000000000000000000 ) ) ;
#214331 = CARTESIAN_POINT ( 'NONE',  ( 7.253248993186731219, 8.524840582548424806, 1.082531754730558626 ) ) ;
#214333 =( NAMED_UNIT ( * ) SI_UNIT ( $, .STERADIAN. ) SOLID_ANGLE_UNIT ( ) );
#214332 = CARTESIAN_POINT ( 'NONE',  ( 4.650930581473819991, -0.4712930505080668575, -2.119270573956061554 ) ) ;
#214334 = CARTESIAN_POINT ( 'NONE',  ( -3.291865441634294509, -0.8887487162373572946, 0.07338535974613247248 ) ) ;
#214336 = CARTESIAN_POINT ( 'NONE',  ( 3.298233973420101606, 1.449563003725433896, -1.135193286699177628 ) ) ;
#214335 = CARTESIAN_POINT ( 'NONE',  ( -3.633221978782283923, 7.182583375313884133, -0.7216878364870267237 ) ) ;
#214337 = CARTESIAN_POINT ( 'NONE',  ( 1.364683531249990311, 5.134375000341417916, 1.214306433183764966E-14 ) ) ;
#214338 = CARTESIAN_POINT ( 'NONE',  ( 4.898067072109578035, -0.7382639882421681010, -2.063579870930781546 ) ) ;
#214339 = DIRECTION ( 'NONE',  ( 0.000000000000000000, 0.000000000000000000, 1.000000000000000000 ) ) ;
#214340 = CARTESIAN_POINT ( 'NONE',  ( 6.332949636392265269, 0.2142684956521986317, 2.252356394309730003 ) ) ;
#214341 = CARTESIAN_POINT ( 'NONE',  ( -5.512600778122673795, 6.408089294489160537, -1.271103323116394845 ) ) ;
#214342 = CARTESIAN_POINT ( 'NONE',  ( 4.648548116941726427, 8.423941524322412278, -0.4686463081053967583 ) ) ;
#214343 = STYLED_ITEM ( 'NONE', ( #175257 ), #25207 ) ;
#214344 = CARTESIAN_POINT ( 'NONE',  ( -5.682275777458886346, 7.722684055159061423, 1.443375672974058777 ) ) ;
#214345 = CARTESIAN_POINT ( 'NONE',  ( 5.248414862265931902, 5.295774558831261913, 0.000000000000000000 ) ) ;
#214346 = CARTESIAN_POINT ( 'NONE',  ( 6.204346024843479412, -0.6390883176130756071, -1.650510209504873593 ) ) ;
#214347 = CARTESIAN_POINT ( 'NONE',  ( 4.670568766136569572, 0.7725349690445941775, 1.859148924064259356 ) ) ;
#214348 = CARTESIAN_POINT ( 'NONE',  ( 6.286176778230493589, 10.48562334124426698, 0.7998128361456462443 ) ) ;
#214349 = CARTESIAN_POINT ( 'NONE',  ( 3.487430266828908998, 1.904693919176775552, -0.8987260315082377105 ) ) ;
#214350 = CARTESIAN_POINT ( 'NONE',  ( 1.616650230726389248, 0.1894562617417178962, 1.906227014244334717 ) ) ;
#214351 = CARTESIAN_POINT ( 'NONE',  ( 4.009460741339333723, 5.700790169694431420, -1.599625672291256295 ) ) ;
#214352 = CARTESIAN_POINT ( 'NONE',  ( 3.297268302959563524, -1.738273807845453600, 0.9259864402798111405 ) ) ;
#214353 = CARTESIAN_POINT ( 'NONE',  ( 4.781513128076603003, 0.1936695275622651868, -2.010448953515688419 ) ) ;
#214354 = CARTESIAN_POINT ( 'NONE',  ( 0.5494049127674709432, 0.5909524230637287490, -1.774924738581270089 ) ) ;
#214355 = CARTESIAN_POINT ( 'NONE',  ( 1.451531895509536874, 1.483362660712842063, 1.284035263222626844 ) ) ;
#214357 = VERTEX_POINT ( 'NONE', #81075 ) ;
#214356 = CARTESIAN_POINT ( 'NONE',  ( 0.1934256698341470238, 1.783621342183003389, -0.6902995980747894667 ) ) ;
#214358 = CARTESIAN_POINT ( 'NONE',  ( 4.690757960648221037, 7.456006139856155457, 1.082531754730558626 ) ) ;
#214359 = CARTESIAN_POINT ( 'NONE',  ( 0.6823417656249882723, 1.238541667008083547, -1.181850606188749264 ) ) ;
#214360 = AXIS2_PLACEMENT_3D ( 'NONE', #138527, #70282, #139606 ) ;
#214361 = CARTESIAN_POINT ( 'NONE',  ( 6.332864056472936376, 0.1854757364097951722, 1.861418627818342664 ) ) ;
#214362 = CARTESIAN_POINT ( 'NONE',  ( 3.379006598303866848, 4.965260336153046516, -1.599625672291262513 ) ) ;
#214363 = DIRECTION ( 'NONE',  ( 1.276756478318932585E-15, -1.000000000000000000, 1.665334536937738262E-16 ) ) ;
#214364 = CARTESIAN_POINT ( 'NONE',  ( 6.262565978045822490, -0.7396069823457154246, -1.933831554736538338 ) ) ;
#214365 = SURFACE_STYLE_FILL_AREA ( #141206 ) ;
#214366 = CARTESIAN_POINT ( 'NONE',  ( 0.4497787391488928810, 1.533077660697563793, 1.391591089521776681 ) ) ;
#214367 = CARTESIAN_POINT ( 'NONE',  ( -1.500000000000013101, 1.170833333333352710, 0.8660254037844403729 ) ) ;
#214368 = CARTESIAN_POINT ( 'NONE',  ( 5.774883364416965037, 8.824782127540085952, -1.199719254218440723 ) ) ;
#214369 = CARTESIAN_POINT ( 'NONE',  ( -7.232384877886063990, 10.52520055992070525, -1.199719254218446718 ) ) ;
#214370 = CARTESIAN_POINT ( 'NONE',  ( 4.797606254389322089, 6.690569611577942943, 1.599625672291268286 ) ) ;
#214371 = CARTESIAN_POINT ( 'NONE',  ( 5.039744756118590630, -2.013340025477545758, 0.6656774797743277849 ) ) ;
#214372 = CARTESIAN_POINT ( 'NONE',  ( 4.947799714344386146, 4.737130853015369958, -0.7998128361456481317 ) ) ;
#214373 = CARTESIAN_POINT ( 'NONE',  ( 1.364683531249986537, 1.905208333674750287, -0.7879004041258239610 ) ) ;
#214374 = ORIENTED_EDGE ( 'NONE', *, *, #161432, .T. ) ;
#214375 = CARTESIAN_POINT ( 'NONE',  ( 0.7499999999999902300, 2.983333333333351600, 1.299038105676669330 ) ) ;
#214377 = CARTESIAN_POINT ( 'NONE',  ( 5.332434488876471868, 5.115595079977664383, 0.7998128361456341429 ) ) ;
#214376 = CARTESIAN_POINT ( 'NONE',  ( 5.881297811770386907, -0.04968318840743202180, 1.961410508136133712 ) ) ;
#214378 = CARTESIAN_POINT ( 'NONE',  ( 2.899767358622063806, 0.2439914025648345919, 2.001204936777578602 ) ) ;
#214379 = EDGE_CURVE ( 'NONE', #28319, #42265, #107116, .T. ) ;
#214380 = CARTESIAN_POINT ( 'NONE',  ( 3.661272352971048694, 1.801931492627879106, -0.6507149165355142761 ) ) ;
#214381 = CARTESIAN_POINT ( 'NONE',  ( -1.886017674307070457, 3.298060805577415877, -0.4014564593431291795 ) ) ;
#214382 = CARTESIAN_POINT ( 'NONE',  ( 2.068174269828721101, -1.345378145056834063, 1.729934933326432445 ) ) ;
#214383 = CARTESIAN_POINT ( 'NONE',  ( 4.924072945520472366, 4.709449622720799589, 0.000000000000000000 ) ) ;
#214384 = CARTESIAN_POINT ( 'NONE',  ( 3.251090012001829788, -1.527204365403836306, -1.079795099579644591 ) ) ;
#214385 = CARTESIAN_POINT ( 'NONE',  ( 1.499999999999987566, -0.4437499993171847845, 0.000000000000000000 ) ) ;
#214386 = CARTESIAN_POINT ( 'NONE',  ( 4.676043659170272093, 1.990676093108449951, -0.2997180003130732739 ) ) ;
#214387 = CARTESIAN_POINT ( 'NONE',  ( -7.049349804101573191, 10.31165964050546258, -1.199719254218440723 ) ) ;
#214389 = CARTESIAN_POINT ( 'NONE',  ( 5.484029812627264633, -2.117403151077674739, 0.0008096548943584136460 ) ) ;
#214388 = CARTESIAN_POINT ( 'NONE',  ( -4.799223189557577207, 4.701441264013013210, 0.7216878364870317197 ) ) ;
#214390 = CARTESIAN_POINT ( 'NONE',  ( -1.247849810309911600, 13.37576698399836594, 0.5524780460566154350 ) ) ;
#214391 = FACE_OUTER_BOUND ( 'NONE', #160669, .T. ) ;
#214393 = CARTESIAN_POINT ( 'NONE',  ( -5.469769711976988802, 6.852634337065973469, -1.200242106353874627 ) ) ;
#214392 = CARTESIAN_POINT ( 'NONE',  ( 1.839510613029649466, 0.7972044211956804682, -1.932997742640076400 ) ) ;
#214395 = EDGE_LOOP ( 'NONE', ( #48515, #121534, #118541, #212337 ) ) ;
#214394 = CARTESIAN_POINT ( 'NONE',  ( 0.5863794435163689478, -0.2038549220112067795, -1.712615276990290480 ) ) ;
#214396 = CARTESIAN_POINT ( 'NONE',  ( 6.449928391799196525, 8.548002428564306143, -1.599625672291262513 ) ) ;
#214397 = CARTESIAN_POINT ( 'NONE',  ( -1.500000000000008216, 12.03125000068279427, 3.469446951953614189E-15 ) ) ;
#214398 = CARTESIAN_POINT ( 'NONE',  ( -0.09916492693111574053, -9.919999999999998153, -9.499482423651645746 ) ) ;
#214399 = CARTESIAN_POINT ( 'NONE',  ( -0.2883962233416142440, -9.094943692057514184, 9.630124952822544770 ) ) ;
#214400 = CARTESIAN_POINT ( 'NONE',  ( 9.232739420781973294, 9.873876867108206667, -0.7216878364870257245 ) ) ;
#214401 = CARTESIAN_POINT ( 'NONE',  ( 0.000000000000000000, 8.500000000000000000, 0.000000000000000000 ) ) ;
#214403 = CARTESIAN_POINT ( 'NONE',  ( 1.646807439477548707, 0.1776336960073976179, 1.802747333403993402 ) ) ;
#214402 = CARTESIAN_POINT ( 'NONE',  ( 4.518610335104485287, 8.493738834255713854, 0.000000000000000000 ) ) ;
#214404 = CARTESIAN_POINT ( 'NONE',  ( -5.856232286098998152, 8.919689202835742847, 1.199719254218452047 ) ) ;
#214405 = CARTESIAN_POINT ( 'NONE',  ( 3.669453130792974971, 7.432779085900453886, 1.040834085586084257E-14 ) ) ;
#214406 = CARTESIAN_POINT ( 'NONE',  ( -6.452141306522730879, 6.789529044577018446, 0.3774816029595753353 ) ) ;
#214407 = CARTESIAN_POINT ( 'NONE',  ( 6.333594036239346359, 7.418223126147930557, 1.199719254218453823 ) ) ;
#214408 = CARTESIAN_POINT ( 'NONE',  ( 6.639320575229259447, 2.978120323461688201, 2.350396677589302374 ) ) ;
#214409 = CARTESIAN_POINT ( 'NONE',  ( -2.081668171172168513E-14, 6.487495393664096888, 3.100011470320013451 ) ) ;
#214410 = CARTESIAN_POINT ( 'NONE',  ( -6.231486212180770146, 6.935029357745537304, 0.8357456600066525132 ) ) ;
#214411 = NEXT_ASSEMBLY_USAGE_OCCURRENCE ( 'NAUO1', ' ', ' ', #19950, #160678, $ ) ;
#214412 = NEXT_ASSEMBLY_USAGE_OCCURRENCE ( 'NAUO2', ' ', ' ', #19950, #90511, $ ) ;
#214413 = NEXT_ASSEMBLY_USAGE_OCCURRENCE ( 'NAUO3', ' ', ' ', #19950, #57493, $ ) ;
#214414 = NEXT_ASSEMBLY_USAGE_OCCURRENCE ( 'NAUO4', ' ', ' ', #19950, #128970, $ ) ;
#214415 = NEXT_ASSEMBLY_USAGE_OCCURRENCE ( 'NAUO5', ' ', ' ', #19950, #95911, $ ) ;
#214416 = NEXT_ASSEMBLY_USAGE_OCCURRENCE ( 'NAUO6', ' ', ' ', #19950, #52109, $ ) ;
#214417 = NEXT_ASSEMBLY_USAGE_OCCURRENCE ( 'NAUO7', ' ', ' ', #19950, #35864, $ ) ;
#214418 = NEXT_ASSEMBLY_USAGE_OCCURRENCE ( 'NAUO8', ' ', ' ', #19950, #35864, $ ) ;
#214419 = NEXT_ASSEMBLY_USAGE_OCCURRENCE ( 'NAUO9', ' ', ' ', #19950, #35864, $ ) ;
#214420 = NEXT_ASSEMBLY_USAGE_OCCURRENCE ( 'NAUO10', ' ', ' ', #19950, #35864, $ ) ;
#214421 = NEXT_ASSEMBLY_USAGE_OCCURRENCE ( 'NAUO11', ' ', ' ', #19950, #151058, $ ) ;
#214422 = NEXT_ASSEMBLY_USAGE_OCCURRENCE ( 'NAUO12', ' ', ' ', #19950, #51771, $ ) ;
#214423 = NEXT_ASSEMBLY_USAGE_OCCURRENCE ( 'NAUO13', ' ', ' ', #19950, #189422, $ ) ;
#214424 = NEXT_ASSEMBLY_USAGE_OCCURRENCE ( 'NAUO14', ' ', ' ', #19950, #135165, $ ) ;
#214425 = NEXT_ASSEMBLY_USAGE_OCCURRENCE ( 'NAUO15', ' ', ' ', #19950, #103356, $ ) ;
#214426 = NEXT_ASSEMBLY_USAGE_OCCURRENCE ( 'NAUO16', ' ', ' ', #19950, #173573, $ ) ;
#214427 = NEXT_ASSEMBLY_USAGE_OCCURRENCE ( 'NAUO17', ' ', ' ', #19950, #196048, $ ) ;
#214428 = NEXT_ASSEMBLY_USAGE_OCCURRENCE ( 'NAUO18', ' ', ' ', #19950, #196048, $ ) ;
#214429 = NEXT_ASSEMBLY_USAGE_OCCURRENCE ( 'NAUO19', ' ', ' ', #19950, #26565, $ ) ;
#214430 = NEXT_ASSEMBLY_USAGE_OCCURRENCE ( 'NAUO20', ' ', ' ', #19950, #141784, $ ) ;
#214431 = NEXT_ASSEMBLY_USAGE_OCCURRENCE ( 'NAUO21', ' ', ' ', #19950, #141784, $ ) ;
#214432 = NEXT_ASSEMBLY_USAGE_OCCURRENCE ( 'NAUO22', ' ', ' ', #19950, #128644, $ ) ;
ENDSEC;
END-ISO-10303-21;
